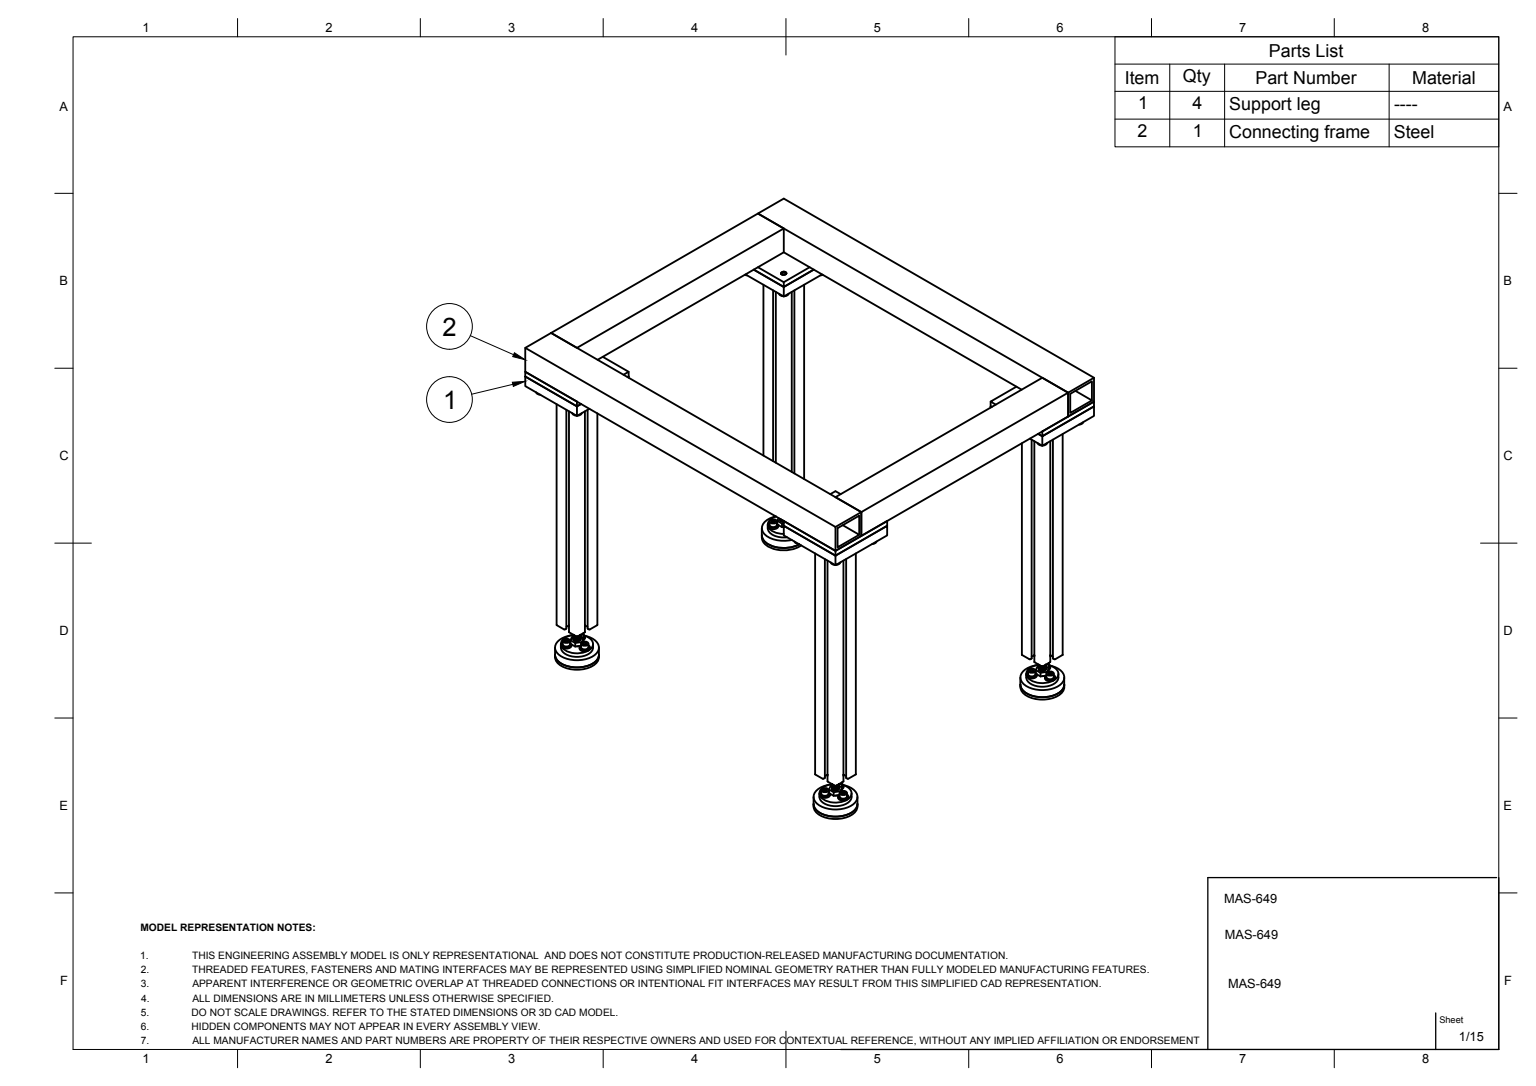
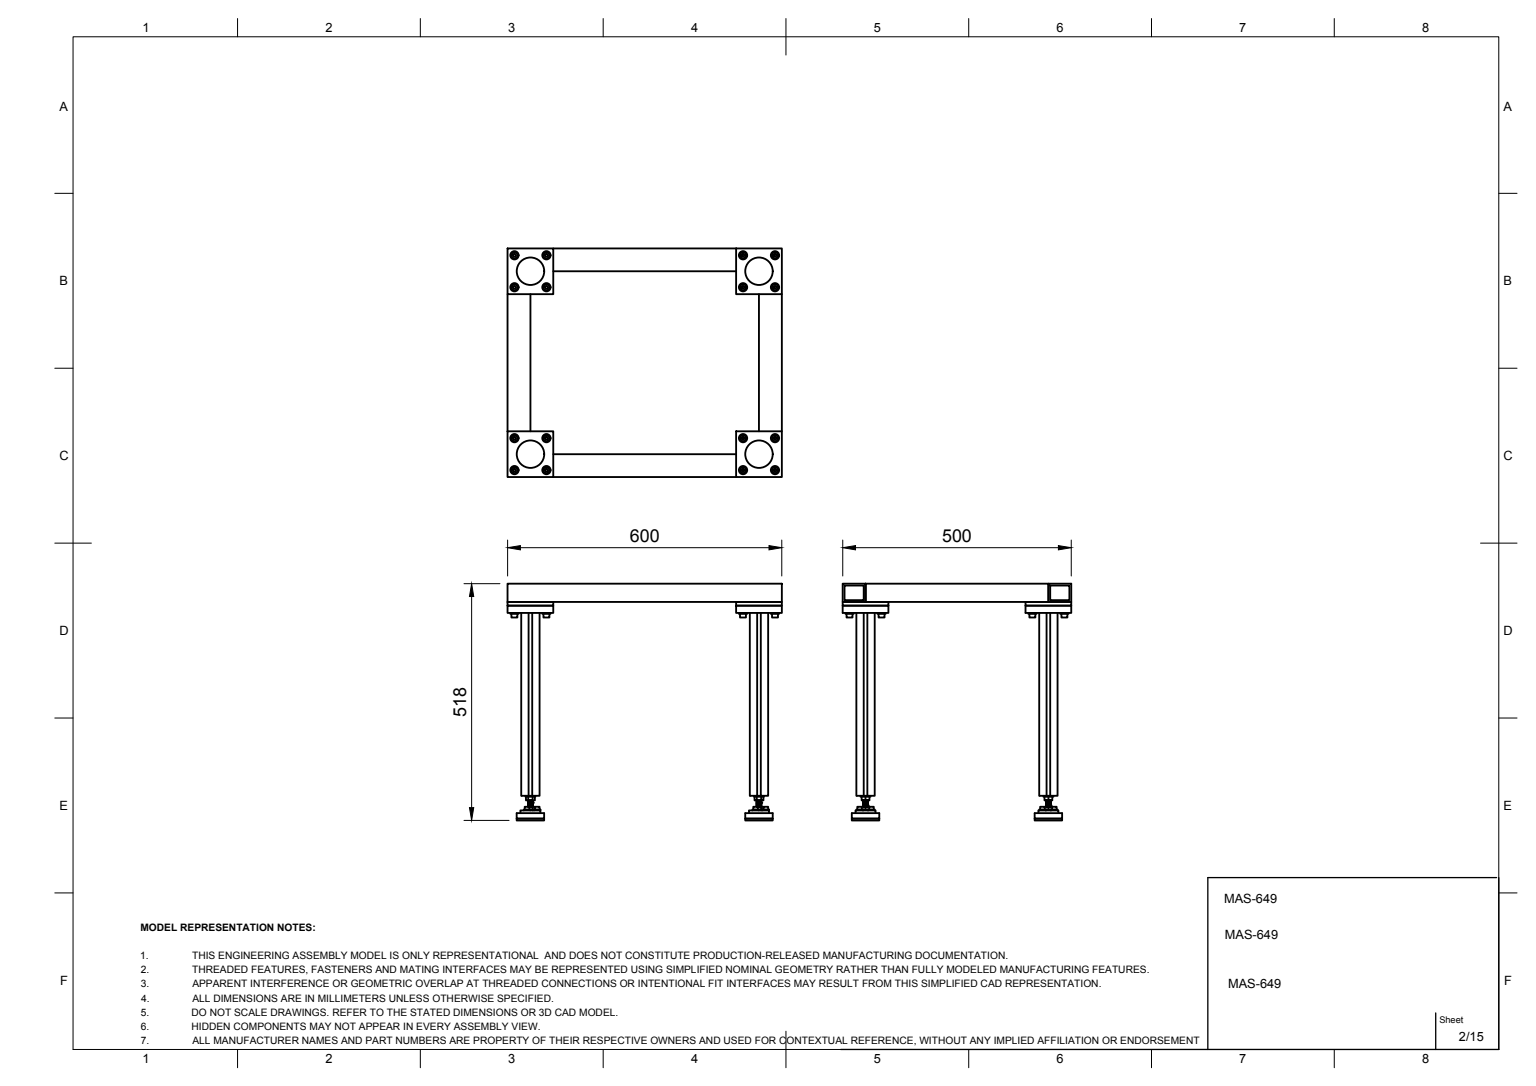
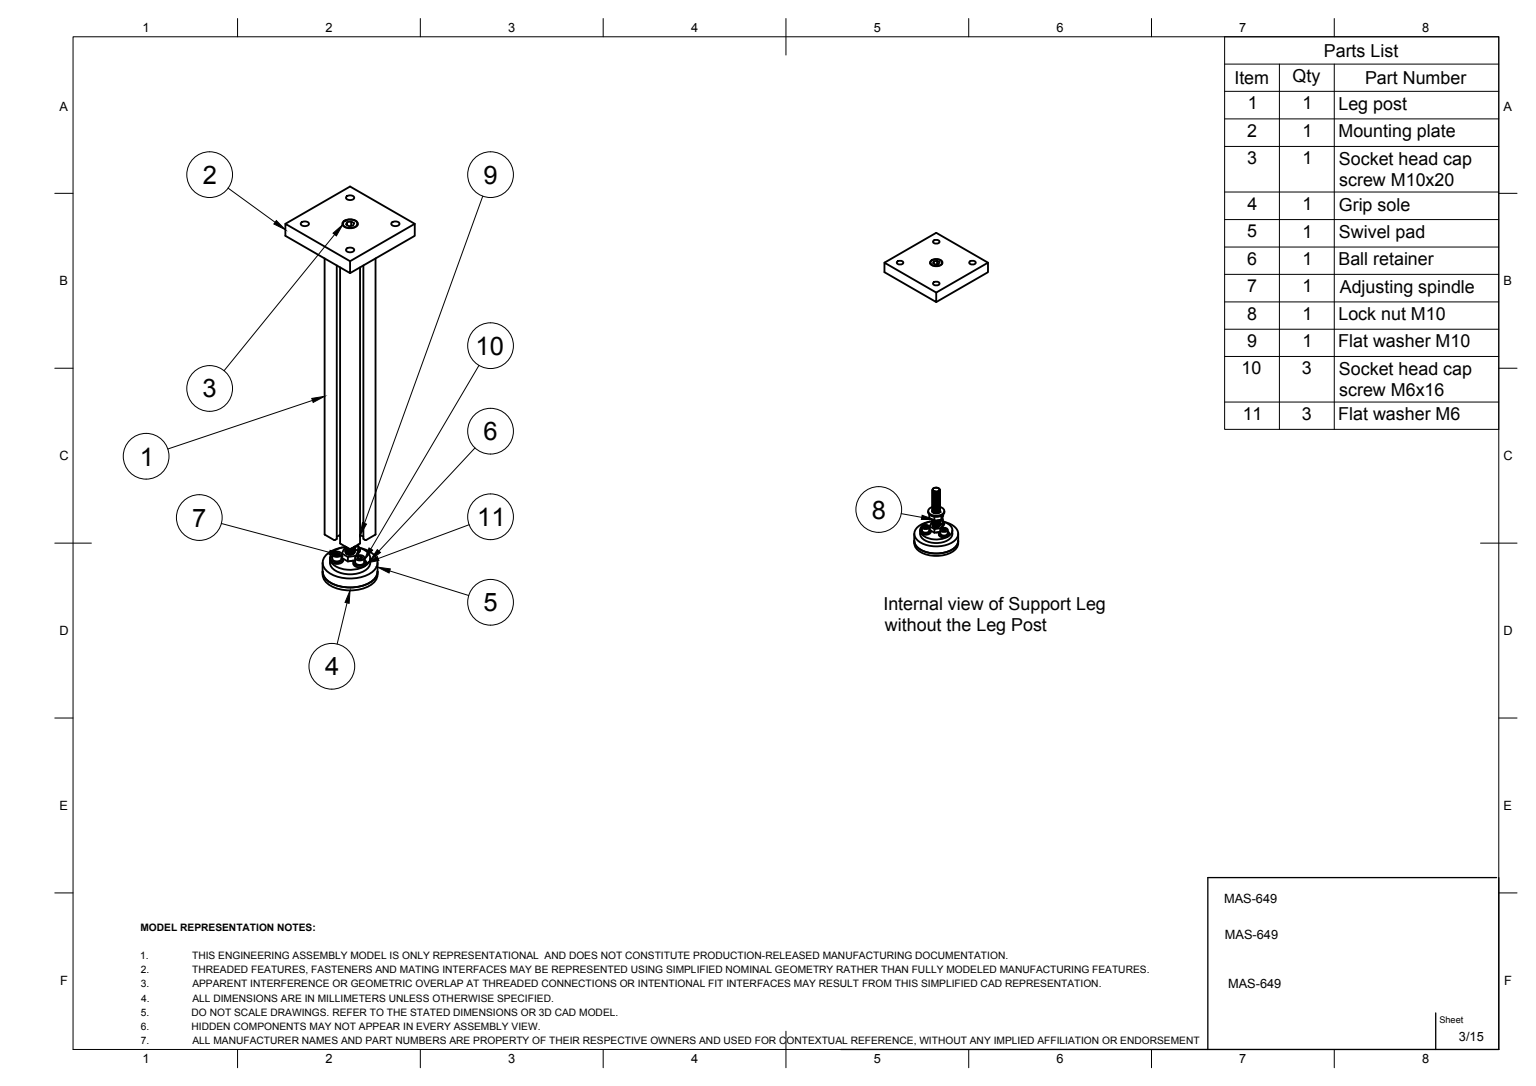
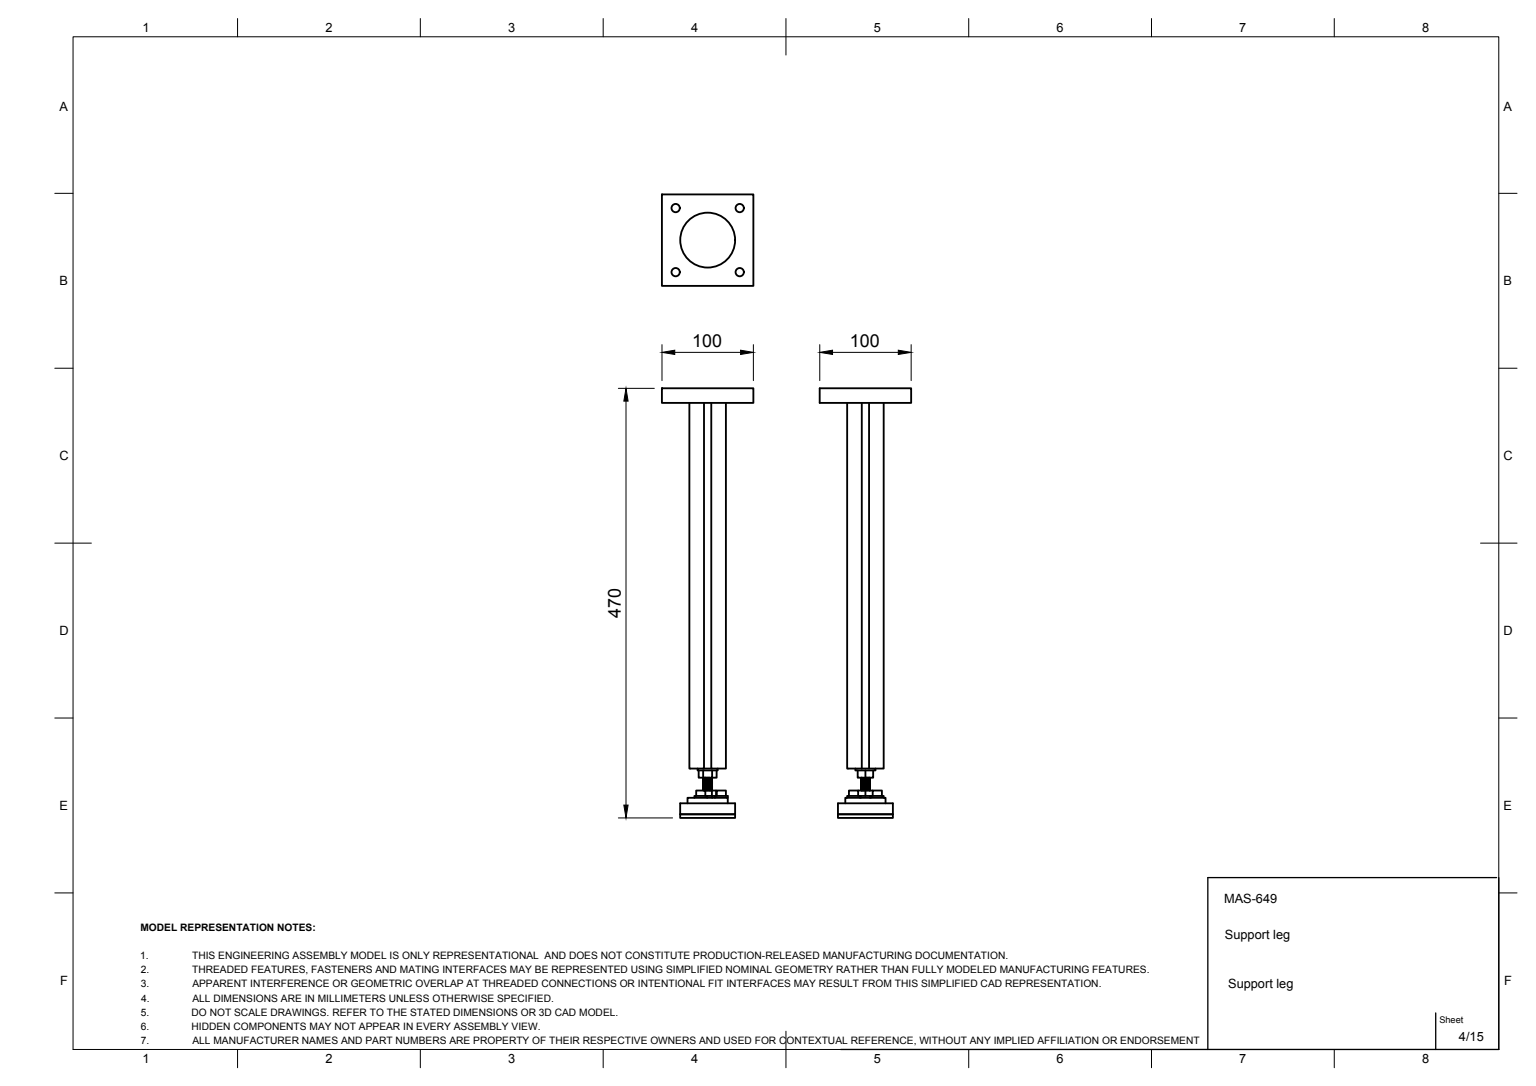
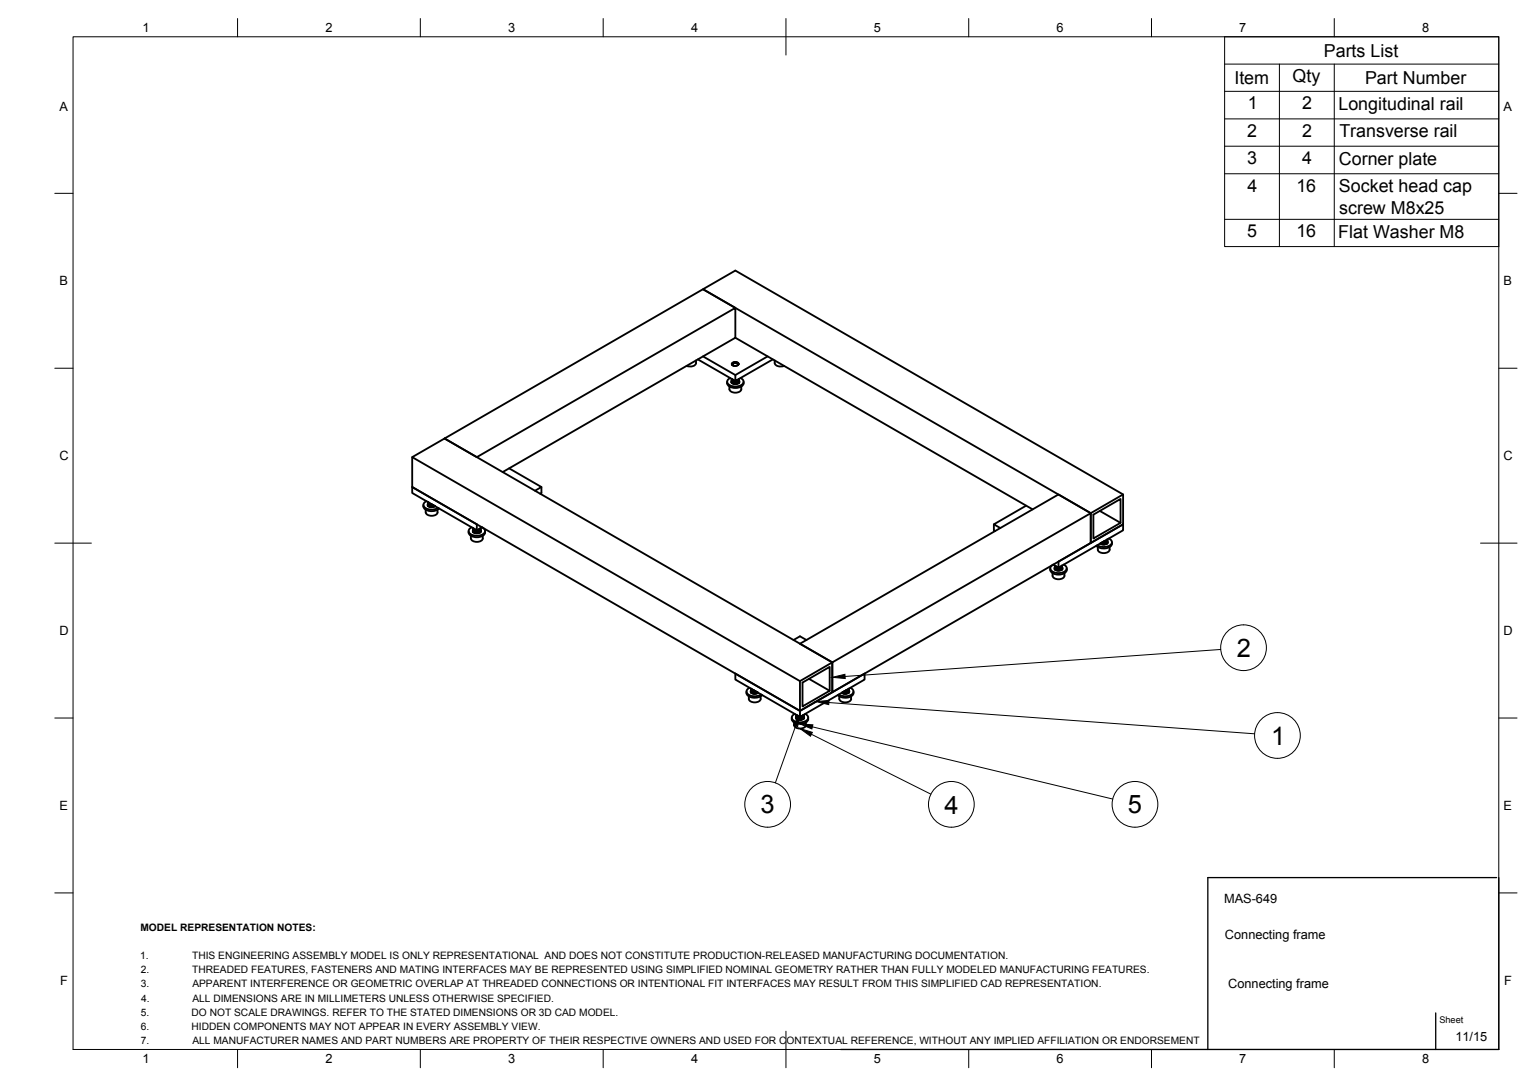
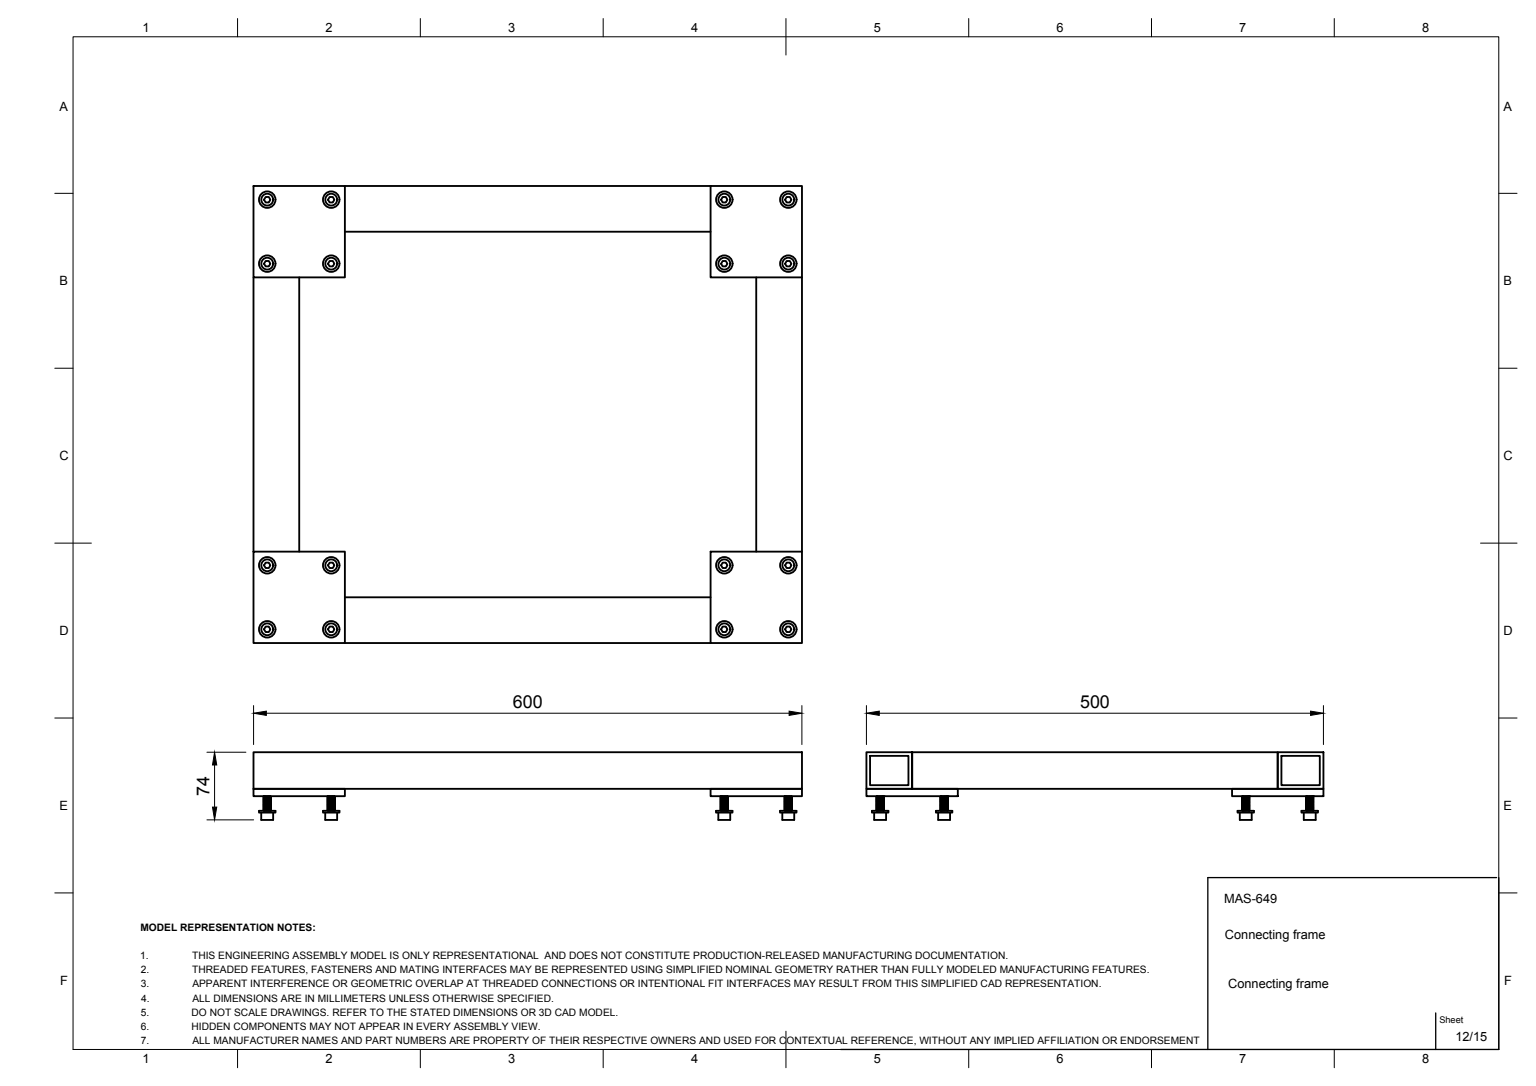
ISO-10303-21;
HEADER;
/* Generated by software containing ST-Developer
 * from STEP Tools, Inc. (www.steptools.com) 
 */

FILE_DESCRIPTION(
/* description */ ('Independent equipment support assembly with bolted 600 x 500 mm welde
d perimeter frame, four adjustable legs and swivel feet. Nominal overa
ll height 518 mm. No load rating assigned.'),
/* implementation_level */ '2;1');

FILE_NAME(
/* name */ 'MAS-649.step',
/* time_stamp */ '2026-11-07T17:30:39-08:00',
/* author */ (''),
/* organization */ (''),
/* preprocessor_version */ 'ST-DEVELOPER v20.2',
/* originating_system */ 'Autodesk Translation Framework v15.17.0.0',
/* authorisation */ '');

FILE_SCHEMA (('AUTOMOTIVE_DESIGN { 1 0 10303 214 3 1 1 }'));
ENDSEC;

DATA;
#10=MECHANICAL_DESIGN_GEOMETRIC_PRESENTATION_REPRESENTATION('',(#2208,#2209,
#2210,#2211,#2212,#2213,#2214,#2215,#2216,#2217,#2218,#2219,#2220,#2221,
#2222,#2223),#63755);
#11=SPHERICAL_SURFACE('',#15224,6.);
#12=SPHERICAL_SURFACE('',#15242,6.);
#13=SPHERICAL_SURFACE('',#15392,6.);
#14=ITEM_DEFINED_TRANSFORMATION($,$,#14504,#14700);
#15=ITEM_DEFINED_TRANSFORMATION($,$,#14515,#14701);
#16=ITEM_DEFINED_TRANSFORMATION($,$,#14526,#14702);
#17=ITEM_DEFINED_TRANSFORMATION($,$,#14621,#14703);
#18=ITEM_DEFINED_TRANSFORMATION($,$,#14691,#14704);
#19=ITEM_DEFINED_TRANSFORMATION($,$,#14504,#14705);
#20=ITEM_DEFINED_TRANSFORMATION($,$,#14515,#14706);
#21=ITEM_DEFINED_TRANSFORMATION($,$,#14526,#14707);
#22=ITEM_DEFINED_TRANSFORMATION($,$,#14526,#14708);
#23=ITEM_DEFINED_TRANSFORMATION($,$,#14526,#14709);
#24=ITEM_DEFINED_TRANSFORMATION($,$,#14621,#14710);
#25=ITEM_DEFINED_TRANSFORMATION($,$,#14691,#14711);
#26=ITEM_DEFINED_TRANSFORMATION($,$,#14621,#14712);
#27=ITEM_DEFINED_TRANSFORMATION($,$,#14691,#14713);
#28=ITEM_DEFINED_TRANSFORMATION($,$,#14621,#14714);
#29=ITEM_DEFINED_TRANSFORMATION($,$,#14691,#14715);
#30=ITEM_DEFINED_TRANSFORMATION($,$,#14621,#14716);
#31=ITEM_DEFINED_TRANSFORMATION($,$,#14691,#14717);
#32=ITEM_DEFINED_TRANSFORMATION($,$,#14621,#14718);
#33=ITEM_DEFINED_TRANSFORMATION($,$,#14691,#14719);
#34=ITEM_DEFINED_TRANSFORMATION($,$,#14621,#14720);
#35=ITEM_DEFINED_TRANSFORMATION($,$,#14691,#14721);
#36=ITEM_DEFINED_TRANSFORMATION($,$,#14621,#14722);
#37=ITEM_DEFINED_TRANSFORMATION($,$,#14691,#14723);
#38=ITEM_DEFINED_TRANSFORMATION($,$,#14621,#14724);
#39=ITEM_DEFINED_TRANSFORMATION($,$,#14691,#14725);
#40=ITEM_DEFINED_TRANSFORMATION($,$,#14621,#14726);
#41=ITEM_DEFINED_TRANSFORMATION($,$,#14691,#14727);
#42=ITEM_DEFINED_TRANSFORMATION($,$,#14621,#14728);
#43=ITEM_DEFINED_TRANSFORMATION($,$,#14691,#14729);
#44=ITEM_DEFINED_TRANSFORMATION($,$,#14621,#14730);
#45=ITEM_DEFINED_TRANSFORMATION($,$,#14691,#14731);
#46=ITEM_DEFINED_TRANSFORMATION($,$,#14621,#14732);
#47=ITEM_DEFINED_TRANSFORMATION($,$,#14691,#14733);
#48=ITEM_DEFINED_TRANSFORMATION($,$,#14621,#14734);
#49=ITEM_DEFINED_TRANSFORMATION($,$,#14691,#14735);
#50=ITEM_DEFINED_TRANSFORMATION($,$,#14621,#14736);
#51=ITEM_DEFINED_TRANSFORMATION($,$,#14691,#14737);
#52=ITEM_DEFINED_TRANSFORMATION($,$,#14621,#14738);
#53=ITEM_DEFINED_TRANSFORMATION($,$,#14691,#14739);
#54=ITEM_DEFINED_TRANSFORMATION($,$,#14741,#15495);
#55=ITEM_DEFINED_TRANSFORMATION($,$,#15053,#15496);
#56=ITEM_DEFINED_TRANSFORMATION($,$,#15079,#15497);
#57=ITEM_DEFINED_TRANSFORMATION($,$,#15139,#15498);
#58=ITEM_DEFINED_TRANSFORMATION($,$,#15145,#15499);
#59=ITEM_DEFINED_TRANSFORMATION($,$,#15232,#15500);
#60=ITEM_DEFINED_TRANSFORMATION($,$,#15253,#15501);
#61=ITEM_DEFINED_TRANSFORMATION($,$,#15394,#15502);
#62=ITEM_DEFINED_TRANSFORMATION($,$,#15425,#15503);
#63=ITEM_DEFINED_TRANSFORMATION($,$,#15434,#15504);
#64=ITEM_DEFINED_TRANSFORMATION($,$,#15486,#15505);
#65=ITEM_DEFINED_TRANSFORMATION($,$,#15434,#15506);
#66=ITEM_DEFINED_TRANSFORMATION($,$,#15486,#15507);
#67=ITEM_DEFINED_TRANSFORMATION($,$,#15434,#15508);
#68=ITEM_DEFINED_TRANSFORMATION($,$,#15486,#15509);
#69=ITEM_DEFINED_TRANSFORMATION($,$,#14740,#15510);
#70=ITEM_DEFINED_TRANSFORMATION($,$,#14503,#15511);
#71=ITEM_DEFINED_TRANSFORMATION($,$,#14740,#15512);
#72=ITEM_DEFINED_TRANSFORMATION($,$,#14740,#15513);
#73=ITEM_DEFINED_TRANSFORMATION($,$,#14740,#15514);
#74=(
REPRESENTATION_RELATIONSHIP($,$,#63860,#63859)
REPRESENTATION_RELATIONSHIP_WITH_TRANSFORMATION(#14)
SHAPE_REPRESENTATION_RELATIONSHIP()
);
#75=(
REPRESENTATION_RELATIONSHIP($,$,#63861,#63859)
REPRESENTATION_RELATIONSHIP_WITH_TRANSFORMATION(#15)
SHAPE_REPRESENTATION_RELATIONSHIP()
);
#76=(
REPRESENTATION_RELATIONSHIP($,$,#63862,#63859)
REPRESENTATION_RELATIONSHIP_WITH_TRANSFORMATION(#16)
SHAPE_REPRESENTATION_RELATIONSHIP()
);
#77=(
REPRESENTATION_RELATIONSHIP($,$,#63863,#63859)
REPRESENTATION_RELATIONSHIP_WITH_TRANSFORMATION(#17)
SHAPE_REPRESENTATION_RELATIONSHIP()
);
#78=(
REPRESENTATION_RELATIONSHIP($,$,#63864,#63859)
REPRESENTATION_RELATIONSHIP_WITH_TRANSFORMATION(#18)
SHAPE_REPRESENTATION_RELATIONSHIP()
);
#79=(
REPRESENTATION_RELATIONSHIP($,$,#63860,#63859)
REPRESENTATION_RELATIONSHIP_WITH_TRANSFORMATION(#19)
SHAPE_REPRESENTATION_RELATIONSHIP()
);
#80=(
REPRESENTATION_RELATIONSHIP($,$,#63861,#63859)
REPRESENTATION_RELATIONSHIP_WITH_TRANSFORMATION(#20)
SHAPE_REPRESENTATION_RELATIONSHIP()
);
#81=(
REPRESENTATION_RELATIONSHIP($,$,#63862,#63859)
REPRESENTATION_RELATIONSHIP_WITH_TRANSFORMATION(#21)
SHAPE_REPRESENTATION_RELATIONSHIP()
);
#82=(
REPRESENTATION_RELATIONSHIP($,$,#63862,#63859)
REPRESENTATION_RELATIONSHIP_WITH_TRANSFORMATION(#22)
SHAPE_REPRESENTATION_RELATIONSHIP()
);
#83=(
REPRESENTATION_RELATIONSHIP($,$,#63862,#63859)
REPRESENTATION_RELATIONSHIP_WITH_TRANSFORMATION(#23)
SHAPE_REPRESENTATION_RELATIONSHIP()
);
#84=(
REPRESENTATION_RELATIONSHIP($,$,#63863,#63859)
REPRESENTATION_RELATIONSHIP_WITH_TRANSFORMATION(#24)
SHAPE_REPRESENTATION_RELATIONSHIP()
);
#85=(
REPRESENTATION_RELATIONSHIP($,$,#63864,#63859)
REPRESENTATION_RELATIONSHIP_WITH_TRANSFORMATION(#25)
SHAPE_REPRESENTATION_RELATIONSHIP()
);
#86=(
REPRESENTATION_RELATIONSHIP($,$,#63863,#63859)
REPRESENTATION_RELATIONSHIP_WITH_TRANSFORMATION(#26)
SHAPE_REPRESENTATION_RELATIONSHIP()
);
#87=(
REPRESENTATION_RELATIONSHIP($,$,#63864,#63859)
REPRESENTATION_RELATIONSHIP_WITH_TRANSFORMATION(#27)
SHAPE_REPRESENTATION_RELATIONSHIP()
);
#88=(
REPRESENTATION_RELATIONSHIP($,$,#63863,#63859)
REPRESENTATION_RELATIONSHIP_WITH_TRANSFORMATION(#28)
SHAPE_REPRESENTATION_RELATIONSHIP()
);
#89=(
REPRESENTATION_RELATIONSHIP($,$,#63864,#63859)
REPRESENTATION_RELATIONSHIP_WITH_TRANSFORMATION(#29)
SHAPE_REPRESENTATION_RELATIONSHIP()
);
#90=(
REPRESENTATION_RELATIONSHIP($,$,#63863,#63859)
REPRESENTATION_RELATIONSHIP_WITH_TRANSFORMATION(#30)
SHAPE_REPRESENTATION_RELATIONSHIP()
);
#91=(
REPRESENTATION_RELATIONSHIP($,$,#63864,#63859)
REPRESENTATION_RELATIONSHIP_WITH_TRANSFORMATION(#31)
SHAPE_REPRESENTATION_RELATIONSHIP()
);
#92=(
REPRESENTATION_RELATIONSHIP($,$,#63863,#63859)
REPRESENTATION_RELATIONSHIP_WITH_TRANSFORMATION(#32)
SHAPE_REPRESENTATION_RELATIONSHIP()
);
#93=(
REPRESENTATION_RELATIONSHIP($,$,#63864,#63859)
REPRESENTATION_RELATIONSHIP_WITH_TRANSFORMATION(#33)
SHAPE_REPRESENTATION_RELATIONSHIP()
);
#94=(
REPRESENTATION_RELATIONSHIP($,$,#63863,#63859)
REPRESENTATION_RELATIONSHIP_WITH_TRANSFORMATION(#34)
SHAPE_REPRESENTATION_RELATIONSHIP()
);
#95=(
REPRESENTATION_RELATIONSHIP($,$,#63864,#63859)
REPRESENTATION_RELATIONSHIP_WITH_TRANSFORMATION(#35)
SHAPE_REPRESENTATION_RELATIONSHIP()
);
#96=(
REPRESENTATION_RELATIONSHIP($,$,#63863,#63859)
REPRESENTATION_RELATIONSHIP_WITH_TRANSFORMATION(#36)
SHAPE_REPRESENTATION_RELATIONSHIP()
);
#97=(
REPRESENTATION_RELATIONSHIP($,$,#63864,#63859)
REPRESENTATION_RELATIONSHIP_WITH_TRANSFORMATION(#37)
SHAPE_REPRESENTATION_RELATIONSHIP()
);
#98=(
REPRESENTATION_RELATIONSHIP($,$,#63863,#63859)
REPRESENTATION_RELATIONSHIP_WITH_TRANSFORMATION(#38)
SHAPE_REPRESENTATION_RELATIONSHIP()
);
#99=(
REPRESENTATION_RELATIONSHIP($,$,#63864,#63859)
REPRESENTATION_RELATIONSHIP_WITH_TRANSFORMATION(#39)
SHAPE_REPRESENTATION_RELATIONSHIP()
);
#100=(
REPRESENTATION_RELATIONSHIP($,$,#63863,#63859)
REPRESENTATION_RELATIONSHIP_WITH_TRANSFORMATION(#40)
SHAPE_REPRESENTATION_RELATIONSHIP()
);
#101=(
REPRESENTATION_RELATIONSHIP($,$,#63864,#63859)
REPRESENTATION_RELATIONSHIP_WITH_TRANSFORMATION(#41)
SHAPE_REPRESENTATION_RELATIONSHIP()
);
#102=(
REPRESENTATION_RELATIONSHIP($,$,#63863,#63859)
REPRESENTATION_RELATIONSHIP_WITH_TRANSFORMATION(#42)
SHAPE_REPRESENTATION_RELATIONSHIP()
);
#103=(
REPRESENTATION_RELATIONSHIP($,$,#63864,#63859)
REPRESENTATION_RELATIONSHIP_WITH_TRANSFORMATION(#43)
SHAPE_REPRESENTATION_RELATIONSHIP()
);
#104=(
REPRESENTATION_RELATIONSHIP($,$,#63863,#63859)
REPRESENTATION_RELATIONSHIP_WITH_TRANSFORMATION(#44)
SHAPE_REPRESENTATION_RELATIONSHIP()
);
#105=(
REPRESENTATION_RELATIONSHIP($,$,#63864,#63859)
REPRESENTATION_RELATIONSHIP_WITH_TRANSFORMATION(#45)
SHAPE_REPRESENTATION_RELATIONSHIP()
);
#106=(
REPRESENTATION_RELATIONSHIP($,$,#63863,#63859)
REPRESENTATION_RELATIONSHIP_WITH_TRANSFORMATION(#46)
SHAPE_REPRESENTATION_RELATIONSHIP()
);
#107=(
REPRESENTATION_RELATIONSHIP($,$,#63864,#63859)
REPRESENTATION_RELATIONSHIP_WITH_TRANSFORMATION(#47)
SHAPE_REPRESENTATION_RELATIONSHIP()
);
#108=(
REPRESENTATION_RELATIONSHIP($,$,#63863,#63859)
REPRESENTATION_RELATIONSHIP_WITH_TRANSFORMATION(#48)
SHAPE_REPRESENTATION_RELATIONSHIP()
);
#109=(
REPRESENTATION_RELATIONSHIP($,$,#63864,#63859)
REPRESENTATION_RELATIONSHIP_WITH_TRANSFORMATION(#49)
SHAPE_REPRESENTATION_RELATIONSHIP()
);
#110=(
REPRESENTATION_RELATIONSHIP($,$,#63863,#63859)
REPRESENTATION_RELATIONSHIP_WITH_TRANSFORMATION(#50)
SHAPE_REPRESENTATION_RELATIONSHIP()
);
#111=(
REPRESENTATION_RELATIONSHIP($,$,#63864,#63859)
REPRESENTATION_RELATIONSHIP_WITH_TRANSFORMATION(#51)
SHAPE_REPRESENTATION_RELATIONSHIP()
);
#112=(
REPRESENTATION_RELATIONSHIP($,$,#63863,#63859)
REPRESENTATION_RELATIONSHIP_WITH_TRANSFORMATION(#52)
SHAPE_REPRESENTATION_RELATIONSHIP()
);
#113=(
REPRESENTATION_RELATIONSHIP($,$,#63864,#63859)
REPRESENTATION_RELATIONSHIP_WITH_TRANSFORMATION(#53)
SHAPE_REPRESENTATION_RELATIONSHIP()
);
#114=(
REPRESENTATION_RELATIONSHIP($,$,#63866,#63865)
REPRESENTATION_RELATIONSHIP_WITH_TRANSFORMATION(#54)
SHAPE_REPRESENTATION_RELATIONSHIP()
);
#115=(
REPRESENTATION_RELATIONSHIP($,$,#63867,#63865)
REPRESENTATION_RELATIONSHIP_WITH_TRANSFORMATION(#55)
SHAPE_REPRESENTATION_RELATIONSHIP()
);
#116=(
REPRESENTATION_RELATIONSHIP($,$,#63868,#63865)
REPRESENTATION_RELATIONSHIP_WITH_TRANSFORMATION(#56)
SHAPE_REPRESENTATION_RELATIONSHIP()
);
#117=(
REPRESENTATION_RELATIONSHIP($,$,#63869,#63865)
REPRESENTATION_RELATIONSHIP_WITH_TRANSFORMATION(#57)
SHAPE_REPRESENTATION_RELATIONSHIP()
);
#118=(
REPRESENTATION_RELATIONSHIP($,$,#63870,#63865)
REPRESENTATION_RELATIONSHIP_WITH_TRANSFORMATION(#58)
SHAPE_REPRESENTATION_RELATIONSHIP()
);
#119=(
REPRESENTATION_RELATIONSHIP($,$,#63871,#63865)
REPRESENTATION_RELATIONSHIP_WITH_TRANSFORMATION(#59)
SHAPE_REPRESENTATION_RELATIONSHIP()
);
#120=(
REPRESENTATION_RELATIONSHIP($,$,#63872,#63865)
REPRESENTATION_RELATIONSHIP_WITH_TRANSFORMATION(#60)
SHAPE_REPRESENTATION_RELATIONSHIP()
);
#121=(
REPRESENTATION_RELATIONSHIP($,$,#63873,#63865)
REPRESENTATION_RELATIONSHIP_WITH_TRANSFORMATION(#61)
SHAPE_REPRESENTATION_RELATIONSHIP()
);
#122=(
REPRESENTATION_RELATIONSHIP($,$,#63874,#63865)
REPRESENTATION_RELATIONSHIP_WITH_TRANSFORMATION(#62)
SHAPE_REPRESENTATION_RELATIONSHIP()
);
#123=(
REPRESENTATION_RELATIONSHIP($,$,#63875,#63865)
REPRESENTATION_RELATIONSHIP_WITH_TRANSFORMATION(#63)
SHAPE_REPRESENTATION_RELATIONSHIP()
);
#124=(
REPRESENTATION_RELATIONSHIP($,$,#63876,#63865)
REPRESENTATION_RELATIONSHIP_WITH_TRANSFORMATION(#64)
SHAPE_REPRESENTATION_RELATIONSHIP()
);
#125=(
REPRESENTATION_RELATIONSHIP($,$,#63875,#63865)
REPRESENTATION_RELATIONSHIP_WITH_TRANSFORMATION(#65)
SHAPE_REPRESENTATION_RELATIONSHIP()
);
#126=(
REPRESENTATION_RELATIONSHIP($,$,#63876,#63865)
REPRESENTATION_RELATIONSHIP_WITH_TRANSFORMATION(#66)
SHAPE_REPRESENTATION_RELATIONSHIP()
);
#127=(
REPRESENTATION_RELATIONSHIP($,$,#63875,#63865)
REPRESENTATION_RELATIONSHIP_WITH_TRANSFORMATION(#67)
SHAPE_REPRESENTATION_RELATIONSHIP()
);
#128=(
REPRESENTATION_RELATIONSHIP($,$,#63876,#63865)
REPRESENTATION_RELATIONSHIP_WITH_TRANSFORMATION(#68)
SHAPE_REPRESENTATION_RELATIONSHIP()
);
#129=(
REPRESENTATION_RELATIONSHIP($,$,#63865,#63858)
REPRESENTATION_RELATIONSHIP_WITH_TRANSFORMATION(#69)
SHAPE_REPRESENTATION_RELATIONSHIP()
);
#130=(
REPRESENTATION_RELATIONSHIP($,$,#63859,#63858)
REPRESENTATION_RELATIONSHIP_WITH_TRANSFORMATION(#70)
SHAPE_REPRESENTATION_RELATIONSHIP()
);
#131=(
REPRESENTATION_RELATIONSHIP($,$,#63865,#63858)
REPRESENTATION_RELATIONSHIP_WITH_TRANSFORMATION(#71)
SHAPE_REPRESENTATION_RELATIONSHIP()
);
#132=(
REPRESENTATION_RELATIONSHIP($,$,#63865,#63858)
REPRESENTATION_RELATIONSHIP_WITH_TRANSFORMATION(#72)
SHAPE_REPRESENTATION_RELATIONSHIP()
);
#133=(
REPRESENTATION_RELATIONSHIP($,$,#63865,#63858)
REPRESENTATION_RELATIONSHIP_WITH_TRANSFORMATION(#73)
SHAPE_REPRESENTATION_RELATIONSHIP()
);
#134=CONTEXT_DEPENDENT_SHAPE_REPRESENTATION(#74,#63786);
#135=CONTEXT_DEPENDENT_SHAPE_REPRESENTATION(#75,#63787);
#136=CONTEXT_DEPENDENT_SHAPE_REPRESENTATION(#76,#63788);
#137=CONTEXT_DEPENDENT_SHAPE_REPRESENTATION(#77,#63789);
#138=CONTEXT_DEPENDENT_SHAPE_REPRESENTATION(#78,#63790);
#139=CONTEXT_DEPENDENT_SHAPE_REPRESENTATION(#79,#63791);
#140=CONTEXT_DEPENDENT_SHAPE_REPRESENTATION(#80,#63792);
#141=CONTEXT_DEPENDENT_SHAPE_REPRESENTATION(#81,#63793);
#142=CONTEXT_DEPENDENT_SHAPE_REPRESENTATION(#82,#63794);
#143=CONTEXT_DEPENDENT_SHAPE_REPRESENTATION(#83,#63795);
#144=CONTEXT_DEPENDENT_SHAPE_REPRESENTATION(#84,#63796);
#145=CONTEXT_DEPENDENT_SHAPE_REPRESENTATION(#85,#63797);
#146=CONTEXT_DEPENDENT_SHAPE_REPRESENTATION(#86,#63798);
#147=CONTEXT_DEPENDENT_SHAPE_REPRESENTATION(#87,#63799);
#148=CONTEXT_DEPENDENT_SHAPE_REPRESENTATION(#88,#63800);
#149=CONTEXT_DEPENDENT_SHAPE_REPRESENTATION(#89,#63801);
#150=CONTEXT_DEPENDENT_SHAPE_REPRESENTATION(#90,#63802);
#151=CONTEXT_DEPENDENT_SHAPE_REPRESENTATION(#91,#63803);
#152=CONTEXT_DEPENDENT_SHAPE_REPRESENTATION(#92,#63804);
#153=CONTEXT_DEPENDENT_SHAPE_REPRESENTATION(#93,#63805);
#154=CONTEXT_DEPENDENT_SHAPE_REPRESENTATION(#94,#63806);
#155=CONTEXT_DEPENDENT_SHAPE_REPRESENTATION(#95,#63807);
#156=CONTEXT_DEPENDENT_SHAPE_REPRESENTATION(#96,#63808);
#157=CONTEXT_DEPENDENT_SHAPE_REPRESENTATION(#97,#63809);
#158=CONTEXT_DEPENDENT_SHAPE_REPRESENTATION(#98,#63810);
#159=CONTEXT_DEPENDENT_SHAPE_REPRESENTATION(#99,#63811);
#160=CONTEXT_DEPENDENT_SHAPE_REPRESENTATION(#100,#63812);
#161=CONTEXT_DEPENDENT_SHAPE_REPRESENTATION(#101,#63813);
#162=CONTEXT_DEPENDENT_SHAPE_REPRESENTATION(#102,#63814);
#163=CONTEXT_DEPENDENT_SHAPE_REPRESENTATION(#103,#63815);
#164=CONTEXT_DEPENDENT_SHAPE_REPRESENTATION(#104,#63816);
#165=CONTEXT_DEPENDENT_SHAPE_REPRESENTATION(#105,#63817);
#166=CONTEXT_DEPENDENT_SHAPE_REPRESENTATION(#106,#63818);
#167=CONTEXT_DEPENDENT_SHAPE_REPRESENTATION(#107,#63819);
#168=CONTEXT_DEPENDENT_SHAPE_REPRESENTATION(#108,#63820);
#169=CONTEXT_DEPENDENT_SHAPE_REPRESENTATION(#109,#63821);
#170=CONTEXT_DEPENDENT_SHAPE_REPRESENTATION(#110,#63822);
#171=CONTEXT_DEPENDENT_SHAPE_REPRESENTATION(#111,#63823);
#172=CONTEXT_DEPENDENT_SHAPE_REPRESENTATION(#112,#63824);
#173=CONTEXT_DEPENDENT_SHAPE_REPRESENTATION(#113,#63825);
#174=CONTEXT_DEPENDENT_SHAPE_REPRESENTATION(#114,#63838);
#175=CONTEXT_DEPENDENT_SHAPE_REPRESENTATION(#115,#63839);
#176=CONTEXT_DEPENDENT_SHAPE_REPRESENTATION(#116,#63840);
#177=CONTEXT_DEPENDENT_SHAPE_REPRESENTATION(#117,#63841);
#178=CONTEXT_DEPENDENT_SHAPE_REPRESENTATION(#118,#63842);
#179=CONTEXT_DEPENDENT_SHAPE_REPRESENTATION(#119,#63843);
#180=CONTEXT_DEPENDENT_SHAPE_REPRESENTATION(#120,#63844);
#181=CONTEXT_DEPENDENT_SHAPE_REPRESENTATION(#121,#63845);
#182=CONTEXT_DEPENDENT_SHAPE_REPRESENTATION(#122,#63846);
#183=CONTEXT_DEPENDENT_SHAPE_REPRESENTATION(#123,#63847);
#184=CONTEXT_DEPENDENT_SHAPE_REPRESENTATION(#124,#63848);
#185=CONTEXT_DEPENDENT_SHAPE_REPRESENTATION(#125,#63849);
#186=CONTEXT_DEPENDENT_SHAPE_REPRESENTATION(#126,#63850);
#187=CONTEXT_DEPENDENT_SHAPE_REPRESENTATION(#127,#63851);
#188=CONTEXT_DEPENDENT_SHAPE_REPRESENTATION(#128,#63852);
#189=CONTEXT_DEPENDENT_SHAPE_REPRESENTATION(#129,#63853);
#190=CONTEXT_DEPENDENT_SHAPE_REPRESENTATION(#130,#63854);
#191=CONTEXT_DEPENDENT_SHAPE_REPRESENTATION(#131,#63855);
#192=CONTEXT_DEPENDENT_SHAPE_REPRESENTATION(#132,#63856);
#193=CONTEXT_DEPENDENT_SHAPE_REPRESENTATION(#133,#63857);
#194=NEXT_ASSEMBLY_USAGE_OCCURRENCE('Longitudinal rail:1',
'Longitudinal rail:1','Longitudinal rail:1',#63879,#63880,
'Longitudinal rail:1');
#195=NEXT_ASSEMBLY_USAGE_OCCURRENCE('Transverse rail:1',
'Transverse rail:1','Transverse rail:1',#63879,#63881,
'Transverse rail:1');
#196=NEXT_ASSEMBLY_USAGE_OCCURRENCE('Corner plate:1','Corner plate:1',
'Corner plate:1',#63879,#63882,'Corner plate:1');
#197=NEXT_ASSEMBLY_USAGE_OCCURRENCE('Socket head cap screw M8x25:1',
'Socket head cap screw M8x25:1','Socket head cap screw M8x25:1',#63879,
#63883,'Socket head cap screw M8x25:1');
#198=NEXT_ASSEMBLY_USAGE_OCCURRENCE('Flat washer M8:1',
'Flat washer M8:1','Flat washer M8:1',#63879,#63884,'Flat washer M8:1');
#199=NEXT_ASSEMBLY_USAGE_OCCURRENCE('Longitudinal rail:2',
'Longitudinal rail:2','Longitudinal rail:2',#63879,#63880,
'Longitudinal rail:2');
#200=NEXT_ASSEMBLY_USAGE_OCCURRENCE('Transverse rail:2',
'Transverse rail:2','Transverse rail:2',#63879,#63881,
'Transverse rail:2');
#201=NEXT_ASSEMBLY_USAGE_OCCURRENCE('Corner plate:2','Corner plate:2',
'Corner plate:2',#63879,#63882,'Corner plate:2');
#202=NEXT_ASSEMBLY_USAGE_OCCURRENCE('Corner plate:3','Corner plate:3',
'Corner plate:3',#63879,#63882,'Corner plate:3');
#203=NEXT_ASSEMBLY_USAGE_OCCURRENCE('Corner plate:4','Corner plate:4',
'Corner plate:4',#63879,#63882,'Corner plate:4');
#204=NEXT_ASSEMBLY_USAGE_OCCURRENCE('Socket head cap screw M8x25:2',
'Socket head cap screw M8x25:2','Socket head cap screw M8x25:2',#63879,
#63883,'Socket head cap screw M8x25:2');
#205=NEXT_ASSEMBLY_USAGE_OCCURRENCE('Flat washer M8:2',
'Flat washer M8:2','Flat washer M8:2',#63879,#63884,'Flat washer M8:2');
#206=NEXT_ASSEMBLY_USAGE_OCCURRENCE('Socket head cap screw M8x25:3',
'Socket head cap screw M8x25:3','Socket head cap screw M8x25:3',#63879,
#63883,'Socket head cap screw M8x25:3');
#207=NEXT_ASSEMBLY_USAGE_OCCURRENCE('Flat washer M8:3',
'Flat washer M8:3','Flat washer M8:3',#63879,#63884,'Flat washer M8:3');
#208=NEXT_ASSEMBLY_USAGE_OCCURRENCE('Socket head cap screw M8x25:4',
'Socket head cap screw M8x25:4','Socket head cap screw M8x25:4',#63879,
#63883,'Socket head cap screw M8x25:4');
#209=NEXT_ASSEMBLY_USAGE_OCCURRENCE('Flat washer M8:4',
'Flat washer M8:4','Flat washer M8:4',#63879,#63884,'Flat washer M8:4');
#210=NEXT_ASSEMBLY_USAGE_OCCURRENCE('Socket head cap screw M8x25:5',
'Socket head cap screw M8x25:5','Socket head cap screw M8x25:5',#63879,
#63883,'Socket head cap screw M8x25:5');
#211=NEXT_ASSEMBLY_USAGE_OCCURRENCE('Flat washer M8:5',
'Flat washer M8:5','Flat washer M8:5',#63879,#63884,'Flat washer M8:5');
#212=NEXT_ASSEMBLY_USAGE_OCCURRENCE('Socket head cap screw M8x25:6',
'Socket head cap screw M8x25:6','Socket head cap screw M8x25:6',#63879,
#63883,'Socket head cap screw M8x25:6');
#213=NEXT_ASSEMBLY_USAGE_OCCURRENCE('Flat washer M8:6',
'Flat washer M8:6','Flat washer M8:6',#63879,#63884,'Flat washer M8:6');
#214=NEXT_ASSEMBLY_USAGE_OCCURRENCE('Socket head cap screw M8x25:7',
'Socket head cap screw M8x25:7','Socket head cap screw M8x25:7',#63879,
#63883,'Socket head cap screw M8x25:7');
#215=NEXT_ASSEMBLY_USAGE_OCCURRENCE('Flat washer M8:7',
'Flat washer M8:7','Flat washer M8:7',#63879,#63884,'Flat washer M8:7');
#216=NEXT_ASSEMBLY_USAGE_OCCURRENCE('Socket head cap screw M8x25:8',
'Socket head cap screw M8x25:8','Socket head cap screw M8x25:8',#63879,
#63883,'Socket head cap screw M8x25:8');
#217=NEXT_ASSEMBLY_USAGE_OCCURRENCE('Flat washer M8:8',
'Flat washer M8:8','Flat washer M8:8',#63879,#63884,'Flat washer M8:8');
#218=NEXT_ASSEMBLY_USAGE_OCCURRENCE('Socket head cap screw M8x25:9',
'Socket head cap screw M8x25:9','Socket head cap screw M8x25:9',#63879,
#63883,'Socket head cap screw M8x25:9');
#219=NEXT_ASSEMBLY_USAGE_OCCURRENCE('Flat washer M8:9',
'Flat washer M8:9','Flat washer M8:9',#63879,#63884,'Flat washer M8:9');
#220=NEXT_ASSEMBLY_USAGE_OCCURRENCE('Socket head cap screw M8x25:10',
'Socket head cap screw M8x25:10','Socket head cap screw M8x25:10',#63879,
#63883,'Socket head cap screw M8x25:10');
#221=NEXT_ASSEMBLY_USAGE_OCCURRENCE('Flat washer M8:10',
'Flat washer M8:10','Flat washer M8:10',#63879,#63884,
'Flat washer M8:10');
#222=NEXT_ASSEMBLY_USAGE_OCCURRENCE('Socket head cap screw M8x25:11',
'Socket head cap screw M8x25:11','Socket head cap screw M8x25:11',#63879,
#63883,'Socket head cap screw M8x25:11');
#223=NEXT_ASSEMBLY_USAGE_OCCURRENCE('Flat washer M8:11',
'Flat washer M8:11','Flat washer M8:11',#63879,#63884,
'Flat washer M8:11');
#224=NEXT_ASSEMBLY_USAGE_OCCURRENCE('Socket head cap screw M8x25:12',
'Socket head cap screw M8x25:12','Socket head cap screw M8x25:12',#63879,
#63883,'Socket head cap screw M8x25:12');
#225=NEXT_ASSEMBLY_USAGE_OCCURRENCE('Flat washer M8:12',
'Flat washer M8:12','Flat washer M8:12',#63879,#63884,
'Flat washer M8:12');
#226=NEXT_ASSEMBLY_USAGE_OCCURRENCE('Socket head cap screw M8x25:13',
'Socket head cap screw M8x25:13','Socket head cap screw M8x25:13',#63879,
#63883,'Socket head cap screw M8x25:13');
#227=NEXT_ASSEMBLY_USAGE_OCCURRENCE('Flat washer M8:13',
'Flat washer M8:13','Flat washer M8:13',#63879,#63884,
'Flat washer M8:13');
#228=NEXT_ASSEMBLY_USAGE_OCCURRENCE('Socket head cap screw M8x25:14',
'Socket head cap screw M8x25:14','Socket head cap screw M8x25:14',#63879,
#63883,'Socket head cap screw M8x25:14');
#229=NEXT_ASSEMBLY_USAGE_OCCURRENCE('Flat washer M8:14',
'Flat washer M8:14','Flat washer M8:14',#63879,#63884,
'Flat washer M8:14');
#230=NEXT_ASSEMBLY_USAGE_OCCURRENCE('Socket head cap screw M8x25:15',
'Socket head cap screw M8x25:15','Socket head cap screw M8x25:15',#63879,
#63883,'Socket head cap screw M8x25:15');
#231=NEXT_ASSEMBLY_USAGE_OCCURRENCE('Flat washer M8:15',
'Flat washer M8:15','Flat washer M8:15',#63879,#63884,
'Flat washer M8:15');
#232=NEXT_ASSEMBLY_USAGE_OCCURRENCE('Socket head cap screw M8x25:16',
'Socket head cap screw M8x25:16','Socket head cap screw M8x25:16',#63879,
#63883,'Socket head cap screw M8x25:16');
#233=NEXT_ASSEMBLY_USAGE_OCCURRENCE('Flat washer M8:16',
'Flat washer M8:16','Flat washer M8:16',#63879,#63884,
'Flat washer M8:16');
#234=NEXT_ASSEMBLY_USAGE_OCCURRENCE('Leg post:1','Leg post:1',
'Leg post:1',#63885,#63886,'Leg post:1');
#235=NEXT_ASSEMBLY_USAGE_OCCURRENCE('Mounting plate:1',
'Mounting plate:1','Mounting plate:1',#63885,#63887,'Mounting plate:1');
#236=NEXT_ASSEMBLY_USAGE_OCCURRENCE('Socket head cap screw M10x20:1',
'Socket head cap screw M10x20:1','Socket head cap screw M10x20:1',#63885,
#63888,'Socket head cap screw M10x20:1');
#237=NEXT_ASSEMBLY_USAGE_OCCURRENCE('Grip sole:1','Grip sole:1',
'Grip sole:1',#63885,#63889,'Grip sole:1');
#238=NEXT_ASSEMBLY_USAGE_OCCURRENCE('Swivel pad:1','Swivel pad:1',
'Swivel pad:1',#63885,#63890,'Swivel pad:1');
#239=NEXT_ASSEMBLY_USAGE_OCCURRENCE('Ball retainer:1','Ball retainer:1',
'Ball retainer:1',#63885,#63891,'Ball retainer:1');
#240=NEXT_ASSEMBLY_USAGE_OCCURRENCE('Adjusting spindle:1',
'Adjusting spindle:1','Adjusting spindle:1',#63885,#63892,
'Adjusting spindle:1');
#241=NEXT_ASSEMBLY_USAGE_OCCURRENCE('Lock nut M10:1','Lock nut M10:1',
'Lock nut M10:1',#63885,#63893,'Lock nut M10:1');
#242=NEXT_ASSEMBLY_USAGE_OCCURRENCE('Flat washer M10:1',
'Flat washer M10:1','Flat washer M10:1',#63885,#63894,
'Flat washer M10:1');
#243=NEXT_ASSEMBLY_USAGE_OCCURRENCE('Socket head cap screw M6x16:1',
'Socket head cap screw M6x16:1','Socket head cap screw M6x16:1',#63885,
#63895,'Socket head cap screw M6x16:1');
#244=NEXT_ASSEMBLY_USAGE_OCCURRENCE('Flat washer M6:1',
'Flat washer M6:1','Flat washer M6:1',#63885,#63896,'Flat washer M6:1');
#245=NEXT_ASSEMBLY_USAGE_OCCURRENCE('Socket head cap screw M6x16:2',
'Socket head cap screw M6x16:2','Socket head cap screw M6x16:2',#63885,
#63895,'Socket head cap screw M6x16:2');
#246=NEXT_ASSEMBLY_USAGE_OCCURRENCE('Flat washer M6:2',
'Flat washer M6:2','Flat washer M6:2',#63885,#63896,'Flat washer M6:2');
#247=NEXT_ASSEMBLY_USAGE_OCCURRENCE('Socket head cap screw M6x16:3',
'Socket head cap screw M6x16:3','Socket head cap screw M6x16:3',#63885,
#63895,'Socket head cap screw M6x16:3');
#248=NEXT_ASSEMBLY_USAGE_OCCURRENCE('Flat washer M6:3',
'Flat washer M6:3','Flat washer M6:3',#63885,#63896,'Flat washer M6:3');
#249=NEXT_ASSEMBLY_USAGE_OCCURRENCE('Support leg:1','Support leg:1',
'Support leg:1',#63878,#63885,'Support leg:1');
#250=NEXT_ASSEMBLY_USAGE_OCCURRENCE('Connecting frame:1',
'Connecting frame:1','Connecting frame:1',#63878,#63879,
'Connecting frame:1');
#251=NEXT_ASSEMBLY_USAGE_OCCURRENCE('Support leg:2','Support leg:2',
'Support leg:2',#63878,#63885,'Support leg:2');
#252=NEXT_ASSEMBLY_USAGE_OCCURRENCE('Support leg:3','Support leg:3',
'Support leg:3',#63878,#63885,'Support leg:3');
#253=NEXT_ASSEMBLY_USAGE_OCCURRENCE('Support leg:4','Support leg:4',
'Support leg:4',#63878,#63885,'Support leg:4');
#254=CONICAL_SURFACE('',#14672,3.5,0.785398163397448);
#255=CONICAL_SURFACE('',#15120,4.5,0.785398163397448);
#256=CONICAL_SURFACE('',#15467,2.5,0.785398163397448);
#257=B_SPLINE_SURFACE_WITH_KNOTS('',3,3,((#20700,#20701,#20702,#20703,#20704,
#20705,#20706,#20707,#20708,#20709,#20710,#20711,#20712,#20713,#20714,#20715,
#20716,#20717,#20718,#20719,#20720,#20721,#20722,#20723,#20724,#20725,#20726,
#20727,#20728,#20729,#20730,#20731,#20732,#20733,#20734,#20735,#20736,#20737,
#20738,#20739,#20740,#20741,#20742,#20743,#20744,#20745,#20746,#20747,#20748,
#20749,#20750,#20751,#20752,#20753,#20754,#20755),(#20756,#20757,#20758,
#20759,#20760,#20761,#20762,#20763,#20764,#20765,#20766,#20767,#20768,#20769,
#20770,#20771,#20772,#20773,#20774,#20775,#20776,#20777,#20778,#20779,#20780,
#20781,#20782,#20783,#20784,#20785,#20786,#20787,#20788,#20789,#20790,#20791,
#20792,#20793,#20794,#20795,#20796,#20797,#20798,#20799,#20800,#20801,#20802,
#20803,#20804,#20805,#20806,#20807,#20808,#20809,#20810,#20811),(#20812,
#20813,#20814,#20815,#20816,#20817,#20818,#20819,#20820,#20821,#20822,#20823,
#20824,#20825,#20826,#20827,#20828,#20829,#20830,#20831,#20832,#20833,#20834,
#20835,#20836,#20837,#20838,#20839,#20840,#20841,#20842,#20843,#20844,#20845,
#20846,#20847,#20848,#20849,#20850,#20851,#20852,#20853,#20854,#20855,#20856,
#20857,#20858,#20859,#20860,#20861,#20862,#20863,#20864,#20865,#20866,#20867),
(#20868,#20869,#20870,#20871,#20872,#20873,#20874,#20875,#20876,#20877,
#20878,#20879,#20880,#20881,#20882,#20883,#20884,#20885,#20886,#20887,#20888,
#20889,#20890,#20891,#20892,#20893,#20894,#20895,#20896,#20897,#20898,#20899,
#20900,#20901,#20902,#20903,#20904,#20905,#20906,#20907,#20908,#20909,#20910,
#20911,#20912,#20913,#20914,#20915,#20916,#20917,#20918,#20919,#20920,#20921,
#20922,#20923)),.UNSPECIFIED.,.F.,.F.,.F.,(4,4),(4,1,1,1,1,1,1,1,1,1,1,
1,1,1,1,1,1,1,1,1,1,1,1,1,1,1,1,1,1,1,1,1,1,1,1,1,1,1,1,1,1,1,1,1,1,1,1,
1,1,1,1,1,1,4),(0.,0.0642013499338865),(11.8589888623078,12.8454497557128,
13.8319106491178,14.8183715425228,15.8048324359278,16.7912933293328,17.7777542227378,
18.7642151161428,19.7506760095478,20.7371369029528,21.7235977963578,22.7100586897628,
23.6965195831678,24.6829804765728,25.6694413699778,26.6559022633828,27.6423631567878,
28.6288240501928,29.6152849435978,30.6017458370028,31.5882067304078,32.5746676238129,
33.5611285172179,34.5475894106229,35.5340503040279,36.5205111974329,37.5069720908379,
38.4934329842429,39.4798938776479,40.4663547710529,41.4528156644579,42.4392765578629,
43.4257374512679,44.4121983446729,45.3986592380779,46.3851201314829,47.3715810248879,
48.3580419182929,49.3445028116979,50.3309637051029,51.3174245985079,52.3038854919129,
53.2903463853179,54.2768072787229,55.2632681721279,56.2497290655329,57.2361899589379,
58.2226508523429,59.2091117457479,60.1955726391529,61.1820335325579,62.1684944259629,
63.1549553193679,64.1414162127729),.UNSPECIFIED.);
#258=B_SPLINE_SURFACE_WITH_KNOTS('',3,3,((#21140,#21141,#21142,#21143,#21144,
#21145,#21146,#21147,#21148,#21149,#21150,#21151,#21152,#21153,#21154,#21155,
#21156,#21157,#21158,#21159,#21160,#21161,#21162,#21163,#21164,#21165,#21166,
#21167,#21168,#21169,#21170,#21171,#21172,#21173,#21174,#21175,#21176,#21177,
#21178,#21179,#21180,#21181,#21182,#21183,#21184,#21185,#21186,#21187,#21188,
#21189,#21190,#21191,#21192,#21193,#21194,#21195),(#21196,#21197,#21198,
#21199,#21200,#21201,#21202,#21203,#21204,#21205,#21206,#21207,#21208,#21209,
#21210,#21211,#21212,#21213,#21214,#21215,#21216,#21217,#21218,#21219,#21220,
#21221,#21222,#21223,#21224,#21225,#21226,#21227,#21228,#21229,#21230,#21231,
#21232,#21233,#21234,#21235,#21236,#21237,#21238,#21239,#21240,#21241,#21242,
#21243,#21244,#21245,#21246,#21247,#21248,#21249,#21250,#21251),(#21252,
#21253,#21254,#21255,#21256,#21257,#21258,#21259,#21260,#21261,#21262,#21263,
#21264,#21265,#21266,#21267,#21268,#21269,#21270,#21271,#21272,#21273,#21274,
#21275,#21276,#21277,#21278,#21279,#21280,#21281,#21282,#21283,#21284,#21285,
#21286,#21287,#21288,#21289,#21290,#21291,#21292,#21293,#21294,#21295,#21296,
#21297,#21298,#21299,#21300,#21301,#21302,#21303,#21304,#21305,#21306,#21307),
(#21308,#21309,#21310,#21311,#21312,#21313,#21314,#21315,#21316,#21317,
#21318,#21319,#21320,#21321,#21322,#21323,#21324,#21325,#21326,#21327,#21328,
#21329,#21330,#21331,#21332,#21333,#21334,#21335,#21336,#21337,#21338,#21339,
#21340,#21341,#21342,#21343,#21344,#21345,#21346,#21347,#21348,#21349,#21350,
#21351,#21352,#21353,#21354,#21355,#21356,#21357,#21358,#21359,#21360,#21361,
#21362,#21363)),.UNSPECIFIED.,.F.,.F.,.F.,(4,4),(4,1,1,1,1,1,1,1,1,1,1,
1,1,1,1,1,1,1,1,1,1,1,1,1,1,1,1,1,1,1,1,1,1,1,1,1,1,1,1,1,1,1,1,1,1,1,1,
1,1,1,1,1,1,4),(0.,0.0642013499338865),(14.3984001269718,15.3848610203768,
16.3713219137818,17.3577828071868,18.3442437005918,19.3307045939968,20.3171654874019,
21.3036263808069,22.2900872742119,23.2765481676169,24.2630090610219,25.2494699544269,
26.2359308478319,27.2223917412369,28.2088526346419,29.1953135280469,30.1817744214519,
31.1682353148569,32.1546962082619,33.1411571016669,34.1276179950719,35.1140788884769,
36.1005397818819,37.0870006752869,38.0734615686919,39.0599224620969,40.0463833555019,
41.0328442489069,42.0193051423119,43.0057660357169,43.9922269291219,44.9786878225269,
45.9651487159319,46.9516096093369,47.9380705027419,48.9245313961469,49.9109922895519,
50.8974531829569,51.8839140763619,52.8703749697669,53.856835863172,54.843296756577,
55.829757649982,56.816218543387,57.802679436792,58.789140330197,59.775601223602,
60.762062117007,61.748523010412,62.734983903817,63.721444797222,64.707905690627,
65.694366584032,66.680827477437),.UNSPECIFIED.);
#259=B_SPLINE_SURFACE_WITH_KNOTS('',3,3,((#22184,#22185,#22186,#22187,#22188,
#22189,#22190,#22191,#22192,#22193,#22194,#22195,#22196,#22197,#22198,#22199,
#22200,#22201,#22202,#22203,#22204,#22205,#22206,#22207,#22208,#22209,#22210,
#22211,#22212,#22213,#22214,#22215,#22216,#22217,#22218,#22219,#22220,#22221,
#22222,#22223,#22224,#22225,#22226,#22227,#22228,#22229,#22230,#22231,#22232,
#22233,#22234,#22235,#22236,#22237,#22238,#22239),(#22240,#22241,#22242,
#22243,#22244,#22245,#22246,#22247,#22248,#22249,#22250,#22251,#22252,#22253,
#22254,#22255,#22256,#22257,#22258,#22259,#22260,#22261,#22262,#22263,#22264,
#22265,#22266,#22267,#22268,#22269,#22270,#22271,#22272,#22273,#22274,#22275,
#22276,#22277,#22278,#22279,#22280,#22281,#22282,#22283,#22284,#22285,#22286,
#22287,#22288,#22289,#22290,#22291,#22292,#22293,#22294,#22295),(#22296,
#22297,#22298,#22299,#22300,#22301,#22302,#22303,#22304,#22305,#22306,#22307,
#22308,#22309,#22310,#22311,#22312,#22313,#22314,#22315,#22316,#22317,#22318,
#22319,#22320,#22321,#22322,#22323,#22324,#22325,#22326,#22327,#22328,#22329,
#22330,#22331,#22332,#22333,#22334,#22335,#22336,#22337,#22338,#22339,#22340,
#22341,#22342,#22343,#22344,#22345,#22346,#22347,#22348,#22349,#22350,#22351),
(#22352,#22353,#22354,#22355,#22356,#22357,#22358,#22359,#22360,#22361,
#22362,#22363,#22364,#22365,#22366,#22367,#22368,#22369,#22370,#22371,#22372,
#22373,#22374,#22375,#22376,#22377,#22378,#22379,#22380,#22381,#22382,#22383,
#22384,#22385,#22386,#22387,#22388,#22389,#22390,#22391,#22392,#22393,#22394,
#22395,#22396,#22397,#22398,#22399,#22400,#22401,#22402,#22403,#22404,#22405,
#22406,#22407)),.UNSPECIFIED.,.F.,.F.,.F.,(4,4),(4,1,1,1,1,1,1,1,1,1,1,
1,1,1,1,1,1,1,1,1,1,1,1,1,1,1,1,1,1,1,1,1,1,1,1,1,1,1,1,1,1,1,1,1,1,1,1,
1,1,1,1,1,1,4),(0.,0.0642013499338865),(11.8589888623078,12.8454497557128,
13.8319106491178,14.8183715425228,15.8048324359278,16.7912933293328,17.7777542227378,
18.7642151161428,19.7506760095478,20.7371369029528,21.7235977963578,22.7100586897628,
23.6965195831678,24.6829804765728,25.6694413699778,26.6559022633828,27.6423631567879,
28.6288240501929,29.6152849435979,30.6017458370029,31.5882067304079,32.5746676238129,
33.5611285172179,34.5475894106229,35.5340503040279,36.5205111974329,37.5069720908379,
38.4934329842429,39.4798938776479,40.4663547710529,41.4528156644579,42.4392765578629,
43.4257374512679,44.4121983446729,45.3986592380779,46.3851201314829,47.3715810248879,
48.3580419182929,49.3445028116979,50.3309637051029,51.3174245985079,52.3038854919129,
53.2903463853179,54.2768072787229,55.2632681721279,56.2497290655329,57.2361899589379,
58.2226508523429,59.2091117457479,60.1955726391529,61.1820335325579,62.1684944259629,
63.154955319368,64.141416212773),.UNSPECIFIED.);
#260=B_SPLINE_SURFACE_WITH_KNOTS('',3,3,((#22530,#22531,#22532,#22533,#22534,
#22535,#22536,#22537,#22538,#22539,#22540,#22541,#22542,#22543,#22544,#22545,
#22546,#22547,#22548,#22549,#22550,#22551,#22552,#22553,#22554,#22555,#22556,
#22557,#22558,#22559,#22560,#22561,#22562,#22563,#22564,#22565,#22566,#22567,
#22568,#22569,#22570,#22571,#22572,#22573,#22574,#22575,#22576,#22577,#22578,
#22579,#22580,#22581,#22582,#22583,#22584,#22585),(#22586,#22587,#22588,
#22589,#22590,#22591,#22592,#22593,#22594,#22595,#22596,#22597,#22598,#22599,
#22600,#22601,#22602,#22603,#22604,#22605,#22606,#22607,#22608,#22609,#22610,
#22611,#22612,#22613,#22614,#22615,#22616,#22617,#22618,#22619,#22620,#22621,
#22622,#22623,#22624,#22625,#22626,#22627,#22628,#22629,#22630,#22631,#22632,
#22633,#22634,#22635,#22636,#22637,#22638,#22639,#22640,#22641),(#22642,
#22643,#22644,#22645,#22646,#22647,#22648,#22649,#22650,#22651,#22652,#22653,
#22654,#22655,#22656,#22657,#22658,#22659,#22660,#22661,#22662,#22663,#22664,
#22665,#22666,#22667,#22668,#22669,#22670,#22671,#22672,#22673,#22674,#22675,
#22676,#22677,#22678,#22679,#22680,#22681,#22682,#22683,#22684,#22685,#22686,
#22687,#22688,#22689,#22690,#22691,#22692,#22693,#22694,#22695,#22696,#22697),
(#22698,#22699,#22700,#22701,#22702,#22703,#22704,#22705,#22706,#22707,
#22708,#22709,#22710,#22711,#22712,#22713,#22714,#22715,#22716,#22717,#22718,
#22719,#22720,#22721,#22722,#22723,#22724,#22725,#22726,#22727,#22728,#22729,
#22730,#22731,#22732,#22733,#22734,#22735,#22736,#22737,#22738,#22739,#22740,
#22741,#22742,#22743,#22744,#22745,#22746,#22747,#22748,#22749,#22750,#22751,
#22752,#22753)),.UNSPECIFIED.,.F.,.F.,.F.,(4,4),(4,1,1,1,1,1,1,1,1,1,1,
1,1,1,1,1,1,1,1,1,1,1,1,1,1,1,1,1,1,1,1,1,1,1,1,1,1,1,1,1,1,1,1,1,1,1,1,
1,1,1,1,1,1,4),(0.,0.0642013499338865),(14.3984001269718,15.3848610203768,
16.3713219137818,17.3577828071869,18.3442437005919,19.3307045939969,20.3171654874019,
21.3036263808069,22.2900872742119,23.2765481676169,24.2630090610219,25.2494699544269,
26.2359308478319,27.2223917412369,28.2088526346419,29.1953135280469,30.1817744214519,
31.1682353148569,32.1546962082619,33.1411571016669,34.1276179950719,35.1140788884769,
36.1005397818819,37.0870006752869,38.0734615686919,39.0599224620969,40.0463833555019,
41.0328442489069,42.0193051423119,43.0057660357169,43.9922269291219,44.9786878225269,
45.9651487159319,46.9516096093369,47.9380705027419,48.9245313961469,49.9109922895519,
50.8974531829569,51.8839140763619,52.8703749697669,53.856835863172,54.843296756577,
55.829757649982,56.816218543387,57.802679436792,58.789140330197,59.775601223602,
60.762062117007,61.748523010412,62.734983903817,63.721444797222,64.707905690627,
65.694366584032,66.680827477437),.UNSPECIFIED.);
#261=B_SPLINE_SURFACE_WITH_KNOTS('',3,3,((#22895,#22896,#22897,#22898,#22899,
#22900,#22901,#22902,#22903,#22904,#22905,#22906,#22907,#22908,#22909,#22910,
#22911,#22912,#22913,#22914,#22915,#22916,#22917,#22918,#22919,#22920,#22921,
#22922,#22923,#22924,#22925,#22926,#22927,#22928,#22929,#22930,#22931,#22932,
#22933,#22934,#22935,#22936,#22937,#22938,#22939,#22940,#22941,#22942,#22943,
#22944,#22945,#22946,#22947,#22948,#22949,#22950),(#22951,#22952,#22953,
#22954,#22955,#22956,#22957,#22958,#22959,#22960,#22961,#22962,#22963,#22964,
#22965,#22966,#22967,#22968,#22969,#22970,#22971,#22972,#22973,#22974,#22975,
#22976,#22977,#22978,#22979,#22980,#22981,#22982,#22983,#22984,#22985,#22986,
#22987,#22988,#22989,#22990,#22991,#22992,#22993,#22994,#22995,#22996,#22997,
#22998,#22999,#23000,#23001,#23002,#23003,#23004,#23005,#23006),(#23007,
#23008,#23009,#23010,#23011,#23012,#23013,#23014,#23015,#23016,#23017,#23018,
#23019,#23020,#23021,#23022,#23023,#23024,#23025,#23026,#23027,#23028,#23029,
#23030,#23031,#23032,#23033,#23034,#23035,#23036,#23037,#23038,#23039,#23040,
#23041,#23042,#23043,#23044,#23045,#23046,#23047,#23048,#23049,#23050,#23051,
#23052,#23053,#23054,#23055,#23056,#23057,#23058,#23059,#23060,#23061,#23062),
(#23063,#23064,#23065,#23066,#23067,#23068,#23069,#23070,#23071,#23072,
#23073,#23074,#23075,#23076,#23077,#23078,#23079,#23080,#23081,#23082,#23083,
#23084,#23085,#23086,#23087,#23088,#23089,#23090,#23091,#23092,#23093,#23094,
#23095,#23096,#23097,#23098,#23099,#23100,#23101,#23102,#23103,#23104,#23105,
#23106,#23107,#23108,#23109,#23110,#23111,#23112,#23113,#23114,#23115,#23116,
#23117,#23118)),.UNSPECIFIED.,.F.,.F.,.F.,(4,4),(4,1,1,1,1,1,1,1,1,1,1,
1,1,1,1,1,1,1,1,1,1,1,1,1,1,1,1,1,1,1,1,1,1,1,1,1,1,1,1,1,1,1,1,1,1,1,1,
1,1,1,1,1,1,4),(0.,0.0642013499338865),(11.8589888623078,12.8454497557128,
13.8319106491178,14.8183715425228,15.8048324359278,16.7912933293328,17.7777542227378,
18.7642151161428,19.7506760095478,20.7371369029528,21.7235977963578,22.7100586897628,
23.6965195831678,24.6829804765728,25.6694413699778,26.6559022633828,27.6423631567878,
28.6288240501928,29.6152849435978,30.6017458370028,31.5882067304078,32.5746676238129,
33.5611285172179,34.5475894106229,35.5340503040279,36.5205111974329,37.5069720908379,
38.4934329842429,39.4798938776479,40.4663547710529,41.4528156644579,42.4392765578629,
43.4257374512679,44.4121983446729,45.3986592380779,46.3851201314829,47.3715810248879,
48.3580419182929,49.3445028116979,50.3309637051029,51.3174245985079,52.3038854919129,
53.2903463853179,54.2768072787229,55.2632681721279,56.2497290655329,57.2361899589379,
58.2226508523429,59.2091117457479,60.1955726391529,61.1820335325579,62.1684944259629,
63.1549553193679,64.1414162127729),.UNSPECIFIED.);
#262=B_SPLINE_SURFACE_WITH_KNOTS('',3,3,((#23241,#23242,#23243,#23244,#23245,
#23246,#23247,#23248,#23249,#23250,#23251,#23252,#23253,#23254,#23255,#23256,
#23257,#23258,#23259,#23260,#23261,#23262,#23263,#23264,#23265,#23266,#23267,
#23268,#23269,#23270,#23271,#23272,#23273,#23274,#23275,#23276,#23277,#23278,
#23279,#23280,#23281,#23282,#23283,#23284,#23285,#23286,#23287,#23288,#23289,
#23290,#23291,#23292,#23293,#23294,#23295,#23296),(#23297,#23298,#23299,
#23300,#23301,#23302,#23303,#23304,#23305,#23306,#23307,#23308,#23309,#23310,
#23311,#23312,#23313,#23314,#23315,#23316,#23317,#23318,#23319,#23320,#23321,
#23322,#23323,#23324,#23325,#23326,#23327,#23328,#23329,#23330,#23331,#23332,
#23333,#23334,#23335,#23336,#23337,#23338,#23339,#23340,#23341,#23342,#23343,
#23344,#23345,#23346,#23347,#23348,#23349,#23350,#23351,#23352),(#23353,
#23354,#23355,#23356,#23357,#23358,#23359,#23360,#23361,#23362,#23363,#23364,
#23365,#23366,#23367,#23368,#23369,#23370,#23371,#23372,#23373,#23374,#23375,
#23376,#23377,#23378,#23379,#23380,#23381,#23382,#23383,#23384,#23385,#23386,
#23387,#23388,#23389,#23390,#23391,#23392,#23393,#23394,#23395,#23396,#23397,
#23398,#23399,#23400,#23401,#23402,#23403,#23404,#23405,#23406,#23407,#23408),
(#23409,#23410,#23411,#23412,#23413,#23414,#23415,#23416,#23417,#23418,
#23419,#23420,#23421,#23422,#23423,#23424,#23425,#23426,#23427,#23428,#23429,
#23430,#23431,#23432,#23433,#23434,#23435,#23436,#23437,#23438,#23439,#23440,
#23441,#23442,#23443,#23444,#23445,#23446,#23447,#23448,#23449,#23450,#23451,
#23452,#23453,#23454,#23455,#23456,#23457,#23458,#23459,#23460,#23461,#23462,
#23463,#23464)),.UNSPECIFIED.,.F.,.F.,.F.,(4,4),(4,1,1,1,1,1,1,1,1,1,1,
1,1,1,1,1,1,1,1,1,1,1,1,1,1,1,1,1,1,1,1,1,1,1,1,1,1,1,1,1,1,1,1,1,1,1,1,
1,1,1,1,1,1,4),(0.,0.0642013499338865),(14.3984001269718,15.3848610203768,
16.3713219137818,17.3577828071868,18.3442437005918,19.3307045939968,20.3171654874019,
21.3036263808069,22.2900872742119,23.2765481676169,24.2630090610219,25.2494699544269,
26.2359308478319,27.2223917412369,28.2088526346419,29.1953135280469,30.1817744214519,
31.1682353148569,32.1546962082619,33.1411571016669,34.1276179950719,35.1140788884769,
36.1005397818819,37.0870006752869,38.0734615686919,39.0599224620969,40.0463833555019,
41.0328442489069,42.0193051423119,43.0057660357169,43.9922269291219,44.9786878225269,
45.9651487159319,46.9516096093369,47.9380705027419,48.9245313961469,49.9109922895519,
50.8974531829569,51.8839140763619,52.8703749697669,53.856835863172,54.843296756577,
55.829757649982,56.816218543387,57.802679436792,58.789140330197,59.775601223602,
60.762062117007,61.748523010412,62.734983903817,63.721444797222,64.707905690627,
65.694366584032,66.680827477437),.UNSPECIFIED.);
#263=B_SPLINE_SURFACE_WITH_KNOTS('',3,3,((#23606,#23607,#23608,#23609,#23610,
#23611,#23612,#23613,#23614,#23615,#23616,#23617,#23618,#23619,#23620,#23621,
#23622,#23623,#23624,#23625,#23626,#23627,#23628,#23629,#23630,#23631,#23632,
#23633,#23634,#23635,#23636,#23637,#23638,#23639,#23640,#23641,#23642,#23643,
#23644,#23645,#23646,#23647,#23648,#23649,#23650,#23651,#23652,#23653,#23654,
#23655,#23656,#23657,#23658,#23659,#23660,#23661),(#23662,#23663,#23664,
#23665,#23666,#23667,#23668,#23669,#23670,#23671,#23672,#23673,#23674,#23675,
#23676,#23677,#23678,#23679,#23680,#23681,#23682,#23683,#23684,#23685,#23686,
#23687,#23688,#23689,#23690,#23691,#23692,#23693,#23694,#23695,#23696,#23697,
#23698,#23699,#23700,#23701,#23702,#23703,#23704,#23705,#23706,#23707,#23708,
#23709,#23710,#23711,#23712,#23713,#23714,#23715,#23716,#23717),(#23718,
#23719,#23720,#23721,#23722,#23723,#23724,#23725,#23726,#23727,#23728,#23729,
#23730,#23731,#23732,#23733,#23734,#23735,#23736,#23737,#23738,#23739,#23740,
#23741,#23742,#23743,#23744,#23745,#23746,#23747,#23748,#23749,#23750,#23751,
#23752,#23753,#23754,#23755,#23756,#23757,#23758,#23759,#23760,#23761,#23762,
#23763,#23764,#23765,#23766,#23767,#23768,#23769,#23770,#23771,#23772,#23773),
(#23774,#23775,#23776,#23777,#23778,#23779,#23780,#23781,#23782,#23783,
#23784,#23785,#23786,#23787,#23788,#23789,#23790,#23791,#23792,#23793,#23794,
#23795,#23796,#23797,#23798,#23799,#23800,#23801,#23802,#23803,#23804,#23805,
#23806,#23807,#23808,#23809,#23810,#23811,#23812,#23813,#23814,#23815,#23816,
#23817,#23818,#23819,#23820,#23821,#23822,#23823,#23824,#23825,#23826,#23827,
#23828,#23829)),.UNSPECIFIED.,.F.,.F.,.F.,(4,4),(4,1,1,1,1,1,1,1,1,1,1,
1,1,1,1,1,1,1,1,1,1,1,1,1,1,1,1,1,1,1,1,1,1,1,1,1,1,1,1,1,1,1,1,1,1,1,1,
1,1,1,1,1,1,4),(0.,0.0642013499338865),(11.8589888623078,12.8454497557128,
13.8319106491178,14.8183715425228,15.8048324359278,16.7912933293328,17.7777542227378,
18.7642151161428,19.7506760095478,20.7371369029528,21.7235977963578,22.7100586897628,
23.6965195831678,24.6829804765728,25.6694413699778,26.6559022633828,27.6423631567879,
28.6288240501929,29.6152849435979,30.6017458370029,31.5882067304079,32.5746676238129,
33.5611285172179,34.5475894106229,35.5340503040279,36.5205111974329,37.5069720908379,
38.4934329842429,39.4798938776479,40.4663547710529,41.4528156644579,42.4392765578629,
43.4257374512679,44.4121983446729,45.3986592380779,46.3851201314829,47.3715810248879,
48.3580419182929,49.3445028116979,50.3309637051029,51.3174245985079,52.3038854919129,
53.2903463853179,54.2768072787229,55.2632681721279,56.2497290655329,57.2361899589379,
58.2226508523429,59.2091117457479,60.1955726391529,61.1820335325579,62.1684944259629,
63.154955319368,64.141416212773),.UNSPECIFIED.);
#264=B_SPLINE_SURFACE_WITH_KNOTS('',3,3,((#23952,#23953,#23954,#23955,#23956,
#23957,#23958,#23959,#23960,#23961,#23962,#23963,#23964,#23965,#23966,#23967,
#23968,#23969,#23970,#23971,#23972,#23973,#23974,#23975,#23976,#23977,#23978,
#23979,#23980,#23981,#23982,#23983,#23984,#23985,#23986,#23987,#23988,#23989,
#23990,#23991,#23992,#23993,#23994,#23995,#23996,#23997,#23998,#23999,#24000,
#24001,#24002,#24003,#24004,#24005,#24006,#24007),(#24008,#24009,#24010,
#24011,#24012,#24013,#24014,#24015,#24016,#24017,#24018,#24019,#24020,#24021,
#24022,#24023,#24024,#24025,#24026,#24027,#24028,#24029,#24030,#24031,#24032,
#24033,#24034,#24035,#24036,#24037,#24038,#24039,#24040,#24041,#24042,#24043,
#24044,#24045,#24046,#24047,#24048,#24049,#24050,#24051,#24052,#24053,#24054,
#24055,#24056,#24057,#24058,#24059,#24060,#24061,#24062,#24063),(#24064,
#24065,#24066,#24067,#24068,#24069,#24070,#24071,#24072,#24073,#24074,#24075,
#24076,#24077,#24078,#24079,#24080,#24081,#24082,#24083,#24084,#24085,#24086,
#24087,#24088,#24089,#24090,#24091,#24092,#24093,#24094,#24095,#24096,#24097,
#24098,#24099,#24100,#24101,#24102,#24103,#24104,#24105,#24106,#24107,#24108,
#24109,#24110,#24111,#24112,#24113,#24114,#24115,#24116,#24117,#24118,#24119),
(#24120,#24121,#24122,#24123,#24124,#24125,#24126,#24127,#24128,#24129,
#24130,#24131,#24132,#24133,#24134,#24135,#24136,#24137,#24138,#24139,#24140,
#24141,#24142,#24143,#24144,#24145,#24146,#24147,#24148,#24149,#24150,#24151,
#24152,#24153,#24154,#24155,#24156,#24157,#24158,#24159,#24160,#24161,#24162,
#24163,#24164,#24165,#24166,#24167,#24168,#24169,#24170,#24171,#24172,#24173,
#24174,#24175)),.UNSPECIFIED.,.F.,.F.,.F.,(4,4),(4,1,1,1,1,1,1,1,1,1,1,
1,1,1,1,1,1,1,1,1,1,1,1,1,1,1,1,1,1,1,1,1,1,1,1,1,1,1,1,1,1,1,1,1,1,1,1,
1,1,1,1,1,1,4),(0.,0.0642013499338865),(14.3984001269718,15.3848610203768,
16.3713219137818,17.3577828071869,18.3442437005919,19.3307045939969,20.3171654874019,
21.3036263808069,22.2900872742119,23.2765481676169,24.2630090610219,25.2494699544269,
26.2359308478319,27.2223917412369,28.2088526346419,29.1953135280469,30.1817744214519,
31.1682353148569,32.1546962082619,33.1411571016669,34.1276179950719,35.1140788884769,
36.1005397818819,37.0870006752869,38.0734615686919,39.0599224620969,40.0463833555019,
41.0328442489069,42.0193051423119,43.0057660357169,43.9922269291219,44.9786878225269,
45.9651487159319,46.9516096093369,47.9380705027419,48.9245313961469,49.9109922895519,
50.8974531829569,51.8839140763619,52.8703749697669,53.856835863172,54.843296756577,
55.829757649982,56.816218543387,57.802679436792,58.789140330197,59.775601223602,
60.762062117007,61.748523010412,62.734983903817,63.721444797222,64.707905690627,
65.694366584032,66.680827477437),.UNSPECIFIED.);
#265=B_SPLINE_SURFACE_WITH_KNOTS('',3,3,((#26409,#26410,#26411,#26412,#26413,
#26414,#26415,#26416,#26417,#26418,#26419,#26420,#26421,#26422,#26423,#26424,
#26425,#26426,#26427,#26428,#26429,#26430,#26431,#26432,#26433,#26434,#26435,
#26436,#26437,#26438,#26439,#26440,#26441,#26442,#26443,#26444,#26445,#26446,
#26447,#26448,#26449,#26450,#26451,#26452,#26453,#26454,#26455,#26456,#26457,
#26458,#26459,#26460,#26461,#26462,#26463,#26464,#26465,#26466,#26467,#26468,
#26469,#26470,#26471,#26472,#26473,#26474,#26475,#26476,#26477,#26478,#26479,
#26480,#26481,#26482,#26483,#26484,#26485,#26486,#26487,#26488,#26489,#26490,
#26491,#26492,#26493,#26494,#26495,#26496,#26497,#26498,#26499,#26500,#26501,
#26502,#26503,#26504,#26505,#26506,#26507,#26508,#26509,#26510,#26511,#26512,
#26513,#26514,#26515,#26516,#26517,#26518,#26519,#26520,#26521,#26522,#26523,
#26524,#26525,#26526,#26527,#26528,#26529,#26530,#26531,#26532,#26533,#26534,
#26535,#26536,#26537,#26538,#26539,#26540,#26541,#26542,#26543,#26544,#26545,
#26546,#26547,#26548,#26549,#26550,#26551,#26552,#26553,#26554,#26555,#26556,
#26557,#26558,#26559,#26560,#26561,#26562,#26563,#26564,#26565,#26566),
(#26567,#26568,#26569,#26570,#26571,#26572,#26573,#26574,#26575,#26576,
#26577,#26578,#26579,#26580,#26581,#26582,#26583,#26584,#26585,#26586,#26587,
#26588,#26589,#26590,#26591,#26592,#26593,#26594,#26595,#26596,#26597,#26598,
#26599,#26600,#26601,#26602,#26603,#26604,#26605,#26606,#26607,#26608,#26609,
#26610,#26611,#26612,#26613,#26614,#26615,#26616,#26617,#26618,#26619,#26620,
#26621,#26622,#26623,#26624,#26625,#26626,#26627,#26628,#26629,#26630,#26631,
#26632,#26633,#26634,#26635,#26636,#26637,#26638,#26639,#26640,#26641,#26642,
#26643,#26644,#26645,#26646,#26647,#26648,#26649,#26650,#26651,#26652,#26653,
#26654,#26655,#26656,#26657,#26658,#26659,#26660,#26661,#26662,#26663,#26664,
#26665,#26666,#26667,#26668,#26669,#26670,#26671,#26672,#26673,#26674,#26675,
#26676,#26677,#26678,#26679,#26680,#26681,#26682,#26683,#26684,#26685,#26686,
#26687,#26688,#26689,#26690,#26691,#26692,#26693,#26694,#26695,#26696,#26697,
#26698,#26699,#26700,#26701,#26702,#26703,#26704,#26705,#26706,#26707,#26708,
#26709,#26710,#26711,#26712,#26713,#26714,#26715,#26716,#26717,#26718,#26719,
#26720,#26721,#26722,#26723,#26724),(#26725,#26726,#26727,#26728,#26729,
#26730,#26731,#26732,#26733,#26734,#26735,#26736,#26737,#26738,#26739,#26740,
#26741,#26742,#26743,#26744,#26745,#26746,#26747,#26748,#26749,#26750,#26751,
#26752,#26753,#26754,#26755,#26756,#26757,#26758,#26759,#26760,#26761,#26762,
#26763,#26764,#26765,#26766,#26767,#26768,#26769,#26770,#26771,#26772,#26773,
#26774,#26775,#26776,#26777,#26778,#26779,#26780,#26781,#26782,#26783,#26784,
#26785,#26786,#26787,#26788,#26789,#26790,#26791,#26792,#26793,#26794,#26795,
#26796,#26797,#26798,#26799,#26800,#26801,#26802,#26803,#26804,#26805,#26806,
#26807,#26808,#26809,#26810,#26811,#26812,#26813,#26814,#26815,#26816,#26817,
#26818,#26819,#26820,#26821,#26822,#26823,#26824,#26825,#26826,#26827,#26828,
#26829,#26830,#26831,#26832,#26833,#26834,#26835,#26836,#26837,#26838,#26839,
#26840,#26841,#26842,#26843,#26844,#26845,#26846,#26847,#26848,#26849,#26850,
#26851,#26852,#26853,#26854,#26855,#26856,#26857,#26858,#26859,#26860,#26861,
#26862,#26863,#26864,#26865,#26866,#26867,#26868,#26869,#26870,#26871,#26872,
#26873,#26874,#26875,#26876,#26877,#26878,#26879,#26880,#26881,#26882),
(#26883,#26884,#26885,#26886,#26887,#26888,#26889,#26890,#26891,#26892,
#26893,#26894,#26895,#26896,#26897,#26898,#26899,#26900,#26901,#26902,#26903,
#26904,#26905,#26906,#26907,#26908,#26909,#26910,#26911,#26912,#26913,#26914,
#26915,#26916,#26917,#26918,#26919,#26920,#26921,#26922,#26923,#26924,#26925,
#26926,#26927,#26928,#26929,#26930,#26931,#26932,#26933,#26934,#26935,#26936,
#26937,#26938,#26939,#26940,#26941,#26942,#26943,#26944,#26945,#26946,#26947,
#26948,#26949,#26950,#26951,#26952,#26953,#26954,#26955,#26956,#26957,#26958,
#26959,#26960,#26961,#26962,#26963,#26964,#26965,#26966,#26967,#26968,#26969,
#26970,#26971,#26972,#26973,#26974,#26975,#26976,#26977,#26978,#26979,#26980,
#26981,#26982,#26983,#26984,#26985,#26986,#26987,#26988,#26989,#26990,#26991,
#26992,#26993,#26994,#26995,#26996,#26997,#26998,#26999,#27000,#27001,#27002,
#27003,#27004,#27005,#27006,#27007,#27008,#27009,#27010,#27011,#27012,#27013,
#27014,#27015,#27016,#27017,#27018,#27019,#27020,#27021,#27022,#27023,#27024,
#27025,#27026,#27027,#27028,#27029,#27030,#27031,#27032,#27033,#27034,#27035,
#27036,#27037,#27038,#27039,#27040)),.UNSPECIFIED.,.F.,.F.,.F.,(4,4),(4,
1,1,1,1,1,1,1,1,1,1,1,1,1,1,1,1,1,1,1,1,1,1,1,1,1,1,1,1,1,1,1,1,1,1,1,1,
1,1,1,1,1,1,1,1,1,1,1,1,1,1,1,1,1,1,1,1,1,1,1,1,1,1,1,1,1,1,1,1,1,1,1,1,
1,1,1,1,1,1,1,1,1,1,1,1,1,1,1,1,1,1,1,1,1,1,1,1,1,1,1,1,1,1,1,1,1,1,1,1,
1,1,1,1,1,1,1,1,1,1,1,1,1,1,1,1,1,1,1,1,1,1,1,1,1,1,1,1,1,1,1,1,1,1,1,1,
1,1,1,1,1,1,1,1,1,1,4),(0.,0.0658467982010769),(11.6150328478184,12.61338032228,
13.6117277967416,14.6100752712031,15.6084227456647,16.6067702201263,17.6051176945879,
18.6034651690495,19.6018126435111,20.6001601179726,21.5985075924342,22.5968550668958,
23.5952025413574,24.593550015819,25.5918974902806,26.5902449647422,27.5885924392037,
28.5869399136653,29.5852873881269,30.5836348625885,31.5819823370501,32.5803298115117,
33.5786772859732,34.5770247604348,35.5753722348964,36.573719709358,37.5720671838196,
38.5704146582812,39.5687621327428,40.5671096072043,41.5654570816659,42.5638045561275,
43.5621520305891,44.5604995050507,45.5588469795123,46.5571944539738,47.5555419284354,
48.553889402897,49.5522368773586,50.5505843518202,51.5489318262818,52.5472793007434,
53.545626775205,54.5439742496665,55.5423217241281,56.5406691985897,57.5390166730513,
58.5373641475129,59.5357116219745,60.534059096436,61.5324065708976,62.5307540453592,
63.5291015198208,64.5274489942824,65.525796468744,66.5241439432056,67.5224914176671,
68.5208388921287,69.5191863665903,70.5175338410519,71.5158813155135,72.5142287899751,
73.5125762644366,74.5109237388982,75.5092712133598,76.5076186878214,77.505966162283,
78.5043136367446,79.5026611112062,80.5010085856677,81.4993560601293,82.4977035345909,
83.4960510090525,84.4943984835141,85.4927459579757,86.4910934324373,87.4894409068988,
88.4877883813604,89.486135855822,90.4844833302836,91.4828308047452,92.4811782792068,
93.4795257536684,94.4778732281299,95.4762207025915,96.4745681770531,97.4729156515147,
98.4712631259763,99.4696106004379,100.467958074899,101.466305549361,102.464653023823,
103.463000498284,104.461347972746,105.459695447207,106.458042921669,107.456390396131,
108.454737870592,109.453085345054,110.451432819515,111.449780293977,112.448127768438,
113.4464752429,114.444822717362,115.443170191823,116.441517666285,117.439865140746,
118.438212615208,119.43656008967,120.434907564131,121.433255038593,122.431602513054,
123.429949987516,124.428297461977,125.426644936439,126.424992410901,127.423339885362,
128.421687359824,129.420034834285,130.418382308747,131.416729783209,132.41507725767,
133.413424732132,134.411772206593,135.410119681055,136.408467155516,137.406814629978,
138.40516210444,139.403509578901,140.401857053363,141.400204527824,142.398552002286,
143.396899476748,144.395246951209,145.393594425671,146.391941900132,147.390289374594,
148.388636849056,149.386984323517,150.385331797979,151.38367927244,152.382026746902,
153.380374221363,154.378721695825,155.377069170287,156.375416644748,157.37376411921,
158.372111593671,159.370459068133,160.368806542595,161.367154017056,162.365501491518,
163.363848965979,164.362196440441,165.360543914902,166.358891389364),
 .UNSPECIFIED.);
#266=B_SPLINE_SURFACE_WITH_KNOTS('',3,3,((#27178,#27179,#27180,#27181,#27182,
#27183,#27184,#27185,#27186,#27187,#27188,#27189,#27190,#27191,#27192,#27193,
#27194,#27195,#27196,#27197,#27198,#27199,#27200,#27201,#27202,#27203,#27204,
#27205,#27206,#27207,#27208,#27209,#27210,#27211,#27212,#27213,#27214,#27215,
#27216,#27217,#27218,#27219,#27220,#27221,#27222,#27223,#27224,#27225,#27226,
#27227,#27228,#27229,#27230,#27231,#27232,#27233,#27234,#27235,#27236,#27237,
#27238,#27239,#27240,#27241,#27242,#27243,#27244,#27245,#27246,#27247,#27248,
#27249,#27250,#27251,#27252,#27253,#27254,#27255,#27256,#27257,#27258,#27259,
#27260,#27261,#27262,#27263,#27264,#27265,#27266,#27267,#27268,#27269,#27270,
#27271,#27272,#27273,#27274,#27275,#27276,#27277,#27278,#27279,#27280,#27281,
#27282,#27283,#27284,#27285,#27286,#27287,#27288,#27289,#27290,#27291,#27292,
#27293,#27294,#27295,#27296,#27297,#27298,#27299,#27300,#27301,#27302,#27303,
#27304,#27305,#27306,#27307,#27308,#27309,#27310,#27311,#27312,#27313,#27314,
#27315,#27316,#27317,#27318,#27319,#27320,#27321,#27322,#27323,#27324,#27325,
#27326,#27327,#27328,#27329,#27330,#27331,#27332,#27333,#27334,#27335,#27336,
#27337),(#27338,#27339,#27340,#27341,#27342,#27343,#27344,#27345,#27346,
#27347,#27348,#27349,#27350,#27351,#27352,#27353,#27354,#27355,#27356,#27357,
#27358,#27359,#27360,#27361,#27362,#27363,#27364,#27365,#27366,#27367,#27368,
#27369,#27370,#27371,#27372,#27373,#27374,#27375,#27376,#27377,#27378,#27379,
#27380,#27381,#27382,#27383,#27384,#27385,#27386,#27387,#27388,#27389,#27390,
#27391,#27392,#27393,#27394,#27395,#27396,#27397,#27398,#27399,#27400,#27401,
#27402,#27403,#27404,#27405,#27406,#27407,#27408,#27409,#27410,#27411,#27412,
#27413,#27414,#27415,#27416,#27417,#27418,#27419,#27420,#27421,#27422,#27423,
#27424,#27425,#27426,#27427,#27428,#27429,#27430,#27431,#27432,#27433,#27434,
#27435,#27436,#27437,#27438,#27439,#27440,#27441,#27442,#27443,#27444,#27445,
#27446,#27447,#27448,#27449,#27450,#27451,#27452,#27453,#27454,#27455,#27456,
#27457,#27458,#27459,#27460,#27461,#27462,#27463,#27464,#27465,#27466,#27467,
#27468,#27469,#27470,#27471,#27472,#27473,#27474,#27475,#27476,#27477,#27478,
#27479,#27480,#27481,#27482,#27483,#27484,#27485,#27486,#27487,#27488,#27489,
#27490,#27491,#27492,#27493,#27494,#27495,#27496,#27497),(#27498,#27499,
#27500,#27501,#27502,#27503,#27504,#27505,#27506,#27507,#27508,#27509,#27510,
#27511,#27512,#27513,#27514,#27515,#27516,#27517,#27518,#27519,#27520,#27521,
#27522,#27523,#27524,#27525,#27526,#27527,#27528,#27529,#27530,#27531,#27532,
#27533,#27534,#27535,#27536,#27537,#27538,#27539,#27540,#27541,#27542,#27543,
#27544,#27545,#27546,#27547,#27548,#27549,#27550,#27551,#27552,#27553,#27554,
#27555,#27556,#27557,#27558,#27559,#27560,#27561,#27562,#27563,#27564,#27565,
#27566,#27567,#27568,#27569,#27570,#27571,#27572,#27573,#27574,#27575,#27576,
#27577,#27578,#27579,#27580,#27581,#27582,#27583,#27584,#27585,#27586,#27587,
#27588,#27589,#27590,#27591,#27592,#27593,#27594,#27595,#27596,#27597,#27598,
#27599,#27600,#27601,#27602,#27603,#27604,#27605,#27606,#27607,#27608,#27609,
#27610,#27611,#27612,#27613,#27614,#27615,#27616,#27617,#27618,#27619,#27620,
#27621,#27622,#27623,#27624,#27625,#27626,#27627,#27628,#27629,#27630,#27631,
#27632,#27633,#27634,#27635,#27636,#27637,#27638,#27639,#27640,#27641,#27642,
#27643,#27644,#27645,#27646,#27647,#27648,#27649,#27650,#27651,#27652,#27653,
#27654,#27655,#27656,#27657),(#27658,#27659,#27660,#27661,#27662,#27663,
#27664,#27665,#27666,#27667,#27668,#27669,#27670,#27671,#27672,#27673,#27674,
#27675,#27676,#27677,#27678,#27679,#27680,#27681,#27682,#27683,#27684,#27685,
#27686,#27687,#27688,#27689,#27690,#27691,#27692,#27693,#27694,#27695,#27696,
#27697,#27698,#27699,#27700,#27701,#27702,#27703,#27704,#27705,#27706,#27707,
#27708,#27709,#27710,#27711,#27712,#27713,#27714,#27715,#27716,#27717,#27718,
#27719,#27720,#27721,#27722,#27723,#27724,#27725,#27726,#27727,#27728,#27729,
#27730,#27731,#27732,#27733,#27734,#27735,#27736,#27737,#27738,#27739,#27740,
#27741,#27742,#27743,#27744,#27745,#27746,#27747,#27748,#27749,#27750,#27751,
#27752,#27753,#27754,#27755,#27756,#27757,#27758,#27759,#27760,#27761,#27762,
#27763,#27764,#27765,#27766,#27767,#27768,#27769,#27770,#27771,#27772,#27773,
#27774,#27775,#27776,#27777,#27778,#27779,#27780,#27781,#27782,#27783,#27784,
#27785,#27786,#27787,#27788,#27789,#27790,#27791,#27792,#27793,#27794,#27795,
#27796,#27797,#27798,#27799,#27800,#27801,#27802,#27803,#27804,#27805,#27806,
#27807,#27808,#27809,#27810,#27811,#27812,#27813,#27814,#27815,#27816,#27817)),
 .UNSPECIFIED.,.F.,.F.,.F.,(4,4),(4,1,1,1,1,1,1,1,1,1,1,1,1,1,1,1,1,1,1,
1,1,1,1,1,1,1,1,1,1,1,1,1,1,1,1,1,1,1,1,1,1,1,1,1,1,1,1,1,1,1,1,1,1,1,1,
1,1,1,1,1,1,1,1,1,1,1,1,1,1,1,1,1,1,1,1,1,1,1,1,1,1,1,1,1,1,1,1,1,1,1,1,
1,1,1,1,1,1,1,1,1,1,1,1,1,1,1,1,1,1,1,1,1,1,1,1,1,1,1,1,1,1,1,1,1,1,1,1,
1,1,1,1,1,1,1,1,1,1,1,1,1,1,1,1,1,1,1,1,1,1,1,1,1,1,1,1,1,1,4),(0.,0.0658467982010769),
(8.30747755240114,9.30628326397092,10.3050889755407,11.3038946871105,12.3027003986802,
13.30150611025,14.3003118218198,15.2991175333896,16.2979232449593,17.2967289565291,
18.2955346680989,19.2943403796687,20.2931460912385,21.2919518028082,22.290757514378,
23.2895632259478,24.2883689375176,25.2871746490873,26.2859803606571,27.2847860722269,
28.2835917837967,29.2823974953664,30.2812032069362,31.280008918506,32.2788146300758,
33.2776203416455,34.2764260532153,35.2752317647851,36.2740374763549,37.2728431879246,
38.2716488994944,39.2704546110642,40.269260322634,41.2680660342037,42.2668717457735,
43.2656774573433,44.2644831689131,45.2632888804829,46.2620945920526,47.2609003036224,
48.2597060151922,49.258511726762,50.2573174383317,51.2561231499015,52.2549288614713,
53.2537345730411,54.2525402846108,55.2513459961806,56.2501517077504,57.2489574193202,
58.2477631308899,59.2465688424597,60.2453745540295,61.2441802655993,62.242985977169,
63.2417916887388,64.2405974003086,65.2394031118784,66.2382088234481,67.2370145350179,
68.2358202465877,69.2346259581575,70.2334316697272,71.232237381297,72.2310430928668,
73.2298488044366,74.2286545160063,75.2274602275761,76.2262659391459,77.2250716507157,
78.2238773622854,79.2226830738552,80.221488785425,81.2202944969948,82.2191002085646,
83.2179059201343,84.2167116317041,85.2155173432739,86.2143230548436,87.2131287664134,
88.2119344779832,89.210740189553,90.2095459011228,91.2083516126925,92.2071573242623,
93.2059630358321,94.2047687474019,95.2035744589716,96.2023801705414,97.2011858821112,
98.199991593681,99.1987973052507,100.197603016821,101.19640872839,102.19521443996,
103.19402015153,104.1928258631,105.191631574669,106.190437286239,107.189242997809,
108.188048709379,109.186854420948,110.185660132518,111.184465844088,112.183271555658,
113.182077267228,114.180882978797,115.179688690367,116.178494401937,117.177300113507,
118.176105825076,119.174911536646,120.173717248216,121.172522959786,122.171328671356,
123.170134382925,124.168940094495,125.167745806065,126.166551517635,127.165357229204,
128.164162940774,129.162968652344,130.161774363914,131.160580075484,132.159385787053,
133.158191498623,134.156997210193,135.155802921763,136.154608633332,137.153414344902,
138.152220056472,139.151025768042,140.149831479612,141.148637191181,142.147442902751,
143.146248614321,144.145054325891,145.14386003746,146.14266574903,147.1414714606,
148.14027717217,149.13908288374,150.137888595309,151.136694306879,152.135500018449,
153.134305730019,154.133111441588,155.131917153158,156.130722864728,157.129528576298,
158.128334287868,159.127139999437,160.125945711007,161.124751422577,162.123557134147,
163.122362845716,164.121168557286,165.119974268856),.UNSPECIFIED.);
#267=B_SPLINE_SURFACE_WITH_KNOTS('',3,3,((#36107,#36108,#36109,#36110,#36111,
#36112,#36113,#36114,#36115,#36116,#36117,#36118,#36119,#36120,#36121,#36122,
#36123,#36124,#36125,#36126,#36127,#36128,#36129,#36130,#36131,#36132,#36133,
#36134,#36135,#36136,#36137,#36138,#36139,#36140,#36141,#36142,#36143,#36144,
#36145,#36146,#36147,#36148,#36149,#36150,#36151,#36152,#36153,#36154,#36155,
#36156,#36157,#36158,#36159,#36160,#36161,#36162,#36163,#36164,#36165,#36166,
#36167,#36168,#36169,#36170,#36171,#36172,#36173,#36174,#36175,#36176,#36177,
#36178,#36179,#36180,#36181,#36182,#36183,#36184,#36185,#36186,#36187,#36188,
#36189,#36190,#36191,#36192,#36193,#36194,#36195,#36196,#36197,#36198,#36199,
#36200,#36201,#36202,#36203,#36204,#36205,#36206,#36207,#36208,#36209,#36210,
#36211,#36212,#36213,#36214,#36215,#36216,#36217,#36218,#36219,#36220,#36221,
#36222,#36223,#36224,#36225,#36226,#36227,#36228,#36229,#36230,#36231,#36232,
#36233,#36234,#36235,#36236,#36237,#36238,#36239,#36240,#36241,#36242,#36243,
#36244,#36245,#36246,#36247,#36248,#36249,#36250,#36251,#36252,#36253,#36254,
#36255,#36256,#36257,#36258,#36259,#36260,#36261,#36262,#36263,#36264,#36265,
#36266,#36267,#36268,#36269,#36270,#36271,#36272,#36273,#36274,#36275,#36276,
#36277,#36278,#36279,#36280,#36281,#36282,#36283,#36284,#36285,#36286,#36287,
#36288,#36289,#36290,#36291,#36292,#36293,#36294,#36295,#36296,#36297,#36298,
#36299,#36300,#36301,#36302,#36303,#36304,#36305,#36306,#36307,#36308,#36309,
#36310,#36311,#36312,#36313,#36314,#36315,#36316,#36317,#36318,#36319,#36320,
#36321,#36322,#36323,#36324,#36325,#36326,#36327,#36328,#36329,#36330,#36331,
#36332,#36333,#36334,#36335,#36336,#36337,#36338,#36339,#36340,#36341,#36342,
#36343,#36344,#36345,#36346,#36347,#36348,#36349,#36350,#36351,#36352,#36353,
#36354,#36355,#36356,#36357,#36358,#36359,#36360,#36361,#36362,#36363,#36364,
#36365,#36366,#36367,#36368,#36369,#36370,#36371,#36372,#36373,#36374,#36375,
#36376,#36377,#36378,#36379,#36380,#36381,#36382,#36383,#36384,#36385,#36386,
#36387,#36388,#36389,#36390,#36391,#36392,#36393,#36394,#36395,#36396,#36397,
#36398,#36399,#36400,#36401,#36402,#36403,#36404,#36405,#36406,#36407,#36408,
#36409,#36410,#36411,#36412,#36413,#36414,#36415,#36416,#36417,#36418,#36419,
#36420,#36421,#36422,#36423,#36424,#36425,#36426,#36427,#36428,#36429,#36430,
#36431,#36432,#36433,#36434,#36435,#36436,#36437,#36438,#36439,#36440,#36441,
#36442,#36443,#36444,#36445,#36446,#36447,#36448,#36449,#36450,#36451,#36452,
#36453,#36454,#36455,#36456,#36457,#36458,#36459,#36460,#36461,#36462,#36463,
#36464,#36465,#36466,#36467,#36468,#36469,#36470,#36471,#36472,#36473,#36474,
#36475,#36476,#36477,#36478,#36479,#36480,#36481,#36482,#36483,#36484,#36485,
#36486,#36487,#36488,#36489,#36490,#36491,#36492,#36493,#36494,#36495,#36496,
#36497,#36498,#36499,#36500,#36501,#36502,#36503,#36504,#36505,#36506,#36507,
#36508,#36509,#36510,#36511,#36512,#36513,#36514,#36515,#36516,#36517,#36518,
#36519,#36520,#36521,#36522,#36523,#36524,#36525,#36526,#36527,#36528,#36529,
#36530,#36531,#36532,#36533,#36534,#36535,#36536,#36537,#36538,#36539,#36540,
#36541,#36542,#36543,#36544,#36545,#36546,#36547,#36548,#36549,#36550,#36551,
#36552,#36553,#36554,#36555,#36556,#36557,#36558,#36559,#36560,#36561,#36562,
#36563,#36564,#36565,#36566,#36567,#36568,#36569,#36570,#36571,#36572,#36573,
#36574,#36575,#36576,#36577,#36578,#36579,#36580,#36581,#36582,#36583,#36584,
#36585,#36586,#36587,#36588,#36589,#36590,#36591,#36592,#36593,#36594,#36595,
#36596,#36597,#36598,#36599,#36600,#36601,#36602,#36603),(#36604,#36605,
#36606,#36607,#36608,#36609,#36610,#36611,#36612,#36613,#36614,#36615,#36616,
#36617,#36618,#36619,#36620,#36621,#36622,#36623,#36624,#36625,#36626,#36627,
#36628,#36629,#36630,#36631,#36632,#36633,#36634,#36635,#36636,#36637,#36638,
#36639,#36640,#36641,#36642,#36643,#36644,#36645,#36646,#36647,#36648,#36649,
#36650,#36651,#36652,#36653,#36654,#36655,#36656,#36657,#36658,#36659,#36660,
#36661,#36662,#36663,#36664,#36665,#36666,#36667,#36668,#36669,#36670,#36671,
#36672,#36673,#36674,#36675,#36676,#36677,#36678,#36679,#36680,#36681,#36682,
#36683,#36684,#36685,#36686,#36687,#36688,#36689,#36690,#36691,#36692,#36693,
#36694,#36695,#36696,#36697,#36698,#36699,#36700,#36701,#36702,#36703,#36704,
#36705,#36706,#36707,#36708,#36709,#36710,#36711,#36712,#36713,#36714,#36715,
#36716,#36717,#36718,#36719,#36720,#36721,#36722,#36723,#36724,#36725,#36726,
#36727,#36728,#36729,#36730,#36731,#36732,#36733,#36734,#36735,#36736,#36737,
#36738,#36739,#36740,#36741,#36742,#36743,#36744,#36745,#36746,#36747,#36748,
#36749,#36750,#36751,#36752,#36753,#36754,#36755,#36756,#36757,#36758,#36759,
#36760,#36761,#36762,#36763,#36764,#36765,#36766,#36767,#36768,#36769,#36770,
#36771,#36772,#36773,#36774,#36775,#36776,#36777,#36778,#36779,#36780,#36781,
#36782,#36783,#36784,#36785,#36786,#36787,#36788,#36789,#36790,#36791,#36792,
#36793,#36794,#36795,#36796,#36797,#36798,#36799,#36800,#36801,#36802,#36803,
#36804,#36805,#36806,#36807,#36808,#36809,#36810,#36811,#36812,#36813,#36814,
#36815,#36816,#36817,#36818,#36819,#36820,#36821,#36822,#36823,#36824,#36825,
#36826,#36827,#36828,#36829,#36830,#36831,#36832,#36833,#36834,#36835,#36836,
#36837,#36838,#36839,#36840,#36841,#36842,#36843,#36844,#36845,#36846,#36847,
#36848,#36849,#36850,#36851,#36852,#36853,#36854,#36855,#36856,#36857,#36858,
#36859,#36860,#36861,#36862,#36863,#36864,#36865,#36866,#36867,#36868,#36869,
#36870,#36871,#36872,#36873,#36874,#36875,#36876,#36877,#36878,#36879,#36880,
#36881,#36882,#36883,#36884,#36885,#36886,#36887,#36888,#36889,#36890,#36891,
#36892,#36893,#36894,#36895,#36896,#36897,#36898,#36899,#36900,#36901,#36902,
#36903,#36904,#36905,#36906,#36907,#36908,#36909,#36910,#36911,#36912,#36913,
#36914,#36915,#36916,#36917,#36918,#36919,#36920,#36921,#36922,#36923,#36924,
#36925,#36926,#36927,#36928,#36929,#36930,#36931,#36932,#36933,#36934,#36935,
#36936,#36937,#36938,#36939,#36940,#36941,#36942,#36943,#36944,#36945,#36946,
#36947,#36948,#36949,#36950,#36951,#36952,#36953,#36954,#36955,#36956,#36957,
#36958,#36959,#36960,#36961,#36962,#36963,#36964,#36965,#36966,#36967,#36968,
#36969,#36970,#36971,#36972,#36973,#36974,#36975,#36976,#36977,#36978,#36979,
#36980,#36981,#36982,#36983,#36984,#36985,#36986,#36987,#36988,#36989,#36990,
#36991,#36992,#36993,#36994,#36995,#36996,#36997,#36998,#36999,#37000,#37001,
#37002,#37003,#37004,#37005,#37006,#37007,#37008,#37009,#37010,#37011,#37012,
#37013,#37014,#37015,#37016,#37017,#37018,#37019,#37020,#37021,#37022,#37023,
#37024,#37025,#37026,#37027,#37028,#37029,#37030,#37031,#37032,#37033,#37034,
#37035,#37036,#37037,#37038,#37039,#37040,#37041,#37042,#37043,#37044,#37045,
#37046,#37047,#37048,#37049,#37050,#37051,#37052,#37053,#37054,#37055,#37056,
#37057,#37058,#37059,#37060,#37061,#37062,#37063,#37064,#37065,#37066,#37067,
#37068,#37069,#37070,#37071,#37072,#37073,#37074,#37075,#37076,#37077,#37078,
#37079,#37080,#37081,#37082,#37083,#37084,#37085,#37086,#37087,#37088,#37089,
#37090,#37091,#37092,#37093,#37094,#37095,#37096,#37097,#37098,#37099,#37100),
(#37101,#37102,#37103,#37104,#37105,#37106,#37107,#37108,#37109,#37110,
#37111,#37112,#37113,#37114,#37115,#37116,#37117,#37118,#37119,#37120,#37121,
#37122,#37123,#37124,#37125,#37126,#37127,#37128,#37129,#37130,#37131,#37132,
#37133,#37134,#37135,#37136,#37137,#37138,#37139,#37140,#37141,#37142,#37143,
#37144,#37145,#37146,#37147,#37148,#37149,#37150,#37151,#37152,#37153,#37154,
#37155,#37156,#37157,#37158,#37159,#37160,#37161,#37162,#37163,#37164,#37165,
#37166,#37167,#37168,#37169,#37170,#37171,#37172,#37173,#37174,#37175,#37176,
#37177,#37178,#37179,#37180,#37181,#37182,#37183,#37184,#37185,#37186,#37187,
#37188,#37189,#37190,#37191,#37192,#37193,#37194,#37195,#37196,#37197,#37198,
#37199,#37200,#37201,#37202,#37203,#37204,#37205,#37206,#37207,#37208,#37209,
#37210,#37211,#37212,#37213,#37214,#37215,#37216,#37217,#37218,#37219,#37220,
#37221,#37222,#37223,#37224,#37225,#37226,#37227,#37228,#37229,#37230,#37231,
#37232,#37233,#37234,#37235,#37236,#37237,#37238,#37239,#37240,#37241,#37242,
#37243,#37244,#37245,#37246,#37247,#37248,#37249,#37250,#37251,#37252,#37253,
#37254,#37255,#37256,#37257,#37258,#37259,#37260,#37261,#37262,#37263,#37264,
#37265,#37266,#37267,#37268,#37269,#37270,#37271,#37272,#37273,#37274,#37275,
#37276,#37277,#37278,#37279,#37280,#37281,#37282,#37283,#37284,#37285,#37286,
#37287,#37288,#37289,#37290,#37291,#37292,#37293,#37294,#37295,#37296,#37297,
#37298,#37299,#37300,#37301,#37302,#37303,#37304,#37305,#37306,#37307,#37308,
#37309,#37310,#37311,#37312,#37313,#37314,#37315,#37316,#37317,#37318,#37319,
#37320,#37321,#37322,#37323,#37324,#37325,#37326,#37327,#37328,#37329,#37330,
#37331,#37332,#37333,#37334,#37335,#37336,#37337,#37338,#37339,#37340,#37341,
#37342,#37343,#37344,#37345,#37346,#37347,#37348,#37349,#37350,#37351,#37352,
#37353,#37354,#37355,#37356,#37357,#37358,#37359,#37360,#37361,#37362,#37363,
#37364,#37365,#37366,#37367,#37368,#37369,#37370,#37371,#37372,#37373,#37374,
#37375,#37376,#37377,#37378,#37379,#37380,#37381,#37382,#37383,#37384,#37385,
#37386,#37387,#37388,#37389,#37390,#37391,#37392,#37393,#37394,#37395,#37396,
#37397,#37398,#37399,#37400,#37401,#37402,#37403,#37404,#37405,#37406,#37407,
#37408,#37409,#37410,#37411,#37412,#37413,#37414,#37415,#37416,#37417,#37418,
#37419,#37420,#37421,#37422,#37423,#37424,#37425,#37426,#37427,#37428,#37429,
#37430,#37431,#37432,#37433,#37434,#37435,#37436,#37437,#37438,#37439,#37440,
#37441,#37442,#37443,#37444,#37445,#37446,#37447,#37448,#37449,#37450,#37451,
#37452,#37453,#37454,#37455,#37456,#37457,#37458,#37459,#37460,#37461,#37462,
#37463,#37464,#37465,#37466,#37467,#37468,#37469,#37470,#37471,#37472,#37473,
#37474,#37475,#37476,#37477,#37478,#37479,#37480,#37481,#37482,#37483,#37484,
#37485,#37486,#37487,#37488,#37489,#37490,#37491,#37492,#37493,#37494,#37495,
#37496,#37497,#37498,#37499,#37500,#37501,#37502,#37503,#37504,#37505,#37506,
#37507,#37508,#37509,#37510,#37511,#37512,#37513,#37514,#37515,#37516,#37517,
#37518,#37519,#37520,#37521,#37522,#37523,#37524,#37525,#37526,#37527,#37528,
#37529,#37530,#37531,#37532,#37533,#37534,#37535,#37536,#37537,#37538,#37539,
#37540,#37541,#37542,#37543,#37544,#37545,#37546,#37547,#37548,#37549,#37550,
#37551,#37552,#37553,#37554,#37555,#37556,#37557,#37558,#37559,#37560,#37561,
#37562,#37563,#37564,#37565,#37566,#37567,#37568,#37569,#37570,#37571,#37572,
#37573,#37574,#37575,#37576,#37577,#37578,#37579,#37580,#37581,#37582,#37583,
#37584,#37585,#37586,#37587,#37588,#37589,#37590,#37591,#37592,#37593,#37594,
#37595,#37596,#37597),(#37598,#37599,#37600,#37601,#37602,#37603,#37604,
#37605,#37606,#37607,#37608,#37609,#37610,#37611,#37612,#37613,#37614,#37615,
#37616,#37617,#37618,#37619,#37620,#37621,#37622,#37623,#37624,#37625,#37626,
#37627,#37628,#37629,#37630,#37631,#37632,#37633,#37634,#37635,#37636,#37637,
#37638,#37639,#37640,#37641,#37642,#37643,#37644,#37645,#37646,#37647,#37648,
#37649,#37650,#37651,#37652,#37653,#37654,#37655,#37656,#37657,#37658,#37659,
#37660,#37661,#37662,#37663,#37664,#37665,#37666,#37667,#37668,#37669,#37670,
#37671,#37672,#37673,#37674,#37675,#37676,#37677,#37678,#37679,#37680,#37681,
#37682,#37683,#37684,#37685,#37686,#37687,#37688,#37689,#37690,#37691,#37692,
#37693,#37694,#37695,#37696,#37697,#37698,#37699,#37700,#37701,#37702,#37703,
#37704,#37705,#37706,#37707,#37708,#37709,#37710,#37711,#37712,#37713,#37714,
#37715,#37716,#37717,#37718,#37719,#37720,#37721,#37722,#37723,#37724,#37725,
#37726,#37727,#37728,#37729,#37730,#37731,#37732,#37733,#37734,#37735,#37736,
#37737,#37738,#37739,#37740,#37741,#37742,#37743,#37744,#37745,#37746,#37747,
#37748,#37749,#37750,#37751,#37752,#37753,#37754,#37755,#37756,#37757,#37758,
#37759,#37760,#37761,#37762,#37763,#37764,#37765,#37766,#37767,#37768,#37769,
#37770,#37771,#37772,#37773,#37774,#37775,#37776,#37777,#37778,#37779,#37780,
#37781,#37782,#37783,#37784,#37785,#37786,#37787,#37788,#37789,#37790,#37791,
#37792,#37793,#37794,#37795,#37796,#37797,#37798,#37799,#37800,#37801,#37802,
#37803,#37804,#37805,#37806,#37807,#37808,#37809,#37810,#37811,#37812,#37813,
#37814,#37815,#37816,#37817,#37818,#37819,#37820,#37821,#37822,#37823,#37824,
#37825,#37826,#37827,#37828,#37829,#37830,#37831,#37832,#37833,#37834,#37835,
#37836,#37837,#37838,#37839,#37840,#37841,#37842,#37843,#37844,#37845,#37846,
#37847,#37848,#37849,#37850,#37851,#37852,#37853,#37854,#37855,#37856,#37857,
#37858,#37859,#37860,#37861,#37862,#37863,#37864,#37865,#37866,#37867,#37868,
#37869,#37870,#37871,#37872,#37873,#37874,#37875,#37876,#37877,#37878,#37879,
#37880,#37881,#37882,#37883,#37884,#37885,#37886,#37887,#37888,#37889,#37890,
#37891,#37892,#37893,#37894,#37895,#37896,#37897,#37898,#37899,#37900,#37901,
#37902,#37903,#37904,#37905,#37906,#37907,#37908,#37909,#37910,#37911,#37912,
#37913,#37914,#37915,#37916,#37917,#37918,#37919,#37920,#37921,#37922,#37923,
#37924,#37925,#37926,#37927,#37928,#37929,#37930,#37931,#37932,#37933,#37934,
#37935,#37936,#37937,#37938,#37939,#37940,#37941,#37942,#37943,#37944,#37945,
#37946,#37947,#37948,#37949,#37950,#37951,#37952,#37953,#37954,#37955,#37956,
#37957,#37958,#37959,#37960,#37961,#37962,#37963,#37964,#37965,#37966,#37967,
#37968,#37969,#37970,#37971,#37972,#37973,#37974,#37975,#37976,#37977,#37978,
#37979,#37980,#37981,#37982,#37983,#37984,#37985,#37986,#37987,#37988,#37989,
#37990,#37991,#37992,#37993,#37994,#37995,#37996,#37997,#37998,#37999,#38000,
#38001,#38002,#38003,#38004,#38005,#38006,#38007,#38008,#38009,#38010,#38011,
#38012,#38013,#38014,#38015,#38016,#38017,#38018,#38019,#38020,#38021,#38022,
#38023,#38024,#38025,#38026,#38027,#38028,#38029,#38030,#38031,#38032,#38033,
#38034,#38035,#38036,#38037,#38038,#38039,#38040,#38041,#38042,#38043,#38044,
#38045,#38046,#38047,#38048,#38049,#38050,#38051,#38052,#38053,#38054,#38055,
#38056,#38057,#38058,#38059,#38060,#38061,#38062,#38063,#38064,#38065,#38066,
#38067,#38068,#38069,#38070,#38071,#38072,#38073,#38074,#38075,#38076,#38077,
#38078,#38079,#38080,#38081,#38082,#38083,#38084,#38085,#38086,#38087,#38088,
#38089,#38090,#38091,#38092,#38093,#38094)),.UNSPECIFIED.,.F.,.F.,.F.,(4,
4),(4,1,1,1,1,1,1,1,1,1,1,1,1,1,1,1,1,1,1,1,1,1,1,1,1,1,1,1,1,1,1,1,1,1,
1,1,1,1,1,1,1,1,1,1,1,1,1,1,1,1,1,1,1,1,1,1,1,1,1,1,1,1,1,1,1,1,1,1,1,1,
1,1,1,1,1,1,1,1,1,1,1,1,1,1,1,1,1,1,1,1,1,1,1,1,1,1,1,1,1,1,1,1,1,1,1,1,
1,1,1,1,1,1,1,1,1,1,1,1,1,1,1,1,1,1,1,1,1,1,1,1,1,1,1,1,1,1,1,1,1,1,1,1,
1,1,1,1,1,1,1,1,1,1,1,1,1,1,1,1,1,1,1,1,1,1,1,1,1,1,1,1,1,1,1,1,1,1,1,1,
1,1,1,1,1,1,1,1,1,1,1,1,1,1,1,1,1,1,1,1,1,1,1,1,1,1,1,1,1,1,1,1,1,1,1,1,
1,1,1,1,1,1,1,1,1,1,1,1,1,1,1,1,1,1,1,1,1,1,1,1,1,1,1,1,1,1,1,1,1,1,1,1,
1,1,1,1,1,1,1,1,1,1,1,1,1,1,1,1,1,1,1,1,1,1,1,1,1,1,1,1,1,1,1,1,1,1,1,1,
1,1,1,1,1,1,1,1,1,1,1,1,1,1,1,1,1,1,1,1,1,1,1,1,1,1,1,1,1,1,1,1,1,1,1,1,
1,1,1,1,1,1,1,1,1,1,1,1,1,1,1,1,1,1,1,1,1,1,1,1,1,1,1,1,1,1,1,1,1,1,1,1,
1,1,1,1,1,1,1,1,1,1,1,1,1,1,1,1,1,1,1,1,1,1,1,1,1,1,1,1,1,1,1,1,1,1,1,1,
1,1,1,1,1,1,1,1,1,1,1,1,1,1,1,1,1,1,1,1,1,1,1,1,1,1,1,1,1,1,1,1,1,1,1,1,
1,1,1,1,1,1,1,1,1,1,1,1,1,1,1,1,1,1,1,1,1,1,1,1,1,1,1,1,1,1,1,1,1,1,1,1,
1,1,1,1,1,1,1,1,1,1,1,1,1,1,1,1,1,1,1,1,1,1,1,1,1,1,1,1,4),(0.,0.0641840294258107),
(11.8589888623082,12.3576971556948,12.8564054490814,13.355113742468,13.8538220358547,
14.3525303292413,14.8512386226279,15.3499469160145,15.8486552094011,16.3473635027878,
16.8460717961744,17.344780089561,17.8434883829476,18.3421966763342,18.8409049697209,
19.3396132631075,19.8383215564941,20.3370298498807,20.8357381432673,21.334446436654,
21.8331547300406,22.3318630234272,22.8305713168138,23.3292796102004,23.8279879035871,
24.3266961969737,24.8254044903603,25.3241127837469,25.8228210771335,26.3215293705201,
26.8202376639068,27.3189459572934,27.81765425068,28.3163625440666,28.8150708374532,
29.3137791308399,29.8124874242265,30.3111957176131,30.8099040109997,31.3086123043863,
31.807320597773,32.3060288911596,32.8047371845462,33.3034454779328,33.8021537713194,
34.3008620647061,34.7995703580927,35.2982786514793,35.7969869448659,36.2956952382525,
36.7944035316392,37.2931118250258,37.7918201184124,38.290528411799,38.7892367051856,
39.2879449985723,39.7866532919589,40.2853615853455,40.7840698787321,41.2827781721187,
41.7814864655054,42.280194758892,42.7789030522786,43.2776113456652,43.7763196390518,
44.2750279324384,44.7737362258251,45.2724445192117,45.7711528125983,46.2698611059849,
46.7685693993716,47.2672776927582,47.7659859861448,48.2646942795314,48.763402572918,
49.2621108663046,49.7608191596913,50.2595274530779,50.7582357464645,51.2569440398511,
51.7556523332377,52.2543606266244,52.753068920011,53.2517772133976,53.7504855067842,
54.2491938001708,54.7479020935575,55.2466103869441,55.7453186803307,56.2440269737173,
56.7427352671039,57.2414435604906,57.7401518538772,58.2388601472638,58.7375684406504,
59.236276734037,59.7349850274237,60.2336933208103,60.7324016141969,61.2311099075835,
61.7298182009701,62.2285264943567,62.7272347877434,63.22594308113,63.7246513745166,
64.2233596679032,64.7220679612898,65.2207762546765,65.7194845480631,66.2181928414497,
66.7169011348363,67.2156094282229,67.7143177216096,68.2130260149962,68.7117343083828,
69.2104426017694,69.709150895156,70.2078591885427,70.7065674819293,71.2052757753159,
71.7039840687025,72.2026923620891,72.7014006554758,73.2001089488624,73.698817242249,
74.1975255356356,74.6962338290222,75.1949421224089,75.6936504157955,76.1923587091821,
76.6910670025687,77.1897752959553,77.6884835893419,78.1871918827286,78.6859001761152,
79.1846084695018,79.6833167628884,80.1820250562751,80.6807333496617,81.1794416430483,
81.6781499364349,82.1768582298215,82.6755665232081,83.1742748165948,83.6729831099814,
84.171691403368,84.6703996967546,85.1691079901412,85.6678162835279,86.1665245769145,
86.6652328703011,87.1639411636877,87.6626494570743,88.161357750461,88.6600660438476,
89.1587743372342,89.6574826306208,90.1561909240074,90.654899217394,91.1536075107807,
91.6523158041673,92.1510240975539,92.6497323909405,93.1484406843271,93.6471489777138,
94.1458572711004,94.644565564487,95.1432738578736,95.6419821512603,96.1406904446469,
96.6393987380335,97.1381070314201,97.6368153248067,98.1355236181933,98.63423191158,
99.1329402049666,99.6316484983532,100.13035679174,100.629065085126,101.127773378513,
101.6264816719,102.125189965286,102.623898258673,103.12260655206,103.621314845446,
104.120023138833,104.618731432219,105.117439725606,105.616148018993,106.114856312379,
106.613564605766,107.112272899152,107.610981192539,108.109689485926,108.608397779312,
109.107106072699,109.605814366086,110.104522659472,110.603230952859,111.101939246245,
111.600647539632,112.099355833019,112.598064126405,113.096772419792,113.595480713179,
114.094189006565,114.592897299952,115.091605593338,115.590313886725,116.089022180112,
116.587730473498,117.086438766885,117.585147060271,118.083855353658,118.582563647045,
119.081271940431,119.579980233818,120.078688527205,120.577396820591,121.076105113978,
121.574813407364,122.073521700751,122.572229994138,123.070938287524,123.569646580911,
124.068354874298,124.567063167684,125.065771461071,125.564479754457,126.063188047844,
126.561896341231,127.060604634617,127.559312928004,128.058021221391,128.556729514777,
129.055437808164,129.55414610155,130.052854394937,130.551562688324,131.05027098171,
131.548979275097,132.54639586187,133.543812448643,134.541229035417,135.53864562219,
136.536062208963,137.533478795736,138.53089538251,139.528311969283,140.525728556056,
141.523145142829,142.520561729602,143.517978316376,144.515394903149,145.512811489922,
146.011519783309,146.510228076695,147.008936370082,147.507644663469,148.006352956855,
148.505061250242,149.003769543629,149.502477837015,150.001186130402,150.499894423788,
150.998602717175,151.497311010562,151.996019303948,152.494727597335,152.993435890721,
153.492144184108,153.990852477495,154.489560770881,154.988269064268,155.486977357655,
155.985685651041,156.484393944428,156.983102237814,157.481810531201,157.980518824588,
158.479227117974,158.977935411361,159.476643704748,159.975351998134,160.474060291521,
160.972768584907,161.471476878294,161.970185171681,162.468893465067,162.967601758454,
163.466310051841,163.965018345227,164.463726638614,164.962434932,165.461143225387,
165.959851518774,166.45855981216,166.957268105547,167.455976398933,167.95468469232,
168.453392985707,168.952101279093,169.45080957248,169.949517865867,170.448226159253,
170.94693445264,171.445642746026,171.944351039413,172.4430593328,172.941767626186,
173.440475919573,173.93918421296,174.437892506346,174.936600799733,175.435309093119,
175.934017386506,176.432725679893,176.931433973279,177.430142266666,177.928850560052,
178.427558853439,178.926267146826,179.424975440212,179.923683733599,180.422392026986,
180.921100320372,181.419808613759,181.918516907145,182.417225200532,182.915933493919,
183.414641787305,183.913350080692,184.412058374079,184.910766667465,185.409474960852,
185.908183254238,186.406891547625,186.905599841012,187.404308134398,187.903016427785,
188.401724721171,188.900433014558,189.399141307945,189.897849601331,190.396557894718,
190.895266188105,191.393974481491,191.892682774878,192.391391068264,192.890099361651,
193.388807655038,193.887515948424,194.386224241811,194.884932535198,195.383640828584,
195.882349121971,196.381057415357,196.879765708744,197.378474002131,197.877182295517,
198.375890588904,198.87459888229,199.373307175677,199.872015469064,200.37072376245,
200.869432055837,201.368140349224,201.86684864261,202.365556935997,202.864265229383,
203.36297352277,203.861681816157,204.360390109543,204.85909840293,205.357806696317,
205.856514989703,206.35522328309,206.853931576476,207.352639869863,207.85134816325,
208.350056456636,208.848764750023,209.347473043409,209.846181336796,210.344889630183,
210.843597923569,211.342306216956,211.841014510343,212.339722803729,212.838431097116,
213.337139390502,213.835847683889,214.334555977276,214.833264270662,215.331972564049,
215.830680857436,216.329389150822,216.828097444209,217.326805737595,217.825514030982,
218.324222324369,218.822930617755,219.321638911142,219.820347204529,220.319055497915,
220.817763791302,221.316472084688,221.815180378075,222.313888671462,222.812596964848,
223.311305258235,223.810013551621,224.308721845008,224.807430138395,225.306138431781,
225.804846725168,226.303555018555,226.802263311941,227.300971605328,227.799679898714,
228.298388192101,228.797096485488,229.295804778874,229.794513072261,230.293221365647,
230.791929659034,231.290637952421,231.789346245807,232.288054539194,232.786762832581,
233.285471125967,233.784179419354,234.28288771274,234.781596006127,235.280304299514,
235.7790125929,236.277720886287,236.776429179674,237.27513747306,237.773845766447,
238.272554059833,238.77126235322,239.269970646607,239.768678939993,240.26738723338,
240.766095526767,241.264803820153,241.76351211354,242.262220406926,242.760928700313,
243.2596369937,243.758345287086,244.257053580473,244.755761873859,245.254470167246,
245.753178460633,246.251886754019,246.750595047406,247.249303340793,247.748011634179,
248.246719927566,248.745428220952,249.244136514339,249.742844807726,250.241553101112,
250.740261394499,251.238969687886,251.737677981272,252.236386274659,252.735094568045,
253.233802861432,253.732511154819,254.231219448205,254.729927741592,255.228636034978,
255.727344328365,256.226052621752,256.724760915138,257.223469208525,257.722177501912,
258.220885795298,258.719594088685,259.218302382071,259.717010675458,260.215718968845,
260.714427262231,261.213135555618,261.711843849004,262.210552142391,262.709260435778,
263.207968729164,263.706677022551,264.205385315938,264.704093609324,265.202801902711),
 .UNSPECIFIED.);
#268=B_SPLINE_SURFACE_WITH_KNOTS('',3,3,((#38244,#38245,#38246,#38247,#38248,
#38249,#38250,#38251,#38252,#38253,#38254,#38255,#38256,#38257,#38258,#38259,
#38260,#38261,#38262,#38263,#38264,#38265,#38266,#38267,#38268,#38269,#38270,
#38271,#38272,#38273,#38274,#38275,#38276,#38277,#38278,#38279,#38280,#38281,
#38282,#38283,#38284,#38285,#38286,#38287,#38288,#38289,#38290,#38291,#38292,
#38293,#38294,#38295,#38296,#38297,#38298,#38299,#38300,#38301,#38302,#38303,
#38304,#38305,#38306,#38307,#38308,#38309,#38310,#38311,#38312,#38313,#38314,
#38315,#38316,#38317,#38318,#38319,#38320,#38321,#38322,#38323,#38324,#38325,
#38326,#38327,#38328,#38329,#38330,#38331,#38332,#38333,#38334,#38335,#38336,
#38337,#38338,#38339,#38340,#38341,#38342,#38343,#38344,#38345,#38346,#38347,
#38348,#38349,#38350,#38351,#38352,#38353,#38354,#38355,#38356,#38357,#38358,
#38359,#38360,#38361,#38362,#38363,#38364,#38365,#38366,#38367,#38368,#38369,
#38370,#38371,#38372,#38373,#38374,#38375,#38376,#38377,#38378,#38379,#38380,
#38381,#38382,#38383,#38384,#38385,#38386,#38387,#38388,#38389,#38390,#38391,
#38392,#38393,#38394,#38395,#38396,#38397,#38398,#38399,#38400,#38401,#38402,
#38403,#38404,#38405,#38406,#38407,#38408,#38409,#38410,#38411,#38412,#38413,
#38414,#38415,#38416,#38417,#38418,#38419,#38420,#38421,#38422,#38423,#38424,
#38425,#38426,#38427,#38428,#38429,#38430,#38431,#38432,#38433,#38434,#38435,
#38436,#38437,#38438,#38439,#38440,#38441,#38442,#38443,#38444,#38445,#38446,
#38447,#38448,#38449,#38450,#38451,#38452,#38453,#38454,#38455,#38456,#38457,
#38458,#38459,#38460,#38461,#38462,#38463,#38464,#38465,#38466,#38467,#38468,
#38469,#38470,#38471,#38472,#38473,#38474,#38475,#38476,#38477,#38478,#38479,
#38480,#38481,#38482,#38483,#38484,#38485,#38486,#38487,#38488,#38489,#38490,
#38491,#38492,#38493,#38494,#38495,#38496,#38497,#38498,#38499,#38500,#38501,
#38502,#38503,#38504,#38505,#38506,#38507,#38508,#38509,#38510,#38511,#38512,
#38513,#38514,#38515,#38516,#38517,#38518,#38519,#38520,#38521,#38522,#38523,
#38524,#38525,#38526,#38527,#38528,#38529,#38530,#38531,#38532,#38533,#38534,
#38535,#38536,#38537,#38538,#38539,#38540,#38541,#38542,#38543,#38544,#38545,
#38546,#38547,#38548,#38549,#38550,#38551,#38552,#38553,#38554,#38555,#38556,
#38557,#38558,#38559,#38560,#38561,#38562,#38563,#38564,#38565,#38566,#38567,
#38568,#38569,#38570,#38571,#38572,#38573,#38574,#38575,#38576,#38577,#38578,
#38579,#38580,#38581,#38582,#38583,#38584,#38585,#38586,#38587,#38588,#38589,
#38590,#38591,#38592,#38593,#38594,#38595,#38596,#38597,#38598,#38599,#38600,
#38601,#38602,#38603,#38604,#38605,#38606,#38607,#38608,#38609,#38610,#38611,
#38612,#38613,#38614,#38615,#38616,#38617,#38618,#38619,#38620,#38621,#38622,
#38623,#38624,#38625,#38626,#38627,#38628,#38629,#38630,#38631,#38632,#38633,
#38634,#38635,#38636,#38637,#38638,#38639,#38640,#38641,#38642,#38643,#38644,
#38645,#38646,#38647,#38648,#38649,#38650,#38651,#38652,#38653,#38654,#38655,
#38656,#38657,#38658,#38659,#38660,#38661,#38662,#38663,#38664,#38665,#38666,
#38667,#38668,#38669,#38670,#38671,#38672,#38673,#38674,#38675,#38676,#38677,
#38678,#38679,#38680,#38681,#38682,#38683,#38684,#38685,#38686,#38687,#38688,
#38689,#38690,#38691,#38692,#38693,#38694,#38695,#38696,#38697,#38698,#38699,
#38700,#38701,#38702,#38703,#38704,#38705,#38706,#38707,#38708,#38709,#38710,
#38711,#38712,#38713,#38714,#38715,#38716,#38717,#38718,#38719,#38720,#38721,
#38722,#38723,#38724,#38725,#38726,#38727,#38728,#38729,#38730,#38731,#38732,
#38733,#38734,#38735,#38736,#38737,#38738,#38739,#38740),(#38741,#38742,
#38743,#38744,#38745,#38746,#38747,#38748,#38749,#38750,#38751,#38752,#38753,
#38754,#38755,#38756,#38757,#38758,#38759,#38760,#38761,#38762,#38763,#38764,
#38765,#38766,#38767,#38768,#38769,#38770,#38771,#38772,#38773,#38774,#38775,
#38776,#38777,#38778,#38779,#38780,#38781,#38782,#38783,#38784,#38785,#38786,
#38787,#38788,#38789,#38790,#38791,#38792,#38793,#38794,#38795,#38796,#38797,
#38798,#38799,#38800,#38801,#38802,#38803,#38804,#38805,#38806,#38807,#38808,
#38809,#38810,#38811,#38812,#38813,#38814,#38815,#38816,#38817,#38818,#38819,
#38820,#38821,#38822,#38823,#38824,#38825,#38826,#38827,#38828,#38829,#38830,
#38831,#38832,#38833,#38834,#38835,#38836,#38837,#38838,#38839,#38840,#38841,
#38842,#38843,#38844,#38845,#38846,#38847,#38848,#38849,#38850,#38851,#38852,
#38853,#38854,#38855,#38856,#38857,#38858,#38859,#38860,#38861,#38862,#38863,
#38864,#38865,#38866,#38867,#38868,#38869,#38870,#38871,#38872,#38873,#38874,
#38875,#38876,#38877,#38878,#38879,#38880,#38881,#38882,#38883,#38884,#38885,
#38886,#38887,#38888,#38889,#38890,#38891,#38892,#38893,#38894,#38895,#38896,
#38897,#38898,#38899,#38900,#38901,#38902,#38903,#38904,#38905,#38906,#38907,
#38908,#38909,#38910,#38911,#38912,#38913,#38914,#38915,#38916,#38917,#38918,
#38919,#38920,#38921,#38922,#38923,#38924,#38925,#38926,#38927,#38928,#38929,
#38930,#38931,#38932,#38933,#38934,#38935,#38936,#38937,#38938,#38939,#38940,
#38941,#38942,#38943,#38944,#38945,#38946,#38947,#38948,#38949,#38950,#38951,
#38952,#38953,#38954,#38955,#38956,#38957,#38958,#38959,#38960,#38961,#38962,
#38963,#38964,#38965,#38966,#38967,#38968,#38969,#38970,#38971,#38972,#38973,
#38974,#38975,#38976,#38977,#38978,#38979,#38980,#38981,#38982,#38983,#38984,
#38985,#38986,#38987,#38988,#38989,#38990,#38991,#38992,#38993,#38994,#38995,
#38996,#38997,#38998,#38999,#39000,#39001,#39002,#39003,#39004,#39005,#39006,
#39007,#39008,#39009,#39010,#39011,#39012,#39013,#39014,#39015,#39016,#39017,
#39018,#39019,#39020,#39021,#39022,#39023,#39024,#39025,#39026,#39027,#39028,
#39029,#39030,#39031,#39032,#39033,#39034,#39035,#39036,#39037,#39038,#39039,
#39040,#39041,#39042,#39043,#39044,#39045,#39046,#39047,#39048,#39049,#39050,
#39051,#39052,#39053,#39054,#39055,#39056,#39057,#39058,#39059,#39060,#39061,
#39062,#39063,#39064,#39065,#39066,#39067,#39068,#39069,#39070,#39071,#39072,
#39073,#39074,#39075,#39076,#39077,#39078,#39079,#39080,#39081,#39082,#39083,
#39084,#39085,#39086,#39087,#39088,#39089,#39090,#39091,#39092,#39093,#39094,
#39095,#39096,#39097,#39098,#39099,#39100,#39101,#39102,#39103,#39104,#39105,
#39106,#39107,#39108,#39109,#39110,#39111,#39112,#39113,#39114,#39115,#39116,
#39117,#39118,#39119,#39120,#39121,#39122,#39123,#39124,#39125,#39126,#39127,
#39128,#39129,#39130,#39131,#39132,#39133,#39134,#39135,#39136,#39137,#39138,
#39139,#39140,#39141,#39142,#39143,#39144,#39145,#39146,#39147,#39148,#39149,
#39150,#39151,#39152,#39153,#39154,#39155,#39156,#39157,#39158,#39159,#39160,
#39161,#39162,#39163,#39164,#39165,#39166,#39167,#39168,#39169,#39170,#39171,
#39172,#39173,#39174,#39175,#39176,#39177,#39178,#39179,#39180,#39181,#39182,
#39183,#39184,#39185,#39186,#39187,#39188,#39189,#39190,#39191,#39192,#39193,
#39194,#39195,#39196,#39197,#39198,#39199,#39200,#39201,#39202,#39203,#39204,
#39205,#39206,#39207,#39208,#39209,#39210,#39211,#39212,#39213,#39214,#39215,
#39216,#39217,#39218,#39219,#39220,#39221,#39222,#39223,#39224,#39225,#39226,
#39227,#39228,#39229,#39230,#39231,#39232,#39233,#39234,#39235,#39236,#39237),
(#39238,#39239,#39240,#39241,#39242,#39243,#39244,#39245,#39246,#39247,
#39248,#39249,#39250,#39251,#39252,#39253,#39254,#39255,#39256,#39257,#39258,
#39259,#39260,#39261,#39262,#39263,#39264,#39265,#39266,#39267,#39268,#39269,
#39270,#39271,#39272,#39273,#39274,#39275,#39276,#39277,#39278,#39279,#39280,
#39281,#39282,#39283,#39284,#39285,#39286,#39287,#39288,#39289,#39290,#39291,
#39292,#39293,#39294,#39295,#39296,#39297,#39298,#39299,#39300,#39301,#39302,
#39303,#39304,#39305,#39306,#39307,#39308,#39309,#39310,#39311,#39312,#39313,
#39314,#39315,#39316,#39317,#39318,#39319,#39320,#39321,#39322,#39323,#39324,
#39325,#39326,#39327,#39328,#39329,#39330,#39331,#39332,#39333,#39334,#39335,
#39336,#39337,#39338,#39339,#39340,#39341,#39342,#39343,#39344,#39345,#39346,
#39347,#39348,#39349,#39350,#39351,#39352,#39353,#39354,#39355,#39356,#39357,
#39358,#39359,#39360,#39361,#39362,#39363,#39364,#39365,#39366,#39367,#39368,
#39369,#39370,#39371,#39372,#39373,#39374,#39375,#39376,#39377,#39378,#39379,
#39380,#39381,#39382,#39383,#39384,#39385,#39386,#39387,#39388,#39389,#39390,
#39391,#39392,#39393,#39394,#39395,#39396,#39397,#39398,#39399,#39400,#39401,
#39402,#39403,#39404,#39405,#39406,#39407,#39408,#39409,#39410,#39411,#39412,
#39413,#39414,#39415,#39416,#39417,#39418,#39419,#39420,#39421,#39422,#39423,
#39424,#39425,#39426,#39427,#39428,#39429,#39430,#39431,#39432,#39433,#39434,
#39435,#39436,#39437,#39438,#39439,#39440,#39441,#39442,#39443,#39444,#39445,
#39446,#39447,#39448,#39449,#39450,#39451,#39452,#39453,#39454,#39455,#39456,
#39457,#39458,#39459,#39460,#39461,#39462,#39463,#39464,#39465,#39466,#39467,
#39468,#39469,#39470,#39471,#39472,#39473,#39474,#39475,#39476,#39477,#39478,
#39479,#39480,#39481,#39482,#39483,#39484,#39485,#39486,#39487,#39488,#39489,
#39490,#39491,#39492,#39493,#39494,#39495,#39496,#39497,#39498,#39499,#39500,
#39501,#39502,#39503,#39504,#39505,#39506,#39507,#39508,#39509,#39510,#39511,
#39512,#39513,#39514,#39515,#39516,#39517,#39518,#39519,#39520,#39521,#39522,
#39523,#39524,#39525,#39526,#39527,#39528,#39529,#39530,#39531,#39532,#39533,
#39534,#39535,#39536,#39537,#39538,#39539,#39540,#39541,#39542,#39543,#39544,
#39545,#39546,#39547,#39548,#39549,#39550,#39551,#39552,#39553,#39554,#39555,
#39556,#39557,#39558,#39559,#39560,#39561,#39562,#39563,#39564,#39565,#39566,
#39567,#39568,#39569,#39570,#39571,#39572,#39573,#39574,#39575,#39576,#39577,
#39578,#39579,#39580,#39581,#39582,#39583,#39584,#39585,#39586,#39587,#39588,
#39589,#39590,#39591,#39592,#39593,#39594,#39595,#39596,#39597,#39598,#39599,
#39600,#39601,#39602,#39603,#39604,#39605,#39606,#39607,#39608,#39609,#39610,
#39611,#39612,#39613,#39614,#39615,#39616,#39617,#39618,#39619,#39620,#39621,
#39622,#39623,#39624,#39625,#39626,#39627,#39628,#39629,#39630,#39631,#39632,
#39633,#39634,#39635,#39636,#39637,#39638,#39639,#39640,#39641,#39642,#39643,
#39644,#39645,#39646,#39647,#39648,#39649,#39650,#39651,#39652,#39653,#39654,
#39655,#39656,#39657,#39658,#39659,#39660,#39661,#39662,#39663,#39664,#39665,
#39666,#39667,#39668,#39669,#39670,#39671,#39672,#39673,#39674,#39675,#39676,
#39677,#39678,#39679,#39680,#39681,#39682,#39683,#39684,#39685,#39686,#39687,
#39688,#39689,#39690,#39691,#39692,#39693,#39694,#39695,#39696,#39697,#39698,
#39699,#39700,#39701,#39702,#39703,#39704,#39705,#39706,#39707,#39708,#39709,
#39710,#39711,#39712,#39713,#39714,#39715,#39716,#39717,#39718,#39719,#39720,
#39721,#39722,#39723,#39724,#39725,#39726,#39727,#39728,#39729,#39730,#39731,
#39732,#39733,#39734),(#39735,#39736,#39737,#39738,#39739,#39740,#39741,
#39742,#39743,#39744,#39745,#39746,#39747,#39748,#39749,#39750,#39751,#39752,
#39753,#39754,#39755,#39756,#39757,#39758,#39759,#39760,#39761,#39762,#39763,
#39764,#39765,#39766,#39767,#39768,#39769,#39770,#39771,#39772,#39773,#39774,
#39775,#39776,#39777,#39778,#39779,#39780,#39781,#39782,#39783,#39784,#39785,
#39786,#39787,#39788,#39789,#39790,#39791,#39792,#39793,#39794,#39795,#39796,
#39797,#39798,#39799,#39800,#39801,#39802,#39803,#39804,#39805,#39806,#39807,
#39808,#39809,#39810,#39811,#39812,#39813,#39814,#39815,#39816,#39817,#39818,
#39819,#39820,#39821,#39822,#39823,#39824,#39825,#39826,#39827,#39828,#39829,
#39830,#39831,#39832,#39833,#39834,#39835,#39836,#39837,#39838,#39839,#39840,
#39841,#39842,#39843,#39844,#39845,#39846,#39847,#39848,#39849,#39850,#39851,
#39852,#39853,#39854,#39855,#39856,#39857,#39858,#39859,#39860,#39861,#39862,
#39863,#39864,#39865,#39866,#39867,#39868,#39869,#39870,#39871,#39872,#39873,
#39874,#39875,#39876,#39877,#39878,#39879,#39880,#39881,#39882,#39883,#39884,
#39885,#39886,#39887,#39888,#39889,#39890,#39891,#39892,#39893,#39894,#39895,
#39896,#39897,#39898,#39899,#39900,#39901,#39902,#39903,#39904,#39905,#39906,
#39907,#39908,#39909,#39910,#39911,#39912,#39913,#39914,#39915,#39916,#39917,
#39918,#39919,#39920,#39921,#39922,#39923,#39924,#39925,#39926,#39927,#39928,
#39929,#39930,#39931,#39932,#39933,#39934,#39935,#39936,#39937,#39938,#39939,
#39940,#39941,#39942,#39943,#39944,#39945,#39946,#39947,#39948,#39949,#39950,
#39951,#39952,#39953,#39954,#39955,#39956,#39957,#39958,#39959,#39960,#39961,
#39962,#39963,#39964,#39965,#39966,#39967,#39968,#39969,#39970,#39971,#39972,
#39973,#39974,#39975,#39976,#39977,#39978,#39979,#39980,#39981,#39982,#39983,
#39984,#39985,#39986,#39987,#39988,#39989,#39990,#39991,#39992,#39993,#39994,
#39995,#39996,#39997,#39998,#39999,#40000,#40001,#40002,#40003,#40004,#40005,
#40006,#40007,#40008,#40009,#40010,#40011,#40012,#40013,#40014,#40015,#40016,
#40017,#40018,#40019,#40020,#40021,#40022,#40023,#40024,#40025,#40026,#40027,
#40028,#40029,#40030,#40031,#40032,#40033,#40034,#40035,#40036,#40037,#40038,
#40039,#40040,#40041,#40042,#40043,#40044,#40045,#40046,#40047,#40048,#40049,
#40050,#40051,#40052,#40053,#40054,#40055,#40056,#40057,#40058,#40059,#40060,
#40061,#40062,#40063,#40064,#40065,#40066,#40067,#40068,#40069,#40070,#40071,
#40072,#40073,#40074,#40075,#40076,#40077,#40078,#40079,#40080,#40081,#40082,
#40083,#40084,#40085,#40086,#40087,#40088,#40089,#40090,#40091,#40092,#40093,
#40094,#40095,#40096,#40097,#40098,#40099,#40100,#40101,#40102,#40103,#40104,
#40105,#40106,#40107,#40108,#40109,#40110,#40111,#40112,#40113,#40114,#40115,
#40116,#40117,#40118,#40119,#40120,#40121,#40122,#40123,#40124,#40125,#40126,
#40127,#40128,#40129,#40130,#40131,#40132,#40133,#40134,#40135,#40136,#40137,
#40138,#40139,#40140,#40141,#40142,#40143,#40144,#40145,#40146,#40147,#40148,
#40149,#40150,#40151,#40152,#40153,#40154,#40155,#40156,#40157,#40158,#40159,
#40160,#40161,#40162,#40163,#40164,#40165,#40166,#40167,#40168,#40169,#40170,
#40171,#40172,#40173,#40174,#40175,#40176,#40177,#40178,#40179,#40180,#40181,
#40182,#40183,#40184,#40185,#40186,#40187,#40188,#40189,#40190,#40191,#40192,
#40193,#40194,#40195,#40196,#40197,#40198,#40199,#40200,#40201,#40202,#40203,
#40204,#40205,#40206,#40207,#40208,#40209,#40210,#40211,#40212,#40213,#40214,
#40215,#40216,#40217,#40218,#40219,#40220,#40221,#40222,#40223,#40224,#40225,
#40226,#40227,#40228,#40229,#40230,#40231)),.UNSPECIFIED.,.F.,.F.,.F.,(4,
4),(4,1,1,1,1,1,1,1,1,1,1,1,1,1,1,1,1,1,1,1,1,1,1,1,1,1,1,1,1,1,1,1,1,1,
1,1,1,1,1,1,1,1,1,1,1,1,1,1,1,1,1,1,1,1,1,1,1,1,1,1,1,1,1,1,1,1,1,1,1,1,
1,1,1,1,1,1,1,1,1,1,1,1,1,1,1,1,1,1,1,1,1,1,1,1,1,1,1,1,1,1,1,1,1,1,1,1,
1,1,1,1,1,1,1,1,1,1,1,1,1,1,1,1,1,1,1,1,1,1,1,1,1,1,1,1,1,1,1,1,1,1,1,1,
1,1,1,1,1,1,1,1,1,1,1,1,1,1,1,1,1,1,1,1,1,1,1,1,1,1,1,1,1,1,1,1,1,1,1,1,
1,1,1,1,1,1,1,1,1,1,1,1,1,1,1,1,1,1,1,1,1,1,1,1,1,1,1,1,1,1,1,1,1,1,1,1,
1,1,1,1,1,1,1,1,1,1,1,1,1,1,1,1,1,1,1,1,1,1,1,1,1,1,1,1,1,1,1,1,1,1,1,1,
1,1,1,1,1,1,1,1,1,1,1,1,1,1,1,1,1,1,1,1,1,1,1,1,1,1,1,1,1,1,1,1,1,1,1,1,
1,1,1,1,1,1,1,1,1,1,1,1,1,1,1,1,1,1,1,1,1,1,1,1,1,1,1,1,1,1,1,1,1,1,1,1,
1,1,1,1,1,1,1,1,1,1,1,1,1,1,1,1,1,1,1,1,1,1,1,1,1,1,1,1,1,1,1,1,1,1,1,1,
1,1,1,1,1,1,1,1,1,1,1,1,1,1,1,1,1,1,1,1,1,1,1,1,1,1,1,1,1,1,1,1,1,1,1,1,
1,1,1,1,1,1,1,1,1,1,1,1,1,1,1,1,1,1,1,1,1,1,1,1,1,1,1,1,1,1,1,1,1,1,1,1,
1,1,1,1,1,1,1,1,1,1,1,1,1,1,1,1,1,1,1,1,1,1,1,1,1,1,1,1,1,1,1,1,1,1,1,1,
1,1,1,1,1,1,1,1,1,1,1,1,1,1,1,1,1,1,1,1,1,1,1,1,1,1,1,1,4),(0.,0.0641840294258107),
(14.3989442667815,14.8976525601681,15.3963608535547,15.8950691469414,16.393777440328,
16.8924857337146,17.3911940271012,17.8899023204878,18.3886106138744,18.8873189072611,
19.3860272006477,19.8847354940343,20.3834437874209,20.8821520808075,21.3808603741942,
21.8795686675808,22.3782769609674,22.876985254354,23.3756935477406,23.8744018411273,
24.3731101345139,24.8718184279005,25.3705267212871,25.8692350146737,26.3679433080604,
26.866651601447,27.3653598948336,27.8640681882202,28.3627764816068,28.8614847749935,
29.3601930683801,29.8589013617667,30.3576096551533,30.8563179485399,31.3550262419266,
31.8537345353132,32.3524428286998,32.8511511220864,33.349859415473,33.8485677088597,
34.3472760022463,34.8459842956329,35.3446925890195,35.8434008824061,36.3421091757927,
36.8408174691794,37.339525762566,37.8382340559526,38.3369423493392,38.8356506427259,
39.3343589361125,39.8330672294991,40.3317755228857,40.8304838162723,41.3291921096589,
41.8279004030456,42.3266086964322,42.8253169898188,43.3240252832054,43.822733576592,
44.3214418699787,44.8201501633653,45.3188584567519,45.8175667501385,46.3162750435251,
46.8149833369118,47.3136916302984,47.812399923685,48.3111082170716,48.8098165104582,
49.3085248038449,49.8072330972315,50.3059413906181,50.8046496840047,51.3033579773913,
51.802066270778,52.3007745641646,52.7994828575512,53.2981911509378,53.7968994443244,
54.2956077377111,54.7943160310977,55.2930243244843,55.7917326178709,56.2904409112575,
56.7891492046442,57.2878574980308,57.7865657914174,58.285274084804,58.7839823781906,
59.2826906715772,59.7813989649639,60.2801072583505,60.7788155517371,61.2775238451237,
61.7762321385104,62.274940431897,62.7736487252836,63.2723570186702,63.7710653120568,
64.2697736054434,64.7684818988301,65.2671901922167,65.7658984856033,66.2646067789899,
66.7633150723765,67.2620233657632,67.7607316591498,68.2594399525364,68.758148245923,
69.2568565393096,69.7555648326963,70.2542731260829,70.7529814194695,71.2516897128561,
71.7503980062427,72.2491062996294,72.747814593016,73.2465228864026,73.7452311797892,
74.2439394731758,74.7426477665625,75.2413560599491,75.7400643533357,76.2387726467223,
76.7374809401089,77.2361892334956,77.7348975268822,78.2336058202688,78.7323141136554,
79.231022407042,79.7297307004287,80.2284389938153,80.7271472872019,81.2258555805885,
81.7245638739751,82.2232721673618,82.7219804607484,83.220688754135,83.7193970475216,
84.2181053409082,84.7168136342949,85.2155219276815,85.7142302210681,86.2129385144547,
86.7116468078413,87.2103551012279,87.7090633946146,88.2077716880012,88.7064799813878,
89.2051882747744,89.703896568161,90.2026048615477,90.7013131549343,91.2000214483209,
91.6987297417075,92.1974380350942,92.6961463284808,93.1948546218674,93.693562915254,
94.1922712086406,94.6909795020272,95.1896877954139,95.6883960888005,96.1871043821871,
96.6858126755737,97.1845209689603,97.683229262347,98.1819375557336,98.6806458491202,
99.1793541425068,99.6780624358935,100.17677072928,100.675479022667,101.174187316053,
101.67289560944,102.171603902827,102.670312196213,103.1690204896,103.667728782986,
104.166437076373,104.66514536976,105.163853663146,105.662561956533,106.161270249919,
106.659978543306,107.158686836693,107.657395130079,108.156103423466,108.654811716853,
109.153520010239,109.652228303626,110.150936597012,110.649644890399,111.148353183786,
111.647061477172,112.145769770559,112.644478063946,113.143186357332,113.641894650719,
114.140602944105,114.639311237492,115.138019530879,115.636727824265,116.135436117652,
116.634144411039,117.132852704425,117.631560997812,118.130269291198,118.628977584585,
119.127685877972,119.626394171358,120.125102464745,120.623810758131,121.122519051518,
121.621227344905,122.119935638291,122.618643931678,123.117352225065,123.616060518451,
124.114768811838,124.613477105224,125.112185398611,125.610893691998,126.109601985384,
126.608310278771,127.107018572158,127.605726865544,128.104435158931,128.603143452317,
129.101851745704,129.600560039091,130.099268332477,130.597976625864,131.09668491925,
131.595393212637,132.094101506024,132.59280979941,133.091518092797,133.590226386184,
134.08893467957,135.086351266343,136.083767853117,137.08118443989,138.078601026663,
139.076017613436,140.07343420021,141.070850786983,142.068267373756,143.065683960529,
144.063100547303,145.060517134076,146.057933720849,147.055350307622,148.052766894396,
148.551475187782,149.050183481169,149.548891774555,150.047600067942,150.546308361329,
151.045016654715,151.543724948102,152.042433241488,152.541141534875,153.039849828262,
153.538558121648,154.037266415035,154.535974708422,155.034683001808,155.533391295195,
156.032099588581,156.530807881968,157.029516175355,157.528224468741,158.026932762128,
158.525641055515,159.024349348901,159.523057642288,160.021765935674,160.520474229061,
161.019182522448,161.517890815834,162.016599109221,162.515307402608,163.014015695994,
163.512723989381,164.011432282767,164.510140576154,165.008848869541,165.507557162927,
166.006265456314,166.5049737497,167.003682043087,167.502390336474,168.00109862986,
168.499806923247,168.998515216634,169.49722351002,169.995931803407,170.494640096793,
170.99334839018,171.492056683567,171.990764976953,172.48947327034,172.988181563726,
173.486889857113,173.9855981505,174.484306443886,174.983014737273,175.48172303066,
175.980431324046,176.479139617433,176.977847910819,177.476556204206,177.975264497593,
178.473972790979,178.972681084366,179.471389377753,179.970097671139,180.468805964526,
180.967514257912,181.466222551299,181.964930844686,182.463639138072,182.962347431459,
183.461055724845,183.959764018232,184.458472311619,184.957180605005,185.455888898392,
185.954597191779,186.453305485165,186.952013778552,187.450722071938,187.949430365325,
188.448138658712,188.946846952098,189.445555245485,189.944263538872,190.442971832258,
190.941680125645,191.440388419031,191.939096712418,192.437805005805,192.936513299191,
193.435221592578,193.933929885965,194.432638179351,194.931346472738,195.430054766124,
195.928763059511,196.427471352898,196.926179646284,197.424887939671,197.923596233057,
198.422304526444,198.921012819831,199.419721113217,199.918429406604,200.417137699991,
200.915845993377,201.414554286764,201.91326258015,202.411970873537,202.910679166924,
203.40938746031,203.908095753697,204.406804047084,204.90551234047,205.404220633857,
205.902928927243,206.40163722063,206.900345514017,207.399053807403,207.89776210079,
208.396470394177,208.895178687563,209.39388698095,209.892595274336,210.391303567723,
210.89001186111,211.388720154496,211.887428447883,212.386136741269,212.884845034656,
213.383553328043,213.882261621429,214.380969914816,214.879678208203,215.378386501589,
215.877094794976,216.375803088362,216.874511381749,217.373219675136,217.871927968522,
218.370636261909,218.869344555295,219.368052848682,219.866761142069,220.365469435455,
220.864177728842,221.362886022229,221.861594315615,222.360302609002,222.859010902388,
223.357719195775,223.856427489162,224.355135782548,224.853844075935,225.352552369322,
225.851260662708,226.349968956095,226.848677249481,227.347385542868,227.846093836255,
228.344802129641,228.843510423028,229.342218716414,229.840927009801,230.339635303188,
230.838343596574,231.337051889961,231.835760183348,232.334468476734,232.833176770121,
233.331885063507,233.830593356894,234.329301650281,234.828009943667,235.326718237054,
235.825426530441,236.324134823827,236.822843117214,237.3215514106,237.820259703987,
238.318967997374,238.81767629076,239.316384584147,239.815092877534,240.31380117092,
240.812509464307,241.311217757693,241.80992605108,242.308634344467,242.807342637853,
243.30605093124,243.804759224626,244.303467518013,244.8021758114,245.300884104786,
245.799592398173,246.29830069156,246.797008984946,247.295717278333,247.794425571719,
248.293133865106,248.791842158493,249.290550451879,249.789258745266,250.287967038653,
250.786675332039,251.285383625426,251.784091918812,252.282800212199,252.781508505586,
253.280216798972,253.778925092359,254.277633385745,254.776341679132,255.275049972519,
255.773758265905,256.272466559292,256.771174852679,257.269883146065,257.768591439452,
258.267299732838,258.766008026225,259.264716319612,259.763424612998,260.262132906385,
260.760841199772,261.259549493158,261.758257786545,262.256966079931,262.755674373318,
263.254382666705,263.753090960091,264.251799253478,264.750507546865,265.249215840251,
265.747924133638,266.246632427024,266.745340720411,267.244049013798,267.742757307184),
 .UNSPECIFIED.);
#269=B_SPLINE_SURFACE_WITH_KNOTS('',3,3,((#40624,#40625,#40626,#40627,#40628,
#40629,#40630,#40631,#40632,#40633,#40634,#40635,#40636,#40637,#40638,#40639,
#40640,#40641,#40642,#40643,#40644,#40645,#40646,#40647,#40648,#40649,#40650,
#40651,#40652,#40653,#40654,#40655,#40656,#40657,#40658,#40659,#40660,#40661,
#40662,#40663,#40664,#40665,#40666,#40667,#40668,#40669,#40670,#40671,#40672,
#40673,#40674,#40675,#40676,#40677,#40678,#40679,#40680,#40681,#40682,#40683,
#40684,#40685,#40686,#40687,#40688,#40689,#40690,#40691,#40692,#40693,#40694,
#40695,#40696,#40697,#40698,#40699,#40700,#40701,#40702,#40703,#40704,#40705,
#40706,#40707,#40708,#40709,#40710,#40711,#40712,#40713,#40714,#40715,#40716,
#40717,#40718,#40719,#40720,#40721,#40722,#40723,#40724,#40725,#40726,#40727,
#40728,#40729,#40730,#40731,#40732,#40733,#40734,#40735,#40736,#40737,#40738,
#40739,#40740,#40741,#40742,#40743,#40744,#40745,#40746,#40747,#40748,#40749,
#40750,#40751,#40752,#40753,#40754,#40755,#40756,#40757,#40758,#40759,#40760,
#40761,#40762,#40763,#40764,#40765,#40766,#40767,#40768,#40769,#40770,#40771,
#40772,#40773,#40774,#40775,#40776,#40777,#40778,#40779,#40780,#40781,#40782,
#40783,#40784,#40785,#40786,#40787,#40788,#40789,#40790,#40791,#40792,#40793,
#40794,#40795,#40796,#40797,#40798,#40799,#40800,#40801,#40802,#40803,#40804,
#40805,#40806,#40807,#40808,#40809,#40810,#40811,#40812,#40813,#40814,#40815,
#40816,#40817,#40818,#40819,#40820,#40821,#40822,#40823,#40824,#40825,#40826,
#40827,#40828,#40829,#40830,#40831,#40832,#40833,#40834,#40835,#40836,#40837,
#40838,#40839,#40840,#40841,#40842,#40843,#40844,#40845,#40846,#40847,#40848,
#40849,#40850,#40851,#40852,#40853,#40854,#40855,#40856,#40857,#40858,#40859,
#40860,#40861,#40862,#40863,#40864,#40865,#40866,#40867,#40868,#40869,#40870,
#40871,#40872,#40873,#40874,#40875,#40876,#40877,#40878,#40879,#40880,#40881,
#40882,#40883,#40884,#40885,#40886,#40887,#40888,#40889,#40890,#40891,#40892,
#40893,#40894,#40895,#40896,#40897,#40898,#40899,#40900,#40901,#40902,#40903,
#40904,#40905,#40906,#40907,#40908,#40909,#40910,#40911,#40912,#40913,#40914,
#40915,#40916,#40917,#40918,#40919,#40920,#40921,#40922,#40923,#40924,#40925,
#40926,#40927,#40928,#40929,#40930,#40931,#40932,#40933,#40934,#40935,#40936,
#40937,#40938,#40939,#40940,#40941,#40942,#40943,#40944,#40945,#40946),
(#40947,#40948,#40949,#40950,#40951,#40952,#40953,#40954,#40955,#40956,
#40957,#40958,#40959,#40960,#40961,#40962,#40963,#40964,#40965,#40966,#40967,
#40968,#40969,#40970,#40971,#40972,#40973,#40974,#40975,#40976,#40977,#40978,
#40979,#40980,#40981,#40982,#40983,#40984,#40985,#40986,#40987,#40988,#40989,
#40990,#40991,#40992,#40993,#40994,#40995,#40996,#40997,#40998,#40999,#41000,
#41001,#41002,#41003,#41004,#41005,#41006,#41007,#41008,#41009,#41010,#41011,
#41012,#41013,#41014,#41015,#41016,#41017,#41018,#41019,#41020,#41021,#41022,
#41023,#41024,#41025,#41026,#41027,#41028,#41029,#41030,#41031,#41032,#41033,
#41034,#41035,#41036,#41037,#41038,#41039,#41040,#41041,#41042,#41043,#41044,
#41045,#41046,#41047,#41048,#41049,#41050,#41051,#41052,#41053,#41054,#41055,
#41056,#41057,#41058,#41059,#41060,#41061,#41062,#41063,#41064,#41065,#41066,
#41067,#41068,#41069,#41070,#41071,#41072,#41073,#41074,#41075,#41076,#41077,
#41078,#41079,#41080,#41081,#41082,#41083,#41084,#41085,#41086,#41087,#41088,
#41089,#41090,#41091,#41092,#41093,#41094,#41095,#41096,#41097,#41098,#41099,
#41100,#41101,#41102,#41103,#41104,#41105,#41106,#41107,#41108,#41109,#41110,
#41111,#41112,#41113,#41114,#41115,#41116,#41117,#41118,#41119,#41120,#41121,
#41122,#41123,#41124,#41125,#41126,#41127,#41128,#41129,#41130,#41131,#41132,
#41133,#41134,#41135,#41136,#41137,#41138,#41139,#41140,#41141,#41142,#41143,
#41144,#41145,#41146,#41147,#41148,#41149,#41150,#41151,#41152,#41153,#41154,
#41155,#41156,#41157,#41158,#41159,#41160,#41161,#41162,#41163,#41164,#41165,
#41166,#41167,#41168,#41169,#41170,#41171,#41172,#41173,#41174,#41175,#41176,
#41177,#41178,#41179,#41180,#41181,#41182,#41183,#41184,#41185,#41186,#41187,
#41188,#41189,#41190,#41191,#41192,#41193,#41194,#41195,#41196,#41197,#41198,
#41199,#41200,#41201,#41202,#41203,#41204,#41205,#41206,#41207,#41208,#41209,
#41210,#41211,#41212,#41213,#41214,#41215,#41216,#41217,#41218,#41219,#41220,
#41221,#41222,#41223,#41224,#41225,#41226,#41227,#41228,#41229,#41230,#41231,
#41232,#41233,#41234,#41235,#41236,#41237,#41238,#41239,#41240,#41241,#41242,
#41243,#41244,#41245,#41246,#41247,#41248,#41249,#41250,#41251,#41252,#41253,
#41254,#41255,#41256,#41257,#41258,#41259,#41260,#41261,#41262,#41263,#41264,
#41265,#41266,#41267,#41268,#41269),(#41270,#41271,#41272,#41273,#41274,
#41275,#41276,#41277,#41278,#41279,#41280,#41281,#41282,#41283,#41284,#41285,
#41286,#41287,#41288,#41289,#41290,#41291,#41292,#41293,#41294,#41295,#41296,
#41297,#41298,#41299,#41300,#41301,#41302,#41303,#41304,#41305,#41306,#41307,
#41308,#41309,#41310,#41311,#41312,#41313,#41314,#41315,#41316,#41317,#41318,
#41319,#41320,#41321,#41322,#41323,#41324,#41325,#41326,#41327,#41328,#41329,
#41330,#41331,#41332,#41333,#41334,#41335,#41336,#41337,#41338,#41339,#41340,
#41341,#41342,#41343,#41344,#41345,#41346,#41347,#41348,#41349,#41350,#41351,
#41352,#41353,#41354,#41355,#41356,#41357,#41358,#41359,#41360,#41361,#41362,
#41363,#41364,#41365,#41366,#41367,#41368,#41369,#41370,#41371,#41372,#41373,
#41374,#41375,#41376,#41377,#41378,#41379,#41380,#41381,#41382,#41383,#41384,
#41385,#41386,#41387,#41388,#41389,#41390,#41391,#41392,#41393,#41394,#41395,
#41396,#41397,#41398,#41399,#41400,#41401,#41402,#41403,#41404,#41405,#41406,
#41407,#41408,#41409,#41410,#41411,#41412,#41413,#41414,#41415,#41416,#41417,
#41418,#41419,#41420,#41421,#41422,#41423,#41424,#41425,#41426,#41427,#41428,
#41429,#41430,#41431,#41432,#41433,#41434,#41435,#41436,#41437,#41438,#41439,
#41440,#41441,#41442,#41443,#41444,#41445,#41446,#41447,#41448,#41449,#41450,
#41451,#41452,#41453,#41454,#41455,#41456,#41457,#41458,#41459,#41460,#41461,
#41462,#41463,#41464,#41465,#41466,#41467,#41468,#41469,#41470,#41471,#41472,
#41473,#41474,#41475,#41476,#41477,#41478,#41479,#41480,#41481,#41482,#41483,
#41484,#41485,#41486,#41487,#41488,#41489,#41490,#41491,#41492,#41493,#41494,
#41495,#41496,#41497,#41498,#41499,#41500,#41501,#41502,#41503,#41504,#41505,
#41506,#41507,#41508,#41509,#41510,#41511,#41512,#41513,#41514,#41515,#41516,
#41517,#41518,#41519,#41520,#41521,#41522,#41523,#41524,#41525,#41526,#41527,
#41528,#41529,#41530,#41531,#41532,#41533,#41534,#41535,#41536,#41537,#41538,
#41539,#41540,#41541,#41542,#41543,#41544,#41545,#41546,#41547,#41548,#41549,
#41550,#41551,#41552,#41553,#41554,#41555,#41556,#41557,#41558,#41559,#41560,
#41561,#41562,#41563,#41564,#41565,#41566,#41567,#41568,#41569,#41570,#41571,
#41572,#41573,#41574,#41575,#41576,#41577,#41578,#41579,#41580,#41581,#41582,
#41583,#41584,#41585,#41586,#41587,#41588,#41589,#41590,#41591,#41592),
(#41593,#41594,#41595,#41596,#41597,#41598,#41599,#41600,#41601,#41602,
#41603,#41604,#41605,#41606,#41607,#41608,#41609,#41610,#41611,#41612,#41613,
#41614,#41615,#41616,#41617,#41618,#41619,#41620,#41621,#41622,#41623,#41624,
#41625,#41626,#41627,#41628,#41629,#41630,#41631,#41632,#41633,#41634,#41635,
#41636,#41637,#41638,#41639,#41640,#41641,#41642,#41643,#41644,#41645,#41646,
#41647,#41648,#41649,#41650,#41651,#41652,#41653,#41654,#41655,#41656,#41657,
#41658,#41659,#41660,#41661,#41662,#41663,#41664,#41665,#41666,#41667,#41668,
#41669,#41670,#41671,#41672,#41673,#41674,#41675,#41676,#41677,#41678,#41679,
#41680,#41681,#41682,#41683,#41684,#41685,#41686,#41687,#41688,#41689,#41690,
#41691,#41692,#41693,#41694,#41695,#41696,#41697,#41698,#41699,#41700,#41701,
#41702,#41703,#41704,#41705,#41706,#41707,#41708,#41709,#41710,#41711,#41712,
#41713,#41714,#41715,#41716,#41717,#41718,#41719,#41720,#41721,#41722,#41723,
#41724,#41725,#41726,#41727,#41728,#41729,#41730,#41731,#41732,#41733,#41734,
#41735,#41736,#41737,#41738,#41739,#41740,#41741,#41742,#41743,#41744,#41745,
#41746,#41747,#41748,#41749,#41750,#41751,#41752,#41753,#41754,#41755,#41756,
#41757,#41758,#41759,#41760,#41761,#41762,#41763,#41764,#41765,#41766,#41767,
#41768,#41769,#41770,#41771,#41772,#41773,#41774,#41775,#41776,#41777,#41778,
#41779,#41780,#41781,#41782,#41783,#41784,#41785,#41786,#41787,#41788,#41789,
#41790,#41791,#41792,#41793,#41794,#41795,#41796,#41797,#41798,#41799,#41800,
#41801,#41802,#41803,#41804,#41805,#41806,#41807,#41808,#41809,#41810,#41811,
#41812,#41813,#41814,#41815,#41816,#41817,#41818,#41819,#41820,#41821,#41822,
#41823,#41824,#41825,#41826,#41827,#41828,#41829,#41830,#41831,#41832,#41833,
#41834,#41835,#41836,#41837,#41838,#41839,#41840,#41841,#41842,#41843,#41844,
#41845,#41846,#41847,#41848,#41849,#41850,#41851,#41852,#41853,#41854,#41855,
#41856,#41857,#41858,#41859,#41860,#41861,#41862,#41863,#41864,#41865,#41866,
#41867,#41868,#41869,#41870,#41871,#41872,#41873,#41874,#41875,#41876,#41877,
#41878,#41879,#41880,#41881,#41882,#41883,#41884,#41885,#41886,#41887,#41888,
#41889,#41890,#41891,#41892,#41893,#41894,#41895,#41896,#41897,#41898,#41899,
#41900,#41901,#41902,#41903,#41904,#41905,#41906,#41907,#41908,#41909,#41910,
#41911,#41912,#41913,#41914,#41915)),.UNSPECIFIED.,.F.,.F.,.F.,(4,4),(4,
1,1,1,1,1,1,1,1,1,1,1,1,1,1,1,1,1,1,1,1,1,1,1,1,1,1,1,1,1,1,1,1,1,1,1,1,
1,1,1,1,1,1,1,1,1,1,1,1,1,1,1,1,1,1,1,1,1,1,1,1,1,1,1,1,1,1,1,1,1,1,1,1,
1,1,1,1,1,1,1,1,1,1,1,1,1,1,1,1,1,1,1,1,1,1,1,1,1,1,1,1,1,1,1,1,1,1,1,1,
1,1,1,1,1,1,1,1,1,1,1,1,1,1,1,1,1,1,1,1,1,1,1,1,1,1,1,1,1,1,1,1,1,1,1,1,
1,1,1,1,1,1,1,1,1,1,1,1,1,1,1,1,1,1,1,1,1,1,1,1,1,1,1,1,1,1,1,1,1,1,1,1,
1,1,1,1,1,1,1,1,1,1,1,1,1,1,1,1,1,1,1,1,1,1,1,1,1,1,1,1,1,1,1,1,1,1,1,1,
1,1,1,1,1,1,1,1,1,1,1,1,1,1,1,1,1,1,1,1,1,1,1,1,1,1,1,1,1,1,1,1,1,1,1,1,
1,1,1,1,1,1,1,1,1,1,1,1,1,1,1,1,1,1,1,1,1,1,1,1,1,1,1,1,1,1,1,1,1,1,1,1,
1,1,1,1,1,1,1,1,1,1,1,1,1,1,1,1,1,1,1,1,1,1,1,1,1,1,1,1,1,1,1,4),(0.,0.0641840294258124),
(11.8589888623079,12.3561639667852,12.8533390712624,13.3505141757396,13.8476892802168,
14.344864384694,14.8420394891712,15.3392145936484,15.8363896981257,16.3335648026029,
16.8307399070801,17.3279150115573,17.8250901160345,18.3222652205117,18.8194403249889,
19.3166154294662,19.8137905339434,20.3109656384206,20.8081407428978,21.305315847375,
21.8024909518522,22.2996660563294,22.7968411608067,23.2940162652839,23.7911913697611,
24.2883664742383,24.7855415787155,25.2827166831927,25.7798917876699,26.2770668921472,
26.7742419966244,27.2714171011016,27.7685922055788,28.265767310056,28.7629424145332,
29.2601175190104,29.7572926234877,30.2544677279649,30.7516428324421,31.2488179369193,
31.7459930413965,32.2431681458737,32.7403432503509,33.2375183548282,33.7346934593054,
34.2318685637826,34.7290436682598,35.226218772737,35.7233938772142,36.2205689816915,
36.7177440861687,37.2149191906459,37.7120942951231,38.2092693996003,38.7064445040775,
39.2036196085547,39.700794713032,40.1979698175092,40.6951449219864,41.1923200264636,
41.6894951309408,42.186670235418,42.6838453398952,43.1810204443725,43.6781955488497,
44.1753706533269,44.6725457578041,45.1697208622813,45.6668959667585,46.1640710712357,
46.661246175713,47.1584212801902,47.6555963846674,48.1527714891446,48.6499465936218,
49.147121698099,49.6442968025762,50.1414719070535,50.6386470115307,51.1358221160079,
51.6329972204851,52.1301723249623,52.6273474294395,53.1245225339167,53.621697638394,
54.1188727428712,54.6160478473484,55.1132229518256,55.6103980563028,56.10757316078,
56.6047482652572,57.1019233697345,57.5990984742117,58.0962735786889,58.5934486831661,
59.0906237876433,59.5877988921205,60.0849739965977,60.582149101075,61.0793242055522,
61.5764993100294,62.0736744145066,62.5708495189838,63.068024623461,63.5651997279382,
64.0623748324155,64.5595499368927,65.0567250413699,65.5539001458471,66.0510752503243,
66.5482503548015,67.0454254592788,67.542600563756,68.0397756682332,68.5369507727104,
69.0341258771876,69.5313009816648,70.028476086142,70.5256511906192,71.0228262950965,
71.5200013995737,72.0171765040509,72.5143516085281,73.0115267130053,73.5087018174825,
74.0058769219598,74.503052026437,75.0002271309142,75.4974022353914,75.9945773398686,
76.4917524443458,76.988927548823,77.4861026533003,77.9832777577775,78.4804528622547,
78.9776279667319,79.4748030712091,79.9719781756863,80.4691532801635,80.9663283846407,
81.463503489118,81.9606785935952,82.4578536980724,82.9550288025496,83.4522039070268,
83.949379011504,84.4465541159813,84.9437292204585,85.4409043249357,85.9380794294129,
86.4352545338901,86.9324296383673,87.4296047428445,87.9267798473217,88.423954951799,
88.9211300562762,89.4183051607534,89.9154802652306,90.4126553697078,90.909830474185,
91.4070055786623,91.9041806831395,92.4013557876167,92.8985308920939,93.3957059965711,
93.8928811010483,94.3900562055255,94.8872313100028,95.38440641448,95.8815815189572,
96.3787566234344,96.8759317279116,97.3731068323888,97.870281936866,98.3674570413433,
98.8646321458205,99.3618072502977,99.8589823547749,100.356157459252,100.853332563729,
101.350507668207,101.847682772684,102.344857877161,102.842032981638,103.339208086115,
103.836383190593,104.33355829507,104.830733399547,105.327908504024,105.825083608501,
106.322258712979,106.819433817456,107.316608921933,107.81378402641,108.310959130888,
108.808134235365,109.305309339842,109.802484444319,110.299659548796,110.796834653274,
111.294009757751,111.791184862228,112.288359966705,112.785535071182,113.28271017566,
113.779885280137,114.277060384614,114.774235489091,115.271410593569,115.768585698046,
116.265760802523,116.762935907,117.260111011477,117.757286115955,118.254461220432,
118.751636324909,119.248811429386,119.745986533863,120.243161638341,120.740336742818,
121.237511847295,121.734686951772,122.23186205625,122.729037160727,123.226212265204,
123.723387369681,124.220562474158,124.717737578636,125.214912683113,125.71208778759,
126.209262892067,126.706437996544,127.203613101022,127.700788205499,128.197963309976,
128.695138414453,129.192313518931,129.689488623408,130.186663727885,130.683838832362,
131.181013936839,131.678189041317,132.175364145794,132.672539250271,133.169714354748,
133.666889459226,134.164064563703,134.66123966818,135.158414772657,135.655589877134,
136.152764981612,136.649940086089,137.147115190566,137.644290295043,138.14146539952,
138.638640503998,139.135815608475,139.632990712952,140.130165817429,140.627340921906,
141.124516026384,141.621691130861,142.118866235338,142.616041339815,143.113216444293,
143.61039154877,144.107566653247,144.604741757724,145.101916862201,145.599091966679,
146.096267071156,146.593442175633,147.09061728011,147.587792384587,148.084967489065,
148.582142593542,149.079317698019,149.576492802496,150.073667906974,150.570843011451,
151.068018115928,151.565193220405,152.062368324882,152.55954342936,153.056718533837,
153.553893638314,154.051068742791,154.548243847269,155.045418951746,155.542594056223,
156.0397691607,156.536944265177,157.034119369655,157.531294474132,158.028469578609,
158.525644683086,159.022819787563,159.519994892041,160.017169996518,160.514345100995,
161.011520205472,161.508695309949,162.005870414427,162.503045518904,163.000220623381,
163.497395727858,163.994570832336,164.491745936813,164.98892104129,165.486096145767,
165.983271250244,166.480446354722,166.977621459199,167.474796563676,167.971971668153,
168.46914677263,168.966321877108,169.463496981585,169.960672086062,170.457847190539,
170.955022295017),.UNSPECIFIED.);
#270=B_SPLINE_SURFACE_WITH_KNOTS('',3,3,((#42065,#42066,#42067,#42068,#42069,
#42070,#42071,#42072,#42073,#42074,#42075,#42076,#42077,#42078,#42079,#42080,
#42081,#42082,#42083,#42084,#42085,#42086,#42087,#42088,#42089,#42090,#42091,
#42092,#42093,#42094,#42095,#42096,#42097,#42098,#42099,#42100,#42101,#42102,
#42103,#42104,#42105,#42106,#42107,#42108,#42109,#42110,#42111,#42112,#42113,
#42114,#42115,#42116,#42117,#42118,#42119,#42120,#42121,#42122,#42123,#42124,
#42125,#42126,#42127,#42128,#42129,#42130,#42131,#42132,#42133,#42134,#42135,
#42136,#42137,#42138,#42139,#42140,#42141,#42142,#42143,#42144,#42145,#42146,
#42147,#42148,#42149,#42150,#42151,#42152,#42153,#42154,#42155,#42156,#42157,
#42158,#42159,#42160,#42161,#42162,#42163,#42164,#42165,#42166,#42167,#42168,
#42169,#42170,#42171,#42172,#42173,#42174,#42175,#42176,#42177,#42178,#42179,
#42180,#42181,#42182,#42183,#42184,#42185,#42186,#42187,#42188,#42189,#42190,
#42191,#42192,#42193,#42194,#42195,#42196,#42197,#42198,#42199,#42200,#42201,
#42202,#42203,#42204,#42205,#42206,#42207,#42208,#42209,#42210,#42211,#42212,
#42213,#42214,#42215,#42216,#42217,#42218,#42219,#42220,#42221,#42222,#42223,
#42224,#42225,#42226,#42227,#42228,#42229,#42230,#42231,#42232,#42233,#42234,
#42235,#42236,#42237,#42238,#42239,#42240,#42241,#42242,#42243,#42244,#42245,
#42246,#42247,#42248,#42249,#42250,#42251,#42252,#42253,#42254,#42255,#42256,
#42257,#42258,#42259,#42260,#42261,#42262,#42263,#42264,#42265,#42266,#42267,
#42268,#42269,#42270,#42271,#42272,#42273,#42274,#42275,#42276,#42277,#42278,
#42279,#42280,#42281,#42282,#42283,#42284,#42285,#42286,#42287,#42288,#42289,
#42290,#42291,#42292,#42293,#42294,#42295,#42296,#42297,#42298,#42299,#42300,
#42301,#42302,#42303,#42304,#42305,#42306,#42307,#42308,#42309,#42310,#42311,
#42312,#42313,#42314,#42315,#42316,#42317,#42318,#42319,#42320,#42321,#42322,
#42323,#42324,#42325,#42326,#42327,#42328,#42329,#42330,#42331,#42332,#42333,
#42334,#42335,#42336,#42337,#42338,#42339,#42340,#42341,#42342,#42343,#42344,
#42345,#42346,#42347,#42348,#42349,#42350,#42351,#42352,#42353,#42354,#42355,
#42356,#42357,#42358,#42359,#42360,#42361,#42362,#42363,#42364,#42365,#42366,
#42367,#42368,#42369,#42370,#42371,#42372,#42373,#42374,#42375,#42376,#42377,
#42378,#42379,#42380,#42381,#42382,#42383,#42384,#42385,#42386,#42387),
(#42388,#42389,#42390,#42391,#42392,#42393,#42394,#42395,#42396,#42397,
#42398,#42399,#42400,#42401,#42402,#42403,#42404,#42405,#42406,#42407,#42408,
#42409,#42410,#42411,#42412,#42413,#42414,#42415,#42416,#42417,#42418,#42419,
#42420,#42421,#42422,#42423,#42424,#42425,#42426,#42427,#42428,#42429,#42430,
#42431,#42432,#42433,#42434,#42435,#42436,#42437,#42438,#42439,#42440,#42441,
#42442,#42443,#42444,#42445,#42446,#42447,#42448,#42449,#42450,#42451,#42452,
#42453,#42454,#42455,#42456,#42457,#42458,#42459,#42460,#42461,#42462,#42463,
#42464,#42465,#42466,#42467,#42468,#42469,#42470,#42471,#42472,#42473,#42474,
#42475,#42476,#42477,#42478,#42479,#42480,#42481,#42482,#42483,#42484,#42485,
#42486,#42487,#42488,#42489,#42490,#42491,#42492,#42493,#42494,#42495,#42496,
#42497,#42498,#42499,#42500,#42501,#42502,#42503,#42504,#42505,#42506,#42507,
#42508,#42509,#42510,#42511,#42512,#42513,#42514,#42515,#42516,#42517,#42518,
#42519,#42520,#42521,#42522,#42523,#42524,#42525,#42526,#42527,#42528,#42529,
#42530,#42531,#42532,#42533,#42534,#42535,#42536,#42537,#42538,#42539,#42540,
#42541,#42542,#42543,#42544,#42545,#42546,#42547,#42548,#42549,#42550,#42551,
#42552,#42553,#42554,#42555,#42556,#42557,#42558,#42559,#42560,#42561,#42562,
#42563,#42564,#42565,#42566,#42567,#42568,#42569,#42570,#42571,#42572,#42573,
#42574,#42575,#42576,#42577,#42578,#42579,#42580,#42581,#42582,#42583,#42584,
#42585,#42586,#42587,#42588,#42589,#42590,#42591,#42592,#42593,#42594,#42595,
#42596,#42597,#42598,#42599,#42600,#42601,#42602,#42603,#42604,#42605,#42606,
#42607,#42608,#42609,#42610,#42611,#42612,#42613,#42614,#42615,#42616,#42617,
#42618,#42619,#42620,#42621,#42622,#42623,#42624,#42625,#42626,#42627,#42628,
#42629,#42630,#42631,#42632,#42633,#42634,#42635,#42636,#42637,#42638,#42639,
#42640,#42641,#42642,#42643,#42644,#42645,#42646,#42647,#42648,#42649,#42650,
#42651,#42652,#42653,#42654,#42655,#42656,#42657,#42658,#42659,#42660,#42661,
#42662,#42663,#42664,#42665,#42666,#42667,#42668,#42669,#42670,#42671,#42672,
#42673,#42674,#42675,#42676,#42677,#42678,#42679,#42680,#42681,#42682,#42683,
#42684,#42685,#42686,#42687,#42688,#42689,#42690,#42691,#42692,#42693,#42694,
#42695,#42696,#42697,#42698,#42699,#42700,#42701,#42702,#42703,#42704,#42705,
#42706,#42707,#42708,#42709,#42710),(#42711,#42712,#42713,#42714,#42715,
#42716,#42717,#42718,#42719,#42720,#42721,#42722,#42723,#42724,#42725,#42726,
#42727,#42728,#42729,#42730,#42731,#42732,#42733,#42734,#42735,#42736,#42737,
#42738,#42739,#42740,#42741,#42742,#42743,#42744,#42745,#42746,#42747,#42748,
#42749,#42750,#42751,#42752,#42753,#42754,#42755,#42756,#42757,#42758,#42759,
#42760,#42761,#42762,#42763,#42764,#42765,#42766,#42767,#42768,#42769,#42770,
#42771,#42772,#42773,#42774,#42775,#42776,#42777,#42778,#42779,#42780,#42781,
#42782,#42783,#42784,#42785,#42786,#42787,#42788,#42789,#42790,#42791,#42792,
#42793,#42794,#42795,#42796,#42797,#42798,#42799,#42800,#42801,#42802,#42803,
#42804,#42805,#42806,#42807,#42808,#42809,#42810,#42811,#42812,#42813,#42814,
#42815,#42816,#42817,#42818,#42819,#42820,#42821,#42822,#42823,#42824,#42825,
#42826,#42827,#42828,#42829,#42830,#42831,#42832,#42833,#42834,#42835,#42836,
#42837,#42838,#42839,#42840,#42841,#42842,#42843,#42844,#42845,#42846,#42847,
#42848,#42849,#42850,#42851,#42852,#42853,#42854,#42855,#42856,#42857,#42858,
#42859,#42860,#42861,#42862,#42863,#42864,#42865,#42866,#42867,#42868,#42869,
#42870,#42871,#42872,#42873,#42874,#42875,#42876,#42877,#42878,#42879,#42880,
#42881,#42882,#42883,#42884,#42885,#42886,#42887,#42888,#42889,#42890,#42891,
#42892,#42893,#42894,#42895,#42896,#42897,#42898,#42899,#42900,#42901,#42902,
#42903,#42904,#42905,#42906,#42907,#42908,#42909,#42910,#42911,#42912,#42913,
#42914,#42915,#42916,#42917,#42918,#42919,#42920,#42921,#42922,#42923,#42924,
#42925,#42926,#42927,#42928,#42929,#42930,#42931,#42932,#42933,#42934,#42935,
#42936,#42937,#42938,#42939,#42940,#42941,#42942,#42943,#42944,#42945,#42946,
#42947,#42948,#42949,#42950,#42951,#42952,#42953,#42954,#42955,#42956,#42957,
#42958,#42959,#42960,#42961,#42962,#42963,#42964,#42965,#42966,#42967,#42968,
#42969,#42970,#42971,#42972,#42973,#42974,#42975,#42976,#42977,#42978,#42979,
#42980,#42981,#42982,#42983,#42984,#42985,#42986,#42987,#42988,#42989,#42990,
#42991,#42992,#42993,#42994,#42995,#42996,#42997,#42998,#42999,#43000,#43001,
#43002,#43003,#43004,#43005,#43006,#43007,#43008,#43009,#43010,#43011,#43012,
#43013,#43014,#43015,#43016,#43017,#43018,#43019,#43020,#43021,#43022,#43023,
#43024,#43025,#43026,#43027,#43028,#43029,#43030,#43031,#43032,#43033),
(#43034,#43035,#43036,#43037,#43038,#43039,#43040,#43041,#43042,#43043,
#43044,#43045,#43046,#43047,#43048,#43049,#43050,#43051,#43052,#43053,#43054,
#43055,#43056,#43057,#43058,#43059,#43060,#43061,#43062,#43063,#43064,#43065,
#43066,#43067,#43068,#43069,#43070,#43071,#43072,#43073,#43074,#43075,#43076,
#43077,#43078,#43079,#43080,#43081,#43082,#43083,#43084,#43085,#43086,#43087,
#43088,#43089,#43090,#43091,#43092,#43093,#43094,#43095,#43096,#43097,#43098,
#43099,#43100,#43101,#43102,#43103,#43104,#43105,#43106,#43107,#43108,#43109,
#43110,#43111,#43112,#43113,#43114,#43115,#43116,#43117,#43118,#43119,#43120,
#43121,#43122,#43123,#43124,#43125,#43126,#43127,#43128,#43129,#43130,#43131,
#43132,#43133,#43134,#43135,#43136,#43137,#43138,#43139,#43140,#43141,#43142,
#43143,#43144,#43145,#43146,#43147,#43148,#43149,#43150,#43151,#43152,#43153,
#43154,#43155,#43156,#43157,#43158,#43159,#43160,#43161,#43162,#43163,#43164,
#43165,#43166,#43167,#43168,#43169,#43170,#43171,#43172,#43173,#43174,#43175,
#43176,#43177,#43178,#43179,#43180,#43181,#43182,#43183,#43184,#43185,#43186,
#43187,#43188,#43189,#43190,#43191,#43192,#43193,#43194,#43195,#43196,#43197,
#43198,#43199,#43200,#43201,#43202,#43203,#43204,#43205,#43206,#43207,#43208,
#43209,#43210,#43211,#43212,#43213,#43214,#43215,#43216,#43217,#43218,#43219,
#43220,#43221,#43222,#43223,#43224,#43225,#43226,#43227,#43228,#43229,#43230,
#43231,#43232,#43233,#43234,#43235,#43236,#43237,#43238,#43239,#43240,#43241,
#43242,#43243,#43244,#43245,#43246,#43247,#43248,#43249,#43250,#43251,#43252,
#43253,#43254,#43255,#43256,#43257,#43258,#43259,#43260,#43261,#43262,#43263,
#43264,#43265,#43266,#43267,#43268,#43269,#43270,#43271,#43272,#43273,#43274,
#43275,#43276,#43277,#43278,#43279,#43280,#43281,#43282,#43283,#43284,#43285,
#43286,#43287,#43288,#43289,#43290,#43291,#43292,#43293,#43294,#43295,#43296,
#43297,#43298,#43299,#43300,#43301,#43302,#43303,#43304,#43305,#43306,#43307,
#43308,#43309,#43310,#43311,#43312,#43313,#43314,#43315,#43316,#43317,#43318,
#43319,#43320,#43321,#43322,#43323,#43324,#43325,#43326,#43327,#43328,#43329,
#43330,#43331,#43332,#43333,#43334,#43335,#43336,#43337,#43338,#43339,#43340,
#43341,#43342,#43343,#43344,#43345,#43346,#43347,#43348,#43349,#43350,#43351,
#43352,#43353,#43354,#43355,#43356)),.UNSPECIFIED.,.F.,.F.,.F.,(4,4),(4,
1,1,1,1,1,1,1,1,1,1,1,1,1,1,1,1,1,1,1,1,1,1,1,1,1,1,1,1,1,1,1,1,1,1,1,1,
1,1,1,1,1,1,1,1,1,1,1,1,1,1,1,1,1,1,1,1,1,1,1,1,1,1,1,1,1,1,1,1,1,1,1,1,
1,1,1,1,1,1,1,1,1,1,1,1,1,1,1,1,1,1,1,1,1,1,1,1,1,1,1,1,1,1,1,1,1,1,1,1,
1,1,1,1,1,1,1,1,1,1,1,1,1,1,1,1,1,1,1,1,1,1,1,1,1,1,1,1,1,1,1,1,1,1,1,1,
1,1,1,1,1,1,1,1,1,1,1,1,1,1,1,1,1,1,1,1,1,1,1,1,1,1,1,1,1,1,1,1,1,1,1,1,
1,1,1,1,1,1,1,1,1,1,1,1,1,1,1,1,1,1,1,1,1,1,1,1,1,1,1,1,1,1,1,1,1,1,1,1,
1,1,1,1,1,1,1,1,1,1,1,1,1,1,1,1,1,1,1,1,1,1,1,1,1,1,1,1,1,1,1,1,1,1,1,1,
1,1,1,1,1,1,1,1,1,1,1,1,1,1,1,1,1,1,1,1,1,1,1,1,1,1,1,1,1,1,1,1,1,1,1,1,
1,1,1,1,1,1,1,1,1,1,1,1,1,1,1,1,1,1,1,1,1,1,1,1,1,1,1,1,1,1,1,4),(0.,0.0641840294258124),
(14.398944266781,14.8961193712582,15.3932944757354,15.8904695802126,16.3876446846898,
16.884819789167,17.3819948936443,17.8791699981215,18.3763451025987,18.8735202070759,
19.3706953115531,19.8678704160303,20.3650455205075,20.8622206249848,21.359395729462,
21.8565708339392,22.3537459384164,22.8509210428936,23.3480961473708,23.845271251848,
24.3424463563253,24.8396214608025,25.3367965652797,25.8339716697569,26.3311467742341,
26.8283218787113,27.3254969831885,27.8226720876658,28.319847192143,28.8170222966202,
29.3141974010974,29.8113725055746,30.3085476100518,30.805722714529,31.3028978190063,
31.8000729234835,32.2972480279607,32.7944231324379,33.2915982369151,33.7887733413923,
34.2859484458695,34.7831235503468,35.280298654824,35.7774737593012,36.2746488637784,
36.7718239682556,37.2689990727328,37.76617417721,38.2633492816873,38.7605243861645,
39.2576994906417,39.7548745951189,40.2520496995961,40.7492248040733,41.2463999085505,
41.7435750130278,42.240750117505,42.7379252219822,43.2351003264594,43.7322754309366,
44.2294505354138,44.726625639891,45.2238007443683,45.7209758488455,46.2181509533227,
46.7153260577999,47.2125011622771,47.7096762667543,48.2068513712315,48.7040264757088,
49.201201580186,49.6983766846632,50.1955517891404,50.6927268936176,51.1899019980948,
51.687077102572,52.1842522070493,52.6814273115265,53.1786024160037,53.6757775204809,
54.1729526249581,54.6701277294353,55.1673028339125,55.6644779383898,56.161653042867,
56.6588281473442,57.1560032518214,57.6531783562986,58.1503534607758,58.647528565253,
59.1447036697303,59.6418787742075,60.1390538786847,60.6362289831619,61.1334040876391,
61.6305791921163,62.1277542965935,62.6249294010708,63.122104505548,63.6192796100252,
64.1164547145024,64.6136298189796,65.1108049234568,65.607980027934,66.1051551324113,
66.6023302368885,67.0995053413657,67.5966804458429,68.0938555503201,68.5910306547973,
69.0882057592745,69.5853808637518,70.082555968229,70.5797310727062,71.0769061771834,
71.5740812816606,72.0712563861378,72.568431490615,73.0656065950923,73.5627816995695,
74.0599568040467,74.5571319085239,75.0543070130011,75.5514821174783,76.0486572219556,
76.5458323264328,77.04300743091,77.5401825353872,78.0373576398644,78.5345327443416,
79.0317078488188,79.528882953296,80.0260580577733,80.5232331622505,81.0204082667277,
81.5175833712049,82.0147584756821,82.5119335801593,83.0091086846365,83.5062837891138,
84.003458893591,84.5006339980682,84.9978091025454,85.4949842070226,85.9921593114998,
86.4893344159771,86.9865095204543,87.4836846249315,87.9808597294087,88.4780348338859,
88.9752099383631,89.4723850428403,89.9695601473175,90.4667352517948,90.963910356272,
91.4610854607492,91.9582605652264,92.4554356697036,92.9526107741808,93.449785878658,
93.9469609831353,94.4441360876125,94.9413111920897,95.4384862965669,95.9356614010441,
96.4328365055213,96.9300116099986,97.4271867144758,97.924361818953,98.4215369234302,
98.9187120279074,99.4158871323846,99.9130622368618,100.410237341339,100.907412445816,
101.404587550293,101.901762654771,102.398937759248,102.896112863725,103.393287968202,
103.89046307268,104.387638177157,104.884813281634,105.381988386111,105.879163490588,
106.376338595066,106.873513699543,107.37068880402,107.867863908497,108.365039012974,
108.862214117452,109.359389221929,109.856564326406,110.353739430883,110.850914535361,
111.348089639838,111.845264744315,112.342439848792,112.839614953269,113.336790057747,
113.833965162224,114.331140266701,114.828315371178,115.325490475655,115.822665580133,
116.31984068461,116.817015789087,117.314190893564,117.811365998042,118.308541102519,
118.805716206996,119.302891311473,119.80006641595,120.297241520428,120.794416624905,
121.291591729382,121.788766833859,122.285941938336,122.783117042814,123.280292147291,
123.777467251768,124.274642356245,124.771817460723,125.2689925652,125.766167669677,
126.263342774154,126.760517878631,127.257692983109,127.754868087586,128.252043192063,
128.74921829654,129.246393401017,129.743568505495,130.240743609972,130.737918714449,
131.235093818926,131.732268923404,132.229444027881,132.726619132358,133.223794236835,
133.720969341312,134.21814444579,134.715319550267,135.212494654744,135.709669759221,
136.206844863698,136.704019968176,137.201195072653,137.69837017713,138.195545281607,
138.692720386085,139.189895490562,139.687070595039,140.184245699516,140.681420803993,
141.178595908471,141.675771012948,142.172946117425,142.670121221902,143.167296326379,
143.664471430857,144.161646535334,144.658821639811,145.155996744288,145.653171848766,
146.150346953243,146.64752205772,147.144697162197,147.641872266674,148.139047371152,
148.636222475629,149.133397580106,149.630572684583,150.12774778906,150.624922893538,
151.122097998015,151.619273102492,152.116448206969,152.613623311447,153.110798415924,
153.607973520401,154.105148624878,154.602323729355,155.099498833833,155.59667393831,
156.093849042787,156.591024147264,157.088199251742,157.585374356219,158.082549460696,
158.579724565173,159.07689966965,159.574074774128,160.071249878605,160.568424983082,
161.065600087559,161.562775192036,162.059950296514,162.557125400991,163.054300505468,
163.551475609945,164.048650714422,164.5458258189,165.043000923377,165.540176027854,
166.037351132331,166.534526236809,167.031701341286,167.528876445763,168.02605155024,
168.523226654717,169.020401759195,169.517576863672,170.014751968149,170.511927072626,
171.009102177104,171.506277281581,172.003452386058,172.500627490535,172.997802595012,
173.49497769949),.UNSPECIFIED.);
#271=B_SPLINE_SURFACE_WITH_KNOTS('',3,3,((#45785,#45786,#45787,#45788,#45789,
#45790,#45791,#45792,#45793,#45794,#45795,#45796,#45797,#45798,#45799,#45800,
#45801,#45802,#45803,#45804,#45805,#45806,#45807,#45808,#45809,#45810,#45811,
#45812,#45813,#45814,#45815,#45816,#45817,#45818,#45819,#45820,#45821,#45822,
#45823,#45824,#45825,#45826,#45827,#45828,#45829,#45830,#45831,#45832,#45833,
#45834,#45835,#45836,#45837,#45838,#45839,#45840,#45841,#45842,#45843,#45844,
#45845,#45846,#45847,#45848,#45849,#45850,#45851,#45852,#45853,#45854,#45855,
#45856,#45857,#45858,#45859,#45860,#45861,#45862,#45863,#45864,#45865,#45866,
#45867,#45868,#45869,#45870,#45871,#45872,#45873,#45874,#45875,#45876,#45877,
#45878,#45879,#45880,#45881,#45882,#45883,#45884,#45885,#45886,#45887,#45888,
#45889,#45890,#45891,#45892,#45893,#45894,#45895,#45896,#45897,#45898,#45899,
#45900,#45901,#45902,#45903,#45904,#45905,#45906,#45907,#45908,#45909,#45910,
#45911,#45912,#45913),(#45914,#45915,#45916,#45917,#45918,#45919,#45920,
#45921,#45922,#45923,#45924,#45925,#45926,#45927,#45928,#45929,#45930,#45931,
#45932,#45933,#45934,#45935,#45936,#45937,#45938,#45939,#45940,#45941,#45942,
#45943,#45944,#45945,#45946,#45947,#45948,#45949,#45950,#45951,#45952,#45953,
#45954,#45955,#45956,#45957,#45958,#45959,#45960,#45961,#45962,#45963,#45964,
#45965,#45966,#45967,#45968,#45969,#45970,#45971,#45972,#45973,#45974,#45975,
#45976,#45977,#45978,#45979,#45980,#45981,#45982,#45983,#45984,#45985,#45986,
#45987,#45988,#45989,#45990,#45991,#45992,#45993,#45994,#45995,#45996,#45997,
#45998,#45999,#46000,#46001,#46002,#46003,#46004,#46005,#46006,#46007,#46008,
#46009,#46010,#46011,#46012,#46013,#46014,#46015,#46016,#46017,#46018,#46019,
#46020,#46021,#46022,#46023,#46024,#46025,#46026,#46027,#46028,#46029,#46030,
#46031,#46032,#46033,#46034,#46035,#46036,#46037,#46038,#46039,#46040,#46041,
#46042),(#46043,#46044,#46045,#46046,#46047,#46048,#46049,#46050,#46051,
#46052,#46053,#46054,#46055,#46056,#46057,#46058,#46059,#46060,#46061,#46062,
#46063,#46064,#46065,#46066,#46067,#46068,#46069,#46070,#46071,#46072,#46073,
#46074,#46075,#46076,#46077,#46078,#46079,#46080,#46081,#46082,#46083,#46084,
#46085,#46086,#46087,#46088,#46089,#46090,#46091,#46092,#46093,#46094,#46095,
#46096,#46097,#46098,#46099,#46100,#46101,#46102,#46103,#46104,#46105,#46106,
#46107,#46108,#46109,#46110,#46111,#46112,#46113,#46114,#46115,#46116,#46117,
#46118,#46119,#46120,#46121,#46122,#46123,#46124,#46125,#46126,#46127,#46128,
#46129,#46130,#46131,#46132,#46133,#46134,#46135,#46136,#46137,#46138,#46139,
#46140,#46141,#46142,#46143,#46144,#46145,#46146,#46147,#46148,#46149,#46150,
#46151,#46152,#46153,#46154,#46155,#46156,#46157,#46158,#46159,#46160,#46161,
#46162,#46163,#46164,#46165,#46166,#46167,#46168,#46169,#46170,#46171),
(#46172,#46173,#46174,#46175,#46176,#46177,#46178,#46179,#46180,#46181,
#46182,#46183,#46184,#46185,#46186,#46187,#46188,#46189,#46190,#46191,#46192,
#46193,#46194,#46195,#46196,#46197,#46198,#46199,#46200,#46201,#46202,#46203,
#46204,#46205,#46206,#46207,#46208,#46209,#46210,#46211,#46212,#46213,#46214,
#46215,#46216,#46217,#46218,#46219,#46220,#46221,#46222,#46223,#46224,#46225,
#46226,#46227,#46228,#46229,#46230,#46231,#46232,#46233,#46234,#46235,#46236,
#46237,#46238,#46239,#46240,#46241,#46242,#46243,#46244,#46245,#46246,#46247,
#46248,#46249,#46250,#46251,#46252,#46253,#46254,#46255,#46256,#46257,#46258,
#46259,#46260,#46261,#46262,#46263,#46264,#46265,#46266,#46267,#46268,#46269,
#46270,#46271,#46272,#46273,#46274,#46275,#46276,#46277,#46278,#46279,#46280,
#46281,#46282,#46283,#46284,#46285,#46286,#46287,#46288,#46289,#46290,#46291,
#46292,#46293,#46294,#46295,#46296,#46297,#46298,#46299,#46300)),
 .UNSPECIFIED.,.F.,.F.,.F.,(4,4),(4,1,1,1,1,1,1,1,1,1,1,1,1,1,1,1,1,1,1,
1,1,1,1,1,1,1,1,1,1,1,1,1,1,1,1,1,1,1,1,1,1,1,1,1,1,1,1,1,1,1,1,1,1,1,1,
1,1,1,1,1,1,1,1,1,1,1,1,1,1,1,1,1,1,1,1,1,1,1,1,1,1,1,1,1,1,1,1,1,1,1,1,
1,1,1,1,1,1,1,1,1,1,1,1,1,1,1,1,1,1,1,1,1,1,1,1,1,1,1,1,1,1,1,1,1,1,1,4),
(0.,0.0658179306876173),(11.6150328478182,12.1123165623719,12.6096002769257,
13.6041677060331,14.5987351351405,15.5933025642479,16.5878699933554,17.5824374224628,
18.5770048515702,19.5715722806776,20.5661397097851,21.5607071388925,22.5552745679999,
23.5498419971074,24.5444094262148,25.5389768553222,26.5335442844296,27.5281117135371,
28.5226791426445,29.5172465717519,30.5118140008593,31.5063814299668,32.5009488590742,
33.4955162881816,34.490083717289,35.4846511463965,36.4792185755039,37.4737860046113,
38.4683534337187,39.4629208628262,40.4574882919336,41.452055721041,42.4466231501485,
43.4411905792559,44.4357580083633,45.4303254374707,46.4248928665782,47.4194602956856,
48.414027724793,49.4085951539004,50.4031625830079,51.3977300121153,52.3922974412227,
53.3868648703302,54.3814322994376,55.375999728545,56.3705671576524,57.3651345867599,
58.3597020158673,59.3542694449747,60.3488368740821,61.3434043031896,62.337971732297,
63.3325391614044,64.3271065905118,65.3216740196193,66.3162414487267,67.3108088778341,
68.3053763069416,69.299943736049,70.2945111651564,71.2890785942638,72.2836460233713,
73.2782134524787,74.2727808815861,75.2673483106935,76.261915739801,77.2564831689084,
78.2510505980158,79.2456180271232,80.2401854562307,81.2347528853381,82.2293203144455,
83.223887743553,84.2184551726604,85.2130226017678,86.2075900308752,87.2021574599827,
88.1967248890901,89.1912923181975,90.1858597473049,91.1804271764124,92.1749946055198,
93.1695620346272,94.1641294637347,95.1586968928421,96.1532643219495,97.1478317510569,
98.1423991801644,99.1369666092718,100.131534038379,101.126101467487,102.120668896594,
103.115236325701,104.109803754809,105.104371183916,106.098938613024,107.093506042131,
108.088073471239,109.082640900346,110.077208329453,111.071775758561,112.066343187668,
113.060910616776,114.055478045883,115.050045474991,116.044612904098,117.039180333205,
118.033747762313,119.02831519142,120.022882620528,121.017450049635,122.012017478743,
123.00658490785,124.001152336957,124.995719766065,125.990287195172,126.98485462428,
127.979422053387,128.973989482495,129.968556911602,130.963124340709,131.957691769817,
132.952259198924,133.946826628032,134.444110342585,134.941394057139),
 .UNSPECIFIED.);
#272=B_SPLINE_SURFACE_WITH_KNOTS('',3,3,((#46445,#46446,#46447,#46448,#46449,
#46450,#46451,#46452,#46453,#46454,#46455,#46456,#46457,#46458,#46459,#46460,
#46461,#46462,#46463,#46464,#46465,#46466,#46467,#46468,#46469,#46470,#46471,
#46472,#46473,#46474,#46475,#46476,#46477,#46478,#46479,#46480,#46481,#46482,
#46483,#46484,#46485,#46486,#46487,#46488,#46489,#46490,#46491,#46492,#46493,
#46494,#46495,#46496,#46497,#46498,#46499,#46500,#46501,#46502,#46503,#46504,
#46505,#46506,#46507,#46508,#46509,#46510,#46511,#46512,#46513,#46514,#46515,
#46516,#46517,#46518,#46519,#46520,#46521,#46522,#46523,#46524,#46525,#46526,
#46527,#46528,#46529,#46530,#46531,#46532,#46533,#46534,#46535,#46536,#46537,
#46538,#46539,#46540,#46541,#46542,#46543,#46544,#46545,#46546,#46547,#46548,
#46549,#46550,#46551,#46552,#46553,#46554,#46555,#46556,#46557,#46558,#46559,
#46560,#46561,#46562,#46563,#46564,#46565,#46566,#46567,#46568,#46569,#46570,
#46571,#46572,#46573,#46574,#46575),(#46576,#46577,#46578,#46579,#46580,
#46581,#46582,#46583,#46584,#46585,#46586,#46587,#46588,#46589,#46590,#46591,
#46592,#46593,#46594,#46595,#46596,#46597,#46598,#46599,#46600,#46601,#46602,
#46603,#46604,#46605,#46606,#46607,#46608,#46609,#46610,#46611,#46612,#46613,
#46614,#46615,#46616,#46617,#46618,#46619,#46620,#46621,#46622,#46623,#46624,
#46625,#46626,#46627,#46628,#46629,#46630,#46631,#46632,#46633,#46634,#46635,
#46636,#46637,#46638,#46639,#46640,#46641,#46642,#46643,#46644,#46645,#46646,
#46647,#46648,#46649,#46650,#46651,#46652,#46653,#46654,#46655,#46656,#46657,
#46658,#46659,#46660,#46661,#46662,#46663,#46664,#46665,#46666,#46667,#46668,
#46669,#46670,#46671,#46672,#46673,#46674,#46675,#46676,#46677,#46678,#46679,
#46680,#46681,#46682,#46683,#46684,#46685,#46686,#46687,#46688,#46689,#46690,
#46691,#46692,#46693,#46694,#46695,#46696,#46697,#46698,#46699,#46700,#46701,
#46702,#46703,#46704,#46705,#46706),(#46707,#46708,#46709,#46710,#46711,
#46712,#46713,#46714,#46715,#46716,#46717,#46718,#46719,#46720,#46721,#46722,
#46723,#46724,#46725,#46726,#46727,#46728,#46729,#46730,#46731,#46732,#46733,
#46734,#46735,#46736,#46737,#46738,#46739,#46740,#46741,#46742,#46743,#46744,
#46745,#46746,#46747,#46748,#46749,#46750,#46751,#46752,#46753,#46754,#46755,
#46756,#46757,#46758,#46759,#46760,#46761,#46762,#46763,#46764,#46765,#46766,
#46767,#46768,#46769,#46770,#46771,#46772,#46773,#46774,#46775,#46776,#46777,
#46778,#46779,#46780,#46781,#46782,#46783,#46784,#46785,#46786,#46787,#46788,
#46789,#46790,#46791,#46792,#46793,#46794,#46795,#46796,#46797,#46798,#46799,
#46800,#46801,#46802,#46803,#46804,#46805,#46806,#46807,#46808,#46809,#46810,
#46811,#46812,#46813,#46814,#46815,#46816,#46817,#46818,#46819,#46820,#46821,
#46822,#46823,#46824,#46825,#46826,#46827,#46828,#46829,#46830,#46831,#46832,
#46833,#46834,#46835,#46836,#46837),(#46838,#46839,#46840,#46841,#46842,
#46843,#46844,#46845,#46846,#46847,#46848,#46849,#46850,#46851,#46852,#46853,
#46854,#46855,#46856,#46857,#46858,#46859,#46860,#46861,#46862,#46863,#46864,
#46865,#46866,#46867,#46868,#46869,#46870,#46871,#46872,#46873,#46874,#46875,
#46876,#46877,#46878,#46879,#46880,#46881,#46882,#46883,#46884,#46885,#46886,
#46887,#46888,#46889,#46890,#46891,#46892,#46893,#46894,#46895,#46896,#46897,
#46898,#46899,#46900,#46901,#46902,#46903,#46904,#46905,#46906,#46907,#46908,
#46909,#46910,#46911,#46912,#46913,#46914,#46915,#46916,#46917,#46918,#46919,
#46920,#46921,#46922,#46923,#46924,#46925,#46926,#46927,#46928,#46929,#46930,
#46931,#46932,#46933,#46934,#46935,#46936,#46937,#46938,#46939,#46940,#46941,
#46942,#46943,#46944,#46945,#46946,#46947,#46948,#46949,#46950,#46951,#46952,
#46953,#46954,#46955,#46956,#46957,#46958,#46959,#46960,#46961,#46962,#46963,
#46964,#46965,#46966,#46967,#46968)),.UNSPECIFIED.,.F.,.F.,.F.,(4,4),(4,
1,1,1,1,1,1,1,1,1,1,1,1,1,1,1,1,1,1,1,1,1,1,1,1,1,1,1,1,1,1,1,1,1,1,1,1,
1,1,1,1,1,1,1,1,1,1,1,1,1,1,1,1,1,1,1,1,1,1,1,1,1,1,1,1,1,1,1,1,1,1,1,1,
1,1,1,1,1,1,1,1,1,1,1,1,1,1,1,1,1,1,1,1,1,1,1,1,1,1,1,1,1,1,1,1,1,1,1,1,
1,1,1,1,1,1,1,1,1,1,1,1,1,1,1,1,1,1,1,4),(0.,0.0658179306876173),(8.30838445208313,
8.80598005718054,9.30357566227795,10.2987668724728,11.2939580826676,12.2891492928624,
13.2843405030573,14.2795317132521,15.2747229234469,16.2699141336417,17.2651053438366,
18.2602965540314,19.2554877642262,20.250678974421,21.2458701846159,22.2410613948107,
23.2362526050055,24.2314438152003,25.2266350253952,26.22182623559,27.2170174457848,
28.2122086559796,29.2073998661744,30.2025910763693,31.1977822865641,32.1929734967589,
33.1881647069537,34.1833559171486,35.1785471273434,36.1737383375382,37.168929547733,
38.1641207579279,39.1593119681227,40.1545031783175,41.1496943885123,42.1448855987072,
43.140076808902,44.1352680190968,45.1304592292916,46.1256504394865,47.1208416496813,
48.1160328598761,49.1112240700709,50.1064152802658,51.1016064904606,52.0967977006554,
53.0919889108502,54.0871801210451,55.0823713312399,56.0775625414347,57.0727537516295,
58.0679449618244,59.0631361720192,60.058327382214,61.0535185924088,62.0487098026037,
63.0439010127985,64.0390922229933,65.0342834331881,66.029474643383,67.0246658535778,
68.0198570637726,69.0150482739674,70.0102394841623,71.0054306943571,72.0006219045519,
72.9958131147467,73.9910043249416,74.9861955351364,75.9813867453312,76.976577955526,
77.9717691657209,78.9669603759157,79.9621515861105,80.9573427963053,81.9525340065002,
82.947725216695,83.9429164268898,84.9381076370846,85.9332988472795,86.9284900574743,
87.9236812676691,88.9188724778639,89.9140636880588,90.9092548982536,91.9044461084484,
92.8996373186432,93.8948285288381,94.8900197390329,95.8852109492277,96.8804021594225,
97.8755933696174,98.8707845798122,99.865975790007,100.861167000202,101.856358210397,
102.851549420591,103.846740630786,104.841931840981,105.837123051176,106.832314261371,
107.827505471566,108.82269668176,109.817887891955,110.81307910215,111.808270312345,
112.80346152254,113.798652732735,114.793843942929,115.789035153124,116.784226363319,
117.779417573514,118.774608783709,119.769799993904,120.764991204098,121.760182414293,
122.755373624488,123.750564834683,124.745756044878,125.740947255072,126.736138465267,
127.731329675462,128.726520885657,129.721712095852,130.716903306047,131.712094516241,
132.707285726436,133.204881331534,133.702476936631),.UNSPECIFIED.);
#273=B_SPLINE_SURFACE_WITH_KNOTS('',3,3,((#49030,#49031,#49032,#49033,#49034,
#49035,#49036,#49037,#49038,#49039,#49040,#49041,#49042,#49043,#49044,#49045,
#49046,#49047,#49048,#49049,#49050,#49051,#49052,#49053,#49054,#49055,#49056,
#49057,#49058,#49059,#49060,#49061,#49062,#49063,#49064,#49065,#49066,#49067,
#49068,#49069,#49070,#49071,#49072,#49073,#49074,#49075,#49076,#49077,#49078,
#49079,#49080,#49081,#49082,#49083,#49084,#49085),(#49086,#49087,#49088,
#49089,#49090,#49091,#49092,#49093,#49094,#49095,#49096,#49097,#49098,#49099,
#49100,#49101,#49102,#49103,#49104,#49105,#49106,#49107,#49108,#49109,#49110,
#49111,#49112,#49113,#49114,#49115,#49116,#49117,#49118,#49119,#49120,#49121,
#49122,#49123,#49124,#49125,#49126,#49127,#49128,#49129,#49130,#49131,#49132,
#49133,#49134,#49135,#49136,#49137,#49138,#49139,#49140,#49141),(#49142,
#49143,#49144,#49145,#49146,#49147,#49148,#49149,#49150,#49151,#49152,#49153,
#49154,#49155,#49156,#49157,#49158,#49159,#49160,#49161,#49162,#49163,#49164,
#49165,#49166,#49167,#49168,#49169,#49170,#49171,#49172,#49173,#49174,#49175,
#49176,#49177,#49178,#49179,#49180,#49181,#49182,#49183,#49184,#49185,#49186,
#49187,#49188,#49189,#49190,#49191,#49192,#49193,#49194,#49195,#49196,#49197),
(#49198,#49199,#49200,#49201,#49202,#49203,#49204,#49205,#49206,#49207,
#49208,#49209,#49210,#49211,#49212,#49213,#49214,#49215,#49216,#49217,#49218,
#49219,#49220,#49221,#49222,#49223,#49224,#49225,#49226,#49227,#49228,#49229,
#49230,#49231,#49232,#49233,#49234,#49235,#49236,#49237,#49238,#49239,#49240,
#49241,#49242,#49243,#49244,#49245,#49246,#49247,#49248,#49249,#49250,#49251,
#49252,#49253)),.UNSPECIFIED.,.F.,.F.,.F.,(4,4),(4,1,1,1,1,1,1,1,1,1,1,
1,1,1,1,1,1,1,1,1,1,1,1,1,1,1,1,1,1,1,1,1,1,1,1,1,1,1,1,1,1,1,1,1,1,1,1,
1,1,1,1,1,1,4),(0.,0.0642013499338865),(11.8589888623078,12.8454497557128,
13.8319106491178,14.8183715425228,15.8048324359278,16.7912933293328,17.7777542227378,
18.7642151161428,19.7506760095478,20.7371369029528,21.7235977963578,22.7100586897628,
23.6965195831678,24.6829804765729,25.6694413699779,26.6559022633829,27.6423631567879,
28.6288240501929,29.6152849435979,30.6017458370029,31.5882067304079,32.5746676238129,
33.5611285172179,34.5475894106229,35.5340503040279,36.5205111974329,37.5069720908379,
38.4934329842429,39.4798938776479,40.4663547710529,41.4528156644579,42.4392765578629,
43.4257374512679,44.4121983446729,45.3986592380779,46.3851201314829,47.3715810248879,
48.3580419182929,49.3445028116979,50.3309637051029,51.3174245985079,52.3038854919129,
53.2903463853179,54.2768072787229,55.2632681721279,56.2497290655329,57.2361899589379,
58.2226508523429,59.2091117457479,60.1955726391529,61.1820335325579,62.1684944259629,
63.154955319368,64.141416212773),.UNSPECIFIED.);
#274=B_SPLINE_SURFACE_WITH_KNOTS('',3,3,((#49370,#49371,#49372,#49373,#49374,
#49375,#49376,#49377,#49378,#49379,#49380,#49381,#49382,#49383,#49384,#49385,
#49386,#49387,#49388,#49389,#49390,#49391,#49392,#49393,#49394,#49395,#49396,
#49397,#49398,#49399,#49400,#49401,#49402,#49403,#49404,#49405,#49406,#49407,
#49408,#49409,#49410,#49411,#49412,#49413,#49414,#49415,#49416,#49417,#49418,
#49419,#49420,#49421,#49422,#49423,#49424,#49425),(#49426,#49427,#49428,
#49429,#49430,#49431,#49432,#49433,#49434,#49435,#49436,#49437,#49438,#49439,
#49440,#49441,#49442,#49443,#49444,#49445,#49446,#49447,#49448,#49449,#49450,
#49451,#49452,#49453,#49454,#49455,#49456,#49457,#49458,#49459,#49460,#49461,
#49462,#49463,#49464,#49465,#49466,#49467,#49468,#49469,#49470,#49471,#49472,
#49473,#49474,#49475,#49476,#49477,#49478,#49479,#49480,#49481),(#49482,
#49483,#49484,#49485,#49486,#49487,#49488,#49489,#49490,#49491,#49492,#49493,
#49494,#49495,#49496,#49497,#49498,#49499,#49500,#49501,#49502,#49503,#49504,
#49505,#49506,#49507,#49508,#49509,#49510,#49511,#49512,#49513,#49514,#49515,
#49516,#49517,#49518,#49519,#49520,#49521,#49522,#49523,#49524,#49525,#49526,
#49527,#49528,#49529,#49530,#49531,#49532,#49533,#49534,#49535,#49536,#49537),
(#49538,#49539,#49540,#49541,#49542,#49543,#49544,#49545,#49546,#49547,
#49548,#49549,#49550,#49551,#49552,#49553,#49554,#49555,#49556,#49557,#49558,
#49559,#49560,#49561,#49562,#49563,#49564,#49565,#49566,#49567,#49568,#49569,
#49570,#49571,#49572,#49573,#49574,#49575,#49576,#49577,#49578,#49579,#49580,
#49581,#49582,#49583,#49584,#49585,#49586,#49587,#49588,#49589,#49590,#49591,
#49592,#49593)),.UNSPECIFIED.,.F.,.F.,.F.,(4,4),(4,1,1,1,1,1,1,1,1,1,1,
1,1,1,1,1,1,1,1,1,1,1,1,1,1,1,1,1,1,1,1,1,1,1,1,1,1,1,1,1,1,1,1,1,1,1,1,
1,1,1,1,1,1,4),(0.,0.0642013499338865),(14.3984001269719,15.3848610203769,
16.3713219137819,17.3577828071869,18.3442437005919,19.3307045939969,20.3171654874019,
21.3036263808069,22.2900872742119,23.2765481676169,24.2630090610219,25.2494699544269,
26.2359308478319,27.2223917412369,28.2088526346419,29.1953135280469,30.1817744214519,
31.1682353148569,32.1546962082619,33.1411571016669,34.1276179950719,35.1140788884769,
36.1005397818819,37.0870006752869,38.0734615686919,39.0599224620969,40.0463833555019,
41.0328442489069,42.0193051423119,43.0057660357169,43.9922269291219,44.9786878225269,
45.9651487159319,46.9516096093369,47.9380705027419,48.9245313961469,49.9109922895519,
50.897453182957,51.883914076362,52.870374969767,53.856835863172,54.843296756577,
55.829757649982,56.816218543387,57.802679436792,58.789140330197,59.775601223602,
60.762062117007,61.748523010412,62.734983903817,63.721444797222,64.707905690627,
65.694366584032,66.680827477437),.UNSPECIFIED.);
#275=B_SPLINE_SURFACE_WITH_KNOTS('',3,3,((#49922,#49923,#49924,#49925,#49926,
#49927,#49928,#49929,#49930,#49931,#49932,#49933,#49934,#49935,#49936,#49937,
#49938,#49939,#49940,#49941,#49942,#49943,#49944,#49945,#49946,#49947,#49948,
#49949,#49950,#49951,#49952,#49953,#49954,#49955,#49956,#49957,#49958,#49959,
#49960,#49961,#49962,#49963,#49964,#49965,#49966,#49967,#49968,#49969,#49970,
#49971,#49972,#49973,#49974,#49975,#49976,#49977),(#49978,#49979,#49980,
#49981,#49982,#49983,#49984,#49985,#49986,#49987,#49988,#49989,#49990,#49991,
#49992,#49993,#49994,#49995,#49996,#49997,#49998,#49999,#50000,#50001,#50002,
#50003,#50004,#50005,#50006,#50007,#50008,#50009,#50010,#50011,#50012,#50013,
#50014,#50015,#50016,#50017,#50018,#50019,#50020,#50021,#50022,#50023,#50024,
#50025,#50026,#50027,#50028,#50029,#50030,#50031,#50032,#50033),(#50034,
#50035,#50036,#50037,#50038,#50039,#50040,#50041,#50042,#50043,#50044,#50045,
#50046,#50047,#50048,#50049,#50050,#50051,#50052,#50053,#50054,#50055,#50056,
#50057,#50058,#50059,#50060,#50061,#50062,#50063,#50064,#50065,#50066,#50067,
#50068,#50069,#50070,#50071,#50072,#50073,#50074,#50075,#50076,#50077,#50078,
#50079,#50080,#50081,#50082,#50083,#50084,#50085,#50086,#50087,#50088,#50089),
(#50090,#50091,#50092,#50093,#50094,#50095,#50096,#50097,#50098,#50099,
#50100,#50101,#50102,#50103,#50104,#50105,#50106,#50107,#50108,#50109,#50110,
#50111,#50112,#50113,#50114,#50115,#50116,#50117,#50118,#50119,#50120,#50121,
#50122,#50123,#50124,#50125,#50126,#50127,#50128,#50129,#50130,#50131,#50132,
#50133,#50134,#50135,#50136,#50137,#50138,#50139,#50140,#50141,#50142,#50143,
#50144,#50145)),.UNSPECIFIED.,.F.,.F.,.F.,(4,4),(4,1,1,1,1,1,1,1,1,1,1,
1,1,1,1,1,1,1,1,1,1,1,1,1,1,1,1,1,1,1,1,1,1,1,1,1,1,1,1,1,1,1,1,1,1,1,1,
1,1,1,1,1,1,4),(0.,0.0642013499338863),(11.8589888623078,12.8454497557128,
13.8319106491178,14.8183715425228,15.8048324359278,16.7912933293328,17.7777542227378,
18.7642151161428,19.7506760095478,20.7371369029528,21.7235977963578,22.7100586897628,
23.6965195831678,24.6829804765729,25.6694413699779,26.6559022633829,27.6423631567879,
28.6288240501929,29.6152849435979,30.6017458370029,31.5882067304079,32.5746676238129,
33.5611285172179,34.5475894106229,35.5340503040279,36.5205111974329,37.5069720908379,
38.4934329842429,39.4798938776479,40.4663547710529,41.4528156644579,42.4392765578629,
43.4257374512679,44.4121983446729,45.3986592380779,46.3851201314829,47.3715810248879,
48.3580419182929,49.3445028116979,50.3309637051029,51.3174245985079,52.3038854919129,
53.2903463853179,54.2768072787229,55.2632681721279,56.2497290655329,57.2361899589379,
58.2226508523429,59.2091117457479,60.1955726391529,61.1820335325579,62.1684944259629,
63.154955319368,64.141416212773),.UNSPECIFIED.);
#276=B_SPLINE_SURFACE_WITH_KNOTS('',3,3,((#50262,#50263,#50264,#50265,#50266,
#50267,#50268,#50269,#50270,#50271,#50272,#50273,#50274,#50275,#50276,#50277,
#50278,#50279,#50280,#50281,#50282,#50283,#50284,#50285,#50286,#50287,#50288,
#50289,#50290,#50291,#50292,#50293,#50294,#50295,#50296,#50297,#50298,#50299,
#50300,#50301,#50302,#50303,#50304,#50305,#50306,#50307,#50308,#50309,#50310,
#50311,#50312,#50313,#50314,#50315,#50316,#50317),(#50318,#50319,#50320,
#50321,#50322,#50323,#50324,#50325,#50326,#50327,#50328,#50329,#50330,#50331,
#50332,#50333,#50334,#50335,#50336,#50337,#50338,#50339,#50340,#50341,#50342,
#50343,#50344,#50345,#50346,#50347,#50348,#50349,#50350,#50351,#50352,#50353,
#50354,#50355,#50356,#50357,#50358,#50359,#50360,#50361,#50362,#50363,#50364,
#50365,#50366,#50367,#50368,#50369,#50370,#50371,#50372,#50373),(#50374,
#50375,#50376,#50377,#50378,#50379,#50380,#50381,#50382,#50383,#50384,#50385,
#50386,#50387,#50388,#50389,#50390,#50391,#50392,#50393,#50394,#50395,#50396,
#50397,#50398,#50399,#50400,#50401,#50402,#50403,#50404,#50405,#50406,#50407,
#50408,#50409,#50410,#50411,#50412,#50413,#50414,#50415,#50416,#50417,#50418,
#50419,#50420,#50421,#50422,#50423,#50424,#50425,#50426,#50427,#50428,#50429),
(#50430,#50431,#50432,#50433,#50434,#50435,#50436,#50437,#50438,#50439,
#50440,#50441,#50442,#50443,#50444,#50445,#50446,#50447,#50448,#50449,#50450,
#50451,#50452,#50453,#50454,#50455,#50456,#50457,#50458,#50459,#50460,#50461,
#50462,#50463,#50464,#50465,#50466,#50467,#50468,#50469,#50470,#50471,#50472,
#50473,#50474,#50475,#50476,#50477,#50478,#50479,#50480,#50481,#50482,#50483,
#50484,#50485)),.UNSPECIFIED.,.F.,.F.,.F.,(4,4),(4,1,1,1,1,1,1,1,1,1,1,
1,1,1,1,1,1,1,1,1,1,1,1,1,1,1,1,1,1,1,1,1,1,1,1,1,1,1,1,1,1,1,1,1,1,1,1,
1,1,1,1,1,1,4),(0.,0.0642013499338863),(14.3984001269719,15.3848610203769,
16.3713219137819,17.3577828071869,18.3442437005919,19.3307045939969,20.3171654874019,
21.3036263808069,22.2900872742119,23.2765481676169,24.2630090610219,25.2494699544269,
26.2359308478319,27.2223917412369,28.2088526346419,29.1953135280469,30.1817744214519,
31.1682353148569,32.1546962082619,33.1411571016669,34.1276179950719,35.1140788884769,
36.1005397818819,37.0870006752869,38.0734615686919,39.0599224620969,40.0463833555019,
41.0328442489069,42.0193051423119,43.0057660357169,43.9922269291219,44.9786878225269,
45.9651487159319,46.9516096093369,47.9380705027419,48.9245313961469,49.9109922895519,
50.897453182957,51.883914076362,52.870374969767,53.856835863172,54.843296756577,
55.829757649982,56.816218543387,57.802679436792,58.789140330197,59.775601223602,
60.762062117007,61.748523010412,62.734983903817,63.721444797222,64.707905690627,
65.694366584032,66.680827477437),.UNSPECIFIED.);
#277=B_SPLINE_SURFACE_WITH_KNOTS('',3,3,((#50814,#50815,#50816,#50817,#50818,
#50819,#50820,#50821,#50822,#50823,#50824,#50825,#50826,#50827,#50828,#50829,
#50830,#50831,#50832,#50833,#50834,#50835,#50836,#50837,#50838,#50839,#50840,
#50841,#50842,#50843,#50844,#50845,#50846,#50847,#50848,#50849,#50850,#50851,
#50852,#50853,#50854,#50855,#50856,#50857,#50858,#50859,#50860,#50861,#50862,
#50863,#50864,#50865,#50866,#50867,#50868,#50869),(#50870,#50871,#50872,
#50873,#50874,#50875,#50876,#50877,#50878,#50879,#50880,#50881,#50882,#50883,
#50884,#50885,#50886,#50887,#50888,#50889,#50890,#50891,#50892,#50893,#50894,
#50895,#50896,#50897,#50898,#50899,#50900,#50901,#50902,#50903,#50904,#50905,
#50906,#50907,#50908,#50909,#50910,#50911,#50912,#50913,#50914,#50915,#50916,
#50917,#50918,#50919,#50920,#50921,#50922,#50923,#50924,#50925),(#50926,
#50927,#50928,#50929,#50930,#50931,#50932,#50933,#50934,#50935,#50936,#50937,
#50938,#50939,#50940,#50941,#50942,#50943,#50944,#50945,#50946,#50947,#50948,
#50949,#50950,#50951,#50952,#50953,#50954,#50955,#50956,#50957,#50958,#50959,
#50960,#50961,#50962,#50963,#50964,#50965,#50966,#50967,#50968,#50969,#50970,
#50971,#50972,#50973,#50974,#50975,#50976,#50977,#50978,#50979,#50980,#50981),
(#50982,#50983,#50984,#50985,#50986,#50987,#50988,#50989,#50990,#50991,
#50992,#50993,#50994,#50995,#50996,#50997,#50998,#50999,#51000,#51001,#51002,
#51003,#51004,#51005,#51006,#51007,#51008,#51009,#51010,#51011,#51012,#51013,
#51014,#51015,#51016,#51017,#51018,#51019,#51020,#51021,#51022,#51023,#51024,
#51025,#51026,#51027,#51028,#51029,#51030,#51031,#51032,#51033,#51034,#51035,
#51036,#51037)),.UNSPECIFIED.,.F.,.F.,.F.,(4,4),(4,1,1,1,1,1,1,1,1,1,1,
1,1,1,1,1,1,1,1,1,1,1,1,1,1,1,1,1,1,1,1,1,1,1,1,1,1,1,1,1,1,1,1,1,1,1,1,
1,1,1,1,1,1,4),(0.,0.0642013499338863),(11.8589888623078,12.8454497557128,
13.8319106491178,14.8183715425228,15.8048324359278,16.7912933293328,17.7777542227378,
18.7642151161429,19.7506760095479,20.7371369029529,21.7235977963579,22.7100586897629,
23.6965195831679,24.6829804765729,25.6694413699779,26.6559022633829,27.6423631567879,
28.6288240501929,29.6152849435979,30.6017458370029,31.5882067304079,32.5746676238129,
33.5611285172179,34.5475894106229,35.5340503040279,36.5205111974329,37.5069720908379,
38.4934329842429,39.4798938776479,40.4663547710529,41.4528156644579,42.4392765578629,
43.4257374512679,44.4121983446729,45.3986592380779,46.3851201314829,47.3715810248879,
48.3580419182929,49.3445028116979,50.3309637051029,51.3174245985079,52.3038854919129,
53.2903463853179,54.2768072787229,55.2632681721279,56.2497290655329,57.2361899589379,
58.222650852343,59.209111745748,60.195572639153,61.182033532558,62.168494425963,
63.154955319368,64.141416212773),.UNSPECIFIED.);
#278=B_SPLINE_SURFACE_WITH_KNOTS('',3,3,((#51154,#51155,#51156,#51157,#51158,
#51159,#51160,#51161,#51162,#51163,#51164,#51165,#51166,#51167,#51168,#51169,
#51170,#51171,#51172,#51173,#51174,#51175,#51176,#51177,#51178,#51179,#51180,
#51181,#51182,#51183,#51184,#51185,#51186,#51187,#51188,#51189,#51190,#51191,
#51192,#51193,#51194,#51195,#51196,#51197,#51198,#51199,#51200,#51201,#51202,
#51203,#51204,#51205,#51206,#51207,#51208,#51209),(#51210,#51211,#51212,
#51213,#51214,#51215,#51216,#51217,#51218,#51219,#51220,#51221,#51222,#51223,
#51224,#51225,#51226,#51227,#51228,#51229,#51230,#51231,#51232,#51233,#51234,
#51235,#51236,#51237,#51238,#51239,#51240,#51241,#51242,#51243,#51244,#51245,
#51246,#51247,#51248,#51249,#51250,#51251,#51252,#51253,#51254,#51255,#51256,
#51257,#51258,#51259,#51260,#51261,#51262,#51263,#51264,#51265),(#51266,
#51267,#51268,#51269,#51270,#51271,#51272,#51273,#51274,#51275,#51276,#51277,
#51278,#51279,#51280,#51281,#51282,#51283,#51284,#51285,#51286,#51287,#51288,
#51289,#51290,#51291,#51292,#51293,#51294,#51295,#51296,#51297,#51298,#51299,
#51300,#51301,#51302,#51303,#51304,#51305,#51306,#51307,#51308,#51309,#51310,
#51311,#51312,#51313,#51314,#51315,#51316,#51317,#51318,#51319,#51320,#51321),
(#51322,#51323,#51324,#51325,#51326,#51327,#51328,#51329,#51330,#51331,
#51332,#51333,#51334,#51335,#51336,#51337,#51338,#51339,#51340,#51341,#51342,
#51343,#51344,#51345,#51346,#51347,#51348,#51349,#51350,#51351,#51352,#51353,
#51354,#51355,#51356,#51357,#51358,#51359,#51360,#51361,#51362,#51363,#51364,
#51365,#51366,#51367,#51368,#51369,#51370,#51371,#51372,#51373,#51374,#51375,
#51376,#51377)),.UNSPECIFIED.,.F.,.F.,.F.,(4,4),(4,1,1,1,1,1,1,1,1,1,1,
1,1,1,1,1,1,1,1,1,1,1,1,1,1,1,1,1,1,1,1,1,1,1,1,1,1,1,1,1,1,1,1,1,1,1,1,
1,1,1,1,1,1,4),(0.,0.0642013499338863),(14.3984001269719,15.3848610203769,
16.3713219137819,17.3577828071869,18.3442437005919,19.3307045939969,20.3171654874019,
21.3036263808069,22.2900872742119,23.2765481676169,24.2630090610219,25.2494699544269,
26.2359308478319,27.2223917412369,28.2088526346419,29.1953135280469,30.1817744214519,
31.1682353148569,32.1546962082619,33.1411571016669,34.1276179950719,35.1140788884769,
36.1005397818819,37.0870006752869,38.0734615686919,39.0599224620969,40.0463833555019,
41.0328442489069,42.0193051423119,43.0057660357169,43.9922269291219,44.978687822527,
45.965148715932,46.951609609337,47.938070502742,48.924531396147,49.910992289552,
50.897453182957,51.883914076362,52.870374969767,53.856835863172,54.843296756577,
55.829757649982,56.816218543387,57.802679436792,58.789140330197,59.775601223602,
60.762062117007,61.748523010412,62.734983903817,63.721444797222,64.707905690627,
65.694366584032,66.680827477437),.UNSPECIFIED.);
#279=B_SPLINE_SURFACE_WITH_KNOTS('',3,3,((#55973,#55974,#55975,#55976,#55977,
#55978,#55979,#55980,#55981,#55982,#55983,#55984,#55985,#55986,#55987,#55988,
#55989,#55990,#55991,#55992,#55993,#55994,#55995,#55996,#55997,#55998,#55999,
#56000,#56001,#56002,#56003,#56004,#56005,#56006,#56007,#56008,#56009,#56010,
#56011,#56012,#56013,#56014,#56015,#56016,#56017,#56018,#56019,#56020,#56021,
#56022,#56023,#56024,#56025,#56026,#56027,#56028,#56029,#56030,#56031,#56032,
#56033,#56034,#56035,#56036,#56037,#56038,#56039,#56040,#56041,#56042,#56043,
#56044,#56045,#56046,#56047,#56048,#56049,#56050,#56051,#56052,#56053,#56054,
#56055,#56056,#56057,#56058,#56059,#56060,#56061,#56062,#56063,#56064,#56065,
#56066,#56067,#56068,#56069,#56070,#56071,#56072,#56073,#56074,#56075,#56076,
#56077,#56078,#56079,#56080,#56081,#56082,#56083,#56084,#56085,#56086,#56087,
#56088,#56089,#56090,#56091,#56092,#56093,#56094,#56095,#56096,#56097,#56098,
#56099,#56100,#56101,#56102,#56103,#56104,#56105,#56106,#56107,#56108,#56109,
#56110,#56111,#56112,#56113,#56114,#56115,#56116,#56117,#56118,#56119,#56120,
#56121,#56122,#56123,#56124,#56125,#56126,#56127,#56128,#56129,#56130,#56131,
#56132,#56133,#56134,#56135,#56136,#56137,#56138,#56139,#56140,#56141,#56142,
#56143,#56144,#56145,#56146,#56147,#56148,#56149,#56150,#56151,#56152,#56153,
#56154,#56155,#56156,#56157,#56158,#56159,#56160,#56161,#56162,#56163,#56164,
#56165,#56166,#56167,#56168,#56169,#56170,#56171,#56172,#56173,#56174,#56175,
#56176,#56177,#56178,#56179,#56180,#56181,#56182,#56183,#56184,#56185,#56186,
#56187,#56188,#56189,#56190,#56191,#56192,#56193,#56194,#56195,#56196,#56197,
#56198,#56199,#56200,#56201,#56202,#56203,#56204,#56205,#56206,#56207,#56208,
#56209,#56210,#56211,#56212,#56213,#56214,#56215,#56216,#56217,#56218,#56219,
#56220,#56221,#56222,#56223,#56224,#56225,#56226,#56227,#56228,#56229,#56230,
#56231,#56232,#56233,#56234,#56235,#56236,#56237,#56238,#56239,#56240,#56241,
#56242,#56243,#56244,#56245,#56246,#56247,#56248,#56249,#56250,#56251,#56252,
#56253,#56254,#56255,#56256,#56257,#56258,#56259,#56260,#56261,#56262,#56263,
#56264,#56265,#56266,#56267,#56268,#56269,#56270,#56271,#56272,#56273,#56274,
#56275,#56276,#56277,#56278,#56279,#56280,#56281,#56282,#56283,#56284,#56285,
#56286,#56287,#56288,#56289,#56290,#56291,#56292,#56293,#56294,#56295,#56296,
#56297,#56298,#56299,#56300,#56301,#56302,#56303,#56304,#56305,#56306,#56307,
#56308,#56309,#56310,#56311,#56312,#56313,#56314,#56315,#56316,#56317,#56318,
#56319,#56320,#56321,#56322,#56323,#56324,#56325,#56326,#56327,#56328,#56329,
#56330,#56331,#56332,#56333,#56334,#56335,#56336,#56337,#56338,#56339,#56340,
#56341,#56342,#56343,#56344,#56345,#56346,#56347,#56348,#56349,#56350,#56351,
#56352,#56353,#56354,#56355,#56356,#56357),(#56358,#56359,#56360,#56361,
#56362,#56363,#56364,#56365,#56366,#56367,#56368,#56369,#56370,#56371,#56372,
#56373,#56374,#56375,#56376,#56377,#56378,#56379,#56380,#56381,#56382,#56383,
#56384,#56385,#56386,#56387,#56388,#56389,#56390,#56391,#56392,#56393,#56394,
#56395,#56396,#56397,#56398,#56399,#56400,#56401,#56402,#56403,#56404,#56405,
#56406,#56407,#56408,#56409,#56410,#56411,#56412,#56413,#56414,#56415,#56416,
#56417,#56418,#56419,#56420,#56421,#56422,#56423,#56424,#56425,#56426,#56427,
#56428,#56429,#56430,#56431,#56432,#56433,#56434,#56435,#56436,#56437,#56438,
#56439,#56440,#56441,#56442,#56443,#56444,#56445,#56446,#56447,#56448,#56449,
#56450,#56451,#56452,#56453,#56454,#56455,#56456,#56457,#56458,#56459,#56460,
#56461,#56462,#56463,#56464,#56465,#56466,#56467,#56468,#56469,#56470,#56471,
#56472,#56473,#56474,#56475,#56476,#56477,#56478,#56479,#56480,#56481,#56482,
#56483,#56484,#56485,#56486,#56487,#56488,#56489,#56490,#56491,#56492,#56493,
#56494,#56495,#56496,#56497,#56498,#56499,#56500,#56501,#56502,#56503,#56504,
#56505,#56506,#56507,#56508,#56509,#56510,#56511,#56512,#56513,#56514,#56515,
#56516,#56517,#56518,#56519,#56520,#56521,#56522,#56523,#56524,#56525,#56526,
#56527,#56528,#56529,#56530,#56531,#56532,#56533,#56534,#56535,#56536,#56537,
#56538,#56539,#56540,#56541,#56542,#56543,#56544,#56545,#56546,#56547,#56548,
#56549,#56550,#56551,#56552,#56553,#56554,#56555,#56556,#56557,#56558,#56559,
#56560,#56561,#56562,#56563,#56564,#56565,#56566,#56567,#56568,#56569,#56570,
#56571,#56572,#56573,#56574,#56575,#56576,#56577,#56578,#56579,#56580,#56581,
#56582,#56583,#56584,#56585,#56586,#56587,#56588,#56589,#56590,#56591,#56592,
#56593,#56594,#56595,#56596,#56597,#56598,#56599,#56600,#56601,#56602,#56603,
#56604,#56605,#56606,#56607,#56608,#56609,#56610,#56611,#56612,#56613,#56614,
#56615,#56616,#56617,#56618,#56619,#56620,#56621,#56622,#56623,#56624,#56625,
#56626,#56627,#56628,#56629,#56630,#56631,#56632,#56633,#56634,#56635,#56636,
#56637,#56638,#56639,#56640,#56641,#56642,#56643,#56644,#56645,#56646,#56647,
#56648,#56649,#56650,#56651,#56652,#56653,#56654,#56655,#56656,#56657,#56658,
#56659,#56660,#56661,#56662,#56663,#56664,#56665,#56666,#56667,#56668,#56669,
#56670,#56671,#56672,#56673,#56674,#56675,#56676,#56677,#56678,#56679,#56680,
#56681,#56682,#56683,#56684,#56685,#56686,#56687,#56688,#56689,#56690,#56691,
#56692,#56693,#56694,#56695,#56696,#56697,#56698,#56699,#56700,#56701,#56702,
#56703,#56704,#56705,#56706,#56707,#56708,#56709,#56710,#56711,#56712,#56713,
#56714,#56715,#56716,#56717,#56718,#56719,#56720,#56721,#56722,#56723,#56724,
#56725,#56726,#56727,#56728,#56729,#56730,#56731,#56732,#56733,#56734,#56735,
#56736,#56737,#56738,#56739,#56740,#56741,#56742),(#56743,#56744,#56745,
#56746,#56747,#56748,#56749,#56750,#56751,#56752,#56753,#56754,#56755,#56756,
#56757,#56758,#56759,#56760,#56761,#56762,#56763,#56764,#56765,#56766,#56767,
#56768,#56769,#56770,#56771,#56772,#56773,#56774,#56775,#56776,#56777,#56778,
#56779,#56780,#56781,#56782,#56783,#56784,#56785,#56786,#56787,#56788,#56789,
#56790,#56791,#56792,#56793,#56794,#56795,#56796,#56797,#56798,#56799,#56800,
#56801,#56802,#56803,#56804,#56805,#56806,#56807,#56808,#56809,#56810,#56811,
#56812,#56813,#56814,#56815,#56816,#56817,#56818,#56819,#56820,#56821,#56822,
#56823,#56824,#56825,#56826,#56827,#56828,#56829,#56830,#56831,#56832,#56833,
#56834,#56835,#56836,#56837,#56838,#56839,#56840,#56841,#56842,#56843,#56844,
#56845,#56846,#56847,#56848,#56849,#56850,#56851,#56852,#56853,#56854,#56855,
#56856,#56857,#56858,#56859,#56860,#56861,#56862,#56863,#56864,#56865,#56866,
#56867,#56868,#56869,#56870,#56871,#56872,#56873,#56874,#56875,#56876,#56877,
#56878,#56879,#56880,#56881,#56882,#56883,#56884,#56885,#56886,#56887,#56888,
#56889,#56890,#56891,#56892,#56893,#56894,#56895,#56896,#56897,#56898,#56899,
#56900,#56901,#56902,#56903,#56904,#56905,#56906,#56907,#56908,#56909,#56910,
#56911,#56912,#56913,#56914,#56915,#56916,#56917,#56918,#56919,#56920,#56921,
#56922,#56923,#56924,#56925,#56926,#56927,#56928,#56929,#56930,#56931,#56932,
#56933,#56934,#56935,#56936,#56937,#56938,#56939,#56940,#56941,#56942,#56943,
#56944,#56945,#56946,#56947,#56948,#56949,#56950,#56951,#56952,#56953,#56954,
#56955,#56956,#56957,#56958,#56959,#56960,#56961,#56962,#56963,#56964,#56965,
#56966,#56967,#56968,#56969,#56970,#56971,#56972,#56973,#56974,#56975,#56976,
#56977,#56978,#56979,#56980,#56981,#56982,#56983,#56984,#56985,#56986,#56987,
#56988,#56989,#56990,#56991,#56992,#56993,#56994,#56995,#56996,#56997,#56998,
#56999,#57000,#57001,#57002,#57003,#57004,#57005,#57006,#57007,#57008,#57009,
#57010,#57011,#57012,#57013,#57014,#57015,#57016,#57017,#57018,#57019,#57020,
#57021,#57022,#57023,#57024,#57025,#57026,#57027,#57028,#57029,#57030,#57031,
#57032,#57033,#57034,#57035,#57036,#57037,#57038,#57039,#57040,#57041,#57042,
#57043,#57044,#57045,#57046,#57047,#57048,#57049,#57050,#57051,#57052,#57053,
#57054,#57055,#57056,#57057,#57058,#57059,#57060,#57061,#57062,#57063,#57064,
#57065,#57066,#57067,#57068,#57069,#57070,#57071,#57072,#57073,#57074,#57075,
#57076,#57077,#57078,#57079,#57080,#57081,#57082,#57083,#57084,#57085,#57086,
#57087,#57088,#57089,#57090,#57091,#57092,#57093,#57094,#57095,#57096,#57097,
#57098,#57099,#57100,#57101,#57102,#57103,#57104,#57105,#57106,#57107,#57108,
#57109,#57110,#57111,#57112,#57113,#57114,#57115,#57116,#57117,#57118,#57119,
#57120,#57121,#57122,#57123,#57124,#57125,#57126,#57127),(#57128,#57129,
#57130,#57131,#57132,#57133,#57134,#57135,#57136,#57137,#57138,#57139,#57140,
#57141,#57142,#57143,#57144,#57145,#57146,#57147,#57148,#57149,#57150,#57151,
#57152,#57153,#57154,#57155,#57156,#57157,#57158,#57159,#57160,#57161,#57162,
#57163,#57164,#57165,#57166,#57167,#57168,#57169,#57170,#57171,#57172,#57173,
#57174,#57175,#57176,#57177,#57178,#57179,#57180,#57181,#57182,#57183,#57184,
#57185,#57186,#57187,#57188,#57189,#57190,#57191,#57192,#57193,#57194,#57195,
#57196,#57197,#57198,#57199,#57200,#57201,#57202,#57203,#57204,#57205,#57206,
#57207,#57208,#57209,#57210,#57211,#57212,#57213,#57214,#57215,#57216,#57217,
#57218,#57219,#57220,#57221,#57222,#57223,#57224,#57225,#57226,#57227,#57228,
#57229,#57230,#57231,#57232,#57233,#57234,#57235,#57236,#57237,#57238,#57239,
#57240,#57241,#57242,#57243,#57244,#57245,#57246,#57247,#57248,#57249,#57250,
#57251,#57252,#57253,#57254,#57255,#57256,#57257,#57258,#57259,#57260,#57261,
#57262,#57263,#57264,#57265,#57266,#57267,#57268,#57269,#57270,#57271,#57272,
#57273,#57274,#57275,#57276,#57277,#57278,#57279,#57280,#57281,#57282,#57283,
#57284,#57285,#57286,#57287,#57288,#57289,#57290,#57291,#57292,#57293,#57294,
#57295,#57296,#57297,#57298,#57299,#57300,#57301,#57302,#57303,#57304,#57305,
#57306,#57307,#57308,#57309,#57310,#57311,#57312,#57313,#57314,#57315,#57316,
#57317,#57318,#57319,#57320,#57321,#57322,#57323,#57324,#57325,#57326,#57327,
#57328,#57329,#57330,#57331,#57332,#57333,#57334,#57335,#57336,#57337,#57338,
#57339,#57340,#57341,#57342,#57343,#57344,#57345,#57346,#57347,#57348,#57349,
#57350,#57351,#57352,#57353,#57354,#57355,#57356,#57357,#57358,#57359,#57360,
#57361,#57362,#57363,#57364,#57365,#57366,#57367,#57368,#57369,#57370,#57371,
#57372,#57373,#57374,#57375,#57376,#57377,#57378,#57379,#57380,#57381,#57382,
#57383,#57384,#57385,#57386,#57387,#57388,#57389,#57390,#57391,#57392,#57393,
#57394,#57395,#57396,#57397,#57398,#57399,#57400,#57401,#57402,#57403,#57404,
#57405,#57406,#57407,#57408,#57409,#57410,#57411,#57412,#57413,#57414,#57415,
#57416,#57417,#57418,#57419,#57420,#57421,#57422,#57423,#57424,#57425,#57426,
#57427,#57428,#57429,#57430,#57431,#57432,#57433,#57434,#57435,#57436,#57437,
#57438,#57439,#57440,#57441,#57442,#57443,#57444,#57445,#57446,#57447,#57448,
#57449,#57450,#57451,#57452,#57453,#57454,#57455,#57456,#57457,#57458,#57459,
#57460,#57461,#57462,#57463,#57464,#57465,#57466,#57467,#57468,#57469,#57470,
#57471,#57472,#57473,#57474,#57475,#57476,#57477,#57478,#57479,#57480,#57481,
#57482,#57483,#57484,#57485,#57486,#57487,#57488,#57489,#57490,#57491,#57492,
#57493,#57494,#57495,#57496,#57497,#57498,#57499,#57500,#57501,#57502,#57503,
#57504,#57505,#57506,#57507,#57508,#57509,#57510,#57511,#57512)),
 .UNSPECIFIED.,.F.,.F.,.F.,(4,4),(4,1,1,1,1,1,1,1,1,1,1,1,1,1,1,1,1,1,1,
1,1,1,1,1,1,1,1,1,1,1,1,1,1,1,1,1,1,1,1,1,1,1,1,1,1,1,1,1,1,1,1,1,1,1,1,
1,1,1,1,1,1,1,1,1,1,1,1,1,1,1,1,1,1,1,1,1,1,1,1,1,1,1,1,1,1,1,1,1,1,1,1,
1,1,1,1,1,1,1,1,1,1,1,1,1,1,1,1,1,1,1,1,1,1,1,1,1,1,1,1,1,1,1,1,1,1,1,1,
1,1,1,1,1,1,1,1,1,1,1,1,1,1,1,1,1,1,1,1,1,1,1,1,1,1,1,1,1,1,1,1,1,1,1,1,
1,1,1,1,1,1,1,1,1,1,1,1,1,1,1,1,1,1,1,1,1,1,1,1,1,1,1,1,1,1,1,1,1,1,1,1,
1,1,1,1,1,1,1,1,1,1,1,1,1,1,1,1,1,1,1,1,1,1,1,1,1,1,1,1,1,1,1,1,1,1,1,1,
1,1,1,1,1,1,1,1,1,1,1,1,1,1,1,1,1,1,1,1,1,1,1,1,1,1,1,1,1,1,1,1,1,1,1,1,
1,1,1,1,1,1,1,1,1,1,1,1,1,1,1,1,1,1,1,1,1,1,1,1,1,1,1,1,1,1,1,1,1,1,1,1,
1,1,1,1,1,1,1,1,1,1,1,1,1,1,1,1,1,1,1,1,1,1,1,1,1,1,1,1,1,1,1,1,1,1,1,1,
1,1,1,1,1,1,1,1,1,1,1,1,1,1,1,1,1,1,1,1,1,1,1,1,1,1,1,1,1,1,1,1,1,1,1,1,
1,1,1,4),(0.,0.0658179306876174),(8.30838445208392,8.80714609643392,9.30590774078392,
10.3034310294839,11.3009543181839,12.2984776068839,13.2960008955839,14.2935241842839,
15.291047472984,16.288570761684,17.286094050384,18.283617339084,19.281140627784,
20.278663916484,21.276187205184,22.273710493884,23.271233782584,24.268757071284,
25.266280359984,26.263803648684,27.261326937384,28.258850226084,29.256373514784,
30.253896803484,31.251420092184,32.2489433808841,33.2464666695841,34.2439899582841,
35.2415132469841,36.2390365356841,37.2365598243841,38.2340831130841,39.2316064017841,
40.2291296904841,41.2266529791841,42.2241762678841,43.2216995565841,44.2192228452841,
45.2167461339841,46.2142694226841,47.2117927113841,48.2093160000841,49.2068392887841,
50.2043625774841,51.2018858661842,52.1994091548842,53.1969324435842,54.1944557322842,
55.1919790209842,56.1895023096842,57.1870255983842,58.1845488870842,59.1820721757842,
60.1795954644842,61.1771187531842,62.1746420418842,63.1721653305842,64.1696886192842,
65.1672119079842,66.1647351966842,67.1622584853842,68.1597817740843,69.1573050627842,
70.1548283514843,71.1523516401843,72.1498749288843,73.1473982175843,74.1449215062843,
75.1424447949843,76.1399680836843,77.1374913723843,78.1350146610843,79.1325379497843,
80.1300612384843,81.1275845271843,82.1251078158843,83.1226311045843,84.1201543932843,
85.1176776819843,86.1152009706843,87.1127242593844,88.1102475480844,89.1077708367844,
90.1052941254844,91.1028174141844,92.1003407028844,93.0978639915844,94.0953872802844,
95.0929105689844,96.0904338576844,97.0879571463844,98.0854804350844,99.0830037237844,
100.080527012484,101.078050301184,102.075573589884,103.073096878584,104.070620167284,
105.068143455984,106.065666744684,107.063190033384,108.060713322084,109.058236610784,
110.055759899484,111.053283188184,112.050806476884,113.048329765584,114.045853054284,
115.043376342985,116.040899631685,117.038422920385,118.035946209085,119.033469497785,
120.030992786485,121.028516075185,122.026039363885,123.023562652585,124.021085941285,
125.018609229985,126.016132518685,127.013655807385,128.011179096085,129.008702384785,
130.006225673485,131.003748962185,132.001272250885,132.998795539585,133.996318828285,
134.993842116985,135.991365405685,136.988888694385,137.986411983085,138.983935271785,
139.981458560485,140.978981849185,141.976505137885,142.974028426585,143.971551715285,
144.969075003985,145.966598292685,146.964121581385,147.961644870085,148.959168158785,
149.956691447485,150.954214736185,151.951738024885,152.949261313585,153.946784602285,
154.944307890985,155.941831179685,156.939354468385,157.936877757085,158.934401045785,
159.931924334485,160.929447623185,161.926970911885,162.924494200585,163.922017489285,
164.919540777985,165.917064066685,166.914587355385,167.912110644085,168.909633932785,
169.907157221485,170.904680510185,171.902203798885,172.899727087585,173.897250376285,
174.894773664985,175.892296953685,176.889820242385,177.887343531085,178.884866819785,
179.882390108485,180.879913397185,181.877436685885,182.874959974585,183.872483263285,
184.870006551985,185.867529840685,186.865053129385,187.862576418085,188.860099706785,
189.857622995485,190.855146284185,191.852669572885,192.850192861585,193.847716150285,
194.845239438985,195.842762727685,196.840286016385,197.837809305085,198.835332593785,
199.832855882485,200.830379171185,201.827902459885,202.825425748585,203.822949037285,
204.820472325985,205.817995614685,206.815518903385,207.813042192085,208.810565480785,
209.808088769485,210.805612058185,211.803135346885,212.800658635585,213.798181924285,
214.795705212985,215.793228501685,216.790751790385,217.788275079085,218.785798367785,
219.783321656485,220.780844945185,221.778368233885,222.775891522585,223.773414811285,
224.770938099985,225.768461388685,226.765984677385,227.763507966085,228.761031254785,
229.758554543485,230.756077832185,231.753601120885,232.751124409585,233.748647698285,
234.746170986985,235.743694275685,236.741217564385,237.738740853085,238.736264141785,
239.733787430485,240.731310719185,241.728834007885,242.726357296585,243.723880585285,
244.721403873985,245.718927162685,246.716450451385,247.713973740085,248.711497028785,
249.709020317485,250.706543606185,251.704066894885,252.701590183585,253.699113472285,
254.696636760985,255.694160049685,256.691683338385,257.689206627085,258.686729915785,
259.684253204485,260.681776493185,261.679299781885,262.676823070585,263.674346359285,
264.671869647985,265.669392936685,266.666916225385,267.664439514085,268.661962802785,
269.659486091485,270.657009380185,271.654532668885,272.652055957585,273.649579246285,
274.647102534985,275.644625823685,276.642149112385,277.639672401085,278.637195689785,
279.634718978485,280.632242267185,281.629765555885,282.627288844585,283.624812133285,
284.622335421985,285.619858710685,286.617381999385,287.614905288085,288.612428576785,
289.609951865485,290.607475154186,291.604998442886,292.602521731586,293.600045020286,
294.597568308986,295.595091597686,296.592614886386,297.590138175086,298.587661463786,
299.585184752486,300.582708041186,301.580231329886,302.577754618586,303.575277907286,
304.572801195986,305.570324484686,306.567847773386,307.565371062086,308.562894350786,
309.560417639486,310.557940928186,311.555464216886,312.552987505586,313.550510794286,
314.548034082986,315.545557371686,316.543080660386,317.540603949086,318.538127237786,
319.535650526486,320.533173815186,321.530697103886,322.528220392586,323.525743681286,
324.523266969986,325.520790258686,326.518313547386,327.515836836086,328.513360124786,
329.510883413486,330.508406702186,331.505929990886,332.503453279586,333.500976568286,
334.498499856986,335.496023145686,336.493546434386,337.491069723086,338.488593011786,
339.486116300486,340.483639589186,341.481162877886,342.478686166586,343.476209455286,
344.473732743986,345.471256032686,346.468779321386,347.466302610086,348.463825898786,
349.461349187486,350.458872476186,351.456395764886,352.453919053586,353.451442342286,
354.448965630986,355.446488919686,356.444012208386,357.441535497086,358.439058785786,
359.436582074486,360.434105363186,361.431628651886,362.429151940586,363.426675229286,
364.424198517986,365.421721806686,366.419245095386,367.416768384086,368.414291672786,
369.411814961486,370.409338250186,371.406861538886,372.404384827586,373.401908116286,
374.399431404986,375.396954693686,376.394477982386,377.392001271086,378.389524559786,
379.387047848486,380.384571137186,381.382094425886,382.379617714586,383.377141003286,
384.374664291986,385.372187580686,386.369710869386,386.868472513736,387.367234158086),
 .UNSPECIFIED.);
#280=B_SPLINE_SURFACE_WITH_KNOTS('',3,3,((#57770,#57771,#57772,#57773,#57774,
#57775,#57776,#57777,#57778,#57779,#57780,#57781,#57782,#57783,#57784,#57785,
#57786,#57787,#57788,#57789,#57790,#57791,#57792,#57793,#57794,#57795,#57796,
#57797,#57798,#57799,#57800,#57801,#57802,#57803,#57804,#57805,#57806,#57807,
#57808,#57809,#57810,#57811,#57812,#57813,#57814,#57815,#57816,#57817,#57818,
#57819,#57820,#57821,#57822,#57823,#57824,#57825,#57826,#57827,#57828,#57829,
#57830,#57831,#57832,#57833,#57834,#57835,#57836,#57837,#57838,#57839,#57840,
#57841,#57842,#57843,#57844,#57845,#57846,#57847,#57848,#57849,#57850,#57851,
#57852,#57853,#57854,#57855,#57856,#57857,#57858,#57859,#57860,#57861,#57862,
#57863,#57864,#57865,#57866,#57867,#57868,#57869,#57870,#57871,#57872,#57873,
#57874,#57875,#57876,#57877,#57878,#57879,#57880,#57881,#57882,#57883,#57884,
#57885,#57886,#57887,#57888,#57889,#57890,#57891,#57892,#57893,#57894,#57895,
#57896,#57897,#57898,#57899,#57900,#57901,#57902,#57903,#57904,#57905,#57906,
#57907,#57908,#57909,#57910,#57911,#57912,#57913,#57914,#57915,#57916,#57917,
#57918,#57919,#57920,#57921,#57922,#57923,#57924,#57925,#57926,#57927,#57928,
#57929,#57930,#57931,#57932,#57933,#57934,#57935,#57936,#57937,#57938,#57939,
#57940,#57941,#57942,#57943,#57944,#57945,#57946,#57947,#57948,#57949,#57950,
#57951,#57952,#57953,#57954,#57955,#57956,#57957,#57958,#57959,#57960,#57961,
#57962,#57963,#57964,#57965,#57966,#57967,#57968,#57969,#57970,#57971,#57972,
#57973,#57974,#57975,#57976,#57977,#57978,#57979,#57980,#57981,#57982,#57983,
#57984,#57985,#57986,#57987,#57988,#57989,#57990,#57991,#57992,#57993,#57994,
#57995,#57996,#57997,#57998,#57999,#58000,#58001,#58002,#58003,#58004,#58005,
#58006,#58007,#58008,#58009,#58010,#58011,#58012,#58013,#58014,#58015,#58016,
#58017,#58018,#58019,#58020,#58021,#58022,#58023,#58024,#58025,#58026,#58027,
#58028,#58029,#58030,#58031,#58032,#58033,#58034,#58035,#58036,#58037,#58038,
#58039,#58040,#58041,#58042,#58043,#58044,#58045,#58046,#58047,#58048,#58049,
#58050,#58051,#58052,#58053,#58054,#58055,#58056,#58057,#58058,#58059,#58060,
#58061,#58062,#58063,#58064,#58065,#58066,#58067,#58068,#58069,#58070,#58071,
#58072,#58073,#58074,#58075,#58076,#58077,#58078,#58079,#58080,#58081,#58082,
#58083,#58084,#58085,#58086,#58087,#58088,#58089,#58090,#58091,#58092,#58093,
#58094,#58095,#58096,#58097,#58098,#58099,#58100,#58101,#58102,#58103,#58104,
#58105,#58106,#58107,#58108,#58109,#58110,#58111,#58112,#58113,#58114,#58115,
#58116,#58117,#58118,#58119,#58120,#58121,#58122,#58123,#58124,#58125,#58126,
#58127,#58128,#58129,#58130,#58131,#58132,#58133,#58134,#58135,#58136,#58137,
#58138,#58139,#58140,#58141,#58142,#58143,#58144,#58145,#58146,#58147,#58148,
#58149,#58150,#58151,#58152,#58153,#58154),(#58155,#58156,#58157,#58158,
#58159,#58160,#58161,#58162,#58163,#58164,#58165,#58166,#58167,#58168,#58169,
#58170,#58171,#58172,#58173,#58174,#58175,#58176,#58177,#58178,#58179,#58180,
#58181,#58182,#58183,#58184,#58185,#58186,#58187,#58188,#58189,#58190,#58191,
#58192,#58193,#58194,#58195,#58196,#58197,#58198,#58199,#58200,#58201,#58202,
#58203,#58204,#58205,#58206,#58207,#58208,#58209,#58210,#58211,#58212,#58213,
#58214,#58215,#58216,#58217,#58218,#58219,#58220,#58221,#58222,#58223,#58224,
#58225,#58226,#58227,#58228,#58229,#58230,#58231,#58232,#58233,#58234,#58235,
#58236,#58237,#58238,#58239,#58240,#58241,#58242,#58243,#58244,#58245,#58246,
#58247,#58248,#58249,#58250,#58251,#58252,#58253,#58254,#58255,#58256,#58257,
#58258,#58259,#58260,#58261,#58262,#58263,#58264,#58265,#58266,#58267,#58268,
#58269,#58270,#58271,#58272,#58273,#58274,#58275,#58276,#58277,#58278,#58279,
#58280,#58281,#58282,#58283,#58284,#58285,#58286,#58287,#58288,#58289,#58290,
#58291,#58292,#58293,#58294,#58295,#58296,#58297,#58298,#58299,#58300,#58301,
#58302,#58303,#58304,#58305,#58306,#58307,#58308,#58309,#58310,#58311,#58312,
#58313,#58314,#58315,#58316,#58317,#58318,#58319,#58320,#58321,#58322,#58323,
#58324,#58325,#58326,#58327,#58328,#58329,#58330,#58331,#58332,#58333,#58334,
#58335,#58336,#58337,#58338,#58339,#58340,#58341,#58342,#58343,#58344,#58345,
#58346,#58347,#58348,#58349,#58350,#58351,#58352,#58353,#58354,#58355,#58356,
#58357,#58358,#58359,#58360,#58361,#58362,#58363,#58364,#58365,#58366,#58367,
#58368,#58369,#58370,#58371,#58372,#58373,#58374,#58375,#58376,#58377,#58378,
#58379,#58380,#58381,#58382,#58383,#58384,#58385,#58386,#58387,#58388,#58389,
#58390,#58391,#58392,#58393,#58394,#58395,#58396,#58397,#58398,#58399,#58400,
#58401,#58402,#58403,#58404,#58405,#58406,#58407,#58408,#58409,#58410,#58411,
#58412,#58413,#58414,#58415,#58416,#58417,#58418,#58419,#58420,#58421,#58422,
#58423,#58424,#58425,#58426,#58427,#58428,#58429,#58430,#58431,#58432,#58433,
#58434,#58435,#58436,#58437,#58438,#58439,#58440,#58441,#58442,#58443,#58444,
#58445,#58446,#58447,#58448,#58449,#58450,#58451,#58452,#58453,#58454,#58455,
#58456,#58457,#58458,#58459,#58460,#58461,#58462,#58463,#58464,#58465,#58466,
#58467,#58468,#58469,#58470,#58471,#58472,#58473,#58474,#58475,#58476,#58477,
#58478,#58479,#58480,#58481,#58482,#58483,#58484,#58485,#58486,#58487,#58488,
#58489,#58490,#58491,#58492,#58493,#58494,#58495,#58496,#58497,#58498,#58499,
#58500,#58501,#58502,#58503,#58504,#58505,#58506,#58507,#58508,#58509,#58510,
#58511,#58512,#58513,#58514,#58515,#58516,#58517,#58518,#58519,#58520,#58521,
#58522,#58523,#58524,#58525,#58526,#58527,#58528,#58529,#58530,#58531,#58532,
#58533,#58534,#58535,#58536,#58537,#58538,#58539),(#58540,#58541,#58542,
#58543,#58544,#58545,#58546,#58547,#58548,#58549,#58550,#58551,#58552,#58553,
#58554,#58555,#58556,#58557,#58558,#58559,#58560,#58561,#58562,#58563,#58564,
#58565,#58566,#58567,#58568,#58569,#58570,#58571,#58572,#58573,#58574,#58575,
#58576,#58577,#58578,#58579,#58580,#58581,#58582,#58583,#58584,#58585,#58586,
#58587,#58588,#58589,#58590,#58591,#58592,#58593,#58594,#58595,#58596,#58597,
#58598,#58599,#58600,#58601,#58602,#58603,#58604,#58605,#58606,#58607,#58608,
#58609,#58610,#58611,#58612,#58613,#58614,#58615,#58616,#58617,#58618,#58619,
#58620,#58621,#58622,#58623,#58624,#58625,#58626,#58627,#58628,#58629,#58630,
#58631,#58632,#58633,#58634,#58635,#58636,#58637,#58638,#58639,#58640,#58641,
#58642,#58643,#58644,#58645,#58646,#58647,#58648,#58649,#58650,#58651,#58652,
#58653,#58654,#58655,#58656,#58657,#58658,#58659,#58660,#58661,#58662,#58663,
#58664,#58665,#58666,#58667,#58668,#58669,#58670,#58671,#58672,#58673,#58674,
#58675,#58676,#58677,#58678,#58679,#58680,#58681,#58682,#58683,#58684,#58685,
#58686,#58687,#58688,#58689,#58690,#58691,#58692,#58693,#58694,#58695,#58696,
#58697,#58698,#58699,#58700,#58701,#58702,#58703,#58704,#58705,#58706,#58707,
#58708,#58709,#58710,#58711,#58712,#58713,#58714,#58715,#58716,#58717,#58718,
#58719,#58720,#58721,#58722,#58723,#58724,#58725,#58726,#58727,#58728,#58729,
#58730,#58731,#58732,#58733,#58734,#58735,#58736,#58737,#58738,#58739,#58740,
#58741,#58742,#58743,#58744,#58745,#58746,#58747,#58748,#58749,#58750,#58751,
#58752,#58753,#58754,#58755,#58756,#58757,#58758,#58759,#58760,#58761,#58762,
#58763,#58764,#58765,#58766,#58767,#58768,#58769,#58770,#58771,#58772,#58773,
#58774,#58775,#58776,#58777,#58778,#58779,#58780,#58781,#58782,#58783,#58784,
#58785,#58786,#58787,#58788,#58789,#58790,#58791,#58792,#58793,#58794,#58795,
#58796,#58797,#58798,#58799,#58800,#58801,#58802,#58803,#58804,#58805,#58806,
#58807,#58808,#58809,#58810,#58811,#58812,#58813,#58814,#58815,#58816,#58817,
#58818,#58819,#58820,#58821,#58822,#58823,#58824,#58825,#58826,#58827,#58828,
#58829,#58830,#58831,#58832,#58833,#58834,#58835,#58836,#58837,#58838,#58839,
#58840,#58841,#58842,#58843,#58844,#58845,#58846,#58847,#58848,#58849,#58850,
#58851,#58852,#58853,#58854,#58855,#58856,#58857,#58858,#58859,#58860,#58861,
#58862,#58863,#58864,#58865,#58866,#58867,#58868,#58869,#58870,#58871,#58872,
#58873,#58874,#58875,#58876,#58877,#58878,#58879,#58880,#58881,#58882,#58883,
#58884,#58885,#58886,#58887,#58888,#58889,#58890,#58891,#58892,#58893,#58894,
#58895,#58896,#58897,#58898,#58899,#58900,#58901,#58902,#58903,#58904,#58905,
#58906,#58907,#58908,#58909,#58910,#58911,#58912,#58913,#58914,#58915,#58916,
#58917,#58918,#58919,#58920,#58921,#58922,#58923,#58924),(#58925,#58926,
#58927,#58928,#58929,#58930,#58931,#58932,#58933,#58934,#58935,#58936,#58937,
#58938,#58939,#58940,#58941,#58942,#58943,#58944,#58945,#58946,#58947,#58948,
#58949,#58950,#58951,#58952,#58953,#58954,#58955,#58956,#58957,#58958,#58959,
#58960,#58961,#58962,#58963,#58964,#58965,#58966,#58967,#58968,#58969,#58970,
#58971,#58972,#58973,#58974,#58975,#58976,#58977,#58978,#58979,#58980,#58981,
#58982,#58983,#58984,#58985,#58986,#58987,#58988,#58989,#58990,#58991,#58992,
#58993,#58994,#58995,#58996,#58997,#58998,#58999,#59000,#59001,#59002,#59003,
#59004,#59005,#59006,#59007,#59008,#59009,#59010,#59011,#59012,#59013,#59014,
#59015,#59016,#59017,#59018,#59019,#59020,#59021,#59022,#59023,#59024,#59025,
#59026,#59027,#59028,#59029,#59030,#59031,#59032,#59033,#59034,#59035,#59036,
#59037,#59038,#59039,#59040,#59041,#59042,#59043,#59044,#59045,#59046,#59047,
#59048,#59049,#59050,#59051,#59052,#59053,#59054,#59055,#59056,#59057,#59058,
#59059,#59060,#59061,#59062,#59063,#59064,#59065,#59066,#59067,#59068,#59069,
#59070,#59071,#59072,#59073,#59074,#59075,#59076,#59077,#59078,#59079,#59080,
#59081,#59082,#59083,#59084,#59085,#59086,#59087,#59088,#59089,#59090,#59091,
#59092,#59093,#59094,#59095,#59096,#59097,#59098,#59099,#59100,#59101,#59102,
#59103,#59104,#59105,#59106,#59107,#59108,#59109,#59110,#59111,#59112,#59113,
#59114,#59115,#59116,#59117,#59118,#59119,#59120,#59121,#59122,#59123,#59124,
#59125,#59126,#59127,#59128,#59129,#59130,#59131,#59132,#59133,#59134,#59135,
#59136,#59137,#59138,#59139,#59140,#59141,#59142,#59143,#59144,#59145,#59146,
#59147,#59148,#59149,#59150,#59151,#59152,#59153,#59154,#59155,#59156,#59157,
#59158,#59159,#59160,#59161,#59162,#59163,#59164,#59165,#59166,#59167,#59168,
#59169,#59170,#59171,#59172,#59173,#59174,#59175,#59176,#59177,#59178,#59179,
#59180,#59181,#59182,#59183,#59184,#59185,#59186,#59187,#59188,#59189,#59190,
#59191,#59192,#59193,#59194,#59195,#59196,#59197,#59198,#59199,#59200,#59201,
#59202,#59203,#59204,#59205,#59206,#59207,#59208,#59209,#59210,#59211,#59212,
#59213,#59214,#59215,#59216,#59217,#59218,#59219,#59220,#59221,#59222,#59223,
#59224,#59225,#59226,#59227,#59228,#59229,#59230,#59231,#59232,#59233,#59234,
#59235,#59236,#59237,#59238,#59239,#59240,#59241,#59242,#59243,#59244,#59245,
#59246,#59247,#59248,#59249,#59250,#59251,#59252,#59253,#59254,#59255,#59256,
#59257,#59258,#59259,#59260,#59261,#59262,#59263,#59264,#59265,#59266,#59267,
#59268,#59269,#59270,#59271,#59272,#59273,#59274,#59275,#59276,#59277,#59278,
#59279,#59280,#59281,#59282,#59283,#59284,#59285,#59286,#59287,#59288,#59289,
#59290,#59291,#59292,#59293,#59294,#59295,#59296,#59297,#59298,#59299,#59300,
#59301,#59302,#59303,#59304,#59305,#59306,#59307,#59308,#59309)),
 .UNSPECIFIED.,.F.,.F.,.F.,(4,4),(4,1,1,1,1,1,1,1,1,1,1,1,1,1,1,1,1,1,1,
1,1,1,1,1,1,1,1,1,1,1,1,1,1,1,1,1,1,1,1,1,1,1,1,1,1,1,1,1,1,1,1,1,1,1,1,
1,1,1,1,1,1,1,1,1,1,1,1,1,1,1,1,1,1,1,1,1,1,1,1,1,1,1,1,1,1,1,1,1,1,1,1,
1,1,1,1,1,1,1,1,1,1,1,1,1,1,1,1,1,1,1,1,1,1,1,1,1,1,1,1,1,1,1,1,1,1,1,1,
1,1,1,1,1,1,1,1,1,1,1,1,1,1,1,1,1,1,1,1,1,1,1,1,1,1,1,1,1,1,1,1,1,1,1,1,
1,1,1,1,1,1,1,1,1,1,1,1,1,1,1,1,1,1,1,1,1,1,1,1,1,1,1,1,1,1,1,1,1,1,1,1,
1,1,1,1,1,1,1,1,1,1,1,1,1,1,1,1,1,1,1,1,1,1,1,1,1,1,1,1,1,1,1,1,1,1,1,1,
1,1,1,1,1,1,1,1,1,1,1,1,1,1,1,1,1,1,1,1,1,1,1,1,1,1,1,1,1,1,1,1,1,1,1,1,
1,1,1,1,1,1,1,1,1,1,1,1,1,1,1,1,1,1,1,1,1,1,1,1,1,1,1,1,1,1,1,1,1,1,1,1,
1,1,1,1,1,1,1,1,1,1,1,1,1,1,1,1,1,1,1,1,1,1,1,1,1,1,1,1,1,1,1,1,1,1,1,1,
1,1,1,1,1,1,1,1,1,1,1,1,1,1,1,1,1,1,1,1,1,1,1,1,1,1,1,1,1,1,1,1,1,1,1,1,
1,1,1,4),(0.,0.0658179306876174),(11.6150328478191,12.1137944921691,12.6125561365191,
13.6100794252191,14.6076027139191,15.6051260026191,16.6026492913191,17.6001725800191,
18.5976958687191,19.5952191574192,20.5927424461192,21.5902657348192,22.5877890235192,
23.5853123122192,24.5828356009192,25.5803588896192,26.5778821783192,27.5754054670192,
28.5729287557192,29.5704520444192,30.5679753331192,31.5654986218192,32.5630219105192,
33.5605451992192,34.5580684879192,35.5555917766192,36.5531150653192,37.5506383540192,
38.5481616427193,39.5456849314193,40.5432082201193,41.5407315088193,42.5382547975193,
43.5357780862193,44.5333013749193,45.5308246636193,46.5283479523193,47.5258712410193,
48.5233945297193,49.5209178184193,50.5184411071193,51.5159643958193,52.5134876845193,
53.5110109732193,54.5085342619193,55.5060575506193,56.5035808393194,57.5011041280194,
58.4986274167194,59.4961507054194,60.4936739941194,61.4911972828194,62.4887205715194,
63.4862438602194,64.4837671489194,65.4812904376194,66.4788137263194,67.4763370150194,
68.4738603037194,69.4713835924194,70.4689068811194,71.4664301698194,72.4639534585194,
73.4614767472195,74.4590000359194,75.4565233246195,76.4540466133195,77.4515699020195,
78.4490931907195,79.4466164794195,80.4441397681195,81.4416630568195,82.4391863455195,
83.4367096342195,84.4342329229195,85.4317562116195,86.4292795003195,87.4268027890195,
88.4243260777195,89.4218493664195,90.4193726551195,91.4168959438195,92.4144192325195,
93.4119425212196,94.4094658099196,95.4069890986196,96.4045123873196,97.4020356760196,
98.3995589647196,99.3970822534196,100.39460554212,101.39212883082,102.38965211952,
103.38717540822,104.38469869692,105.38222198562,106.37974527432,107.37726856302,
108.37479185172,109.37231514042,110.36983842912,111.36736171782,112.36488500652,
113.36240829522,114.35993158392,115.35745487262,116.35497816132,117.35250145002,
118.35002473872,119.34754802742,120.34507131612,121.34259460482,122.34011789352,
123.33764118222,124.33516447092,125.33268775962,126.33021104832,127.32773433702,
128.32525762572,129.32278091442,130.32030420312,131.31782749182,132.31535078052,
133.31287406922,134.31039735792,135.30792064662,136.30544393532,137.30296722402,
138.30049051272,139.29801380142,140.29553709012,141.29306037882,142.29058366752,
143.28810695622,144.28563024492,145.28315353362,146.28067682232,147.27820011102,
148.27572339972,149.27324668842,150.27076997712,151.26829326582,152.26581655452,
153.26333984322,154.26086313192,155.25838642062,156.25590970932,157.25343299802,
158.25095628672,159.24847957542,160.24600286412,161.24352615282,162.24104944152,
163.23857273022,164.23609601892,165.23361930762,166.23114259632,167.22866588502,
168.22618917372,169.22371246242,170.22123575112,171.21875903982,172.21628232852,
173.21380561722,174.21132890592,175.20885219462,176.20637548332,177.20389877202,
178.20142206072,179.19894534942,180.19646863812,181.19399192682,182.19151521552,
183.18903850422,184.18656179292,185.18408508162,186.18160837032,187.17913165902,
188.17665494772,189.17417823642,190.17170152512,191.16922481382,192.16674810252,
193.16427139122,194.16179467992,195.15931796862,196.15684125732,197.15436454602,
198.15188783472,199.14941112342,200.14693441212,201.14445770082,202.14198098952,
203.13950427822,204.13702756692,205.13455085562,206.13207414432,207.12959743302,
208.12712072172,209.12464401042,210.12216729912,211.11969058782,212.11721387652,
213.11473716522,214.11226045392,215.10978374262,216.10730703132,217.10483032002,
218.10235360872,219.09987689742,220.09740018612,221.09492347482,222.09244676352,
223.08997005222,224.08749334092,225.08501662962,226.08253991832,227.08006320702,
228.07758649572,229.07510978442,230.07263307312,231.07015636182,232.06767965052,
233.06520293922,234.06272622792,235.06024951662,236.05777280532,237.05529609402,
238.05281938272,239.05034267142,240.04786596012,241.04538924882,242.04291253752,
243.04043582622,244.03795911492,245.03548240362,246.03300569232,247.03052898102,
248.02805226972,249.02557555842,250.02309884712,251.02062213582,252.01814542452,
253.01566871322,254.01319200192,255.01071529062,256.00823857932,257.00576186802,
258.00328515672,259.00080844542,259.99833173412,260.99585502282,261.99337831152,
262.99090160022,263.98842488892,264.98594817762,265.983471466321,266.980994755021,
267.97851804372,268.97604133242,269.973564621121,270.971087909821,271.968611198521,
272.966134487221,273.963657775921,274.961181064621,275.958704353321,276.956227642021,
277.953750930721,278.951274219421,279.948797508121,280.946320796821,281.943844085521,
282.941367374221,283.938890662921,284.936413951621,285.933937240321,286.931460529021,
287.928983817721,288.926507106421,289.924030395121,290.921553683821,291.919076972521,
292.916600261221,293.914123549921,294.911646838621,295.909170127321,296.906693416021,
297.904216704721,298.901739993421,299.899263282121,300.896786570821,301.894309859521,
302.891833148221,303.889356436921,304.886879725621,305.884403014321,306.881926303021,
307.879449591721,308.876972880421,309.874496169121,310.872019457821,311.869542746521,
312.867066035221,313.864589323921,314.862112612621,315.859635901321,316.857159190021,
317.854682478721,318.852205767421,319.849729056121,320.847252344821,321.844775633521,
322.842298922221,323.839822210921,324.837345499621,325.834868788321,326.832392077021,
327.829915365721,328.827438654421,329.824961943121,330.822485231821,331.820008520521,
332.817531809221,333.815055097921,334.812578386621,335.810101675321,336.807624964021,
337.805148252721,338.802671541421,339.800194830121,340.797718118821,341.795241407521,
342.792764696221,343.790287984921,344.787811273621,345.785334562321,346.782857851021,
347.780381139721,348.777904428421,349.775427717121,350.772951005821,351.770474294521,
352.767997583221,353.765520871921,354.763044160621,355.760567449321,356.758090738021,
357.755614026721,358.753137315421,359.750660604121,360.748183892821,361.745707181521,
362.743230470221,363.740753758921,364.738277047621,365.735800336321,366.733323625021,
367.730846913721,368.728370202421,369.725893491121,370.723416779821,371.720940068521,
372.718463357221,373.715986645921,374.713509934621,375.711033223321,376.708556512021,
377.706079800721,378.703603089421,379.701126378121,380.698649666821,381.696172955521,
382.693696244221,383.691219532921,384.688742821621,385.686266110321,386.683789399021,
387.681312687721,388.678835976421,389.676359265121,390.175120909471,390.673882553821),
 .UNSPECIFIED.);
#281=B_SPLINE_SURFACE_WITH_KNOTS('',3,3,((#60172,#60173,#60174,#60175,#60176,
#60177,#60178,#60179,#60180,#60181,#60182,#60183,#60184,#60185,#60186,#60187,
#60188,#60189,#60190,#60191,#60192,#60193,#60194,#60195,#60196,#60197,#60198,
#60199,#60200,#60201,#60202,#60203,#60204,#60205,#60206,#60207,#60208,#60209,
#60210,#60211,#60212,#60213,#60214,#60215,#60216,#60217,#60218,#60219,#60220,
#60221,#60222,#60223,#60224,#60225,#60226,#60227,#60228,#60229),(#60230,
#60231,#60232,#60233,#60234,#60235,#60236,#60237,#60238,#60239,#60240,#60241,
#60242,#60243,#60244,#60245,#60246,#60247,#60248,#60249,#60250,#60251,#60252,
#60253,#60254,#60255,#60256,#60257,#60258,#60259,#60260,#60261,#60262,#60263,
#60264,#60265,#60266,#60267,#60268,#60269,#60270,#60271,#60272,#60273,#60274,
#60275,#60276,#60277,#60278,#60279,#60280,#60281,#60282,#60283,#60284,#60285,
#60286,#60287),(#60288,#60289,#60290,#60291,#60292,#60293,#60294,#60295,
#60296,#60297,#60298,#60299,#60300,#60301,#60302,#60303,#60304,#60305,#60306,
#60307,#60308,#60309,#60310,#60311,#60312,#60313,#60314,#60315,#60316,#60317,
#60318,#60319,#60320,#60321,#60322,#60323,#60324,#60325,#60326,#60327,#60328,
#60329,#60330,#60331,#60332,#60333,#60334,#60335,#60336,#60337,#60338,#60339,
#60340,#60341,#60342,#60343,#60344,#60345),(#60346,#60347,#60348,#60349,
#60350,#60351,#60352,#60353,#60354,#60355,#60356,#60357,#60358,#60359,#60360,
#60361,#60362,#60363,#60364,#60365,#60366,#60367,#60368,#60369,#60370,#60371,
#60372,#60373,#60374,#60375,#60376,#60377,#60378,#60379,#60380,#60381,#60382,
#60383,#60384,#60385,#60386,#60387,#60388,#60389,#60390,#60391,#60392,#60393,
#60394,#60395,#60396,#60397,#60398,#60399,#60400,#60401,#60402,#60403)),
 .UNSPECIFIED.,.F.,.F.,.F.,(4,4),(4,1,1,1,1,1,1,1,1,1,1,1,1,1,1,1,1,1,1,
1,1,1,1,1,1,1,1,1,1,1,1,1,1,1,1,1,1,1,1,1,1,1,1,1,1,1,1,1,1,1,1,1,1,1,1,
4),(0.,0.0641840294258107),(11.8589888623078,12.3522141756159,12.8454394889239,
13.8318901155401,14.8183407421562,15.8047913687724,16.7912419953885,17.7776926220047,
18.7641432486208,19.750593875237,20.7370445018531,21.7234951284693,22.7099457550854,
23.6963963817016,24.6828470083177,25.6692976349339,26.65574826155,27.6421988881662,
28.6286495147823,29.6151001413985,30.6015507680146,31.5880013946308,32.5744520212469,
33.5609026478631,34.5473532744792,35.5338039010954,36.5202545277115,37.5067051543277,
38.4931557809438,39.47960640756,40.4660570341761,41.4525076607923,42.4389582874084,
43.4254089140245,44.4118595406407,45.3983101672568,46.384760793873,47.3712114204891,
48.3576620471053,49.3441126737214,50.3305633003376,51.3170139269537,52.3034645535699,
53.289915180186,54.2763658068022,55.2628164334183,56.2492670600345,57.2357176866506,
58.2221683132668,59.2086189398829,60.1950695664991,61.1815201931152,62.1679708197314,
63.1544214463475,63.6476467596556,64.1408720729637),.UNSPECIFIED.);
#282=B_SPLINE_SURFACE_WITH_KNOTS('',3,3,((#60638,#60639,#60640,#60641,#60642,
#60643,#60644,#60645,#60646,#60647,#60648,#60649,#60650,#60651,#60652,#60653,
#60654,#60655,#60656,#60657,#60658,#60659,#60660,#60661,#60662,#60663,#60664,
#60665,#60666,#60667,#60668,#60669,#60670,#60671,#60672,#60673,#60674,#60675,
#60676,#60677,#60678,#60679,#60680,#60681,#60682,#60683,#60684,#60685,#60686,
#60687,#60688,#60689,#60690,#60691,#60692,#60693,#60694,#60695),(#60696,
#60697,#60698,#60699,#60700,#60701,#60702,#60703,#60704,#60705,#60706,#60707,
#60708,#60709,#60710,#60711,#60712,#60713,#60714,#60715,#60716,#60717,#60718,
#60719,#60720,#60721,#60722,#60723,#60724,#60725,#60726,#60727,#60728,#60729,
#60730,#60731,#60732,#60733,#60734,#60735,#60736,#60737,#60738,#60739,#60740,
#60741,#60742,#60743,#60744,#60745,#60746,#60747,#60748,#60749,#60750,#60751,
#60752,#60753),(#60754,#60755,#60756,#60757,#60758,#60759,#60760,#60761,
#60762,#60763,#60764,#60765,#60766,#60767,#60768,#60769,#60770,#60771,#60772,
#60773,#60774,#60775,#60776,#60777,#60778,#60779,#60780,#60781,#60782,#60783,
#60784,#60785,#60786,#60787,#60788,#60789,#60790,#60791,#60792,#60793,#60794,
#60795,#60796,#60797,#60798,#60799,#60800,#60801,#60802,#60803,#60804,#60805,
#60806,#60807,#60808,#60809,#60810,#60811),(#60812,#60813,#60814,#60815,
#60816,#60817,#60818,#60819,#60820,#60821,#60822,#60823,#60824,#60825,#60826,
#60827,#60828,#60829,#60830,#60831,#60832,#60833,#60834,#60835,#60836,#60837,
#60838,#60839,#60840,#60841,#60842,#60843,#60844,#60845,#60846,#60847,#60848,
#60849,#60850,#60851,#60852,#60853,#60854,#60855,#60856,#60857,#60858,#60859,
#60860,#60861,#60862,#60863,#60864,#60865,#60866,#60867,#60868,#60869)),
 .UNSPECIFIED.,.F.,.F.,.F.,(4,4),(4,1,1,1,1,1,1,1,1,1,1,1,1,1,1,1,1,1,1,
1,1,1,1,1,1,1,1,1,1,1,1,1,1,1,1,1,1,1,1,1,1,1,1,1,1,1,1,1,1,1,1,1,1,1,1,
4),(0.,0.0641840294258107),(14.3989442667811,14.8921695800892,15.3853948933972,
16.3718455200134,17.3582961466295,18.3447467732457,19.3311973998618,20.317648026478,
21.3040986530941,22.2905492797103,23.2769999063264,24.2634505329426,25.2499011595587,
26.2363517861749,27.222802412791,28.2092530394072,29.1957036660233,30.1821542926395,
31.1686049192556,32.1550555458718,33.1415061724879,34.1279567991041,35.1144074257202,
36.1008580523364,37.0873086789525,38.0737593055687,39.0602099321848,40.046660558801,
41.0331111854171,42.0195618120333,43.0060124386494,43.9924630652656,44.9789136918817,
45.9653643184979,46.951814945114,47.9382655717301,48.9247161983463,49.9111668249625,
50.8976174515786,51.8840680781948,52.8705187048109,53.856969331427,54.8434199580432,
55.8298705846593,56.8163212112755,57.8027718378916,58.7892224645078,59.7756730911239,
60.7621237177401,61.7485743443562,62.7350249709724,63.7214755975885,64.7079262242047,
65.6943768508208,66.1876021641289,66.680827477437),.UNSPECIFIED.);
#283=B_SPLINE_SURFACE_WITH_KNOTS('',3,3,((#62572,#62573,#62574,#62575,#62576,
#62577,#62578,#62579,#62580,#62581,#62582,#62583,#62584,#62585,#62586,#62587,
#62588,#62589,#62590,#62591,#62592,#62593,#62594,#62595,#62596,#62597,#62598,
#62599,#62600,#62601,#62602,#62603,#62604,#62605,#62606,#62607,#62608,#62609,
#62610,#62611,#62612,#62613,#62614,#62615,#62616,#62617,#62618,#62619,#62620,
#62621,#62622,#62623,#62624,#62625,#62626,#62627,#62628,#62629,#62630,#62631,
#62632,#62633,#62634,#62635,#62636,#62637,#62638,#62639,#62640,#62641,#62642,
#62643,#62644,#62645,#62646,#62647,#62648,#62649,#62650,#62651,#62652,#62653,
#62654,#62655,#62656,#62657,#62658,#62659,#62660,#62661,#62662,#62663,#62664,
#62665,#62666,#62667,#62668,#62669,#62670,#62671,#62672,#62673),(#62674,
#62675,#62676,#62677,#62678,#62679,#62680,#62681,#62682,#62683,#62684,#62685,
#62686,#62687,#62688,#62689,#62690,#62691,#62692,#62693,#62694,#62695,#62696,
#62697,#62698,#62699,#62700,#62701,#62702,#62703,#62704,#62705,#62706,#62707,
#62708,#62709,#62710,#62711,#62712,#62713,#62714,#62715,#62716,#62717,#62718,
#62719,#62720,#62721,#62722,#62723,#62724,#62725,#62726,#62727,#62728,#62729,
#62730,#62731,#62732,#62733,#62734,#62735,#62736,#62737,#62738,#62739,#62740,
#62741,#62742,#62743,#62744,#62745,#62746,#62747,#62748,#62749,#62750,#62751,
#62752,#62753,#62754,#62755,#62756,#62757,#62758,#62759,#62760,#62761,#62762,
#62763,#62764,#62765,#62766,#62767,#62768,#62769,#62770,#62771,#62772,#62773,
#62774,#62775),(#62776,#62777,#62778,#62779,#62780,#62781,#62782,#62783,
#62784,#62785,#62786,#62787,#62788,#62789,#62790,#62791,#62792,#62793,#62794,
#62795,#62796,#62797,#62798,#62799,#62800,#62801,#62802,#62803,#62804,#62805,
#62806,#62807,#62808,#62809,#62810,#62811,#62812,#62813,#62814,#62815,#62816,
#62817,#62818,#62819,#62820,#62821,#62822,#62823,#62824,#62825,#62826,#62827,
#62828,#62829,#62830,#62831,#62832,#62833,#62834,#62835,#62836,#62837,#62838,
#62839,#62840,#62841,#62842,#62843,#62844,#62845,#62846,#62847,#62848,#62849,
#62850,#62851,#62852,#62853,#62854,#62855,#62856,#62857,#62858,#62859,#62860,
#62861,#62862,#62863,#62864,#62865,#62866,#62867,#62868,#62869,#62870,#62871,
#62872,#62873,#62874,#62875,#62876,#62877),(#62878,#62879,#62880,#62881,
#62882,#62883,#62884,#62885,#62886,#62887,#62888,#62889,#62890,#62891,#62892,
#62893,#62894,#62895,#62896,#62897,#62898,#62899,#62900,#62901,#62902,#62903,
#62904,#62905,#62906,#62907,#62908,#62909,#62910,#62911,#62912,#62913,#62914,
#62915,#62916,#62917,#62918,#62919,#62920,#62921,#62922,#62923,#62924,#62925,
#62926,#62927,#62928,#62929,#62930,#62931,#62932,#62933,#62934,#62935,#62936,
#62937,#62938,#62939,#62940,#62941,#62942,#62943,#62944,#62945,#62946,#62947,
#62948,#62949,#62950,#62951,#62952,#62953,#62954,#62955,#62956,#62957,#62958,
#62959,#62960,#62961,#62962,#62963,#62964,#62965,#62966,#62967,#62968,#62969,
#62970,#62971,#62972,#62973,#62974,#62975,#62976,#62977,#62978,#62979)),
 .UNSPECIFIED.,.F.,.F.,.F.,(4,4),(4,1,1,1,1,1,1,1,1,1,1,1,1,1,1,1,1,1,1,
1,1,1,1,1,1,1,1,1,1,1,1,1,1,1,1,1,1,1,1,1,1,1,1,1,1,1,1,1,1,1,1,1,1,1,1,
1,1,1,1,1,1,1,1,1,1,1,1,1,1,1,1,1,1,1,1,1,1,1,1,1,1,1,1,1,1,1,1,1,1,1,1,
1,1,1,1,1,1,1,1,4),(0.,0.0658467982010768),(11.6150328478182,12.6069034617266,
13.598774075635,14.5906446895433,15.5825153034517,16.5743859173601,17.5662565312685,
18.5581271451769,19.5499977590852,20.5418683729936,21.533738986902,22.5256096008104,
23.5174802147187,24.5093508286271,25.5012214425355,26.4930920564439,27.4849626703523,
28.4768332842606,29.468703898169,30.4605745120774,31.4524451259858,32.4443157398941,
33.4361863538025,34.4280569677109,35.4199275816193,36.4117981955277,37.403668809436,
38.3955394233444,39.3874100372528,40.3792806511612,41.3711512650695,42.3630218789779,
43.3548924928863,44.3467631067947,45.3386337207031,46.3305043346114,47.3223749485198,
48.3142455624282,49.3061161763366,50.2979867902449,51.2898574041533,52.2817280180617,
53.2735986319701,54.2654692458785,55.2573398597868,56.2492104736952,57.2410810876036,
58.232951701512,59.2248223154203,60.2166929293287,61.2085635432371,62.2004341571455,
63.1923047710539,64.1841753849622,65.1760459988706,66.167916612779,67.1597872266874,
68.1516578405957,69.1435284545041,70.1353990684125,71.1272696823209,72.1191402962293,
73.1110109101376,74.102881524046,75.0947521379544,76.0866227518628,77.0784933657711,
78.0703639796795,79.0622345935879,80.0541052074963,81.0459758214047,82.037846435313,
83.0297170492214,84.0215876631298,85.0134582770382,86.0053288909465,86.9971995048549,
87.9890701187633,88.9809407326717,89.9728113465801,90.9646819604884,91.9565525743968,
92.9484231883052,93.9402938022136,94.9321644161219,95.9240350300303,96.9159056439387,
97.9077762578471,98.8996468717555,99.8915174856638,100.883388099572,101.875258713481,
102.867129327389,103.858999941297,104.850870555206,105.842741169114,106.834611783022,
107.826482396931,108.818353010839,109.810223624748),.UNSPECIFIED.);
#284=B_SPLINE_SURFACE_WITH_KNOTS('',3,3,((#63108,#63109,#63110,#63111,#63112,
#63113,#63114,#63115,#63116,#63117,#63118,#63119,#63120,#63121,#63122,#63123,
#63124,#63125,#63126,#63127,#63128,#63129,#63130,#63131,#63132,#63133,#63134,
#63135,#63136,#63137,#63138,#63139,#63140,#63141,#63142,#63143,#63144,#63145,
#63146,#63147,#63148,#63149,#63150,#63151,#63152,#63153,#63154,#63155,#63156,
#63157,#63158,#63159,#63160,#63161,#63162,#63163,#63164,#63165,#63166,#63167,
#63168,#63169,#63170,#63171,#63172,#63173,#63174,#63175,#63176,#63177,#63178,
#63179,#63180,#63181,#63182,#63183,#63184,#63185,#63186,#63187,#63188,#63189,
#63190,#63191,#63192,#63193,#63194,#63195,#63196,#63197,#63198,#63199,#63200,
#63201,#63202,#63203,#63204,#63205,#63206,#63207,#63208,#63209,#63210,#63211),
(#63212,#63213,#63214,#63215,#63216,#63217,#63218,#63219,#63220,#63221,
#63222,#63223,#63224,#63225,#63226,#63227,#63228,#63229,#63230,#63231,#63232,
#63233,#63234,#63235,#63236,#63237,#63238,#63239,#63240,#63241,#63242,#63243,
#63244,#63245,#63246,#63247,#63248,#63249,#63250,#63251,#63252,#63253,#63254,
#63255,#63256,#63257,#63258,#63259,#63260,#63261,#63262,#63263,#63264,#63265,
#63266,#63267,#63268,#63269,#63270,#63271,#63272,#63273,#63274,#63275,#63276,
#63277,#63278,#63279,#63280,#63281,#63282,#63283,#63284,#63285,#63286,#63287,
#63288,#63289,#63290,#63291,#63292,#63293,#63294,#63295,#63296,#63297,#63298,
#63299,#63300,#63301,#63302,#63303,#63304,#63305,#63306,#63307,#63308,#63309,
#63310,#63311,#63312,#63313,#63314,#63315),(#63316,#63317,#63318,#63319,
#63320,#63321,#63322,#63323,#63324,#63325,#63326,#63327,#63328,#63329,#63330,
#63331,#63332,#63333,#63334,#63335,#63336,#63337,#63338,#63339,#63340,#63341,
#63342,#63343,#63344,#63345,#63346,#63347,#63348,#63349,#63350,#63351,#63352,
#63353,#63354,#63355,#63356,#63357,#63358,#63359,#63360,#63361,#63362,#63363,
#63364,#63365,#63366,#63367,#63368,#63369,#63370,#63371,#63372,#63373,#63374,
#63375,#63376,#63377,#63378,#63379,#63380,#63381,#63382,#63383,#63384,#63385,
#63386,#63387,#63388,#63389,#63390,#63391,#63392,#63393,#63394,#63395,#63396,
#63397,#63398,#63399,#63400,#63401,#63402,#63403,#63404,#63405,#63406,#63407,
#63408,#63409,#63410,#63411,#63412,#63413,#63414,#63415,#63416,#63417,#63418,
#63419),(#63420,#63421,#63422,#63423,#63424,#63425,#63426,#63427,#63428,
#63429,#63430,#63431,#63432,#63433,#63434,#63435,#63436,#63437,#63438,#63439,
#63440,#63441,#63442,#63443,#63444,#63445,#63446,#63447,#63448,#63449,#63450,
#63451,#63452,#63453,#63454,#63455,#63456,#63457,#63458,#63459,#63460,#63461,
#63462,#63463,#63464,#63465,#63466,#63467,#63468,#63469,#63470,#63471,#63472,
#63473,#63474,#63475,#63476,#63477,#63478,#63479,#63480,#63481,#63482,#63483,
#63484,#63485,#63486,#63487,#63488,#63489,#63490,#63491,#63492,#63493,#63494,
#63495,#63496,#63497,#63498,#63499,#63500,#63501,#63502,#63503,#63504,#63505,
#63506,#63507,#63508,#63509,#63510,#63511,#63512,#63513,#63514,#63515,#63516,
#63517,#63518,#63519,#63520,#63521,#63522,#63523)),.UNSPECIFIED.,.F.,.F.,
 .F.,(4,4),(4,1,1,1,1,1,1,1,1,1,1,1,1,1,1,1,1,1,1,1,1,1,1,1,1,1,1,1,1,1,
1,1,1,1,1,1,1,1,1,1,1,1,1,1,1,1,1,1,1,1,1,1,1,1,1,1,1,1,1,1,1,1,1,1,1,1,
1,1,1,1,1,1,1,1,1,1,1,1,1,1,1,1,1,1,1,1,1,1,1,1,1,1,1,1,1,1,1,1,1,1,1,4),
(0.,0.0658467982010768),(8.30747755240101,9.30018873014199,10.292899907883,
11.2856110856239,12.2783222633649,13.2710334411059,14.2637446188469,15.2564557965878,
16.2491669743288,17.2418781520698,18.2345893298108,19.2273005075518,20.2200116852927,
21.2127228630337,22.2054340407747,23.1981452185157,24.1908563962566,25.1835675739976,
26.1762787517386,27.1689899294796,28.1617011072206,29.1544122849615,30.1471234627025,
31.1398346404435,32.1325458181845,33.1252569959254,34.1179681736664,35.1106793514074,
36.1033905291484,37.0961017068893,38.0888128846303,39.0815240623713,40.0742352401123,
41.0669464178533,42.0596575955942,43.0523687733352,44.0450799510762,45.0377911288172,
46.0305023065581,47.0232134842991,48.0159246620401,49.0086358397811,50.001347017522,
50.994058195263,51.986769373004,52.979480550745,53.972191728486,54.9649029062269,
55.9576140839679,56.9503252617089,57.9430364394499,58.9357476171908,59.9284587949318,
60.9211699726728,61.9138811504138,62.9065923281547,63.8993035058957,64.8920146836367,
65.8847258613777,66.8774370391187,67.8701482168596,68.8628593946006,69.8555705723416,
70.8482817500825,71.8409929278235,72.8337041055645,73.8264152833055,74.8191264610465,
75.8118376387874,76.8045488165284,77.7972599942694,78.7899711720104,79.7826823497514,
80.7753935274923,81.7681047052333,82.7608158829743,83.7535270607153,84.7462382384562,
85.7389494161972,86.7316605939382,87.7243717716792,88.7170829494201,89.7097941271611,
90.7025053049021,91.6952164826431,92.687927660384,93.680638838125,94.673350015866,
95.666061193607,96.658772371348,97.6514835490889,98.6441947268299,99.6369059045709,
100.629617082312,101.622328260053,102.615039437794,103.607750615535,104.600461793276,
105.593172971017,106.585884148758,107.578595326499,108.57130650424),
 .UNSPECIFIED.);
#285=CIRCLE('',#14528,3.5175);
#286=CIRCLE('',#14536,3.5175);
#287=CIRCLE('',#14538,3.5175);
#288=CIRCLE('',#14546,3.5175);
#289=CIRCLE('',#14548,3.5175);
#290=CIRCLE('',#14556,3.5175);
#291=CIRCLE('',#14558,3.5175);
#292=CIRCLE('',#14566,3.5175);
#293=CIRCLE('',#14568,4.0735);
#294=CIRCLE('',#14576,4.07350000000001);
#295=CIRCLE('',#14578,4.0735);
#296=CIRCLE('',#14586,4.07350000000001);
#297=CIRCLE('',#14588,4.0735);
#298=CIRCLE('',#14596,4.0735);
#299=CIRCLE('',#14598,4.0735);
#300=CIRCLE('',#14606,4.0735);
#301=CIRCLE('',#14623,3.942);
#302=CIRCLE('',#14648,3.37175);
#303=CIRCLE('',#14673,3.942);
#304=CIRCLE('',#14674,3.);
#305=CIRCLE('',#14676,3.37175);
#306=CIRCLE('',#14686,6.5);
#307=CIRCLE('',#14688,6.5);
#308=CIRCLE('',#14693,4.5);
#309=CIRCLE('',#14694,4.5);
#310=CIRCLE('',#14696,9.);
#311=CIRCLE('',#14697,9.);
#312=CIRCLE('',#14743,4.51775);
#313=CIRCLE('',#14744,4.51775);
#314=CIRCLE('',#14745,4.51775);
#315=CIRCLE('',#14770,4.51775);
#316=CIRCLE('',#14772,5.0736);
#317=CIRCLE('',#14797,5.0736);
#318=CIRCLE('',#14799,4.51775);
#319=CIRCLE('',#14800,4.51775);
#320=CIRCLE('',#14801,4.51775);
#321=CIRCLE('',#14841,4.51775);
#322=CIRCLE('',#14843,5.07359999999999);
#323=CIRCLE('',#14883,5.0736);
#324=CIRCLE('',#14888,4.);
#325=CIRCLE('',#14893,4.);
#326=CIRCLE('',#14895,1.);
#327=CIRCLE('',#14896,1.);
#328=CIRCLE('',#14899,1.);
#329=CIRCLE('',#14900,1.);
#330=CIRCLE('',#14901,1.);
#331=CIRCLE('',#14902,1.);
#332=CIRCLE('',#14903,1.);
#333=CIRCLE('',#14904,1.);
#334=CIRCLE('',#14905,1.);
#335=CIRCLE('',#14906,1.);
#336=CIRCLE('',#14907,1.);
#337=CIRCLE('',#14908,1.);
#338=CIRCLE('',#14909,1.);
#339=CIRCLE('',#14910,1.);
#340=CIRCLE('',#14911,1.);
#341=CIRCLE('',#14912,1.);
#342=CIRCLE('',#14913,1.);
#343=CIRCLE('',#14914,1.);
#344=CIRCLE('',#14915,1.);
#345=CIRCLE('',#14916,1.);
#346=CIRCLE('',#14917,1.);
#347=CIRCLE('',#14918,1.);
#348=CIRCLE('',#14919,1.);
#349=CIRCLE('',#14920,1.);
#350=CIRCLE('',#14921,1.);
#351=CIRCLE('',#14922,1.);
#352=CIRCLE('',#14923,1.);
#353=CIRCLE('',#14924,1.);
#354=CIRCLE('',#14925,1.);
#355=CIRCLE('',#14926,1.);
#356=CIRCLE('',#14927,1.);
#357=CIRCLE('',#14928,1.);
#358=CIRCLE('',#14929,1.);
#359=CIRCLE('',#14930,1.);
#360=CIRCLE('',#14931,1.);
#361=CIRCLE('',#14932,1.);
#362=CIRCLE('',#14933,1.);
#363=CIRCLE('',#14934,3.);
#364=CIRCLE('',#14935,3.);
#365=CIRCLE('',#14936,3.);
#366=CIRCLE('',#14937,3.);
#367=CIRCLE('',#14939,1.);
#368=CIRCLE('',#14942,1.);
#369=CIRCLE('',#14945,1.);
#370=CIRCLE('',#14948,1.);
#371=CIRCLE('',#14951,1.);
#372=CIRCLE('',#14953,1.);
#373=CIRCLE('',#14956,1.);
#374=CIRCLE('',#14958,1.);
#375=CIRCLE('',#14961,1.);
#376=CIRCLE('',#14963,1.);
#377=CIRCLE('',#14966,1.);
#378=CIRCLE('',#14969,1.);
#379=CIRCLE('',#14972,1.);
#380=CIRCLE('',#14975,1.);
#381=CIRCLE('',#14977,1.);
#382=CIRCLE('',#14980,1.);
#383=CIRCLE('',#14982,1.);
#384=CIRCLE('',#14985,1.);
#385=CIRCLE('',#14987,1.);
#386=CIRCLE('',#14990,1.);
#387=CIRCLE('',#14993,1.);
#388=CIRCLE('',#14996,1.);
#389=CIRCLE('',#14999,1.);
#390=CIRCLE('',#15001,1.);
#391=CIRCLE('',#15004,1.);
#392=CIRCLE('',#15006,1.);
#393=CIRCLE('',#15009,1.);
#394=CIRCLE('',#15011,1.);
#395=CIRCLE('',#15014,1.);
#396=CIRCLE('',#15017,1.);
#397=CIRCLE('',#15020,1.);
#398=CIRCLE('',#15023,1.);
#399=CIRCLE('',#15025,1.);
#400=CIRCLE('',#15028,1.);
#401=CIRCLE('',#15030,1.);
#402=CIRCLE('',#15032,3.);
#403=CIRCLE('',#15034,3.);
#404=CIRCLE('',#15037,3.);
#405=CIRCLE('',#15039,3.);
#406=CIRCLE('',#15055,8.5);
#407=CIRCLE('',#15056,5.5);
#408=CIRCLE('',#15058,8.5);
#409=CIRCLE('',#15060,5.5);
#410=CIRCLE('',#15062,4.5);
#411=CIRCLE('',#15063,4.5);
#412=CIRCLE('',#15065,4.5);
#413=CIRCLE('',#15066,4.5);
#414=CIRCLE('',#15068,4.5);
#415=CIRCLE('',#15069,4.5);
#416=CIRCLE('',#15071,4.5);
#417=CIRCLE('',#15072,4.5);
#418=CIRCLE('',#15081,4.942);
#419=CIRCLE('',#15101,4.372);
#420=CIRCLE('',#15121,4.942);
#421=CIRCLE('',#15122,4.);
#422=CIRCLE('',#15124,4.372);
#423=CIRCLE('',#15134,8.);
#424=CIRCLE('',#15136,8.);
#425=CIRCLE('',#15141,30.);
#426=CIRCLE('',#15142,30.);
#427=CIRCLE('',#15147,2.5175);
#428=CIRCLE('',#15148,2.5175);
#429=CIRCLE('',#15149,2.5175);
#430=CIRCLE('',#15157,2.5175);
#431=CIRCLE('',#15159,3.0735);
#432=CIRCLE('',#15167,3.0735);
#433=CIRCLE('',#15169,2.5175);
#434=CIRCLE('',#15170,2.5175);
#435=CIRCLE('',#15171,2.5175);
#436=CIRCLE('',#15179,2.5175);
#437=CIRCLE('',#15181,3.0735);
#438=CIRCLE('',#15189,3.0735);
#439=CIRCLE('',#15191,2.5175);
#440=CIRCLE('',#15192,2.5175);
#441=CIRCLE('',#15193,2.5175);
#442=CIRCLE('',#15201,2.5175);
#443=CIRCLE('',#15203,3.0735);
#444=CIRCLE('',#15211,3.0735);
#445=CIRCLE('',#15225,5.65685424949238);
#446=CIRCLE('',#15226,6.);
#447=CIRCLE('',#15228,30.);
#448=CIRCLE('',#15229,30.);
#449=CIRCLE('',#15234,3.5);
#450=CIRCLE('',#15235,3.5);
#451=CIRCLE('',#15237,3.5);
#452=CIRCLE('',#15238,3.5);
#453=CIRCLE('',#15240,3.5);
#454=CIRCLE('',#15241,3.5);
#455=CIRCLE('',#15243,5.65685424949238);
#456=CIRCLE('',#15244,6.);
#457=CIRCLE('',#15245,5.5);
#458=CIRCLE('',#15247,5.5);
#459=CIRCLE('',#15249,22.);
#460=CIRCLE('',#15250,22.);
#461=CIRCLE('',#15255,4.942);
#462=CIRCLE('',#15316,4.372);
#463=CIRCLE('',#15377,4.372);
#464=CIRCLE('',#15379,4.942);
#465=CIRCLE('',#15382,5.);
#466=CIRCLE('',#15390,5.);
#467=CIRCLE('',#15393,6.);
#468=CIRCLE('',#15396,4.51775);
#469=CIRCLE('',#15404,4.51775);
#470=CIRCLE('',#15406,5.0736);
#471=CIRCLE('',#15414,5.0736);
#472=CIRCLE('',#15427,5.5);
#473=CIRCLE('',#15428,5.5);
#474=CIRCLE('',#15430,11.);
#475=CIRCLE('',#15431,11.);
#476=CIRCLE('',#15436,2.942);
#477=CIRCLE('',#15452,2.37175);
#478=CIRCLE('',#15468,2.942);
#479=CIRCLE('',#15469,2.);
#480=CIRCLE('',#15471,2.37175);
#481=CIRCLE('',#15481,5.);
#482=CIRCLE('',#15483,5.);
#483=CIRCLE('',#15488,3.5);
#484=CIRCLE('',#15489,3.5);
#485=CIRCLE('',#15491,7.);
#486=CIRCLE('',#15492,7.);
#487=B_SPLINE_CURVE_WITH_KNOTS('',3,(#18487,#18488,#18489,#18490),
 .UNSPECIFIED.,.F.,.F.,(4,4),(51.5750455984138,52.2824273504652),
 .UNSPECIFIED.);
#488=B_SPLINE_CURVE_WITH_KNOTS('',3,(#18493,#18494,#18495,#18496,#18497,
#18498,#18499,#18500,#18501,#18502),.UNSPECIFIED.,.F.,.F.,(4,3,3,4),(-50.2654824574367,
-49.3230446702501,-48.3365837768451,-47.8312715558983),.UNSPECIFIED.);
#489=B_SPLINE_CURVE_WITH_KNOTS('',3,(#18507,#18508,#18509,#18510,#18511,
#18512,#18513,#18514,#18515,#18516,#18517,#18518,#18519,#18520,#18521,#18522,
#18523,#18524,#18525,#18526,#18527,#18528,#18529,#18530,#18531),
 .UNSPECIFIED.,.F.,.F.,(4,3,3,3,3,3,3,3,4),(45.2918602912342,45.3772010966301,
46.3636619900351,47.3501228834401,48.3365837768452,49.3230446702501,50.3095055636552,
51.2959664570602,51.5750455984138),.UNSPECIFIED.);
#490=B_SPLINE_CURVE_WITH_KNOTS('',3,(#18532,#18533,#18534,#18535,#18536,
#18537,#18538,#18539,#18540,#18541,#18542,#18543,#18544,#18545,#18546,#18547,
#18548,#18549,#18550,#18551,#18552,#18553),.UNSPECIFIED.,.F.,.F.,(4,3,3,
3,3,3,3,4),(-47.8312715558983,-47.3501228834401,-46.3636619900351,-45.3772010966301,
-44.3907402032251,-43.4042793098201,-42.4178184164151,-41.5480862487187),
 .UNSPECIFIED.);
#491=B_SPLINE_CURVE_WITH_KNOTS('',3,(#18558,#18559,#18560,#18561,#18562,
#18563,#18564,#18565,#18566,#18567,#18568,#18569,#18570,#18571,#18572,#18573,
#18574,#18575,#18576,#18577,#18578,#18579),.UNSPECIFIED.,.F.,.F.,(4,3,3,
3,3,3,3,4),(39.0086749840546,39.4584357362001,40.4448966296051,41.4313575230101,
42.4178184164151,43.4042793098201,44.3907402032251,45.2918602912342),
 .UNSPECIFIED.);
#492=B_SPLINE_CURVE_WITH_KNOTS('',3,(#18580,#18581,#18582,#18583,#18584,
#18585,#18586,#18587,#18588,#18589,#18590,#18591,#18592,#18593,#18594,#18595,
#18596,#18597,#18598,#18599,#18600,#18601,#18602,#18603,#18604),
 .UNSPECIFIED.,.F.,.F.,(4,3,3,3,3,3,3,3,4),(-41.5480862487187,-41.4313575230101,
-40.4448966296051,-39.4584357362001,-38.4719748427951,-37.4855139493901,
-36.4990530559851,-35.5125921625801,-35.2649009415391),.UNSPECIFIED.);
#493=B_SPLINE_CURVE_WITH_KNOTS('',3,(#18609,#18610,#18611,#18612,#18613,
#18614,#18615,#18616,#18617,#18618,#18619,#18620,#18621,#18622,#18623,#18624,
#18625,#18626,#18627,#18628,#18629,#18630),.UNSPECIFIED.,.F.,.F.,(4,3,3,
3,3,3,3,4),(32.725489676875,33.5396703757701,34.5261312691751,35.5125921625801,
36.4990530559851,37.4855139493901,38.4719748427951,39.0086749840546),
 .UNSPECIFIED.);
#494=B_SPLINE_CURVE_WITH_KNOTS('',3,(#18631,#18632,#18633,#18634,#18635,
#18636,#18637,#18638,#18639,#18640,#18641,#18642,#18643,#18644,#18645,#18646,
#18647,#18648,#18649,#18650,#18651,#18652),.UNSPECIFIED.,.F.,.F.,(4,3,3,
3,3,3,3,4),(-35.2649009415391,-34.5261312691751,-33.5396703757701,-32.5532094823651,
-31.5667485889601,-30.5802876955551,-29.5938268021501,-28.9817156343595),
 .UNSPECIFIED.);
#495=B_SPLINE_CURVE_WITH_KNOTS('',3,(#18657,#18658,#18659,#18660,#18661,
#18662,#18663,#18664,#18665,#18666,#18667,#18668,#18669,#18670,#18671,#18672,
#18673,#18674,#18675,#18676,#18677,#18678,#18679,#18680,#18681),
 .UNSPECIFIED.,.F.,.F.,(4,3,3,3,3,3,3,3,4),(26.4423043696954,26.6344441219351,
27.6209050153401,28.6073659087451,29.5938268021501,30.5802876955551,31.5667485889601,
32.5532094823651,32.725489676875),.UNSPECIFIED.);
#496=B_SPLINE_CURVE_WITH_KNOTS('',3,(#18682,#18683,#18684,#18685,#18686,
#18687,#18688,#18689,#18690,#18691,#18692,#18693,#18694,#18695,#18696,#18697,
#18698,#18699,#18700,#18701,#18702,#18703),.UNSPECIFIED.,.F.,.F.,(4,3,3,
3,3,3,3,4),(-28.9817156343595,-28.6073659087451,-27.6209050153401,-26.6344441219351,
-25.6479832285301,-24.6615223351251,-23.6750614417201,-22.6985303271799),
 .UNSPECIFIED.);
#497=B_SPLINE_CURVE_WITH_KNOTS('',3,(#18708,#18709,#18710,#18711,#18712,
#18713,#18714,#18715,#18716,#18717,#18718,#18719,#18720,#18721,#18722,#18723,
#18724,#18725,#18726,#18727,#18728,#18729),.UNSPECIFIED.,.F.,.F.,(4,3,3,
3,3,3,3,4),(20.1591190625159,20.7156787615051,21.7021396549101,22.6886005483151,
23.6750614417201,24.6615223351251,25.6479832285301,26.4423043696954),
 .UNSPECIFIED.);
#498=B_SPLINE_CURVE_WITH_KNOTS('',3,(#18730,#18731,#18732,#18733,#18734,
#18735,#18736,#18737,#18738,#18739,#18740,#18741,#18742,#18743,#18744,#18745,
#18746,#18747,#18748,#18749,#18750,#18751,#18752,#18753,#18754),
 .UNSPECIFIED.,.F.,.F.,(4,3,3,3,3,3,3,3,4),(-22.6985303271799,-22.6886005483151,
-21.7021396549101,-20.7156787615051,-19.7292178681001,-18.7427569746951,
-17.7562960812901,-16.7698351878851,-16.4153450200003),.UNSPECIFIED.);
#499=B_SPLINE_CURVE_WITH_KNOTS('',3,(#18759,#18760,#18761,#18762,#18763,
#18764,#18765,#18766,#18767,#18768,#18769,#18770,#18771,#18772,#18773,#18774,
#18775,#18776,#18777,#18778,#18779,#18780),.UNSPECIFIED.,.F.,.F.,(4,3,3,
3,3,3,3,4),(13.8759337553363,14.7969134010751,15.78337429448,16.7698351878851,
17.75629608129,18.7427569746951,19.7292178681001,20.1591190625159),
 .UNSPECIFIED.);
#500=B_SPLINE_CURVE_WITH_KNOTS('',3,(#18781,#18782,#18783,#18784,#18785,
#18786,#18787,#18788,#18789,#18790,#18791,#18792,#18793,#18794,#18795,#18796,
#18797,#18798,#18799,#18800,#18801,#18802),.UNSPECIFIED.,.F.,.F.,(4,3,3,
3,3,3,3,4),(-16.4153450200003,-15.78337429448,-14.796913401075,-13.81045250767,
-12.823991614265,-11.83753072086,-10.851069827455,-10.1321597128207),
 .UNSPECIFIED.);
#501=B_SPLINE_CURVE_WITH_KNOTS('',3,(#18808,#18809,#18810,#18811,#18812,
#18813,#18814,#18815,#18816,#18817,#18818,#18819,#18820),.UNSPECIFIED.,
 .F.,.F.,(4,3,3,3,4),(-3.84897440564115,-2.95938268021501,-1.97292178681001,
-0.986460893405001,0.),.UNSPECIFIED.);
#502=B_SPLINE_CURVE_WITH_KNOTS('',3,(#18823,#18824,#18825,#18826,#18827,
#18828,#18829,#18830,#18831,#18832,#18833,#18834,#18835,#18836,#18837,#18838,
#18839,#18840,#18841),.UNSPECIFIED.,.F.,.F.,(4,3,3,3,3,3,4),(2.01694489302848,
2.95938268021501,3.94584357362001,4.93230446702502,5.91876536043002,6.90522625383502,
7.59274844815668),.UNSPECIFIED.);
#503=B_SPLINE_CURVE_WITH_KNOTS('',3,(#18847,#18848,#18849,#18850),
 .UNSPECIFIED.,.F.,.F.,(4,4),(51.5750455984138,52.2824273504652),
 .UNSPECIFIED.);
#504=B_SPLINE_CURVE_WITH_KNOTS('',3,(#18853,#18854,#18855,#18856,#18857,
#18858,#18859,#18860,#18861,#18862),.UNSPECIFIED.,.F.,.F.,(4,3,3,4),(-50.2654824574367,
-49.3230446702501,-48.3365837768451,-47.8312715558982),.UNSPECIFIED.);
#505=B_SPLINE_CURVE_WITH_KNOTS('',3,(#18867,#18868,#18869,#18870,#18871,
#18872,#18873,#18874,#18875,#18876,#18877,#18878,#18879,#18880,#18881,#18882,
#18883,#18884,#18885,#18886,#18887,#18888,#18889,#18890,#18891),
 .UNSPECIFIED.,.F.,.F.,(4,3,3,3,3,3,3,3,4),(45.2918602912342,45.3772010966301,
46.3636619900351,47.3501228834401,48.3365837768451,49.3230446702501,50.3095055636551,
51.2959664570602,51.5750455984138),.UNSPECIFIED.);
#506=B_SPLINE_CURVE_WITH_KNOTS('',3,(#18892,#18893,#18894,#18895,#18896,
#18897,#18898,#18899,#18900,#18901,#18902,#18903,#18904,#18905,#18906,#18907,
#18908,#18909,#18910,#18911,#18912,#18913),.UNSPECIFIED.,.F.,.F.,(4,3,3,
3,3,3,3,4),(-47.8312715558982,-47.3501228834401,-46.3636619900351,-45.3772010966301,
-44.3907402032251,-43.4042793098201,-42.4178184164151,-41.5480862487187),
 .UNSPECIFIED.);
#507=B_SPLINE_CURVE_WITH_KNOTS('',3,(#18918,#18919,#18920,#18921,#18922,
#18923,#18924,#18925,#18926,#18927,#18928,#18929,#18930,#18931,#18932,#18933,
#18934,#18935,#18936,#18937,#18938,#18939),.UNSPECIFIED.,.F.,.F.,(4,3,3,
3,3,3,3,4),(39.0086749840546,39.4584357362001,40.4448966296051,41.4313575230101,
42.4178184164151,43.4042793098201,44.3907402032251,45.2918602912342),
 .UNSPECIFIED.);
#508=B_SPLINE_CURVE_WITH_KNOTS('',3,(#18940,#18941,#18942,#18943,#18944,
#18945,#18946,#18947,#18948,#18949,#18950,#18951,#18952,#18953,#18954,#18955,
#18956,#18957,#18958,#18959,#18960,#18961,#18962,#18963,#18964),
 .UNSPECIFIED.,.F.,.F.,(4,3,3,3,3,3,3,3,4),(-41.5480862487187,-41.4313575230101,
-40.4448966296051,-39.4584357362001,-38.4719748427951,-37.4855139493901,
-36.4990530559851,-35.5125921625801,-35.2649009415391),.UNSPECIFIED.);
#509=B_SPLINE_CURVE_WITH_KNOTS('',3,(#18969,#18970,#18971,#18972,#18973,
#18974,#18975,#18976,#18977,#18978,#18979,#18980,#18981,#18982,#18983,#18984,
#18985,#18986,#18987,#18988,#18989,#18990),.UNSPECIFIED.,.F.,.F.,(4,3,3,
3,3,3,3,4),(32.725489676875,33.5396703757701,34.5261312691751,35.5125921625801,
36.4990530559851,37.4855139493901,38.4719748427951,39.0086749840546),
 .UNSPECIFIED.);
#510=B_SPLINE_CURVE_WITH_KNOTS('',3,(#18991,#18992,#18993,#18994,#18995,
#18996,#18997,#18998,#18999,#19000,#19001,#19002,#19003,#19004,#19005,#19006,
#19007,#19008,#19009,#19010,#19011,#19012),.UNSPECIFIED.,.F.,.F.,(4,3,3,
3,3,3,3,4),(-35.2649009415391,-34.5261312691751,-33.5396703757701,-32.5532094823651,
-31.5667485889601,-30.5802876955551,-29.5938268021501,-28.9817156343595),
 .UNSPECIFIED.);
#511=B_SPLINE_CURVE_WITH_KNOTS('',3,(#19017,#19018,#19019,#19020,#19021,
#19022,#19023,#19024,#19025,#19026,#19027,#19028,#19029,#19030,#19031,#19032,
#19033,#19034,#19035,#19036,#19037,#19038,#19039,#19040,#19041),
 .UNSPECIFIED.,.F.,.F.,(4,3,3,3,3,3,3,3,4),(26.4423043696954,26.6344441219351,
27.6209050153401,28.6073659087451,29.5938268021501,30.5802876955551,31.5667485889601,
32.5532094823651,32.725489676875),.UNSPECIFIED.);
#512=B_SPLINE_CURVE_WITH_KNOTS('',3,(#19042,#19043,#19044,#19045,#19046,
#19047,#19048,#19049,#19050,#19051,#19052,#19053,#19054,#19055,#19056,#19057,
#19058,#19059,#19060,#19061,#19062,#19063),.UNSPECIFIED.,.F.,.F.,(4,3,3,
3,3,3,3,4),(-28.9817156343595,-28.6073659087451,-27.6209050153401,-26.6344441219351,
-25.6479832285301,-24.6615223351251,-23.6750614417201,-22.6985303271799),
 .UNSPECIFIED.);
#513=B_SPLINE_CURVE_WITH_KNOTS('',3,(#19068,#19069,#19070,#19071,#19072,
#19073,#19074,#19075,#19076,#19077,#19078,#19079,#19080,#19081,#19082,#19083,
#19084,#19085,#19086,#19087,#19088,#19089),.UNSPECIFIED.,.F.,.F.,(4,3,3,
3,3,3,3,4),(20.1591190625158,20.7156787615051,21.7021396549101,22.6886005483151,
23.6750614417201,24.6615223351251,25.6479832285301,26.4423043696954),
 .UNSPECIFIED.);
#514=B_SPLINE_CURVE_WITH_KNOTS('',3,(#19090,#19091,#19092,#19093,#19094,
#19095,#19096,#19097,#19098,#19099,#19100,#19101,#19102,#19103,#19104,#19105,
#19106,#19107,#19108,#19109,#19110,#19111,#19112,#19113,#19114),
 .UNSPECIFIED.,.F.,.F.,(4,3,3,3,3,3,3,3,4),(-22.6985303271799,-22.6886005483151,
-21.7021396549101,-20.7156787615051,-19.7292178681001,-18.7427569746951,
-17.7562960812901,-16.7698351878851,-16.4153450200003),.UNSPECIFIED.);
#515=B_SPLINE_CURVE_WITH_KNOTS('',3,(#19119,#19120,#19121,#19122,#19123,
#19124,#19125,#19126,#19127,#19128,#19129,#19130,#19131,#19132,#19133,#19134,
#19135,#19136,#19137,#19138,#19139,#19140),.UNSPECIFIED.,.F.,.F.,(4,3,3,
3,3,3,3,4),(13.8759337553363,14.796913401075,15.78337429448,16.7698351878851,
17.7562960812901,18.7427569746951,19.7292178681001,20.1591190625158),
 .UNSPECIFIED.);
#516=B_SPLINE_CURVE_WITH_KNOTS('',3,(#19141,#19142,#19143,#19144,#19145,
#19146,#19147,#19148,#19149,#19150,#19151,#19152,#19153,#19154,#19155,#19156,
#19157,#19158,#19159,#19160,#19161,#19162),.UNSPECIFIED.,.F.,.F.,(4,3,3,
3,3,3,3,4),(-16.4153450200003,-15.7833742944801,-14.796913401075,-13.81045250767,
-12.823991614265,-11.83753072086,-10.851069827455,-10.1321597128207),
 .UNSPECIFIED.);
#517=B_SPLINE_CURVE_WITH_KNOTS('',3,(#19168,#19169,#19170,#19171,#19172,
#19173,#19174,#19175,#19176,#19177,#19178,#19179,#19180),.UNSPECIFIED.,
 .F.,.F.,(4,3,3,3,4),(-3.84897440564114,-2.95938268021501,-1.97292178681001,
-0.986460893405001,0.),.UNSPECIFIED.);
#518=B_SPLINE_CURVE_WITH_KNOTS('',3,(#19183,#19184,#19185,#19186,#19187,
#19188,#19189,#19190,#19191,#19192,#19193,#19194,#19195,#19196,#19197,#19198,
#19199,#19200,#19201),.UNSPECIFIED.,.F.,.F.,(4,3,3,3,3,3,4),(2.01694489302845,
2.95938268021501,3.94584357362001,4.93230446702501,5.91876536043001,6.90522625383501,
7.59274844815667),.UNSPECIFIED.);
#519=B_SPLINE_CURVE_WITH_KNOTS('',3,(#19207,#19208,#19209,#19210),
 .UNSPECIFIED.,.F.,.F.,(4,4),(51.5750455984138,52.2824273504652),
 .UNSPECIFIED.);
#520=B_SPLINE_CURVE_WITH_KNOTS('',3,(#19213,#19214,#19215,#19216,#19217,
#19218,#19219,#19220,#19221,#19222),.UNSPECIFIED.,.F.,.F.,(4,3,3,4),(-50.2654824574367,
-49.3230446702501,-48.3365837768451,-47.8312715558982),.UNSPECIFIED.);
#521=B_SPLINE_CURVE_WITH_KNOTS('',3,(#19227,#19228,#19229,#19230,#19231,
#19232,#19233,#19234,#19235,#19236,#19237,#19238,#19239,#19240,#19241,#19242,
#19243,#19244,#19245,#19246,#19247,#19248,#19249,#19250,#19251),
 .UNSPECIFIED.,.F.,.F.,(4,3,3,3,3,3,3,3,4),(45.2918602912342,45.3772010966301,
46.3636619900351,47.3501228834401,48.3365837768451,49.3230446702501,50.3095055636552,
51.2959664570602,51.5750455984138),.UNSPECIFIED.);
#522=B_SPLINE_CURVE_WITH_KNOTS('',3,(#19252,#19253,#19254,#19255,#19256,
#19257,#19258,#19259,#19260,#19261,#19262,#19263,#19264,#19265,#19266,#19267,
#19268,#19269,#19270,#19271,#19272,#19273),.UNSPECIFIED.,.F.,.F.,(4,3,3,
3,3,3,3,4),(-47.8312715558982,-47.3501228834401,-46.3636619900351,-45.3772010966301,
-44.3907402032251,-43.4042793098201,-42.4178184164151,-41.5480862487187),
 .UNSPECIFIED.);
#523=B_SPLINE_CURVE_WITH_KNOTS('',3,(#19278,#19279,#19280,#19281,#19282,
#19283,#19284,#19285,#19286,#19287,#19288,#19289,#19290,#19291,#19292,#19293,
#19294,#19295,#19296,#19297,#19298,#19299),.UNSPECIFIED.,.F.,.F.,(4,3,3,
3,3,3,3,4),(39.0086749840546,39.4584357362001,40.4448966296051,41.4313575230101,
42.4178184164151,43.4042793098201,44.3907402032251,45.2918602912342),
 .UNSPECIFIED.);
#524=B_SPLINE_CURVE_WITH_KNOTS('',3,(#19300,#19301,#19302,#19303,#19304,
#19305,#19306,#19307,#19308,#19309,#19310,#19311,#19312,#19313,#19314,#19315,
#19316,#19317,#19318,#19319,#19320,#19321,#19322,#19323,#19324),
 .UNSPECIFIED.,.F.,.F.,(4,3,3,3,3,3,3,3,4),(-41.5480862487187,-41.4313575230101,
-40.4448966296051,-39.4584357362001,-38.4719748427951,-37.4855139493901,
-36.4990530559851,-35.5125921625801,-35.2649009415391),.UNSPECIFIED.);
#525=B_SPLINE_CURVE_WITH_KNOTS('',3,(#19329,#19330,#19331,#19332,#19333,
#19334,#19335,#19336,#19337,#19338,#19339,#19340,#19341,#19342,#19343,#19344,
#19345,#19346,#19347,#19348,#19349,#19350),.UNSPECIFIED.,.F.,.F.,(4,3,3,
3,3,3,3,4),(32.725489676875,33.5396703757701,34.5261312691751,35.5125921625801,
36.4990530559851,37.4855139493901,38.4719748427951,39.0086749840546),
 .UNSPECIFIED.);
#526=B_SPLINE_CURVE_WITH_KNOTS('',3,(#19351,#19352,#19353,#19354,#19355,
#19356,#19357,#19358,#19359,#19360,#19361,#19362,#19363,#19364,#19365,#19366,
#19367,#19368,#19369,#19370,#19371,#19372),.UNSPECIFIED.,.F.,.F.,(4,3,3,
3,3,3,3,4),(-35.2649009415391,-34.5261312691751,-33.5396703757701,-32.5532094823651,
-31.5667485889601,-30.5802876955551,-29.5938268021501,-28.9817156343595),
 .UNSPECIFIED.);
#527=B_SPLINE_CURVE_WITH_KNOTS('',3,(#19377,#19378,#19379,#19380,#19381,
#19382,#19383,#19384,#19385,#19386,#19387,#19388,#19389,#19390,#19391,#19392,
#19393,#19394,#19395,#19396,#19397,#19398,#19399,#19400,#19401),
 .UNSPECIFIED.,.F.,.F.,(4,3,3,3,3,3,3,3,4),(26.4423043696954,26.6344441219351,
27.6209050153401,28.6073659087451,29.5938268021501,30.5802876955551,31.5667485889601,
32.5532094823651,32.725489676875),.UNSPECIFIED.);
#528=B_SPLINE_CURVE_WITH_KNOTS('',3,(#19402,#19403,#19404,#19405,#19406,
#19407,#19408,#19409,#19410,#19411,#19412,#19413,#19414,#19415,#19416,#19417,
#19418,#19419,#19420,#19421,#19422,#19423),.UNSPECIFIED.,.F.,.F.,(4,3,3,
3,3,3,3,4),(-28.9817156343595,-28.6073659087451,-27.6209050153401,-26.6344441219351,
-25.6479832285301,-24.6615223351251,-23.6750614417201,-22.6985303271799),
 .UNSPECIFIED.);
#529=B_SPLINE_CURVE_WITH_KNOTS('',3,(#19428,#19429,#19430,#19431,#19432,
#19433,#19434,#19435,#19436,#19437,#19438,#19439,#19440,#19441,#19442,#19443,
#19444,#19445,#19446,#19447,#19448,#19449),.UNSPECIFIED.,.F.,.F.,(4,3,3,
3,3,3,3,4),(20.1591190625158,20.7156787615051,21.7021396549101,22.6886005483151,
23.6750614417201,24.6615223351251,25.6479832285301,26.4423043696954),
 .UNSPECIFIED.);
#530=B_SPLINE_CURVE_WITH_KNOTS('',3,(#19450,#19451,#19452,#19453,#19454,
#19455,#19456,#19457,#19458,#19459,#19460,#19461,#19462,#19463,#19464,#19465,
#19466,#19467,#19468,#19469,#19470,#19471,#19472,#19473,#19474),
 .UNSPECIFIED.,.F.,.F.,(4,3,3,3,3,3,3,3,4),(-22.6985303271799,-22.6886005483151,
-21.7021396549101,-20.715678761505,-19.7292178681001,-18.742756974695,-17.75629608129,
-16.769835187885,-16.4153450200003),.UNSPECIFIED.);
#531=B_SPLINE_CURVE_WITH_KNOTS('',3,(#19479,#19480,#19481,#19482,#19483,
#19484,#19485,#19486,#19487,#19488,#19489,#19490,#19491,#19492,#19493,#19494,
#19495,#19496,#19497,#19498,#19499,#19500),.UNSPECIFIED.,.F.,.F.,(4,3,3,
3,3,3,3,4),(13.8759337553363,14.796913401075,15.78337429448,16.7698351878851,
17.7562960812901,18.7427569746951,19.7292178681001,20.1591190625158),
 .UNSPECIFIED.);
#532=B_SPLINE_CURVE_WITH_KNOTS('',3,(#19501,#19502,#19503,#19504,#19505,
#19506,#19507,#19508,#19509,#19510,#19511,#19512,#19513,#19514,#19515,#19516,
#19517,#19518,#19519,#19520,#19521,#19522),.UNSPECIFIED.,.F.,.F.,(4,3,3,
3,3,3,3,4),(-16.4153450200003,-15.78337429448,-14.796913401075,-13.81045250767,
-12.823991614265,-11.83753072086,-10.851069827455,-10.1321597128207),
 .UNSPECIFIED.);
#533=B_SPLINE_CURVE_WITH_KNOTS('',3,(#19528,#19529,#19530,#19531,#19532,
#19533,#19534,#19535,#19536,#19537,#19538,#19539,#19540),.UNSPECIFIED.,
 .F.,.F.,(4,3,3,3,4),(-3.84897440564114,-2.95938268021501,-1.97292178681001,
-0.986460893405004,0.),.UNSPECIFIED.);
#534=B_SPLINE_CURVE_WITH_KNOTS('',3,(#19543,#19544,#19545,#19546,#19547,
#19548,#19549,#19550,#19551,#19552,#19553,#19554,#19555,#19556,#19557,#19558,
#19559,#19560,#19561),.UNSPECIFIED.,.F.,.F.,(4,3,3,3,3,3,4),(2.01694489302844,
2.95938268021501,3.94584357362001,4.93230446702501,5.91876536043001,6.90522625383502,
7.59274844815667),.UNSPECIFIED.);
#535=B_SPLINE_CURVE_WITH_KNOTS('',3,(#19567,#19568,#19569,#19570),
 .UNSPECIFIED.,.F.,.F.,(4,4),(51.5750455984138,52.2824273504652),
 .UNSPECIFIED.);
#536=B_SPLINE_CURVE_WITH_KNOTS('',3,(#19573,#19574,#19575,#19576,#19577,
#19578,#19579,#19580,#19581,#19582),.UNSPECIFIED.,.F.,.F.,(4,3,3,4),(-50.2654824574367,
-49.3230446702501,-48.3365837768451,-47.8312715558983),.UNSPECIFIED.);
#537=B_SPLINE_CURVE_WITH_KNOTS('',3,(#19587,#19588,#19589,#19590,#19591,
#19592,#19593,#19594,#19595,#19596,#19597,#19598,#19599,#19600,#19601,#19602,
#19603,#19604,#19605,#19606,#19607,#19608,#19609,#19610,#19611),
 .UNSPECIFIED.,.F.,.F.,(4,3,3,3,3,3,3,3,4),(45.2918602912342,45.3772010966301,
46.3636619900351,47.3501228834401,48.3365837768452,49.3230446702501,50.3095055636552,
51.2959664570602,51.5750455984138),.UNSPECIFIED.);
#538=B_SPLINE_CURVE_WITH_KNOTS('',3,(#19612,#19613,#19614,#19615,#19616,
#19617,#19618,#19619,#19620,#19621,#19622,#19623,#19624,#19625,#19626,#19627,
#19628,#19629,#19630,#19631,#19632,#19633),.UNSPECIFIED.,.F.,.F.,(4,3,3,
3,3,3,3,4),(-47.8312715558983,-47.3501228834401,-46.3636619900351,-45.3772010966301,
-44.3907402032251,-43.4042793098201,-42.4178184164151,-41.5480862487187),
 .UNSPECIFIED.);
#539=B_SPLINE_CURVE_WITH_KNOTS('',3,(#19638,#19639,#19640,#19641,#19642,
#19643,#19644,#19645,#19646,#19647,#19648,#19649,#19650,#19651,#19652,#19653,
#19654,#19655,#19656,#19657,#19658,#19659),.UNSPECIFIED.,.F.,.F.,(4,3,3,
3,3,3,3,4),(39.0086749840546,39.4584357362001,40.4448966296051,41.4313575230101,
42.4178184164151,43.4042793098201,44.3907402032251,45.2918602912342),
 .UNSPECIFIED.);
#540=B_SPLINE_CURVE_WITH_KNOTS('',3,(#19660,#19661,#19662,#19663,#19664,
#19665,#19666,#19667,#19668,#19669,#19670,#19671,#19672,#19673,#19674,#19675,
#19676,#19677,#19678,#19679,#19680,#19681,#19682,#19683,#19684),
 .UNSPECIFIED.,.F.,.F.,(4,3,3,3,3,3,3,3,4),(-41.5480862487187,-41.4313575230101,
-40.4448966296051,-39.4584357362001,-38.4719748427951,-37.4855139493901,
-36.4990530559851,-35.5125921625801,-35.2649009415391),.UNSPECIFIED.);
#541=B_SPLINE_CURVE_WITH_KNOTS('',3,(#19689,#19690,#19691,#19692,#19693,
#19694,#19695,#19696,#19697,#19698,#19699,#19700,#19701,#19702,#19703,#19704,
#19705,#19706,#19707,#19708,#19709,#19710),.UNSPECIFIED.,.F.,.F.,(4,3,3,
3,3,3,3,4),(32.725489676875,33.5396703757701,34.5261312691751,35.5125921625801,
36.4990530559851,37.4855139493901,38.4719748427951,39.0086749840546),
 .UNSPECIFIED.);
#542=B_SPLINE_CURVE_WITH_KNOTS('',3,(#19711,#19712,#19713,#19714,#19715,
#19716,#19717,#19718,#19719,#19720,#19721,#19722,#19723,#19724,#19725,#19726,
#19727,#19728,#19729,#19730,#19731,#19732),.UNSPECIFIED.,.F.,.F.,(4,3,3,
3,3,3,3,4),(-35.2649009415391,-34.5261312691751,-33.5396703757701,-32.5532094823651,
-31.5667485889601,-30.5802876955551,-29.5938268021501,-28.9817156343595),
 .UNSPECIFIED.);
#543=B_SPLINE_CURVE_WITH_KNOTS('',3,(#19737,#19738,#19739,#19740,#19741,
#19742,#19743,#19744,#19745,#19746,#19747,#19748,#19749,#19750,#19751,#19752,
#19753,#19754,#19755,#19756,#19757,#19758,#19759,#19760,#19761),
 .UNSPECIFIED.,.F.,.F.,(4,3,3,3,3,3,3,3,4),(26.4423043696954,26.6344441219351,
27.6209050153401,28.6073659087451,29.5938268021501,30.5802876955551,31.5667485889601,
32.5532094823651,32.725489676875),.UNSPECIFIED.);
#544=B_SPLINE_CURVE_WITH_KNOTS('',3,(#19762,#19763,#19764,#19765,#19766,
#19767,#19768,#19769,#19770,#19771,#19772,#19773,#19774,#19775,#19776,#19777,
#19778,#19779,#19780,#19781,#19782,#19783),.UNSPECIFIED.,.F.,.F.,(4,3,3,
3,3,3,3,4),(-28.9817156343595,-28.6073659087451,-27.6209050153401,-26.6344441219351,
-25.6479832285301,-24.6615223351251,-23.6750614417201,-22.6985303271799),
 .UNSPECIFIED.);
#545=B_SPLINE_CURVE_WITH_KNOTS('',3,(#19788,#19789,#19790,#19791,#19792,
#19793,#19794,#19795,#19796,#19797,#19798,#19799,#19800,#19801,#19802,#19803,
#19804,#19805,#19806,#19807,#19808,#19809),.UNSPECIFIED.,.F.,.F.,(4,3,3,
3,3,3,3,4),(20.1591190625159,20.7156787615051,21.7021396549101,22.6886005483151,
23.6750614417201,24.6615223351251,25.6479832285301,26.4423043696954),
 .UNSPECIFIED.);
#546=B_SPLINE_CURVE_WITH_KNOTS('',3,(#19810,#19811,#19812,#19813,#19814,
#19815,#19816,#19817,#19818,#19819,#19820,#19821,#19822,#19823,#19824,#19825,
#19826,#19827,#19828,#19829,#19830,#19831,#19832,#19833,#19834),
 .UNSPECIFIED.,.F.,.F.,(4,3,3,3,3,3,3,3,4),(-22.6985303271799,-22.6886005483151,
-21.7021396549101,-20.7156787615051,-19.7292178681001,-18.7427569746951,
-17.7562960812901,-16.7698351878851,-16.4153450200003),.UNSPECIFIED.);
#547=B_SPLINE_CURVE_WITH_KNOTS('',3,(#19839,#19840,#19841,#19842,#19843,
#19844,#19845,#19846,#19847,#19848,#19849,#19850,#19851,#19852,#19853,#19854,
#19855,#19856,#19857,#19858,#19859,#19860),.UNSPECIFIED.,.F.,.F.,(4,3,3,
3,3,3,3,4),(13.8759337553363,14.7969134010751,15.78337429448,16.7698351878851,
17.75629608129,18.7427569746951,19.7292178681001,20.1591190625159),
 .UNSPECIFIED.);
#548=B_SPLINE_CURVE_WITH_KNOTS('',3,(#19861,#19862,#19863,#19864,#19865,
#19866,#19867,#19868,#19869,#19870,#19871,#19872,#19873,#19874,#19875,#19876,
#19877,#19878,#19879,#19880,#19881,#19882),.UNSPECIFIED.,.F.,.F.,(4,3,3,
3,3,3,3,4),(-16.4153450200003,-15.78337429448,-14.796913401075,-13.81045250767,
-12.823991614265,-11.83753072086,-10.851069827455,-10.1321597128207),
 .UNSPECIFIED.);
#549=B_SPLINE_CURVE_WITH_KNOTS('',3,(#19888,#19889,#19890,#19891,#19892,
#19893,#19894,#19895,#19896,#19897,#19898,#19899,#19900),.UNSPECIFIED.,
 .F.,.F.,(4,3,3,3,4),(-3.84897440564115,-2.95938268021501,-1.97292178681001,
-0.986460893405001,0.),.UNSPECIFIED.);
#550=B_SPLINE_CURVE_WITH_KNOTS('',3,(#19903,#19904,#19905,#19906,#19907,
#19908,#19909,#19910,#19911,#19912,#19913,#19914,#19915,#19916,#19917,#19918,
#19919,#19920,#19921),.UNSPECIFIED.,.F.,.F.,(4,3,3,3,3,3,4),(2.01694489302845,
2.95938268021501,3.94584357362001,4.93230446702501,5.91876536043001,6.90522625383502,
7.59274844815668),.UNSPECIFIED.);
#551=B_SPLINE_CURVE_WITH_KNOTS('',3,(#19927,#19928,#19929,#19930,#19931,
#19932,#19933,#19934),.UNSPECIFIED.,.F.,.F.,(4,1,1,1,1,4),(59.6902604182061,
60.1955726391529,61.1820335325579,62.1684944259629,63.154955319368,64.141416212773),
 .UNSPECIFIED.);
#552=B_SPLINE_CURVE_WITH_KNOTS('',3,(#19937,#19938,#19939,#19940,#19941,
#19942,#19943,#19944,#19945),.UNSPECIFIED.,.F.,.F.,(4,1,1,1,1,1,4),(59.6902604182061,
59.775601223602,60.762062117007,61.748523010412,62.734983903817,63.721444797222,
64.6638825844085),.UNSPECIFIED.);
#553=B_SPLINE_CURVE_WITH_KNOTS('',3,(#19950,#19951,#19952,#19953,#19954,
#19955,#19956,#19957,#19958,#19959),.UNSPECIFIED.,.F.,.F.,(4,1,1,1,1,1,
1,4),(53.4070751110265,54.2768072787229,55.2632681721279,56.2497290655329,
57.2361899589379,58.2226508523429,59.2091117457479,59.6902604182061),
 .UNSPECIFIED.);
#554=B_SPLINE_CURVE_WITH_KNOTS('',3,(#19960,#19961,#19962,#19963,#19964,
#19965,#19966,#19967,#19968,#19969),.UNSPECIFIED.,.F.,.F.,(4,1,1,1,1,1,
1,4),(53.4070751110265,53.856835863172,54.843296756577,55.829757649982,
56.816218543387,57.802679436792,58.789140330197,59.6902604182061),
 .UNSPECIFIED.);
#555=B_SPLINE_CURVE_WITH_KNOTS('',3,(#19974,#19975,#19976,#19977,#19978,
#19979,#19980,#19981,#19982,#19983,#19984),.UNSPECIFIED.,.F.,.F.,(4,1,1,
1,1,1,1,1,4),(47.1238898038469,47.3715810248879,48.3580419182929,49.3445028116979,
50.3309637051029,51.3174245985079,52.3038854919129,53.2903463853179,53.4070751110265),
 .UNSPECIFIED.);
#556=B_SPLINE_CURVE_WITH_KNOTS('',3,(#19985,#19986,#19987,#19988,#19989,
#19990,#19991,#19992,#19993,#19994),.UNSPECIFIED.,.F.,.F.,(4,1,1,1,1,1,
1,4),(47.1238898038469,47.9380705027419,48.9245313961469,49.9109922895519,
50.8974531829569,51.8839140763619,52.8703749697669,53.4070751110265),
 .UNSPECIFIED.);
#557=B_SPLINE_CURVE_WITH_KNOTS('',3,(#19999,#20000,#20001,#20002,#20003,
#20004,#20005,#20006,#20007,#20008),.UNSPECIFIED.,.F.,.F.,(4,1,1,1,1,1,
1,4),(40.8407044966673,41.4528156644579,42.4392765578629,43.4257374512679,
44.4121983446729,45.3986592380779,46.3851201314829,47.1238898038469),
 .UNSPECIFIED.);
#558=B_SPLINE_CURVE_WITH_KNOTS('',3,(#20009,#20010,#20011,#20012,#20013,
#20014,#20015,#20016,#20017,#20018,#20019),.UNSPECIFIED.,.F.,.F.,(4,1,1,
1,1,1,1,1,4),(40.8407044966673,41.0328442489069,42.0193051423119,43.0057660357169,
43.9922269291219,44.9786878225269,45.9651487159319,46.9516096093369,47.1238898038469),
 .UNSPECIFIED.);
#559=B_SPLINE_CURVE_WITH_KNOTS('',3,(#20024,#20025,#20026,#20027,#20028,
#20029,#20030,#20031,#20032,#20033),.UNSPECIFIED.,.F.,.F.,(4,1,1,1,1,1,
1,4),(34.5575191894877,35.5340503040279,36.5205111974329,37.5069720908379,
38.4934329842429,39.4798938776479,40.4663547710529,40.8407044966673),
 .UNSPECIFIED.);
#560=B_SPLINE_CURVE_WITH_KNOTS('',3,(#20034,#20035,#20036,#20037,#20038,
#20039,#20040,#20041,#20042,#20043),.UNSPECIFIED.,.F.,.F.,(4,1,1,1,1,1,
1,4),(34.5575191894877,35.1140788884769,36.1005397818819,37.0870006752869,
38.0734615686919,39.0599224620969,40.0463833555019,40.8407044966673),
 .UNSPECIFIED.);
#561=B_SPLINE_CURVE_WITH_KNOTS('',3,(#20048,#20049,#20050,#20051,#20052,
#20053,#20054,#20055,#20056,#20057,#20058),.UNSPECIFIED.,.F.,.F.,(4,1,1,
1,1,1,1,1,4),(28.2743338823081,28.6288240501929,29.6152849435979,30.6017458370029,
31.5882067304079,32.5746676238129,33.5611285172179,34.5475894106229,34.5575191894877),
 .UNSPECIFIED.);
#562=B_SPLINE_CURVE_WITH_KNOTS('',3,(#20059,#20060,#20061,#20062,#20063,
#20064,#20065,#20066,#20067,#20068),.UNSPECIFIED.,.F.,.F.,(4,1,1,1,1,1,
1,4),(28.2743338823081,29.1953135280469,30.1817744214519,31.1682353148569,
32.1546962082619,33.1411571016669,34.1276179950719,34.5575191894877),
 .UNSPECIFIED.);
#563=B_SPLINE_CURVE_WITH_KNOTS('',3,(#20073,#20074,#20075,#20076,#20077,
#20078,#20079,#20080,#20081,#20082),.UNSPECIFIED.,.F.,.F.,(4,1,1,1,1,1,
1,4),(21.9911485751285,22.7100586897628,23.6965195831678,24.6829804765728,
25.6694413699778,26.6559022633828,27.6423631567879,28.2743338823081),
 .UNSPECIFIED.);
#564=B_SPLINE_CURVE_WITH_KNOTS('',3,(#20083,#20084,#20085,#20086,#20087,
#20088,#20089,#20090,#20091,#20092,#20093),.UNSPECIFIED.,.F.,.F.,(4,1,1,
1,1,1,1,1,4),(21.9911485751285,22.2900872742119,23.2765481676169,24.2630090610219,
25.2494699544269,26.2359308478319,27.2223917412369,28.2088526346419,28.2743338823081),
 .UNSPECIFIED.);
#565=B_SPLINE_CURVE_WITH_KNOTS('',3,(#20099,#20100,#20101,#20102,#20103),
 .UNSPECIFIED.,.F.,.F.,(4,1,4),(14.3984001269718,15.3848610203768,15.7079632679489),
 .UNSPECIFIED.);
#566=B_SPLINE_CURVE_WITH_KNOTS('',3,(#20106,#20107,#20108,#20109,#20110),
 .UNSPECIFIED.,.F.,.F.,(4,1,4),(13.8759337553363,14.8183715425228,15.7079632679489),
 .UNSPECIFIED.);
#567=B_SPLINE_CURVE_WITH_KNOTS('',3,(#20116,#20117,#20118,#20119,#20120,
#20121,#20122,#20123),.UNSPECIFIED.,.F.,.F.,(4,1,1,1,1,4),(59.6902604182061,
60.1955726391529,61.1820335325579,62.1684944259629,63.1549553193679,64.1414162127729),
 .UNSPECIFIED.);
#568=B_SPLINE_CURVE_WITH_KNOTS('',3,(#20126,#20127,#20128,#20129,#20130,
#20131,#20132,#20133,#20134),.UNSPECIFIED.,.F.,.F.,(4,1,1,1,1,1,4),(59.6902604182061,
59.775601223602,60.762062117007,61.748523010412,62.734983903817,63.721444797222,
64.6638825844085),.UNSPECIFIED.);
#569=B_SPLINE_CURVE_WITH_KNOTS('',3,(#20139,#20140,#20141,#20142,#20143,
#20144,#20145,#20146,#20147,#20148),.UNSPECIFIED.,.F.,.F.,(4,1,1,1,1,1,
1,4),(53.4070751110265,54.2768072787229,55.2632681721279,56.2497290655329,
57.2361899589379,58.2226508523429,59.2091117457479,59.6902604182061),
 .UNSPECIFIED.);
#570=B_SPLINE_CURVE_WITH_KNOTS('',3,(#20149,#20150,#20151,#20152,#20153,
#20154,#20155,#20156,#20157,#20158),.UNSPECIFIED.,.F.,.F.,(4,1,1,1,1,1,
1,4),(53.4070751110265,53.856835863172,54.843296756577,55.829757649982,
56.816218543387,57.802679436792,58.789140330197,59.6902604182061),
 .UNSPECIFIED.);
#571=B_SPLINE_CURVE_WITH_KNOTS('',3,(#20163,#20164,#20165,#20166,#20167,
#20168,#20169,#20170,#20171,#20172,#20173),.UNSPECIFIED.,.F.,.F.,(4,1,1,
1,1,1,1,1,4),(47.1238898038469,47.3715810248879,48.3580419182929,49.3445028116979,
50.3309637051029,51.3174245985079,52.3038854919129,53.2903463853179,53.4070751110265),
 .UNSPECIFIED.);
#572=B_SPLINE_CURVE_WITH_KNOTS('',3,(#20174,#20175,#20176,#20177,#20178,
#20179,#20180,#20181,#20182,#20183),.UNSPECIFIED.,.F.,.F.,(4,1,1,1,1,1,
1,4),(47.1238898038469,47.9380705027419,48.9245313961469,49.9109922895519,
50.8974531829569,51.8839140763619,52.8703749697669,53.4070751110265),
 .UNSPECIFIED.);
#573=B_SPLINE_CURVE_WITH_KNOTS('',3,(#20188,#20189,#20190,#20191,#20192,
#20193,#20194,#20195,#20196,#20197),.UNSPECIFIED.,.F.,.F.,(4,1,1,1,1,1,
1,4),(40.8407044966673,41.4528156644579,42.4392765578629,43.4257374512679,
44.4121983446729,45.3986592380779,46.3851201314829,47.1238898038469),
 .UNSPECIFIED.);
#574=B_SPLINE_CURVE_WITH_KNOTS('',3,(#20198,#20199,#20200,#20201,#20202,
#20203,#20204,#20205,#20206,#20207,#20208),.UNSPECIFIED.,.F.,.F.,(4,1,1,
1,1,1,1,1,4),(40.8407044966673,41.0328442489069,42.0193051423119,43.0057660357169,
43.9922269291219,44.9786878225269,45.9651487159319,46.9516096093369,47.1238898038469),
 .UNSPECIFIED.);
#575=B_SPLINE_CURVE_WITH_KNOTS('',3,(#20213,#20214,#20215,#20216,#20217,
#20218,#20219,#20220,#20221,#20222),.UNSPECIFIED.,.F.,.F.,(4,1,1,1,1,1,
1,4),(34.5575191894877,35.5340503040279,36.5205111974329,37.5069720908379,
38.4934329842429,39.4798938776479,40.4663547710529,40.8407044966673),
 .UNSPECIFIED.);
#576=B_SPLINE_CURVE_WITH_KNOTS('',3,(#20223,#20224,#20225,#20226,#20227,
#20228,#20229,#20230,#20231,#20232),.UNSPECIFIED.,.F.,.F.,(4,1,1,1,1,1,
1,4),(34.5575191894877,35.1140788884769,36.1005397818819,37.0870006752869,
38.0734615686919,39.0599224620969,40.0463833555019,40.8407044966673),
 .UNSPECIFIED.);
#577=B_SPLINE_CURVE_WITH_KNOTS('',3,(#20237,#20238,#20239,#20240,#20241,
#20242,#20243,#20244,#20245,#20246,#20247),.UNSPECIFIED.,.F.,.F.,(4,1,1,
1,1,1,1,1,4),(28.2743338823081,28.6288240501928,29.6152849435978,30.6017458370028,
31.5882067304078,32.5746676238129,33.5611285172179,34.5475894106229,34.5575191894877),
 .UNSPECIFIED.);
#578=B_SPLINE_CURVE_WITH_KNOTS('',3,(#20248,#20249,#20250,#20251,#20252,
#20253,#20254,#20255,#20256,#20257),.UNSPECIFIED.,.F.,.F.,(4,1,1,1,1,1,
1,4),(28.2743338823081,29.1953135280469,30.1817744214519,31.1682353148569,
32.1546962082619,33.1411571016669,34.1276179950719,34.5575191894877),
 .UNSPECIFIED.);
#579=B_SPLINE_CURVE_WITH_KNOTS('',3,(#20262,#20263,#20264,#20265,#20266,
#20267,#20268,#20269,#20270,#20271),.UNSPECIFIED.,.F.,.F.,(4,1,1,1,1,1,
1,4),(21.9911485751285,22.7100586897628,23.6965195831678,24.6829804765728,
25.6694413699778,26.6559022633828,27.6423631567878,28.2743338823081),
 .UNSPECIFIED.);
#580=B_SPLINE_CURVE_WITH_KNOTS('',3,(#20272,#20273,#20274,#20275,#20276,
#20277,#20278,#20279,#20280,#20281,#20282),.UNSPECIFIED.,.F.,.F.,(4,1,1,
1,1,1,1,1,4),(21.9911485751285,22.2900872742119,23.2765481676169,24.2630090610219,
25.2494699544269,26.2359308478319,27.2223917412369,28.2088526346419,28.2743338823081),
 .UNSPECIFIED.);
#581=B_SPLINE_CURVE_WITH_KNOTS('',3,(#20288,#20289,#20290,#20291,#20292),
 .UNSPECIFIED.,.F.,.F.,(4,1,4),(14.3984001269718,15.3848610203768,15.7079632679489),
 .UNSPECIFIED.);
#582=B_SPLINE_CURVE_WITH_KNOTS('',3,(#20295,#20296,#20297,#20298,#20299),
 .UNSPECIFIED.,.F.,.F.,(4,1,4),(13.8759337553362,14.8183715425228,15.707963267949),
 .UNSPECIFIED.);
#583=B_SPLINE_CURVE_WITH_KNOTS('',3,(#20305,#20306,#20307,#20308,#20309,
#20310,#20311,#20312),.UNSPECIFIED.,.F.,.F.,(4,1,1,1,1,4),(59.6902604182061,
60.1955726391529,61.1820335325579,62.1684944259629,63.154955319368,64.141416212773),
 .UNSPECIFIED.);
#584=B_SPLINE_CURVE_WITH_KNOTS('',3,(#20315,#20316,#20317,#20318,#20319,
#20320,#20321,#20322,#20323),.UNSPECIFIED.,.F.,.F.,(4,1,1,1,1,1,4),(59.6902604182061,
59.775601223602,60.762062117007,61.748523010412,62.734983903817,63.721444797222,
64.6638825844085),.UNSPECIFIED.);
#585=B_SPLINE_CURVE_WITH_KNOTS('',3,(#20328,#20329,#20330,#20331,#20332,
#20333,#20334,#20335,#20336,#20337),.UNSPECIFIED.,.F.,.F.,(4,1,1,1,1,1,
1,4),(53.4070751110265,54.2768072787229,55.2632681721279,56.2497290655329,
57.2361899589379,58.2226508523429,59.2091117457479,59.6902604182061),
 .UNSPECIFIED.);
#586=B_SPLINE_CURVE_WITH_KNOTS('',3,(#20338,#20339,#20340,#20341,#20342,
#20343,#20344,#20345,#20346,#20347),.UNSPECIFIED.,.F.,.F.,(4,1,1,1,1,1,
1,4),(53.4070751110265,53.856835863172,54.843296756577,55.829757649982,
56.816218543387,57.802679436792,58.789140330197,59.6902604182061),
 .UNSPECIFIED.);
#587=B_SPLINE_CURVE_WITH_KNOTS('',3,(#20352,#20353,#20354,#20355,#20356,
#20357,#20358,#20359,#20360,#20361,#20362),.UNSPECIFIED.,.F.,.F.,(4,1,1,
1,1,1,1,1,4),(47.1238898038469,47.3715810248879,48.3580419182929,49.3445028116979,
50.3309637051029,51.3174245985079,52.3038854919129,53.2903463853179,53.4070751110265),
 .UNSPECIFIED.);
#588=B_SPLINE_CURVE_WITH_KNOTS('',3,(#20363,#20364,#20365,#20366,#20367,
#20368,#20369,#20370,#20371,#20372),.UNSPECIFIED.,.F.,.F.,(4,1,1,1,1,1,
1,4),(47.1238898038469,47.9380705027419,48.9245313961469,49.9109922895519,
50.8974531829569,51.8839140763619,52.8703749697669,53.4070751110265),
 .UNSPECIFIED.);
#589=B_SPLINE_CURVE_WITH_KNOTS('',3,(#20377,#20378,#20379,#20380,#20381,
#20382,#20383,#20384,#20385,#20386),.UNSPECIFIED.,.F.,.F.,(4,1,1,1,1,1,
1,4),(40.8407044966673,41.4528156644579,42.4392765578629,43.4257374512679,
44.4121983446729,45.3986592380779,46.3851201314829,47.1238898038469),
 .UNSPECIFIED.);
#590=B_SPLINE_CURVE_WITH_KNOTS('',3,(#20387,#20388,#20389,#20390,#20391,
#20392,#20393,#20394,#20395,#20396,#20397),.UNSPECIFIED.,.F.,.F.,(4,1,1,
1,1,1,1,1,4),(40.8407044966673,41.0328442489069,42.0193051423119,43.0057660357169,
43.9922269291219,44.9786878225269,45.9651487159319,46.9516096093369,47.1238898038469),
 .UNSPECIFIED.);
#591=B_SPLINE_CURVE_WITH_KNOTS('',3,(#20402,#20403,#20404,#20405,#20406,
#20407,#20408,#20409,#20410,#20411),.UNSPECIFIED.,.F.,.F.,(4,1,1,1,1,1,
1,4),(34.5575191894877,35.5340503040279,36.5205111974329,37.5069720908379,
38.4934329842429,39.4798938776479,40.4663547710529,40.8407044966673),
 .UNSPECIFIED.);
#592=B_SPLINE_CURVE_WITH_KNOTS('',3,(#20412,#20413,#20414,#20415,#20416,
#20417,#20418,#20419,#20420,#20421),.UNSPECIFIED.,.F.,.F.,(4,1,1,1,1,1,
1,4),(34.5575191894877,35.1140788884769,36.1005397818819,37.0870006752869,
38.0734615686919,39.0599224620969,40.0463833555019,40.8407044966673),
 .UNSPECIFIED.);
#593=B_SPLINE_CURVE_WITH_KNOTS('',3,(#20426,#20427,#20428,#20429,#20430,
#20431,#20432,#20433,#20434,#20435,#20436),.UNSPECIFIED.,.F.,.F.,(4,1,1,
1,1,1,1,1,4),(28.2743338823081,28.6288240501929,29.6152849435979,30.6017458370029,
31.5882067304079,32.5746676238129,33.5611285172179,34.5475894106229,34.5575191894877),
 .UNSPECIFIED.);
#594=B_SPLINE_CURVE_WITH_KNOTS('',3,(#20437,#20438,#20439,#20440,#20441,
#20442,#20443,#20444,#20445,#20446),.UNSPECIFIED.,.F.,.F.,(4,1,1,1,1,1,
1,4),(28.2743338823081,29.1953135280469,30.1817744214519,31.1682353148569,
32.1546962082619,33.1411571016669,34.1276179950719,34.5575191894877),
 .UNSPECIFIED.);
#595=B_SPLINE_CURVE_WITH_KNOTS('',3,(#20451,#20452,#20453,#20454,#20455,
#20456,#20457,#20458,#20459,#20460),.UNSPECIFIED.,.F.,.F.,(4,1,1,1,1,1,
1,4),(21.9911485751285,22.7100586897628,23.6965195831678,24.6829804765728,
25.6694413699778,26.6559022633828,27.6423631567879,28.2743338823081),
 .UNSPECIFIED.);
#596=B_SPLINE_CURVE_WITH_KNOTS('',3,(#20461,#20462,#20463,#20464,#20465,
#20466,#20467,#20468,#20469,#20470,#20471),.UNSPECIFIED.,.F.,.F.,(4,1,1,
1,1,1,1,1,4),(21.9911485751285,22.2900872742119,23.2765481676169,24.2630090610219,
25.2494699544269,26.2359308478319,27.2223917412369,28.2088526346419,28.2743338823081),
 .UNSPECIFIED.);
#597=B_SPLINE_CURVE_WITH_KNOTS('',3,(#20477,#20478,#20479,#20480,#20481),
 .UNSPECIFIED.,.F.,.F.,(4,1,4),(14.3984001269718,15.3848610203768,15.7079632679489),
 .UNSPECIFIED.);
#598=B_SPLINE_CURVE_WITH_KNOTS('',3,(#20484,#20485,#20486,#20487,#20488),
 .UNSPECIFIED.,.F.,.F.,(4,1,4),(13.8759337553363,14.8183715425228,15.707963267949),
 .UNSPECIFIED.);
#599=B_SPLINE_CURVE_WITH_KNOTS('',3,(#20494,#20495,#20496,#20497,#20498,
#20499,#20500,#20501),.UNSPECIFIED.,.F.,.F.,(4,1,1,1,1,4),(59.6902604182061,
60.1955726391529,61.1820335325579,62.1684944259629,63.1549553193679,64.1414162127729),
 .UNSPECIFIED.);
#600=B_SPLINE_CURVE_WITH_KNOTS('',3,(#20504,#20505,#20506,#20507,#20508,
#20509,#20510,#20511,#20512),.UNSPECIFIED.,.F.,.F.,(4,1,1,1,1,1,4),(59.6902604182061,
59.775601223602,60.762062117007,61.748523010412,62.734983903817,63.721444797222,
64.6638825844085),.UNSPECIFIED.);
#601=B_SPLINE_CURVE_WITH_KNOTS('',3,(#20517,#20518,#20519,#20520,#20521,
#20522,#20523,#20524,#20525,#20526),.UNSPECIFIED.,.F.,.F.,(4,1,1,1,1,1,
1,4),(53.4070751110265,54.2768072787229,55.2632681721279,56.2497290655329,
57.2361899589379,58.2226508523429,59.2091117457479,59.6902604182061),
 .UNSPECIFIED.);
#602=B_SPLINE_CURVE_WITH_KNOTS('',3,(#20527,#20528,#20529,#20530,#20531,
#20532,#20533,#20534,#20535,#20536),.UNSPECIFIED.,.F.,.F.,(4,1,1,1,1,1,
1,4),(53.4070751110265,53.856835863172,54.843296756577,55.829757649982,
56.816218543387,57.802679436792,58.789140330197,59.6902604182061),
 .UNSPECIFIED.);
#603=B_SPLINE_CURVE_WITH_KNOTS('',3,(#20541,#20542,#20543,#20544,#20545,
#20546,#20547,#20548,#20549,#20550,#20551),.UNSPECIFIED.,.F.,.F.,(4,1,1,
1,1,1,1,1,4),(47.1238898038469,47.3715810248879,48.3580419182929,49.3445028116979,
50.3309637051029,51.3174245985079,52.3038854919129,53.2903463853179,53.4070751110265),
 .UNSPECIFIED.);
#604=B_SPLINE_CURVE_WITH_KNOTS('',3,(#20552,#20553,#20554,#20555,#20556,
#20557,#20558,#20559,#20560,#20561),.UNSPECIFIED.,.F.,.F.,(4,1,1,1,1,1,
1,4),(47.1238898038469,47.9380705027419,48.9245313961469,49.9109922895519,
50.8974531829569,51.8839140763619,52.8703749697669,53.4070751110265),
 .UNSPECIFIED.);
#605=B_SPLINE_CURVE_WITH_KNOTS('',3,(#20566,#20567,#20568,#20569,#20570,
#20571,#20572,#20573,#20574,#20575),.UNSPECIFIED.,.F.,.F.,(4,1,1,1,1,1,
1,4),(40.8407044966673,41.4528156644579,42.4392765578629,43.4257374512679,
44.4121983446729,45.3986592380779,46.3851201314829,47.1238898038469),
 .UNSPECIFIED.);
#606=B_SPLINE_CURVE_WITH_KNOTS('',3,(#20576,#20577,#20578,#20579,#20580,
#20581,#20582,#20583,#20584,#20585,#20586),.UNSPECIFIED.,.F.,.F.,(4,1,1,
1,1,1,1,1,4),(40.8407044966673,41.0328442489069,42.0193051423119,43.0057660357169,
43.9922269291219,44.9786878225269,45.9651487159319,46.9516096093369,47.1238898038469),
 .UNSPECIFIED.);
#607=B_SPLINE_CURVE_WITH_KNOTS('',3,(#20591,#20592,#20593,#20594,#20595,
#20596,#20597,#20598,#20599,#20600),.UNSPECIFIED.,.F.,.F.,(4,1,1,1,1,1,
1,4),(34.5575191894877,35.5340503040279,36.5205111974329,37.5069720908379,
38.4934329842429,39.4798938776479,40.4663547710529,40.8407044966673),
 .UNSPECIFIED.);
#608=B_SPLINE_CURVE_WITH_KNOTS('',3,(#20601,#20602,#20603,#20604,#20605,
#20606,#20607,#20608,#20609,#20610),.UNSPECIFIED.,.F.,.F.,(4,1,1,1,1,1,
1,4),(34.5575191894877,35.1140788884769,36.1005397818819,37.0870006752869,
38.0734615686919,39.0599224620969,40.0463833555019,40.8407044966673),
 .UNSPECIFIED.);
#609=B_SPLINE_CURVE_WITH_KNOTS('',3,(#20615,#20616,#20617,#20618,#20619,
#20620,#20621,#20622,#20623,#20624,#20625),.UNSPECIFIED.,.F.,.F.,(4,1,1,
1,1,1,1,1,4),(28.2743338823081,28.6288240501928,29.6152849435978,30.6017458370028,
31.5882067304078,32.5746676238129,33.5611285172179,34.5475894106229,34.5575191894877),
 .UNSPECIFIED.);
#610=B_SPLINE_CURVE_WITH_KNOTS('',3,(#20626,#20627,#20628,#20629,#20630,
#20631,#20632,#20633,#20634,#20635),.UNSPECIFIED.,.F.,.F.,(4,1,1,1,1,1,
1,4),(28.2743338823081,29.1953135280469,30.1817744214519,31.1682353148569,
32.1546962082619,33.1411571016669,34.1276179950719,34.5575191894877),
 .UNSPECIFIED.);
#611=B_SPLINE_CURVE_WITH_KNOTS('',3,(#20640,#20641,#20642,#20643,#20644,
#20645,#20646,#20647,#20648,#20649),.UNSPECIFIED.,.F.,.F.,(4,1,1,1,1,1,
1,4),(21.9911485751285,22.7100586897628,23.6965195831678,24.6829804765728,
25.6694413699778,26.6559022633828,27.6423631567878,28.2743338823081),
 .UNSPECIFIED.);
#612=B_SPLINE_CURVE_WITH_KNOTS('',3,(#20650,#20651,#20652,#20653,#20654,
#20655,#20656,#20657,#20658,#20659,#20660),.UNSPECIFIED.,.F.,.F.,(4,1,1,
1,1,1,1,1,4),(21.9911485751285,22.2900872742119,23.2765481676169,24.2630090610219,
25.2494699544269,26.2359308478319,27.2223917412369,28.2088526346419,28.2743338823081),
 .UNSPECIFIED.);
#613=B_SPLINE_CURVE_WITH_KNOTS('',3,(#20666,#20667,#20668,#20669,#20670),
 .UNSPECIFIED.,.F.,.F.,(4,1,4),(14.3984001269718,15.3848610203768,15.7079632679489),
 .UNSPECIFIED.);
#614=B_SPLINE_CURVE_WITH_KNOTS('',3,(#20673,#20674,#20675,#20676,#20677),
 .UNSPECIFIED.,.F.,.F.,(4,1,4),(13.8759337553362,14.8183715425228,15.707963267949),
 .UNSPECIFIED.);
#615=B_SPLINE_CURVE_WITH_KNOTS('',3,(#20679,#20680,#20681,#20682,#20683,
#20684,#20685,#20686,#20687,#20688,#20689),.UNSPECIFIED.,.F.,.F.,(4,1,1,
1,1,1,1,1,4),(15.707963267949,15.8048324359278,16.7912933293328,17.7777542227378,
18.7642151161428,19.7506760095478,20.7371369029528,21.7235977963578,21.9911485751285),
 .UNSPECIFIED.);
#616=B_SPLINE_CURVE_WITH_KNOTS('',3,(#20690,#20691,#20692,#20693,#20694,
#20695,#20696,#20697,#20698,#20699),.UNSPECIFIED.,.F.,.F.,(4,1,1,1,1,1,
1,4),(15.7079632679489,16.3713219137818,17.3577828071868,18.3442437005918,
19.3307045939968,20.3171654874019,21.3036263808069,21.9911485751285),
 .UNSPECIFIED.);
#617=B_SPLINE_CURVE_WITH_KNOTS('',3,(#20924,#20925,#20926,#20927,#20928,
#20929,#20930,#20931,#20932,#20933,#20934,#20935,#20936,#20937,#20938,#20939,
#20940,#20941,#20942,#20943,#20944,#20945,#20946,#20947,#20948,#20949,#20950,
#20951,#20952,#20953,#20954,#20955,#20956,#20957,#20958,#20959,#20960,#20961,
#20962,#20963,#20964,#20965,#20966,#20967,#20968,#20969,#20970,#20971,#20972,
#20973,#20974,#20975,#20976,#20977,#20978,#20979,#20980,#20981,#20982,#20983,
#20984,#20985,#20986,#20987,#20988,#20989,#20990,#20991,#20992,#20993,#20994,
#20995,#20996,#20997,#20998,#20999,#21000,#21001,#21002,#21003,#21004,#21005,
#21006,#21007,#21008,#21009,#21010,#21011,#21012,#21013,#21014,#21015,#21016,
#21017,#21018,#21019,#21020),.UNSPECIFIED.,.F.,.F.,(4,3,3,3,3,3,3,3,3,3,
3,3,3,3,3,3,3,3,3,3,3,3,3,3,3,3,3,3,3,3,3,3,4),(0.,0.0368039760561726,0.0744333368184212,
0.113993729911609,0.148609073868149,0.155428926386467,0.160415234743925,
0.197652231831378,0.234804645306633,0.271449203389433,0.301316022933056,
0.308903620706599,0.314301810562592,0.350380482429235,0.385744360315095,
0.390916481563925,0.427339708572203,0.447829010654916,0.457282929707203,
0.462717601073039,0.49927396867586,0.535072006502099,0.570520288994985,
0.593601320607563,0.601390745293023,0.606406519246091,0.641366357839995,
0.669816903853899,0.683592867357584,0.691680491796103,0.725189672020684,
0.755168541895609,0.770777738583641),.UNSPECIFIED.);
#618=B_SPLINE_CURVE_WITH_KNOTS('',3,(#21021,#21022,#21023,#21024,#21025,
#21026,#21027,#21028,#21029,#21030,#21031,#21032,#21033,#21034,#21035,#21036,
#21037,#21038,#21039,#21040,#21041,#21042,#21043,#21044,#21045,#21046,#21047,
#21048,#21049,#21050,#21051,#21052,#21053,#21054,#21055,#21056,#21057,#21058,
#21059,#21060,#21061,#21062,#21063,#21064,#21065,#21066,#21067,#21068,#21069,
#21070,#21071,#21072,#21073,#21074,#21075,#21076,#21077,#21078,#21079,#21080,
#21081,#21082,#21083,#21084,#21085,#21086,#21087,#21088,#21089,#21090,#21091,
#21092,#21093,#21094,#21095,#21096,#21097,#21098,#21099,#21100,#21101,#21102,
#21103,#21104,#21105,#21106,#21107,#21108,#21109,#21110,#21111,#21112,#21113,
#21114),.UNSPECIFIED.,.F.,.F.,(4,3,3,3,3,3,3,3,3,3,3,3,3,3,3,3,3,3,3,3,
3,3,3,3,3,3,3,3,3,3,3,4),(0.,0.032722467477059,0.0662804545367435,0.10053688939052,
0.133256613707586,0.138568806761047,0.143645866999149,0.178633816756561,
0.214080697136686,0.251134193834276,0.278924316357469,0.285558989874725,
0.321777082201843,0.35776277380543,0.362294683927046,0.397656589907163,
0.419708610865643,0.427245995316486,0.432639299360784,0.468078725795143,
0.504737384281388,0.54174098163239,0.567834474583697,0.579481956142016,
0.584481809181592,0.622063983748247,0.654170219121896,0.668576993434055,
0.678363333947687,0.716158233455664,0.750488925242844,0.768398079192646),
 .UNSPECIFIED.);
#619=B_SPLINE_CURVE_WITH_KNOTS('',3,(#21115,#21116,#21117,#21118,#21119,
#21120,#21121,#21122,#21123,#21124,#21125,#21126,#21127,#21128,#21129,#21130,
#21131,#21132,#21133,#21134,#21135,#21136,#21137,#21138,#21139),
 .UNSPECIFIED.,.F.,.F.,(4,3,3,3,3,3,3,3,4),(-10.1321597128207,-9.86460893405003,
-8.87814804064502,-7.89168714724003,-6.90522625383502,-5.91876536043002,
-4.93230446702502,-3.94584357362001,-3.84897440564115),.UNSPECIFIED.);
#620=B_SPLINE_CURVE_WITH_KNOTS('',3,(#21364,#21365,#21366,#21367,#21368,
#21369,#21370,#21371,#21372,#21373,#21374,#21375,#21376,#21377,#21378,#21379,
#21380,#21381,#21382,#21383,#21384,#21385,#21386,#21387,#21388,#21389,#21390,
#21391,#21392,#21393,#21394,#21395,#21396,#21397,#21398,#21399,#21400,#21401,
#21402,#21403,#21404,#21405,#21406,#21407,#21408,#21409,#21410,#21411,#21412,
#21413,#21414,#21415,#21416,#21417,#21418,#21419,#21420,#21421,#21422,#21423,
#21424,#21425,#21426,#21427,#21428,#21429,#21430,#21431,#21432,#21433,#21434,
#21435,#21436,#21437,#21438,#21439,#21440,#21441,#21442,#21443,#21444,#21445,
#21446,#21447,#21448,#21449,#21450,#21451,#21452,#21453,#21454,#21455,#21456,
#21457),.UNSPECIFIED.,.F.,.F.,(4,3,3,3,3,3,3,3,3,3,3,3,3,3,3,3,3,3,3,3,
3,3,3,3,3,3,3,3,3,3,3,4),(0.,0.0327225799773267,0.0662806658545984,0.100537171029244,
0.133256860141472,0.138569969050608,0.143646002487887,0.178634022059388,
0.214080931165366,0.251134369355791,0.27892444799861,0.285558993885552,
0.321777092476967,0.357762747477908,0.362294683927068,0.397656542631737,
0.419708566544936,0.427246605750548,0.432639210952107,0.468078568034648,
0.504737197455354,0.541740788532467,0.567834305621274,0.579481260120421,
0.584480754431237,0.622062913075079,0.654169416117039,0.668576403279121,
0.678363443657298,0.716158340709877,0.750488925242921,0.768398079192729),
 .UNSPECIFIED.);
#621=B_SPLINE_CURVE_WITH_KNOTS('',3,(#21458,#21459,#21460,#21461,#21462,
#21463,#21464,#21465,#21466,#21467,#21468,#21469,#21470,#21471,#21472,#21473,
#21474,#21475,#21476,#21477,#21478,#21479,#21480,#21481,#21482),
 .UNSPECIFIED.,.F.,.F.,(4,3,3,3,3,3,3,3,4),(7.59274844815668,7.89168714724002,
8.87814804064503,9.86460893405003,10.851069827455,11.83753072086,12.823991614265,
13.81045250767,13.8759337553363),.UNSPECIFIED.);
#622=B_SPLINE_CURVE_WITH_KNOTS('',3,(#21483,#21484,#21485,#21486,#21487,
#21488,#21489,#21490,#21491,#21492,#21493,#21494,#21495,#21496,#21497,#21498,
#21499,#21500,#21501,#21502,#21503,#21504,#21505,#21506,#21507,#21508,#21509,
#21510,#21511,#21512,#21513,#21514,#21515,#21516,#21517,#21518,#21519,#21520,
#21521,#21522,#21523,#21524,#21525,#21526,#21527,#21528,#21529,#21530,#21531,
#21532,#21533,#21534,#21535,#21536,#21537,#21538,#21539,#21540,#21541,#21542,
#21543,#21544,#21545,#21546,#21547,#21548,#21549,#21550,#21551,#21552,#21553,
#21554,#21555,#21556,#21557,#21558,#21559,#21560,#21561,#21562,#21563,#21564,
#21565,#21566,#21567,#21568,#21569,#21570,#21571,#21572,#21573,#21574,#21575,
#21576,#21577,#21578,#21579),.UNSPECIFIED.,.F.,.F.,(4,3,3,3,3,3,3,3,3,3,
3,3,3,3,3,3,3,3,3,3,3,3,3,3,3,3,3,3,3,3,3,3,4),(0.,0.0368040733914109,0.0744334923513577,
0.113993866002931,0.148609192948057,0.155429662167008,0.160415950914505,
0.197652959912295,0.23480534579311,0.271449857509325,0.301316513522979,
0.308905291482282,0.314302114409216,0.350380752512021,0.385744595636286,
0.390916481563942,0.427339707606562,0.447829009749629,0.457282909273663,
0.462717595625807,0.499273963909537,0.53507200404104,0.57052027575377,0.593601309021504,
0.60139070143526,0.60640643038342,0.641366263001721,0.669816832725203,0.683592798284754,
0.691680481858046,0.725189622506651,0.755168541895646,0.770777738583679),
 .UNSPECIFIED.);
#623=B_SPLINE_CURVE_WITH_KNOTS('',3,(#21589,#21590,#21591,#21592,#21593,
#21594,#21595,#21596,#21597,#21598,#21599,#21600,#21601,#21602,#21603,#21604,
#21605,#21606,#21607,#21608,#21609,#21610,#21611,#21612,#21613,#21614,#21615,
#21616,#21617,#21618,#21619,#21620,#21621,#21622,#21623,#21624,#21625,#21626,
#21627,#21628,#21629,#21630,#21631,#21632,#21633,#21634,#21635,#21636,#21637,
#21638,#21639,#21640,#21641,#21642,#21643,#21644,#21645,#21646,#21647,#21648,
#21649,#21650,#21651,#21652,#21653,#21654,#21655,#21656,#21657,#21658,#21659,
#21660,#21661,#21662,#21663,#21664,#21665,#21666,#21667,#21668,#21669,#21670,
#21671,#21672,#21673,#21674,#21675,#21676,#21677,#21678,#21679,#21680,#21681,
#21682),.UNSPECIFIED.,.F.,.F.,(4,3,3,3,3,3,3,3,3,3,3,3,3,3,3,3,3,3,3,3,
3,3,3,3,3,3,3,3,3,3,3,4),(0.,0.0327224959120641,0.0662805079475318,0.100536960576692,
0.133256675995489,0.138569100515552,0.143645901206212,0.1786338686101,0.214080756253453,
0.251134238171856,0.278924349610658,0.285558990870915,0.321777084786821,
0.35776276714434,0.362294683927063,0.39765657796237,0.419708599667403,0.427246149485785,
0.432639276975905,0.468078685886249,0.504737337027106,0.541740932792406,
0.567834431848717,0.579481780097231,0.584481542244862,0.622063712786212,
0.654170015900382,0.6685768440841,0.678363361689231,0.716158260579035,0.750488925242892,
0.768398079192696),.UNSPECIFIED.);
#624=B_SPLINE_CURVE_WITH_KNOTS('',3,(#21683,#21684,#21685,#21686,#21687,
#21688,#21689,#21690,#21691,#21692,#21693,#21694,#21695,#21696,#21697,#21698,
#21699,#21700,#21701,#21702,#21703,#21704,#21705,#21706,#21707,#21708,#21709,
#21710,#21711,#21712,#21713,#21714,#21715,#21716,#21717,#21718,#21719,#21720,
#21721,#21722,#21723,#21724,#21725,#21726,#21727,#21728,#21729,#21730,#21731,
#21732,#21733,#21734,#21735,#21736,#21737,#21738,#21739,#21740,#21741,#21742,
#21743,#21744,#21745,#21746,#21747,#21748,#21749,#21750,#21751,#21752,#21753,
#21754,#21755,#21756,#21757,#21758,#21759,#21760,#21761,#21762,#21763,#21764,
#21765,#21766,#21767,#21768,#21769,#21770,#21771,#21772,#21773,#21774,#21775,
#21776,#21777,#21778,#21779),.UNSPECIFIED.,.F.,.F.,(4,3,3,3,3,3,3,3,3,3,
3,3,3,3,3,3,3,3,3,3,3,3,3,3,3,3,3,3,3,3,3,3,4),(0.,0.0368039914157241,0.0744333613634087,
0.113993751388472,0.148609092660403,0.155429042492168,0.160415347695229,
0.197652346662473,0.234804755786334,0.271449306551343,0.301316100304487,
0.308903884150417,0.314301858425386,0.350380524963378,0.385744397367857,
0.390916481563918,0.427339708424226,0.447829010516186,0.457282926489124,
0.462717600214839,0.499273967924932,0.53507200611566,0.570520286913965,
0.593601318786667,0.601390738323114,0.606406505217338,0.64136634286951,
0.669816892626028,0.683592856456032,0.691680490247784,0.725189664234744,
0.75516854189558,0.770777738583609),.UNSPECIFIED.);
#625=B_SPLINE_CURVE_WITH_KNOTS('',3,(#21780,#21781,#21782,#21783,#21784,
#21785,#21786,#21787,#21788,#21789,#21790,#21791,#21792,#21793,#21794,#21795,
#21796,#21797,#21798,#21799,#21800,#21801,#21802,#21803,#21804,#21805,#21806,
#21807,#21808,#21809,#21810,#21811,#21812,#21813,#21814,#21815,#21816,#21817,
#21818,#21819,#21820,#21821,#21822,#21823,#21824,#21825,#21826,#21827,#21828,
#21829,#21830,#21831,#21832,#21833,#21834,#21835,#21836,#21837,#21838,#21839,
#21840,#21841,#21842,#21843,#21844,#21845,#21846,#21847,#21848,#21849,#21850,
#21851,#21852,#21853,#21854,#21855,#21856,#21857,#21858,#21859,#21860,#21861,
#21862,#21863,#21864,#21865,#21866,#21867,#21868,#21869,#21870,#21871,#21872,
#21873),.UNSPECIFIED.,.F.,.F.,(4,3,3,3,3,3,3,3,3,3,3,3,3,3,3,3,3,3,3,3,
3,3,3,3,3,3,3,3,3,3,3,4),(0.,0.0327225294770781,0.0662805709960721,0.100537044605592,
0.133256749520777,0.138569447222746,0.143645941610917,0.17863392984422,
0.214080826059521,0.251134290526409,0.278924388876575,0.285558992053491,
0.321777087844177,0.357762759284444,0.362294683927074,0.397656563857957,
0.419708586444518,0.427246331524387,0.432639250564409,0.468078638783316,
0.50473728125208,0.541740875145429,0.567834381407617,0.579481572313244,
0.584481227357561,0.622063393148413,0.654169776172043,0.668576667903374,
0.678363394448717,0.71615829260595,0.750488925242933,0.768398079192735),
 .UNSPECIFIED.);
#626=B_SPLINE_CURVE_WITH_KNOTS('',3,(#21874,#21875,#21876,#21877,#21878,
#21879,#21880,#21881,#21882,#21883,#21884,#21885,#21886,#21887,#21888,#21889,
#21890,#21891,#21892,#21893,#21894,#21895,#21896,#21897,#21898,#21899,#21900,
#21901,#21902,#21903,#21904,#21905,#21906,#21907,#21908,#21909,#21910,#21911,
#21912,#21913,#21914,#21915,#21916,#21917,#21918,#21919,#21920,#21921,#21922,
#21923,#21924,#21925,#21926,#21927,#21928,#21929,#21930,#21931,#21932,#21933,
#21934,#21935,#21936,#21937,#21938,#21939,#21940,#21941,#21942,#21943,#21944,
#21945,#21946,#21947,#21948,#21949,#21950,#21951,#21952,#21953,#21954,#21955,
#21956,#21957,#21958,#21959,#21960,#21961,#21962,#21963,#21964,#21965,#21966,
#21967,#21968,#21969,#21970),.UNSPECIFIED.,.F.,.F.,(4,3,3,3,3,3,3,3,3,3,
3,3,3,3,3,3,3,3,3,3,3,3,3,3,3,3,3,3,3,3,3,3,4),(0.,0.0368040169038835,0.0744334020924358,
0.11399378702637,0.148609123843563,0.155429235171562,0.160415535189551,
0.197652537277058,0.234804939176668,0.271449477805488,0.301316228745094,
0.308904321525207,0.31430193792665,0.350380595626898,0.385744458930709,
0.390916481563911,0.427339708170469,0.447829010278287,0.45728292112946,
0.462717598788197,0.499273966676618,0.535072005472898,0.570520283450759,
0.593601315756361,0.601390726866048,0.606406481970154,0.641366318060403,
0.669816874019195,0.683592838382448,0.691680487645043,0.725189651274617,
0.75516854189557,0.770777738583599),.UNSPECIFIED.);
#627=B_SPLINE_CURVE_WITH_KNOTS('',3,(#21971,#21972,#21973,#21974,#21975,
#21976,#21977,#21978,#21979,#21980,#21981,#21982,#21983,#21984,#21985,#21986,
#21987,#21988,#21989,#21990,#21991,#21992,#21993,#21994,#21995,#21996,#21997,
#21998,#21999,#22000,#22001,#22002,#22003,#22004,#22005,#22006,#22007,#22008,
#22009,#22010,#22011,#22012,#22013,#22014,#22015,#22016,#22017,#22018,#22019,
#22020,#22021,#22022,#22023,#22024,#22025,#22026,#22027,#22028,#22029,#22030,
#22031,#22032,#22033,#22034,#22035,#22036,#22037,#22038,#22039,#22040,#22041,
#22042,#22043,#22044,#22045,#22046,#22047,#22048,#22049,#22050,#22051,#22052,
#22053,#22054,#22055,#22056,#22057,#22058,#22059,#22060,#22061,#22062,#22063,
#22064),.UNSPECIFIED.,.F.,.F.,(4,3,3,3,3,3,3,3,3,3,3,3,3,3,3,3,3,3,3,3,
3,3,3,3,3,3,3,3,3,3,3,4),(0.,0.0327224441775746,0.0662804107708102,0.100536831058394,
0.133256562666979,0.138568566128973,0.143645838996043,0.178633774293771,
0.214080648720454,0.251134157522108,0.278924289123348,0.285558989031475,
0.321777080052277,0.357762779229756,0.362294683927068,0.397656599693718,
0.419708620040541,0.427245869011975,0.432639317722629,0.468078758515067,
0.504737423019667,0.541741021670041,0.567834509616647,0.5794821004587,0.584482028048437,
0.622064205916635,0.6541703857482,0.668577115889702,0.678363311229139,0.716158211242659,
0.750488925242892,0.768398079192695),.UNSPECIFIED.);
#628=B_SPLINE_CURVE_WITH_KNOTS('',3,(#22065,#22066,#22067,#22068,#22069,
#22070,#22071,#22072,#22073,#22074,#22075,#22076,#22077,#22078,#22079,#22080,
#22081,#22082,#22083,#22084,#22085,#22086,#22087,#22088,#22089,#22090,#22091,
#22092,#22093,#22094,#22095,#22096,#22097,#22098,#22099,#22100,#22101,#22102,
#22103,#22104,#22105,#22106,#22107,#22108,#22109,#22110,#22111,#22112,#22113,
#22114,#22115,#22116,#22117,#22118,#22119,#22120,#22121,#22122,#22123,#22124,
#22125,#22126,#22127,#22128,#22129,#22130,#22131,#22132,#22133,#22134,#22135,
#22136,#22137,#22138,#22139,#22140,#22141,#22142,#22143,#22144,#22145,#22146,
#22147,#22148,#22149,#22150,#22151,#22152,#22153,#22154,#22155,#22156,#22157,
#22158,#22159,#22160,#22161),.UNSPECIFIED.,.F.,.F.,(4,3,3,3,3,3,3,3,3,3,
3,3,3,3,3,3,3,3,3,3,3,3,3,3,3,3,3,3,3,3,3,3,4),(0.,0.036804046830165,0.0744334499110545,
0.113993828867664,0.148609160454698,0.155429461366191,0.160415755364031,
0.197652761113477,0.234805154528782,0.271449678901402,0.301316379567035,
0.30890483519103,0.314302031357973,0.350380678677425,0.385744531292533,
0.390916481563933,0.427339707871941,0.447829009998422,0.457282914861488,
0.462717597114684,0.499273965212302,0.535072004716797,0.570520279377824,
0.59360131219255,0.601390713399489,0.606406454642536,0.641366288894707,
0.669816852144937,0.683592817141769,0.691680484574319,0.72518963603372,
0.75516854189563,0.77077773858366),.UNSPECIFIED.);
#629=B_SPLINE_CURVE_WITH_KNOTS('',3,(#22163,#22164,#22165,#22166,#22167,
#22168,#22169,#22170,#22171,#22172,#22173),.UNSPECIFIED.,.F.,.F.,(4,1,1,
1,1,1,1,1,4),(15.707963267949,15.8048324359278,16.7912933293328,17.7777542227378,
18.7642151161428,19.7506760095478,20.7371369029528,21.7235977963578,21.9911485751285),
 .UNSPECIFIED.);
#630=B_SPLINE_CURVE_WITH_KNOTS('',3,(#22174,#22175,#22176,#22177,#22178,
#22179,#22180,#22181,#22182,#22183),.UNSPECIFIED.,.F.,.F.,(4,1,1,1,1,1,
1,4),(15.7079632679489,16.3713219137818,17.3577828071869,18.3442437005919,
19.3307045939969,20.3171654874019,21.3036263808069,21.9911485751285),
 .UNSPECIFIED.);
#631=B_SPLINE_CURVE_WITH_KNOTS('',3,(#22408,#22409,#22410,#22411,#22412,
#22413,#22414,#22415,#22416,#22417,#22418,#22419,#22420,#22421,#22422,#22423,
#22424,#22425,#22426,#22427,#22428,#22429,#22430,#22431,#22432,#22433,#22434,
#22435,#22436,#22437,#22438,#22439,#22440,#22441,#22442,#22443,#22444,#22445,
#22446,#22447,#22448,#22449,#22450,#22451,#22452,#22453,#22454,#22455,#22456,
#22457,#22458,#22459,#22460,#22461,#22462,#22463,#22464,#22465,#22466,#22467,
#22468,#22469,#22470,#22471,#22472,#22473,#22474,#22475,#22476,#22477,#22478,
#22479,#22480,#22481,#22482,#22483,#22484,#22485,#22486,#22487,#22488,#22489,
#22490,#22491,#22492,#22493,#22494,#22495,#22496,#22497,#22498,#22499,#22500,
#22501,#22502,#22503,#22504),.UNSPECIFIED.,.F.,.F.,(4,3,3,3,3,3,3,3,3,3,
3,3,3,3,3,3,3,3,3,3,3,3,3,3,3,3,3,3,3,3,3,3,4),(0.,0.0368040006584821,0.0744333761311954,
0.113993764310286,0.14860910396699,0.155429112383965,0.160415415803185,
0.19765241590165,0.234804822404722,0.27144936877189,0.301316146969897,0.308904043046986,
0.314301887301155,0.350380550636825,0.385744419741531,0.39091648156392,
0.427339708332513,0.447829010430206,0.45728292453119,0.462717599696291,
0.499273967471206,0.535072005882051,0.570520285658179,0.593601317687859,
0.601390734201157,0.60640649698701,0.641366334082055,0.669816886035445,
0.683592850009941,0.691680489272535,0.725189659504915,0.755168541895614,
0.770777738583643),.UNSPECIFIED.);
#632=B_SPLINE_CURVE_WITH_KNOTS('',3,(#22505,#22506,#22507,#22508,#22509,
#22510,#22511,#22512,#22513,#22514,#22515,#22516,#22517,#22518,#22519,#22520,
#22521,#22522,#22523,#22524,#22525,#22526,#22527,#22528,#22529),
 .UNSPECIFIED.,.F.,.F.,(4,3,3,3,3,3,3,3,4),(-10.1321597128207,-9.86460893405003,
-8.87814804064502,-7.89168714724002,-6.90522625383502,-5.91876536043002,
-4.93230446702501,-3.94584357362001,-3.84897440564114),.UNSPECIFIED.);
#633=B_SPLINE_CURVE_WITH_KNOTS('',3,(#22754,#22755,#22756,#22757,#22758,
#22759,#22760,#22761,#22762,#22763,#22764,#22765,#22766,#22767,#22768,#22769,
#22770,#22771,#22772,#22773,#22774,#22775,#22776,#22777,#22778,#22779,#22780,
#22781,#22782,#22783,#22784,#22785,#22786,#22787,#22788,#22789,#22790,#22791,
#22792,#22793,#22794,#22795,#22796,#22797,#22798,#22799,#22800,#22801,#22802,
#22803,#22804,#22805,#22806,#22807,#22808,#22809,#22810,#22811,#22812,#22813,
#22814,#22815,#22816,#22817,#22818,#22819,#22820,#22821,#22822,#22823,#22824,
#22825,#22826,#22827,#22828,#22829,#22830,#22831,#22832,#22833,#22834,#22835,
#22836,#22837,#22838,#22839,#22840,#22841,#22842,#22843,#22844,#22845,#22846,
#22847),.UNSPECIFIED.,.F.,.F.,(4,3,3,3,3,3,3,3,3,3,3,3,3,3,3,3,3,3,3,3,
3,3,3,3,3,3,3,3,3,3,3,4),(0.,0.0327224852298601,0.0662804878799529,0.100536933829056,
0.133256652591307,0.138568990289855,0.143645888367285,0.178633849142766,
0.214080734056413,0.251134221524075,0.278924337124821,0.285558990484342,
0.321777083808023,0.357762769641534,0.362294683927059,0.397656582449134,
0.419708603873742,0.427246091593913,0.432639285230977,0.468078700718258,
0.504737354615871,0.541740950976496,0.567834447759792,0.579481845655055,
0.584481641657808,0.62206381370368,0.654170091588477,0.668576899729838,
0.678363351333556,0.716158250454694,0.750488925242868,0.768398079192674),
 .UNSPECIFIED.);
#634=B_SPLINE_CURVE_WITH_KNOTS('',3,(#22848,#22849,#22850,#22851,#22852,
#22853,#22854,#22855,#22856,#22857,#22858,#22859,#22860,#22861,#22862,#22863,
#22864,#22865,#22866,#22867,#22868,#22869,#22870,#22871,#22872),
 .UNSPECIFIED.,.F.,.F.,(4,3,3,3,3,3,3,3,4),(7.59274844815667,7.89168714724002,
8.87814804064502,9.86460893405003,10.851069827455,11.83753072086,12.823991614265,
13.81045250767,13.8759337553363),.UNSPECIFIED.);
#635=B_SPLINE_CURVE_WITH_KNOTS('',3,(#22874,#22875,#22876,#22877,#22878,
#22879,#22880,#22881,#22882,#22883,#22884),.UNSPECIFIED.,.F.,.F.,(4,1,1,
1,1,1,1,1,4),(15.707963267949,15.8048324359278,16.7912933293328,17.7777542227378,
18.7642151161428,19.7506760095478,20.7371369029528,21.7235977963578,21.9911485751285),
 .UNSPECIFIED.);
#636=B_SPLINE_CURVE_WITH_KNOTS('',3,(#22885,#22886,#22887,#22888,#22889,
#22890,#22891,#22892,#22893,#22894),.UNSPECIFIED.,.F.,.F.,(4,1,1,1,1,1,
1,4),(15.7079632679489,16.3713219137818,17.3577828071868,18.3442437005918,
19.3307045939968,20.3171654874019,21.3036263808069,21.9911485751285),
 .UNSPECIFIED.);
#637=B_SPLINE_CURVE_WITH_KNOTS('',3,(#23119,#23120,#23121,#23122,#23123,
#23124,#23125,#23126,#23127,#23128,#23129,#23130,#23131,#23132,#23133,#23134,
#23135,#23136,#23137,#23138,#23139,#23140,#23141,#23142,#23143,#23144,#23145,
#23146,#23147,#23148,#23149,#23150,#23151,#23152,#23153,#23154,#23155,#23156,
#23157,#23158,#23159,#23160,#23161,#23162,#23163,#23164,#23165,#23166,#23167,
#23168,#23169,#23170,#23171,#23172,#23173,#23174,#23175,#23176,#23177,#23178,
#23179,#23180,#23181,#23182,#23183,#23184,#23185,#23186,#23187,#23188,#23189,
#23190,#23191,#23192,#23193,#23194,#23195,#23196,#23197,#23198,#23199,#23200,
#23201,#23202,#23203,#23204,#23205,#23206,#23207,#23208,#23209,#23210,#23211,
#23212,#23213,#23214,#23215),.UNSPECIFIED.,.F.,.F.,(4,3,3,3,3,3,3,3,3,3,
3,3,3,3,3,3,3,3,3,3,3,3,3,3,3,3,3,3,3,3,3,3,4),(0.,0.0368039558979425,0.074433304608195,
0.113993701727663,0.148609049207197,0.155428774052918,0.160415086629183,
0.19765208124705,0.234804500431717,0.271449068097489,0.301315921464101,
0.308903275242872,0.314301747825082,0.350380426672586,0.385744311753463,
0.390916481563936,0.427339708778546,0.447829010848363,0.457282933923372,
0.462717602197838,0.49927396966006,0.535072007005015,0.570520291726377,
0.593601322997532,0.601390754314479,0.606406537654944,0.641366377472567,
0.669816918578329,0.683592881655056,0.691680493901417,0.725189682307058,
0.755168541895614,0.770777738583641),.UNSPECIFIED.);
#638=B_SPLINE_CURVE_WITH_KNOTS('',3,(#23216,#23217,#23218,#23219,#23220,
#23221,#23222,#23223,#23224,#23225,#23226,#23227,#23228,#23229,#23230,#23231,
#23232,#23233,#23234,#23235,#23236,#23237,#23238,#23239,#23240),
 .UNSPECIFIED.,.F.,.F.,(4,3,3,3,3,3,3,3,4),(-10.1321597128207,-9.86460893405003,
-8.87814804064502,-7.89168714724003,-6.90522625383502,-5.91876536043002,
-4.93230446702502,-3.94584357362001,-3.84897440564115),.UNSPECIFIED.);
#639=B_SPLINE_CURVE_WITH_KNOTS('',3,(#23465,#23466,#23467,#23468,#23469,
#23470,#23471,#23472,#23473,#23474,#23475,#23476,#23477,#23478,#23479,#23480,
#23481,#23482,#23483,#23484,#23485,#23486,#23487,#23488,#23489,#23490,#23491,
#23492,#23493,#23494,#23495,#23496,#23497,#23498,#23499,#23500,#23501,#23502,
#23503,#23504,#23505,#23506,#23507,#23508,#23509,#23510,#23511,#23512,#23513,
#23514,#23515,#23516,#23517,#23518,#23519,#23520,#23521,#23522,#23523,#23524,
#23525,#23526,#23527,#23528,#23529,#23530,#23531,#23532,#23533,#23534,#23535,
#23536,#23537,#23538,#23539,#23540,#23541,#23542,#23543,#23544,#23545,#23546,
#23547,#23548,#23549,#23550,#23551,#23552,#23553,#23554,#23555,#23556,#23557,
#23558),.UNSPECIFIED.,.F.,.F.,(4,3,3,3,3,3,3,3,3,3,3,3,3,3,3,3,3,3,3,3,
3,3,3,3,3,3,3,3,3,3,3,4),(0.,0.0327225492804934,0.0662806081929849,0.100537094180834,
0.133256792899112,0.138569651942616,0.143645965484312,0.178633966005382,
0.214080867277344,0.251134321439773,0.278924412061594,0.285558992744241,
0.321777089637378,0.35776275463403,0.362294683927058,0.397656555534726,
0.419708578641487,0.427246439006672,0.432639234997264,0.468078611004923,
0.504737248356826,0.541740841146129,0.567834351658225,0.579481449773753,
0.584481041781399,0.622063204762494,0.654169634882595,0.668576564062872,
0.678363413635591,0.716158311359956,0.750488925242897,0.768398079192707),
 .UNSPECIFIED.);
#640=B_SPLINE_CURVE_WITH_KNOTS('',3,(#23559,#23560,#23561,#23562,#23563,
#23564,#23565,#23566,#23567,#23568,#23569,#23570,#23571,#23572,#23573,#23574,
#23575,#23576,#23577,#23578,#23579,#23580,#23581,#23582,#23583),
 .UNSPECIFIED.,.F.,.F.,(4,3,3,3,3,3,3,3,4),(7.59274844815668,7.89168714724002,
8.87814804064503,9.86460893405003,10.851069827455,11.83753072086,12.823991614265,
13.81045250767,13.8759337553363),.UNSPECIFIED.);
#641=B_SPLINE_CURVE_WITH_KNOTS('',3,(#23585,#23586,#23587,#23588,#23589,
#23590,#23591,#23592,#23593,#23594,#23595),.UNSPECIFIED.,.F.,.F.,(4,1,1,
1,1,1,1,1,4),(15.7079632679489,15.8048324359278,16.7912933293328,17.7777542227378,
18.7642151161428,19.7506760095478,20.7371369029528,21.7235977963578,21.9911485751285),
 .UNSPECIFIED.);
#642=B_SPLINE_CURVE_WITH_KNOTS('',3,(#23596,#23597,#23598,#23599,#23600,
#23601,#23602,#23603,#23604,#23605),.UNSPECIFIED.,.F.,.F.,(4,1,1,1,1,1,
1,4),(15.7079632679489,16.3713219137818,17.3577828071869,18.3442437005919,
19.3307045939969,20.3171654874019,21.3036263808069,21.9911485751285),
 .UNSPECIFIED.);
#643=B_SPLINE_CURVE_WITH_KNOTS('',3,(#23830,#23831,#23832,#23833,#23834,
#23835,#23836,#23837,#23838,#23839,#23840,#23841,#23842,#23843,#23844,#23845,
#23846,#23847,#23848,#23849,#23850,#23851,#23852,#23853,#23854,#23855,#23856,
#23857,#23858,#23859,#23860,#23861,#23862,#23863,#23864,#23865,#23866,#23867,
#23868,#23869,#23870,#23871,#23872,#23873,#23874,#23875,#23876,#23877,#23878,
#23879,#23880,#23881,#23882,#23883,#23884,#23885,#23886,#23887,#23888,#23889,
#23890,#23891,#23892,#23893,#23894,#23895,#23896,#23897,#23898,#23899,#23900,
#23901,#23902,#23903,#23904,#23905,#23906,#23907,#23908,#23909,#23910,#23911,
#23912,#23913,#23914,#23915,#23916,#23917,#23918,#23919,#23920,#23921,#23922,
#23923,#23924,#23925,#23926),.UNSPECIFIED.,.F.,.F.,(4,3,3,3,3,3,3,3,3,3,
3,3,3,3,3,3,3,3,3,3,3,3,3,3,3,3,3,3,3,3,3,3,4),(0.,0.0368040296983295,0.0744334225357169,
0.113993804914242,0.148609139495452,0.155429331856321,0.160415629309949,
0.19765263296232,0.234805031233744,0.271449563770314,0.301316293218716,
0.308904541097941,0.314301977856807,0.350380631124549,0.385744489860858,
0.39091648156392,0.427339708037647,0.447829010153769,0.457282918385807,
0.462717598065727,0.499273966044462,0.535072005142963,0.570520281705417,
0.593601314229191,0.601390721049491,0.606406470197016,0.641366305496701,
0.669816864596427,0.6835928292529,0.691680486306265,0.725189644734797,0.755168541895606,
0.770777738583634),.UNSPECIFIED.);
#644=B_SPLINE_CURVE_WITH_KNOTS('',3,(#23927,#23928,#23929,#23930,#23931,
#23932,#23933,#23934,#23935,#23936,#23937,#23938,#23939,#23940,#23941,#23942,
#23943,#23944,#23945,#23946,#23947,#23948,#23949,#23950,#23951),
 .UNSPECIFIED.,.F.,.F.,(4,3,3,3,3,3,3,3,4),(-10.1321597128207,-9.86460893405003,
-8.87814804064502,-7.89168714724002,-6.90522625383502,-5.91876536043002,
-4.93230446702502,-3.94584357362001,-3.84897440564114),.UNSPECIFIED.);
#645=B_SPLINE_CURVE_WITH_KNOTS('',3,(#24176,#24177,#24178,#24179,#24180,
#24181,#24182,#24183,#24184,#24185,#24186,#24187,#24188,#24189,#24190,#24191,
#24192,#24193,#24194,#24195,#24196,#24197,#24198,#24199,#24200,#24201,#24202,
#24203,#24204,#24205,#24206,#24207,#24208,#24209,#24210,#24211,#24212,#24213,
#24214,#24215,#24216,#24217,#24218,#24219,#24220,#24221,#24222,#24223,#24224,
#24225,#24226,#24227,#24228,#24229,#24230,#24231,#24232,#24233,#24234,#24235,
#24236,#24237,#24238,#24239,#24240,#24241,#24242,#24243,#24244,#24245,#24246,
#24247,#24248,#24249,#24250,#24251,#24252,#24253,#24254,#24255,#24256,#24257,
#24258,#24259,#24260,#24261,#24262,#24263,#24264,#24265,#24266,#24267,#24268,
#24269),.UNSPECIFIED.,.F.,.F.,(4,3,3,3,3,3,3,3,3,3,3,3,3,3,3,3,3,3,3,3,
3,3,3,3,3,3,3,3,3,3,3,4),(0.,0.0327225146876364,0.0662805432171355,0.10053700758566,
0.133256717128334,0.138569294358745,0.143645923792125,0.178633902850418,
0.21408079528951,0.251134267448895,0.278924371568434,0.28555899152832,0.321777086502174,
0.357762762756158,0.36229468392705,0.397656570072467,0.419708592270616,
0.427246251204994,0.432639262274467,0.468078659615991,0.504737305906693,
0.541740900625277,0.567834403702473,0.579481664146009,0.584481366534682,
0.622063534445468,0.654169882144813,0.668576745773135,0.678363380045444,
0.716158278526066,0.750488925242846,0.768398079192654),.UNSPECIFIED.);
#646=B_SPLINE_CURVE_WITH_KNOTS('',3,(#24270,#24271,#24272,#24273,#24274,
#24275,#24276,#24277,#24278,#24279,#24280,#24281,#24282,#24283,#24284,#24285,
#24286,#24287,#24288,#24289,#24290,#24291,#24292,#24293,#24294),
 .UNSPECIFIED.,.F.,.F.,(4,3,3,3,3,3,3,3,4),(7.59274844815667,7.89168714724002,
8.87814804064502,9.86460893405002,10.851069827455,11.83753072086,12.823991614265,
13.81045250767,13.8759337553363),.UNSPECIFIED.);
#647=B_SPLINE_CURVE_WITH_KNOTS('',3,(#24322,#24323,#24324,#24325,#24326,
#24327,#24328,#24329,#24330,#24331),.UNSPECIFIED.,.F.,.F.,(4,3,3,4),(-4.09293042013064,
-3.99338989784634,-2.99504242338475,-2.06863817490912),.UNSPECIFIED.);
#648=B_SPLINE_CURVE_WITH_KNOTS('',3,(#24334,#24335,#24336,#24337,#24338,
#24339,#24340),.UNSPECIFIED.,.F.,.F.,(4,3,4),(0.,0.998805711569778,1.11730040836826),
 .UNSPECIFIED.);
#649=B_SPLINE_CURVE_WITH_KNOTS('',3,(#24345,#24346,#24347,#24348,#24349,
#24350,#24351,#24352,#24353,#24354,#24355,#24356,#24357,#24358,#24359,#24360,
#24361,#24362,#24363,#24364,#24365,#24366),.UNSPECIFIED.,.F.,.F.,(4,3,3,
3,3,3,3,4),(-10.3761157273102,-9.98347474461585,-8.98512727015427,-7.98677979569268,
-6.98843232123109,-5.99008484676951,-4.99173737230793,-4.09293042013064),
 .UNSPECIFIED.);
#650=B_SPLINE_CURVE_WITH_KNOTS('',3,(#24367,#24368,#24369,#24370,#24371,
#24372,#24373,#24374,#24375,#24376,#24377,#24378,#24379,#24380,#24381,#24382,
#24383,#24384,#24385,#24386,#24387,#24388),.UNSPECIFIED.,.F.,.F.,(4,3,3,
3,3,3,3,4),(1.11730040836826,1.99761142313956,2.99641713470934,3.99522284627912,
4.99402855784889,5.99283426941867,6.99163998098846,7.40048571554784),
 .UNSPECIFIED.);
#651=B_SPLINE_CURVE_WITH_KNOTS('',3,(#24393,#24394,#24395,#24396,#24397,
#24398,#24399,#24400,#24401,#24402,#24403,#24404,#24405,#24406,#24407,#24408,
#24409,#24410,#24411,#24412,#24413,#24414),.UNSPECIFIED.,.F.,.F.,(4,3,3,
3,3,3,3,4),(-16.6593010344898,-15.9735595913854,-14.9752121169238,-13.9768646424622,
-12.9785171680006,-11.980169693539,-10.9818222190774,-10.3761157273102),
 .UNSPECIFIED.);
#652=B_SPLINE_CURVE_WITH_KNOTS('',3,(#24415,#24416,#24417,#24418,#24419,
#24420,#24421,#24422,#24423,#24424,#24425,#24426,#24427,#24428,#24429,#24430,
#24431,#24432,#24433,#24434,#24435,#24436),.UNSPECIFIED.,.F.,.F.,(4,3,3,
3,3,3,3,4),(7.40048571554784,7.99044569255823,8.989251404128,9.98805711569777,
10.9868628272675,11.9856685388373,12.9844742504071,13.6836710227274),
 .UNSPECIFIED.);
#653=B_SPLINE_CURVE_WITH_KNOTS('',3,(#24441,#24442,#24443,#24444,#24445,
#24446,#24447,#24448,#24449,#24450,#24451,#24452,#24453,#24454,#24455,#24456,
#24457,#24458,#24459,#24460,#24461,#24462),.UNSPECIFIED.,.F.,.F.,(4,3,3,
3,3,3,3,4),(-22.9424863416694,-21.9636444381549,-20.9652969636933,-19.9669494892317,
-18.9686020147701,-17.9702545403085,-16.9719070658469,-16.6593010344898),
 .UNSPECIFIED.);
#654=B_SPLINE_CURVE_WITH_KNOTS('',3,(#24463,#24464,#24465,#24466,#24467,
#24468,#24469,#24470,#24471,#24472,#24473,#24474,#24475,#24476,#24477,#24478,
#24479,#24480,#24481,#24482,#24483,#24484),.UNSPECIFIED.,.F.,.F.,(4,3,3,
3,3,3,3,4),(13.6836710227274,13.9832799619769,14.9820856735466,15.9808913851164,
16.9796970966862,17.978502808256,18.9773085198257,19.966856329907),
 .UNSPECIFIED.);
#655=B_SPLINE_CURVE_WITH_KNOTS('',3,(#24489,#24490,#24491,#24492,#24493,
#24494,#24495,#24496,#24497,#24498,#24499,#24500,#24501,#24502,#24503,#24504,
#24505,#24506,#24507,#24508,#24509,#24510,#24511,#24512,#24513),
 .UNSPECIFIED.,.F.,.F.,(4,3,3,3,3,3,3,3,4),(-29.225671648849,-28.952076759386,
-27.9537292849244,-26.9553818104628,-25.9570343360012,-24.9586868615396,
-23.960339387078,-22.9619919126165,-22.9424863416694),.UNSPECIFIED.);
#656=B_SPLINE_CURVE_WITH_KNOTS('',3,(#24514,#24515,#24516,#24517,#24518,
#24519,#24520,#24521,#24522,#24523,#24524,#24525,#24526,#24527,#24528,#24529,
#24530,#24531,#24532,#24533,#24534,#24535,#24536,#24537,#24538),
 .UNSPECIFIED.,.F.,.F.,(4,3,3,3,3,3,3,3,4),(19.966856329907,19.9761142313955,
20.9749199429653,21.9737256545351,22.9725313661048,23.9713370776746,24.9701427892444,
25.9689485008142,26.2500416370866),.UNSPECIFIED.);
#657=B_SPLINE_CURVE_WITH_KNOTS('',3,(#24543,#24544,#24545,#24546,#24547,
#24548,#24549,#24550,#24551,#24552,#24553,#24554,#24555,#24556,#24557,#24558,
#24559,#24560,#24561,#24562,#24563,#24564),.UNSPECIFIED.,.F.,.F.,(4,3,3,
3,3,3,3,4),(-35.5088569560286,-34.9421616061555,-33.9438141316939,-32.9454666572323,
-31.9471191827707,-30.9487717083091,-29.9504242338475,-29.225671648849),
 .UNSPECIFIED.);
#658=B_SPLINE_CURVE_WITH_KNOTS('',3,(#24565,#24566,#24567,#24568,#24569,
#24570,#24571,#24572,#24573,#24574,#24575,#24576,#24577,#24578,#24579,#24580,
#24581,#24582,#24583,#24584,#24585,#24586),.UNSPECIFIED.,.F.,.F.,(4,3,3,
3,3,3,3,4),(26.2500416370866,26.9677542123839,27.9665599239537,28.9653656355235,
29.9641713470933,30.9629770586631,31.9617827702328,32.5332269442662),
 .UNSPECIFIED.);
#659=B_SPLINE_CURVE_WITH_KNOTS('',3,(#24591,#24592,#24593,#24594,#24595,
#24596,#24597,#24598,#24599,#24600,#24601,#24602,#24603,#24604,#24605,#24606,
#24607,#24608,#24609,#24610,#24611,#24612),.UNSPECIFIED.,.F.,.F.,(4,3,3,
3,3,3,3,4),(-41.7920422632082,-40.932246452925,-39.9338989784634,-38.9355515040018,
-37.9372040295402,-36.9388565550787,-35.9405090806171,-35.5088569560286),
 .UNSPECIFIED.);
#660=B_SPLINE_CURVE_WITH_KNOTS('',3,(#24613,#24614,#24615,#24616,#24617,
#24618,#24619,#24620,#24621,#24622,#24623,#24624,#24625,#24626,#24627,#24628,
#24629,#24630,#24631,#24632,#24633,#24634),.UNSPECIFIED.,.F.,.F.,(4,3,3,
3,3,3,3,4),(32.5332269442662,32.9605884818026,33.9593941933724,34.9581999049422,
35.9570056165119,36.9558113280817,37.9546170396515,38.8164122514458),
 .UNSPECIFIED.);
#661=B_SPLINE_CURVE_WITH_KNOTS('',3,(#24639,#24640,#24641,#24642,#24643,
#24644,#24645,#24646,#24647,#24648,#24649,#24650,#24651,#24652,#24653,#24654,
#24655,#24656,#24657,#24658,#24659,#24660,#24661,#24662,#24663),
 .UNSPECIFIED.,.F.,.F.,(4,3,3,3,3,3,3,3,4),(-48.0752275703878,-47.9206787741561,
-46.9223312996945,-45.9239838252329,-44.9256363507713,-43.9272888763097,
-42.9289414018482,-41.9305939273866,-41.7920422632082),.UNSPECIFIED.);
#662=B_SPLINE_CURVE_WITH_KNOTS('',3,(#24664,#24665,#24666,#24667,#24668,
#24669,#24670,#24671,#24672,#24673,#24674,#24675,#24676,#24677,#24678,#24679,
#24680,#24681,#24682,#24683,#24684,#24685,#24686,#24687,#24688),
 .UNSPECIFIED.,.F.,.F.,(4,3,3,3,3,3,3,3,4),(38.8164122514458,38.9534227512213,
39.952228462791,40.9510341743608,41.9498398859306,42.9486455975004,43.9474513090701,
44.9462570206399,45.0995975586254),.UNSPECIFIED.);
#663=B_SPLINE_CURVE_WITH_KNOTS('',3,(#24693,#24694,#24695,#24696,#24697,
#24698,#24699,#24700,#24701,#24702,#24703,#24704,#24705,#24706,#24707,#24708,
#24709,#24710,#24711,#24712,#24713,#24714),.UNSPECIFIED.,.F.,.F.,(4,3,3,
3,3,3,3,4),(-54.3584128775673,-53.9107636209256,-52.912416146464,-51.9140686720024,
-50.9157211975408,-49.9173737230793,-48.9190262486177,-48.0752275703878),
 .UNSPECIFIED.);
#664=B_SPLINE_CURVE_WITH_KNOTS('',3,(#24715,#24716,#24717,#24718,#24719,
#24720,#24721,#24722,#24723,#24724,#24725,#24726,#24727,#24728,#24729,#24730,
#24731,#24732,#24733,#24734,#24735,#24736),.UNSPECIFIED.,.F.,.F.,(4,3,3,
3,3,3,3,4),(45.0995975586254,45.9450627322097,46.9438684437795,47.9426741553493,
48.941479866919,49.9402855784888,50.9390912900586,51.382782865805),
 .UNSPECIFIED.);
#665=B_SPLINE_CURVE_WITH_KNOTS('',3,(#24741,#24742,#24743,#24744,#24745,
#24746,#24747,#24748,#24749,#24750,#24751,#24752,#24753,#24754,#24755,#24756,
#24757,#24758,#24759,#24760,#24761,#24762),.UNSPECIFIED.,.F.,.F.,(4,3,3,
3,3,3,3,4),(-60.6415981847469,-59.9008484676951,-58.9025009932335,-57.9041535187719,
-56.9058060443103,-55.9074585698488,-54.9091110953872,-54.3584128775673),
 .UNSPECIFIED.);
#666=B_SPLINE_CURVE_WITH_KNOTS('',3,(#24763,#24764,#24765,#24766,#24767,
#24768,#24769,#24770,#24771,#24772,#24773,#24774,#24775,#24776,#24777,#24778,
#24779,#24780,#24781,#24782,#24783,#24784),.UNSPECIFIED.,.F.,.F.,(4,3,3,
3,3,3,3,4),(51.382782865805,51.9378970016283,52.9367027131981,53.9355084247679,
54.9343141363377,55.9331198479074,56.9319255594772,57.6659681729846),
 .UNSPECIFIED.);
#667=B_SPLINE_CURVE_WITH_KNOTS('',3,(#24789,#24790,#24791,#24792,#24793,
#24794,#24795,#24796,#24797,#24798,#24799,#24800,#24801,#24802,#24803,#24804,
#24805,#24806,#24807,#24808,#24809,#24810,#24811,#24812,#24813),
 .UNSPECIFIED.,.F.,.F.,(4,3,3,3,3,3,3,3,4),(-66.9247834919265,-66.8892807889262,
-65.8909333144646,-64.892585840003,-63.8942383655414,-62.8958908910799,
-61.8975434166182,-60.8991959421567,-60.6415981847469),.UNSPECIFIED.);
#668=B_SPLINE_CURVE_WITH_KNOTS('',3,(#24814,#24815,#24816,#24817,#24818,
#24819,#24820,#24821,#24822,#24823,#24824,#24825,#24826,#24827,#24828,#24829,
#24830,#24831,#24832,#24833,#24834,#24835,#24836,#24837,#24838),
 .UNSPECIFIED.,.F.,.F.,(4,3,3,3,3,3,3,3,4),(57.6659681729846,57.930731271047,
58.9295369826168,59.9283426941866,60.9271484057563,61.9259541173261,62.9247598288959,
63.9235655404657,63.9491534801642),.UNSPECIFIED.);
#669=B_SPLINE_CURVE_WITH_KNOTS('',3,(#24843,#24844,#24845,#24846,#24847,
#24848,#24849,#24850,#24851,#24852,#24853,#24854,#24855,#24856,#24857,#24858,
#24859,#24860,#24861,#24862,#24863,#24864),.UNSPECIFIED.,.F.,.F.,(4,3,3,
3,3,3,3,4),(-73.2079687991061,-72.8793656356957,-71.8810181612341,-70.8826706867726,
-69.8843232123109,-68.8859757378494,-67.8876282633878,-66.9247834919265),
 .UNSPECIFIED.);
#670=B_SPLINE_CURVE_WITH_KNOTS('',3,(#24865,#24866,#24867,#24868,#24869,
#24870,#24871,#24872,#24873,#24874,#24875,#24876,#24877,#24878,#24879,#24880,
#24881,#24882,#24883,#24884,#24885,#24886),.UNSPECIFIED.,.F.,.F.,(4,3,3,
3,3,3,3,4),(63.9491534801642,64.9223712520354,65.9211769636052,66.919982675175,
67.9187883867447,68.9175940983145,69.9163998098843,70.2323387873437),
 .UNSPECIFIED.);
#671=B_SPLINE_CURVE_WITH_KNOTS('',3,(#24891,#24892,#24893,#24894,#24895,
#24896,#24897,#24898,#24899,#24900,#24901,#24902,#24903,#24904,#24905,#24906,
#24907,#24908,#24909,#24910,#24911,#24912),.UNSPECIFIED.,.F.,.F.,(4,3,3,
3,3,3,3,4),(-79.4911541062857,-78.8694504824652,-77.8711030080036,-76.8727555335421,
-75.8744080590805,-74.8760605846189,-73.8777131101573,-73.2079687991061),
 .UNSPECIFIED.);
#672=B_SPLINE_CURVE_WITH_KNOTS('',3,(#24913,#24914,#24915,#24916,#24917,
#24918,#24919,#24920,#24921,#24922,#24923,#24924,#24925,#24926,#24927,#24928,
#24929,#24930,#24931,#24932,#24933,#24934),.UNSPECIFIED.,.F.,.F.,(4,3,3,
3,3,3,3,4),(70.2323387873437,70.9152055214541,71.9140112330238,72.9128169445936,
73.9116226561634,74.9104283677332,75.909234079303,76.5155240945233),
 .UNSPECIFIED.);
#673=B_SPLINE_CURVE_WITH_KNOTS('',3,(#24939,#24940,#24941,#24942,#24943,
#24944,#24945,#24946,#24947,#24948,#24949,#24950,#24951,#24952,#24953,#24954,
#24955,#24956,#24957,#24958,#24959,#24960),.UNSPECIFIED.,.F.,.F.,(4,3,3,
3,3,3,3,4),(-85.7743394134653,-84.8595353292348,-83.8611878547731,-82.8628403803116,
-81.86449290585,-80.8661454313884,-79.8677979569268,-79.4911541062857),
 .UNSPECIFIED.);
#674=B_SPLINE_CURVE_WITH_KNOTS('',3,(#24961,#24962,#24963,#24964,#24965,
#24966,#24967,#24968,#24969,#24970,#24971,#24972,#24973,#24974,#24975,#24976,
#24977,#24978,#24979,#24980,#24981,#24982),.UNSPECIFIED.,.F.,.F.,(4,3,3,
3,3,3,3,4),(76.5155240945233,76.9080397908727,77.9068455024425,78.9056512140123,
79.9044569255821,80.9032626371518,81.9020683487216,82.7987094017029),
 .UNSPECIFIED.);
#675=B_SPLINE_CURVE_WITH_KNOTS('',3,(#24987,#24988,#24989,#24990,#24991,
#24992,#24993,#24994,#24995,#24996,#24997,#24998,#24999,#25000,#25001,#25002,
#25003,#25004,#25005,#25006,#25007,#25008,#25009,#25010,#25011),
 .UNSPECIFIED.,.F.,.F.,(4,3,3,3,3,3,3,3,4),(-92.0575247206449,-91.8479676504658,
-90.8496201760042,-89.8512727015427,-88.8529252270811,-87.8545777526195,
-86.8562302781579,-85.8578828036963,-85.7743394134653),.UNSPECIFIED.);
#676=B_SPLINE_CURVE_WITH_KNOTS('',3,(#25012,#25013,#25014,#25015,#25016,
#25017,#25018,#25019,#25020,#25021,#25022,#25023,#25024,#25025,#25026,#25027,
#25028,#25029,#25030,#25031,#25032,#25033,#25034,#25035,#25036),
 .UNSPECIFIED.,.F.,.F.,(4,3,3,3,3,3,3,3,4),(82.7987094017029,82.9008740602914,
83.8996797718612,84.8984854834309,85.8972911950007,86.8960969065705,87.8949026181403,
88.8937083297101,89.0818947088825),.UNSPECIFIED.);
#677=B_SPLINE_CURVE_WITH_KNOTS('',3,(#25041,#25042,#25043,#25044,#25045,
#25046,#25047,#25048,#25049,#25050,#25051,#25052,#25053,#25054,#25055,#25056,
#25057,#25058,#25059,#25060,#25061,#25062),.UNSPECIFIED.,.F.,.F.,(4,3,3,
3,3,3,3,4),(-98.3407100278245,-97.8380524972353,-96.8397050227737,-95.8413575483122,
-94.8430100738506,-93.844662599389,-92.8463151249274,-92.0575247206449),
 .UNSPECIFIED.);
#678=B_SPLINE_CURVE_WITH_KNOTS('',3,(#25063,#25064,#25065,#25066,#25067,
#25068,#25069,#25070,#25071,#25072,#25073,#25074,#25075,#25076,#25077,#25078,
#25079,#25080,#25081,#25082,#25083,#25084),.UNSPECIFIED.,.F.,.F.,(4,3,3,
3,3,3,3,4),(89.0818947088825,89.8925140412798,90.8913197528496,91.8901254644194,
92.8889311759891,93.8877368875589,94.8865425991287,95.3650800160621),
 .UNSPECIFIED.);
#679=B_SPLINE_CURVE_WITH_KNOTS('',3,(#25089,#25090,#25091,#25092,#25093,
#25094,#25095,#25096,#25097,#25098,#25099,#25100,#25101,#25102,#25103,#25104,
#25105,#25106,#25107,#25108,#25109,#25110),.UNSPECIFIED.,.F.,.F.,(4,3,3,
3,3,3,3,4),(-104.623895335004,-103.828137344005,-102.829789869543,-101.831442395082,
-100.83309492062,-99.8347474461585,-98.8363999716969,-98.3407100278245),
 .UNSPECIFIED.);
#680=B_SPLINE_CURVE_WITH_KNOTS('',3,(#25111,#25112,#25113,#25114,#25115,
#25116,#25117,#25118,#25119,#25120,#25121,#25122,#25123,#25124,#25125,#25126,
#25127,#25128,#25129,#25130,#25131,#25132),.UNSPECIFIED.,.F.,.F.,(4,3,3,
3,3,3,3,4),(95.3650800160621,95.8853483106984,96.8841540222682,97.882959733838,
98.8817654454078,99.8805711569776,100.879376868547,101.648265323242),
 .UNSPECIFIED.);
#681=B_SPLINE_CURVE_WITH_KNOTS('',3,(#25137,#25138,#25139,#25140,#25141,
#25142,#25143,#25144,#25145,#25146,#25147,#25148,#25149,#25150,#25151,#25152,
#25153,#25154,#25155,#25156,#25157,#25158,#25159,#25160,#25161),
 .UNSPECIFIED.,.F.,.F.,(4,3,3,3,3,3,3,3,4),(-110.907080642184,-110.816569665236,
-109.818222190774,-108.819874716313,-107.821527241851,-106.82317976739,
-105.824832292928,-104.826484818466,-104.623895335004),.UNSPECIFIED.);
#682=B_SPLINE_CURVE_WITH_KNOTS('',3,(#25162,#25163,#25164,#25165,#25166,
#25167,#25168,#25169,#25170,#25171,#25172,#25173,#25174,#25175,#25176,#25177,
#25178,#25179,#25180,#25181,#25182,#25183,#25184,#25185,#25186),
 .UNSPECIFIED.,.F.,.F.,(4,3,3,3,3,3,3,3,4),(101.648265323242,101.878182580117,
102.876988291687,103.875794003257,104.874599714826,105.873405426396,106.872211137966,
107.871016849536,107.931450630421),.UNSPECIFIED.);
#683=B_SPLINE_CURVE_WITH_KNOTS('',3,(#25191,#25192,#25193,#25194,#25195,
#25196,#25197,#25198,#25199,#25200,#25201,#25202,#25203,#25204,#25205,#25206,
#25207,#25208,#25209,#25210,#25211,#25212),.UNSPECIFIED.,.F.,.F.,(4,3,3,
3,3,3,3,4),(-117.190265949363,-116.806654512005,-115.808307037544,-114.809959563082,
-113.811612088621,-112.813264614159,-111.814917139698,-110.907080642184),
 .UNSPECIFIED.);
#684=B_SPLINE_CURVE_WITH_KNOTS('',3,(#25213,#25214,#25215,#25216,#25217,
#25218,#25219,#25220,#25221,#25222,#25223,#25224,#25225,#25226,#25227,#25228,
#25229,#25230,#25231,#25232,#25233,#25234),.UNSPECIFIED.,.F.,.F.,(4,3,3,
3,3,3,3,4),(107.931450630421,108.869822561106,109.868628272675,110.867433984245,
111.866239695815,112.865045407385,113.863851118954,114.214635937601),
 .UNSPECIFIED.);
#685=B_SPLINE_CURVE_WITH_KNOTS('',3,(#25239,#25240,#25241,#25242,#25243,
#25244,#25245,#25246,#25247,#25248,#25249,#25250,#25251,#25252,#25253,#25254,
#25255,#25256,#25257,#25258,#25259,#25260),.UNSPECIFIED.,.F.,.F.,(4,3,3,
3,3,3,3,4),(-123.473451256543,-122.796739358775,-121.798391884313,-120.800044409852,
-119.80169693539,-118.803349460929,-117.805001986467,-117.190265949363),
 .UNSPECIFIED.);
#686=B_SPLINE_CURVE_WITH_KNOTS('',3,(#25261,#25262,#25263,#25264,#25265,
#25266,#25267,#25268,#25269,#25270,#25271,#25272,#25273,#25274,#25275,#25276,
#25277,#25278,#25279,#25280,#25281,#25282),.UNSPECIFIED.,.F.,.F.,(4,3,3,
3,3,3,3,4),(114.214635937601,114.862656830524,115.861462542094,116.860268253664,
117.859073965234,118.857879676803,119.856685388373,120.49782124478),
 .UNSPECIFIED.);
#687=B_SPLINE_CURVE_WITH_KNOTS('',3,(#25287,#25288,#25289,#25290,#25291,
#25292,#25293,#25294,#25295,#25296,#25297,#25298,#25299,#25300,#25301,#25302,
#25303,#25304,#25305,#25306,#25307,#25308),.UNSPECIFIED.,.F.,.F.,(4,3,3,
3,3,3,3,4),(-129.756636563722,-128.786824205544,-127.788476731083,-126.790129256621,
-125.79178178216,-124.793434307698,-123.795086833237,-123.473451256543),
 .UNSPECIFIED.);
#688=B_SPLINE_CURVE_WITH_KNOTS('',3,(#25309,#25310,#25311,#25312,#25313,
#25314,#25315,#25316,#25317,#25318,#25319,#25320,#25321,#25322,#25323,#25324,
#25325,#25326,#25327,#25328,#25329,#25330),.UNSPECIFIED.,.F.,.F.,(4,3,3,
3,3,3,3,4),(120.49782124478,120.855491099943,121.854296811513,122.853102523082,
123.851908234652,124.850713946222,125.849519657792,126.78100655196),
 .UNSPECIFIED.);
#689=B_SPLINE_CURVE_WITH_KNOTS('',3,(#25335,#25336,#25337,#25338,#25339,
#25340,#25341,#25342,#25343,#25344,#25345,#25346,#25347,#25348,#25349,#25350,
#25351,#25352,#25353,#25354,#25355,#25356,#25357,#25358,#25359),
 .UNSPECIFIED.,.F.,.F.,(4,3,3,3,3,3,3,3,4),(-136.039821870902,-135.775256526776,
-134.776909052314,-133.778561577852,-132.780214103391,-131.781866628929,
-130.783519154468,-129.785171680006,-129.756636563722),.UNSPECIFIED.);
#690=B_SPLINE_CURVE_WITH_KNOTS('',3,(#25360,#25361,#25362,#25363,#25364,
#25365,#25366,#25367,#25368,#25369,#25370,#25371,#25372,#25373,#25374,#25375,
#25376,#25377,#25378,#25379,#25380,#25381,#25382,#25383,#25384),
 .UNSPECIFIED.,.F.,.F.,(4,3,3,3,3,3,3,3,4),(126.78100655196,126.848325369362,
127.847131080931,128.845936792501,129.844742504071,130.843548215641,131.84235392721,
132.84115963878,133.06419185914),.UNSPECIFIED.);
#691=B_SPLINE_CURVE_WITH_KNOTS('',3,(#25389,#25390,#25391,#25392,#25393,
#25394,#25395,#25396,#25397,#25398,#25399,#25400,#25401,#25402,#25403,#25404,
#25405,#25406,#25407,#25408,#25409,#25410),.UNSPECIFIED.,.F.,.F.,(4,3,3,
3,3,3,3,4),(-142.323007178082,-141.765341373545,-140.766993899083,-139.768646424622,
-138.77029895016,-137.771951475699,-136.773604001237,-136.039821870902),
 .UNSPECIFIED.);
#692=B_SPLINE_CURVE_WITH_KNOTS('',3,(#25411,#25412,#25413,#25414,#25415,
#25416,#25417,#25418,#25419,#25420,#25421,#25422,#25423,#25424,#25425,#25426,
#25427,#25428,#25429,#25430,#25431,#25432),.UNSPECIFIED.,.F.,.F.,(4,3,3,
3,3,3,3,4),(133.06419185914,133.83996535035,134.83877106192,135.83757677349,
136.836382485059,137.835188196629,138.833993908199,139.347377166319),
 .UNSPECIFIED.);
#693=B_SPLINE_CURVE_WITH_KNOTS('',3,(#25437,#25438,#25439,#25440,#25441,
#25442,#25443,#25444,#25445,#25446,#25447,#25448,#25449,#25450,#25451,#25452,
#25453,#25454,#25455,#25456,#25457,#25458),.UNSPECIFIED.,.F.,.F.,(4,3,3,
3,3,3,3,4),(-148.606192485261,-147.755426220315,-146.757078745853,-145.758731271391,
-144.76038379693,-143.762036322468,-142.763688848007,-142.323007178082),
 .UNSPECIFIED.);
#694=B_SPLINE_CURVE_WITH_KNOTS('',3,(#25459,#25460,#25461,#25462,#25463,
#25464,#25465,#25466,#25467,#25468,#25469,#25470,#25471,#25472,#25473,#25474,
#25475,#25476,#25477,#25478,#25479,#25480),.UNSPECIFIED.,.F.,.F.,(4,3,3,
3,3,3,3,4),(139.347377166319,139.832799619769,140.831605331338,141.830411042908,
142.829216754478,143.828022466048,144.826828177618,145.630562473499),
 .UNSPECIFIED.);
#695=B_SPLINE_CURVE_WITH_KNOTS('',3,(#25486,#25487,#25488,#25489,#25490,
#25491,#25492,#25493,#25494,#25495),.UNSPECIFIED.,.F.,.F.,(4,1,1,1,1,1,
1,4),(160.221225333079,160.368806542595,161.367154017056,162.365501491518,
163.363848965979,164.362196440441,165.360543914902,166.358891389364),
 .UNSPECIFIED.);
#696=B_SPLINE_CURVE_WITH_KNOTS('',3,(#25498,#25499,#25500,#25501,#25502,
#25503,#25504,#25505),.UNSPECIFIED.,.F.,.F.,(4,1,1,1,1,4),(160.221225333079,
161.124751422577,162.123557134147,163.122362845716,164.121168557286,165.119974268856),
 .UNSPECIFIED.);
#697=B_SPLINE_CURVE_WITH_KNOTS('',3,(#25510,#25511,#25512,#25513,#25514,
#25515,#25516,#25517,#25518,#25519),.UNSPECIFIED.,.F.,.F.,(4,1,1,1,1,1,
1,4),(153.9380400259,154.378721695825,155.377069170287,156.375416644748,
157.37376411921,158.372111593671,159.370459068133,160.221225333079),
 .UNSPECIFIED.);
#698=B_SPLINE_CURVE_WITH_KNOTS('',3,(#25520,#25521,#25522,#25523,#25524,
#25525,#25526,#25527,#25528,#25529,#25530),.UNSPECIFIED.,.F.,.F.,(4,1,1,
1,1,1,1,1,4),(153.9380400259,154.133111441588,155.131917153158,156.130722864728,
157.129528576298,158.128334287868,159.127139999437,160.125945711007,160.221225333079),
 .UNSPECIFIED.);
#699=B_SPLINE_CURVE_WITH_KNOTS('',3,(#25535,#25536,#25537,#25538,#25539,
#25540,#25541,#25542,#25543,#25544),.UNSPECIFIED.,.F.,.F.,(4,1,1,1,1,1,
1,4),(147.65485471872,148.388636849056,149.386984323517,150.385331797979,
151.38367927244,152.382026746902,153.380374221363,153.9380400259),
 .UNSPECIFIED.);
#700=B_SPLINE_CURVE_WITH_KNOTS('',3,(#25545,#25546,#25547,#25548,#25549,
#25550,#25551,#25552,#25553,#25554),.UNSPECIFIED.,.F.,.F.,(4,1,1,1,1,1,
1,4),(147.65485471872,148.14027717217,149.13908288374,150.137888595309,
151.136694306879,152.135500018449,153.134305730019,153.9380400259),
 .UNSPECIFIED.);
#701=B_SPLINE_CURVE_WITH_KNOTS('',3,(#25559,#25560,#25561,#25562,#25563,
#25564,#25565,#25566,#25567,#25568,#25569),.UNSPECIFIED.,.F.,.F.,(4,1,1,
1,1,1,1,1,4),(141.371669411541,141.400204527824,142.398552002286,143.396899476748,
144.395246951209,145.393594425671,146.391941900132,147.390289374594,147.65485471872),
 .UNSPECIFIED.);
#702=B_SPLINE_CURVE_WITH_KNOTS('',3,(#25570,#25571,#25572,#25573,#25574,
#25575,#25576,#25577,#25578,#25579),.UNSPECIFIED.,.F.,.F.,(4,1,1,1,1,1,
1,4),(141.371669411541,142.147442902751,143.146248614321,144.145054325891,
145.14386003746,146.14266574903,147.1414714606,147.65485471872),
 .UNSPECIFIED.);
#703=B_SPLINE_CURVE_WITH_KNOTS('',3,(#25584,#25585,#25586,#25587,#25588,
#25589,#25590,#25591,#25592,#25593),.UNSPECIFIED.,.F.,.F.,(4,1,1,1,1,1,
1,4),(135.088484104361,135.410119681055,136.408467155516,137.406814629978,
138.40516210444,139.403509578901,140.401857053363,141.371669411541),
 .UNSPECIFIED.);
#704=B_SPLINE_CURVE_WITH_KNOTS('',3,(#25594,#25595,#25596,#25597,#25598,
#25599,#25600,#25601,#25602,#25603,#25604),.UNSPECIFIED.,.F.,.F.,(4,1,1,
1,1,1,1,1,4),(135.088484104361,135.155802921763,136.154608633332,137.153414344902,
138.152220056472,139.151025768042,140.149831479612,141.148637191181,141.371669411541),
 .UNSPECIFIED.);
#705=B_SPLINE_CURVE_WITH_KNOTS('',3,(#25609,#25610,#25611,#25612,#25613,
#25614,#25615,#25616,#25617,#25618),.UNSPECIFIED.,.F.,.F.,(4,1,1,1,1,1,
1,4),(128.805298797182,129.420034834285,130.418382308747,131.416729783209,
132.41507725767,133.413424732132,134.411772206593,135.088484104361),
 .UNSPECIFIED.);
#706=B_SPLINE_CURVE_WITH_KNOTS('',3,(#25619,#25620,#25621,#25622,#25623,
#25624,#25625,#25626,#25627,#25628),.UNSPECIFIED.,.F.,.F.,(4,1,1,1,1,1,
1,4),(128.805298797182,129.162968652344,130.161774363914,131.160580075484,
132.159385787053,133.158191498623,134.156997210193,135.088484104361),
 .UNSPECIFIED.);
#707=B_SPLINE_CURVE_WITH_KNOTS('',3,(#25633,#25634,#25635,#25636,#25637,
#25638,#25639,#25640,#25641,#25642),.UNSPECIFIED.,.F.,.F.,(4,1,1,1,1,1,
1,4),(122.522113490002,123.429949987516,124.428297461977,125.426644936439,
126.424992410901,127.423339885362,128.421687359824,128.805298797182),
 .UNSPECIFIED.);
#708=B_SPLINE_CURVE_WITH_KNOTS('',3,(#25643,#25644,#25645,#25646,#25647,
#25648,#25649,#25650,#25651,#25652),.UNSPECIFIED.,.F.,.F.,(4,1,1,1,1,1,
1,4),(122.522113490002,123.170134382925,124.168940094495,125.167745806065,
126.166551517635,127.165357229204,128.164162940774,128.805298797182),
 .UNSPECIFIED.);
#709=B_SPLINE_CURVE_WITH_KNOTS('',3,(#25657,#25658,#25659,#25660,#25661,
#25662,#25663,#25664,#25665,#25666,#25667),.UNSPECIFIED.,.F.,.F.,(4,1,1,
1,1,1,1,1,4),(116.238928182822,116.441517666285,117.439865140746,118.438212615208,
119.43656008967,120.434907564131,121.433255038593,122.431602513054,122.522113490002),
 .UNSPECIFIED.);
#710=B_SPLINE_CURVE_WITH_KNOTS('',3,(#25668,#25669,#25670,#25671,#25672,
#25673,#25674,#25675,#25676,#25677),.UNSPECIFIED.,.F.,.F.,(4,1,1,1,1,1,
1,4),(116.238928182822,117.177300113507,118.176105825076,119.174911536646,
120.173717248216,121.172522959786,122.171328671356,122.522113490002),
 .UNSPECIFIED.);
#711=B_SPLINE_CURVE_WITH_KNOTS('',3,(#25682,#25683,#25684,#25685,#25686,
#25687,#25688,#25689,#25690,#25691),.UNSPECIFIED.,.F.,.F.,(4,1,1,1,1,1,
1,4),(109.955742875643,110.451432819515,111.449780293977,112.448127768438,
113.4464752429,114.444822717362,115.443170191823,116.238928182822),
 .UNSPECIFIED.);
#712=B_SPLINE_CURVE_WITH_KNOTS('',3,(#25692,#25693,#25694,#25695,#25696,
#25697,#25698,#25699,#25700,#25701,#25702),.UNSPECIFIED.,.F.,.F.,(4,1,1,
1,1,1,1,1,4),(109.955742875643,110.185660132518,111.184465844088,112.183271555658,
113.182077267228,114.180882978797,115.179688690367,116.178494401937,116.238928182822),
 .UNSPECIFIED.);
#713=B_SPLINE_CURVE_WITH_KNOTS('',3,(#25707,#25708,#25709,#25710,#25711,
#25712,#25713,#25714,#25715,#25716),.UNSPECIFIED.,.F.,.F.,(4,1,1,1,1,1,
1,4),(103.672557568463,104.461347972746,105.459695447207,106.458042921669,
107.456390396131,108.454737870592,109.453085345054,109.955742875643),
 .UNSPECIFIED.);
#714=B_SPLINE_CURVE_WITH_KNOTS('',3,(#25717,#25718,#25719,#25720,#25721,
#25722,#25723,#25724,#25725,#25726),.UNSPECIFIED.,.F.,.F.,(4,1,1,1,1,1,
1,4),(103.672557568463,104.1928258631,105.191631574669,106.190437286239,
107.189242997809,108.188048709379,109.186854420948,109.955742875643),
 .UNSPECIFIED.);
#715=B_SPLINE_CURVE_WITH_KNOTS('',3,(#25731,#25732,#25733,#25734,#25735,
#25736,#25737,#25738,#25739,#25740,#25741),.UNSPECIFIED.,.F.,.F.,(4,1,1,
1,1,1,1,1,4),(97.3893722612837,97.4729156515147,98.4712631259763,99.4696106004379,
100.467958074899,101.466305549361,102.464653023823,103.463000498284,103.672557568463),
 .UNSPECIFIED.);
#716=B_SPLINE_CURVE_WITH_KNOTS('',3,(#25742,#25743,#25744,#25745,#25746,
#25747,#25748,#25749,#25750,#25751),.UNSPECIFIED.,.F.,.F.,(4,1,1,1,1,1,
1,4),(97.3893722612837,98.199991593681,99.1987973052507,100.197603016821,
101.19640872839,102.19521443996,103.19402015153,103.672557568463),
 .UNSPECIFIED.);
#717=B_SPLINE_CURVE_WITH_KNOTS('',3,(#25756,#25757,#25758,#25759,#25760,
#25761,#25762,#25763,#25764,#25765),.UNSPECIFIED.,.F.,.F.,(4,1,1,1,1,1,
1,4),(91.1061869541041,91.4828308047452,92.4811782792068,93.4795257536684,
94.4778732281299,95.4762207025915,96.4745681770531,97.3893722612837),
 .UNSPECIFIED.);
#718=B_SPLINE_CURVE_WITH_KNOTS('',3,(#25766,#25767,#25768,#25769,#25770,
#25771,#25772,#25773,#25774,#25775,#25776),.UNSPECIFIED.,.F.,.F.,(4,1,1,
1,1,1,1,1,4),(91.1061869541041,91.2083516126925,92.2071573242623,93.2059630358321,
94.2047687474019,95.2035744589716,96.2023801705414,97.2011858821112,97.3893722612837),
 .UNSPECIFIED.);
#719=B_SPLINE_CURVE_WITH_KNOTS('',3,(#25781,#25782,#25783,#25784,#25785,
#25786,#25787,#25788,#25789,#25790),.UNSPECIFIED.,.F.,.F.,(4,1,1,1,1,1,
1,4),(84.8230016469245,85.4927459579757,86.4910934324373,87.4894409068988,
88.4877883813604,89.486135855822,90.4844833302836,91.1061869541041),
 .UNSPECIFIED.);
#720=B_SPLINE_CURVE_WITH_KNOTS('',3,(#25791,#25792,#25793,#25794,#25795,
#25796,#25797,#25798,#25799,#25800),.UNSPECIFIED.,.F.,.F.,(4,1,1,1,1,1,
1,4),(84.8230016469245,85.2155173432739,86.2143230548436,87.2131287664134,
88.2119344779832,89.210740189553,90.2095459011228,91.1061869541041),
 .UNSPECIFIED.);
#721=B_SPLINE_CURVE_WITH_KNOTS('',3,(#25805,#25806,#25807,#25808,#25809,
#25810,#25811,#25812,#25813,#25814),.UNSPECIFIED.,.F.,.F.,(4,1,1,1,1,1,
1,4),(78.5398163397449,79.5026611112062,80.5010085856677,81.4993560601293,
82.4977035345909,83.4960510090525,84.4943984835141,84.8230016469245),
 .UNSPECIFIED.);
#722=B_SPLINE_CURVE_WITH_KNOTS('',3,(#25815,#25816,#25817,#25818,#25819,
#25820,#25821,#25822,#25823,#25824),.UNSPECIFIED.,.F.,.F.,(4,1,1,1,1,1,
1,4),(78.5398163397449,79.2226830738552,80.221488785425,81.2202944969948,
82.2191002085646,83.2179059201343,84.2167116317041,84.8230016469245),
 .UNSPECIFIED.);
#723=B_SPLINE_CURVE_WITH_KNOTS('',3,(#25829,#25830,#25831,#25832,#25833,
#25834,#25835,#25836,#25837,#25838,#25839),.UNSPECIFIED.,.F.,.F.,(4,1,1,
1,1,1,1,1,4),(72.2566310325653,72.5142287899751,73.5125762644366,74.5109237388982,
75.5092712133598,76.5076186878214,77.505966162283,78.5043136367446,78.5398163397449),
 .UNSPECIFIED.);
#724=B_SPLINE_CURVE_WITH_KNOTS('',3,(#25840,#25841,#25842,#25843,#25844,
#25845,#25846,#25847,#25848,#25849),.UNSPECIFIED.,.F.,.F.,(4,1,1,1,1,1,
1,4),(72.2566310325653,73.2298488044366,74.2286545160063,75.2274602275761,
76.2262659391459,77.2250716507157,78.2238773622854,78.5398163397449),
 .UNSPECIFIED.);
#725=B_SPLINE_CURVE_WITH_KNOTS('',3,(#25854,#25855,#25856,#25857,#25858,
#25859,#25860,#25861,#25862,#25863),.UNSPECIFIED.,.F.,.F.,(4,1,1,1,1,1,
1,4),(65.9734457253857,66.5241439432056,67.5224914176671,68.5208388921287,
69.5191863665903,70.5175338410519,71.5158813155135,72.2566310325653),
 .UNSPECIFIED.);
#726=B_SPLINE_CURVE_WITH_KNOTS('',3,(#25864,#25865,#25866,#25867,#25868,
#25869,#25870,#25871,#25872,#25873,#25874),.UNSPECIFIED.,.F.,.F.,(4,1,1,
1,1,1,1,1,4),(65.9734457253857,66.2382088234481,67.2370145350179,68.2358202465877,
69.2346259581575,70.2334316697272,71.232237381297,72.2310430928668,72.2566310325653),
 .UNSPECIFIED.);
#727=B_SPLINE_CURVE_WITH_KNOTS('',3,(#25879,#25880,#25881,#25882,#25883,
#25884,#25885,#25886,#25887,#25888),.UNSPECIFIED.,.F.,.F.,(4,1,1,1,1,1,
1,4),(59.6902604182061,60.534059096436,61.5324065708976,62.5307540453592,
63.5291015198208,64.5274489942824,65.525796468744,65.9734457253857),
 .UNSPECIFIED.);
#728=B_SPLINE_CURVE_WITH_KNOTS('',3,(#25889,#25890,#25891,#25892,#25893,
#25894,#25895,#25896,#25897,#25898),.UNSPECIFIED.,.F.,.F.,(4,1,1,1,1,1,
1,4),(59.6902604182061,60.2453745540295,61.2441802655993,62.242985977169,
63.2417916887388,64.2405974003086,65.2394031118784,65.9734457253857),
 .UNSPECIFIED.);
#729=B_SPLINE_CURVE_WITH_KNOTS('',3,(#25903,#25904,#25905,#25906,#25907,
#25908,#25909,#25910,#25911,#25912,#25913),.UNSPECIFIED.,.F.,.F.,(4,1,1,
1,1,1,1,1,4),(53.4070751110265,53.545626775205,54.5439742496665,55.5423217241281,
56.5406691985897,57.5390166730513,58.5373641475129,59.5357116219745,59.6902604182061),
 .UNSPECIFIED.);
#730=B_SPLINE_CURVE_WITH_KNOTS('',3,(#25914,#25915,#25916,#25917,#25918,
#25919,#25920,#25921,#25922,#25923),.UNSPECIFIED.,.F.,.F.,(4,1,1,1,1,1,
1,4),(53.4070751110265,54.2525402846108,55.2513459961806,56.2501517077504,
57.2489574193202,58.2477631308899,59.2465688424597,59.6902604182061),
 .UNSPECIFIED.);
#731=B_SPLINE_CURVE_WITH_KNOTS('',3,(#25928,#25929,#25930,#25931,#25932,
#25933,#25934,#25935,#25936,#25937),.UNSPECIFIED.,.F.,.F.,(4,1,1,1,1,1,
1,4),(47.1238898038469,47.5555419284354,48.553889402897,49.5522368773586,
50.5505843518202,51.5489318262818,52.5472793007434,53.4070751110265),
 .UNSPECIFIED.);
#732=B_SPLINE_CURVE_WITH_KNOTS('',3,(#25938,#25939,#25940,#25941,#25942,
#25943,#25944,#25945,#25946,#25947,#25948),.UNSPECIFIED.,.F.,.F.,(4,1,1,
1,1,1,1,1,4),(47.1238898038469,47.2609003036224,48.2597060151922,49.258511726762,
50.2573174383317,51.2561231499015,52.2549288614713,53.2537345730411,53.4070751110265),
 .UNSPECIFIED.);
#733=B_SPLINE_CURVE_WITH_KNOTS('',3,(#25953,#25954,#25955,#25956,#25957,
#25958,#25959,#25960,#25961,#25962),.UNSPECIFIED.,.F.,.F.,(4,1,1,1,1,1,
1,4),(40.8407044966673,41.5654570816659,42.5638045561275,43.5621520305891,
44.5604995050507,45.5588469795123,46.5571944539738,47.1238898038469),
 .UNSPECIFIED.);
#734=B_SPLINE_CURVE_WITH_KNOTS('',3,(#25963,#25964,#25965,#25966,#25967,
#25968,#25969,#25970,#25971,#25972),.UNSPECIFIED.,.F.,.F.,(4,1,1,1,1,1,
1,4),(40.8407044966673,41.2680660342037,42.2668717457735,43.2656774573433,
44.2644831689131,45.2632888804829,46.2620945920526,47.1238898038469),
 .UNSPECIFIED.);
#735=B_SPLINE_CURVE_WITH_KNOTS('',3,(#25977,#25978,#25979,#25980,#25981,
#25982,#25983,#25984,#25985,#25986,#25987),.UNSPECIFIED.,.F.,.F.,(4,1,1,
1,1,1,1,1,4),(34.5575191894877,34.5770247604348,35.5753722348964,36.573719709358,
37.5720671838196,38.5704146582812,39.5687621327428,40.5671096072043,40.8407044966673),
 .UNSPECIFIED.);
#736=B_SPLINE_CURVE_WITH_KNOTS('',3,(#25988,#25989,#25990,#25991,#25992,
#25993,#25994,#25995,#25996,#25997),.UNSPECIFIED.,.F.,.F.,(4,1,1,1,1,1,
1,4),(34.5575191894877,35.2752317647851,36.2740374763549,37.2728431879246,
38.2716488994944,39.2704546110642,40.269260322634,40.8407044966673),
 .UNSPECIFIED.);
#737=B_SPLINE_CURVE_WITH_KNOTS('',3,(#26002,#26003,#26004,#26005,#26006,
#26007,#26008,#26009,#26010,#26011),.UNSPECIFIED.,.F.,.F.,(4,1,1,1,1,1,
1,4),(28.2743338823082,28.5869399136653,29.5852873881269,30.5836348625885,
31.5819823370501,32.5803298115117,33.5786772859732,34.5575191894877),
 .UNSPECIFIED.);
#738=B_SPLINE_CURVE_WITH_KNOTS('',3,(#26012,#26013,#26014,#26015,#26016,
#26017,#26018,#26019,#26020,#26021,#26022),.UNSPECIFIED.,.F.,.F.,(4,1,1,
1,1,1,1,1,4),(28.2743338823082,28.2835917837967,29.2823974953664,30.2812032069362,
31.280008918506,32.2788146300758,33.2776203416455,34.2764260532153,34.5575191894877),
 .UNSPECIFIED.);
#739=B_SPLINE_CURVE_WITH_KNOTS('',3,(#26027,#26028,#26029,#26030,#26031,
#26032,#26033,#26034,#26035,#26036),.UNSPECIFIED.,.F.,.F.,(4,1,1,1,1,1,
1,4),(21.9911485751286,22.5968550668958,23.5952025413574,24.593550015819,
25.5918974902806,26.5902449647422,27.5885924392037,28.2743338823082),
 .UNSPECIFIED.);
#740=B_SPLINE_CURVE_WITH_KNOTS('',3,(#26037,#26038,#26039,#26040,#26041,
#26042,#26043,#26044,#26045,#26046),.UNSPECIFIED.,.F.,.F.,(4,1,1,1,1,1,
1,4),(21.9911485751286,22.290757514378,23.2895632259478,24.2883689375176,
25.2871746490873,26.2859803606571,27.2847860722269,28.2743338823082),
 .UNSPECIFIED.);
#741=B_SPLINE_CURVE_WITH_KNOTS('',3,(#26051,#26052,#26053,#26054,#26055,
#26056,#26057,#26058,#26059,#26060),.UNSPECIFIED.,.F.,.F.,(4,1,1,1,1,1,
1,4),(15.707963267949,16.6067702201263,17.6051176945879,18.6034651690495,
19.6018126435111,20.6001601179726,21.5985075924342,21.9911485751286),
 .UNSPECIFIED.);
#742=B_SPLINE_CURVE_WITH_KNOTS('',3,(#26061,#26062,#26063,#26064,#26065,
#26066,#26067,#26068,#26069,#26070),.UNSPECIFIED.,.F.,.F.,(4,1,1,1,1,1,
1,4),(15.707963267949,16.2979232449593,17.2967289565291,18.2955346680989,
19.2943403796687,20.2931460912385,21.2919518028082,21.9911485751286),
 .UNSPECIFIED.);
#743=B_SPLINE_CURVE_WITH_KNOTS('',3,(#26073,#26074,#26075,#26076,#26077,
#26078,#26079,#26080,#26081,#26082,#26083,#26084,#26085,#26086,#26087,#26088,
#26089,#26090,#26091,#26092,#26093,#26094,#26095,#26096,#26097,#26098,#26099,
#26100,#26101,#26102,#26103,#26104,#26105,#26106,#26107,#26108,#26109,#26110,
#26111,#26112,#26113,#26114,#26115,#26116,#26117,#26118,#26119,#26120,#26121,
#26122,#26123,#26124,#26125,#26126,#26127,#26128,#26129,#26130,#26131,#26132,
#26133,#26134,#26135,#26136,#26137,#26138,#26139,#26140,#26141,#26142,#26143,
#26144,#26145,#26146,#26147,#26148,#26149,#26150,#26151,#26152,#26153,#26154,
#26155,#26156,#26157,#26158,#26159,#26160,#26161,#26162,#26163,#26164,#26165,
#26166,#26167,#26168,#26169,#26170,#26171,#26172,#26173,#26174,#26175,#26176,
#26177,#26178,#26179,#26180,#26181,#26182,#26183,#26184,#26185,#26186,#26187,
#26188,#26189,#26190,#26191,#26192,#26193,#26194,#26195,#26196,#26197,#26198,
#26199,#26200,#26201,#26202,#26203,#26204,#26205,#26206,#26207,#26208,#26209,
#26210,#26211,#26212,#26213,#26214,#26215,#26216,#26217,#26218,#26219,#26220,
#26221,#26222,#26223,#26224,#26225,#26226,#26227,#26228,#26229,#26230,#26231,
#26232,#26233,#26234,#26235,#26236,#26237,#26238,#26239,#26240,#26241,#26242,
#26243,#26244,#26245,#26246,#26247,#26248,#26249,#26250,#26251,#26252,#26253,
#26254,#26255,#26256,#26257,#26258,#26259,#26260,#26261,#26262,#26263,#26264,
#26265,#26266,#26267,#26268,#26269,#26270,#26271,#26272,#26273,#26274,#26275,
#26276,#26277,#26278,#26279,#26280,#26281,#26282,#26283,#26284,#26285,#26286,
#26287,#26288,#26289,#26290,#26291,#26292,#26293,#26294,#26295,#26296,#26297,
#26298,#26299,#26300,#26301,#26302,#26303,#26304),.UNSPECIFIED.,.F.,.F.,
(4,3,3,3,3,3,3,3,3,3,3,3,3,3,3,3,3,3,3,3,3,3,3,3,3,3,3,3,3,3,3,3,3,3,3,
3,3,3,3,3,3,3,3,3,3,3,3,3,3,3,3,3,3,3,3,3,3,3,3,3,3,3,3,3,3,3,3,3,3,3,3,
3,3,3,3,3,3,4),(-2.07787844821581,-2.04563640817454,-2.01260600406739,-1.99390262471517,
-1.97880815407869,-1.97343611688677,-1.93978265453417,-1.90587423526444,
-1.88438455677208,-1.87589993511254,-1.87071648916707,-1.83652656870669,
-1.80253536734925,-1.7682460873374,-1.75110144733148,-1.74333138277347,
-1.73705920337893,-1.73395680732556,-1.70122489773177,-1.66760788468754,
-1.63163034935991,-1.61589017765406,-1.60492981834386,-1.60020318232811,
-1.56577415958123,-1.53098947454713,-1.49635100238812,-1.4672101523077,
-1.46216466120046,-1.42716054566692,-1.39267814268788,-1.37978760206645,
-1.34531390132733,-1.33245646351828,-1.32592267957129,-1.32082668753048,
-1.28679878189102,-1.2516716099619,-1.21635641577775,-1.19129075085948,
-1.18499879133774,-1.18014246087519,-1.1446795062145,-1.10922024591651,
-1.07424600071327,-1.04503854857244,-1.03811338002803,-1.0158310964316,
-0.981392848951218,-0.946133107350497,-0.910369520876374,-0.899628872347486,
-0.89368994999567,-0.857962841308724,-0.82181130706931,-0.785718553763474,
-0.767732714465289,-0.754402261382112,-0.748013249342093,-0.711600160631613,
-0.675777877337977,-0.641831839377992,-0.620163722971144,-0.609175591942721,
-0.603763283335243,-0.56872451739821,-0.532416642828612,-0.495724942594248,
-0.470652071878519,-0.458093605572563,-0.451831603827856,-0.415093157349795,
-0.378123471546787,-0.341518871530435,-0.318330424199427,-0.308274893383926,
-0.301672805800084,-0.295141976868419),.UNSPECIFIED.);
#744=B_SPLINE_CURVE_WITH_KNOTS('',3,(#26306,#26307,#26308,#26309,#26310,
#26311,#26312,#26313,#26314,#26315,#26316,#26317,#26318,#26319,#26320,#26321,
#26322,#26323,#26324,#26325,#26326,#26327,#26328,#26329,#26330,#26331,#26332,
#26333,#26334,#26335,#26336,#26337,#26338,#26339,#26340,#26341,#26342,#26343,
#26344,#26345,#26346,#26347,#26348,#26349,#26350,#26351,#26352,#26353,#26354,
#26355,#26356,#26357,#26358,#26359,#26360,#26361,#26362,#26363,#26364,#26365,
#26366,#26367,#26368,#26369,#26370,#26371,#26372),.UNSPECIFIED.,.F.,.F.,
(4,3,3,3,3,3,3,3,3,3,3,3,3,3,3,3,3,3,3,3,3,3,4),(-0.560387248253829,-0.523489675423405,
-0.486909280826814,-0.451409765500931,-0.428581929912694,-0.422644096024468,
-0.417538776764712,-0.382486843658728,-0.360098423147984,-0.324342694600126,
-0.288456460870319,-0.277039646852259,-0.272658549855339,-0.23782854730266,
-0.202954723102529,-0.168490668078001,-0.147429334568251,-0.135539740506508,
-0.130645012249701,-0.0971180289394068,-0.0640503905793665,-0.0319885771286076,
0.),.UNSPECIFIED.);
#745=B_SPLINE_CURVE_WITH_KNOTS('',3,(#26375,#26376,#26377,#26378,#26379,
#26380,#26381,#26382,#26383,#26384,#26385,#26386,#26387,#26388,#26389,#26390,
#26391,#26392,#26393,#26394,#26395,#26396,#26397,#26398,#26399,#26400,#26401,
#26402,#26403,#26404,#26405),.UNSPECIFIED.,.F.,.F.,(4,3,3,3,3,3,3,3,3,3,
4),(-0.295141976868419,-0.258118008913044,-0.221832521729933,-0.184905796964689,
-0.161792572344103,-0.155196944416255,-0.149950158553442,-0.112462618915081,
-0.0749997768837546,-0.0374998884418773,0.),.UNSPECIFIED.);
#746=B_SPLINE_CURVE_WITH_KNOTS('',3,(#27042,#27043,#27044,#27045,#27046,
#27047,#27048,#27049),.UNSPECIFIED.,.F.,.F.,(4,1,1,1,1,4),(11.6150328478184,
12.61338032228,13.6117277967416,14.6100752712031,15.6084227456647,15.707963267949),
 .UNSPECIFIED.);
#747=B_SPLINE_CURVE_WITH_KNOTS('',3,(#27050,#27051,#27052,#27053,#27054,
#27055,#27056,#27057,#27058,#27059,#27060,#27061,#27062,#27063,#27064,#27065,
#27066,#27067,#27068,#27069,#27070,#27071,#27072,#27073,#27074,#27075,#27076,
#27077,#27078,#27079,#27080,#27081,#27082,#27083,#27084,#27085,#27086,#27087,
#27088,#27089,#27090,#27091,#27092,#27093,#27094,#27095,#27096,#27097,#27098,
#27099,#27100,#27101,#27102,#27103,#27104,#27105,#27106,#27107,#27108,#27109,
#27110,#27111,#27112,#27113,#27114,#27115,#27116,#27117,#27118,#27119,#27120,
#27121,#27122,#27123,#27124,#27125,#27126,#27127,#27128,#27129,#27130,#27131,
#27132,#27133,#27134,#27135,#27136,#27137,#27138,#27139,#27140,#27141,#27142,
#27143,#27144,#27145,#27146),.UNSPECIFIED.,.F.,.F.,(4,3,3,3,3,3,3,3,3,3,
3,3,3,3,3,3,3,3,3,3,3,3,3,3,3,3,3,3,3,3,3,3,4),(-0.75940314415766,-0.731099230044352,
-0.694405090916541,-0.673021753795954,-0.659792230351525,-0.653579099280099,
-0.615915673993481,-0.58296017686769,-0.568542146875157,-0.56016187063185,
-0.554528541316208,-0.518574457756444,-0.482794928028838,-0.44802285832865,
-0.424085067993276,-0.41225754927003,-0.407433722504049,-0.373002009397425,
-0.352271696987154,-0.317344582417244,-0.282174956583422,-0.274866834214802,
-0.269904808501567,-0.23562822660491,-0.201185303792214,-0.167047167238569,
-0.146166271333748,-0.135071182701311,-0.130169248221992,-0.0967451917617864,
-0.0637506042838665,-0.03178494031496,0.),.UNSPECIFIED.);
#748=B_SPLINE_CURVE_WITH_KNOTS('',3,(#27147,#27148,#27149,#27150,#27151,
#27152,#27153,#27154,#27155,#27156,#27157,#27158,#27159,#27160,#27161,#27162,
#27163,#27164,#27165),.UNSPECIFIED.,.F.,.F.,(4,3,3,3,3,3,4),(-153.229510295036,
-152.747163592623,-151.748816118161,-150.750468643699,-149.752121169238,
-148.753773694776,-148.606192485261),.UNSPECIFIED.);
#749=B_SPLINE_CURVE_WITH_KNOTS('',3,(#27168,#27169,#27170,#27171,#27172,
#27173,#27174,#27175,#27176),.UNSPECIFIED.,.F.,.F.,(4,1,1,1,1,1,4),(10.3761157273103,
11.3038946871105,12.3027003986802,13.30150611025,14.3003118218198,15.2991175333896,
15.707963267949),.UNSPECIFIED.);
#750=B_SPLINE_CURVE_WITH_KNOTS('',3,(#27818,#27819,#27820,#27821,#27822,
#27823,#27824,#27825,#27826,#27827,#27828,#27829,#27830,#27831,#27832,#27833,
#27834,#27835,#27836,#27837,#27838,#27839),.UNSPECIFIED.,.F.,.F.,(4,3,3,
3,3,3,3,4),(145.630562473499,145.825633889187,146.824439600757,147.823245312327,
148.822051023897,149.820856735466,150.819662447036,151.160872120127),
 .UNSPECIFIED.);
#751=B_SPLINE_CURVE_WITH_KNOTS('',3,(#27840,#27841,#27842,#27843,#27844,
#27845,#27846,#27847,#27848,#27849,#27850,#27851,#27852,#27853,#27854,#27855,
#27856,#27857,#27858,#27859,#27860,#27861,#27862,#27863,#27864,#27865,#27866,
#27867,#27868,#27869,#27870,#27871,#27872,#27873,#27874,#27875,#27876,#27877,
#27878,#27879,#27880,#27881,#27882,#27883,#27884,#27885,#27886,#27887,#27888,
#27889,#27890,#27891,#27892,#27893,#27894,#27895,#27896,#27897,#27898,#27899,
#27900,#27901,#27902,#27903,#27904,#27905,#27906,#27907,#27908,#27909,#27910,
#27911,#27912,#27913,#27914,#27915,#27916,#27917,#27918,#27919,#27920,#27921,
#27922,#27923,#27924,#27925,#27926,#27927,#27928,#27929,#27930,#27931,#27932,
#27933,#27934,#27935,#27936),.UNSPECIFIED.,.F.,.F.,(4,3,3,3,3,3,3,3,3,3,
3,3,3,3,3,3,3,3,3,3,3,3,3,3,3,3,3,3,3,3,3,3,4),(-0.761903739928579,-0.737714840814909,
-0.705408016786385,-0.685226614670373,-0.676627161339419,-0.668738660960247,
-0.635678094311993,-0.604031530389268,-0.590186158673076,-0.583843379993958,
-0.578312161070379,-0.543995147795815,-0.509206617715678,-0.474634013675463,
-0.451601905989146,-0.445054542245308,-0.439067220218037,-0.403526955466083,
-0.382505582930195,-0.348068670802762,-0.312989133154698,-0.301425205487243,
-0.296110141258073,-0.261171717718659,-0.225140081955213,-0.188826370911274,
-0.165223074547365,-0.15245028863213,-0.147771515823046,-0.110734161208511,
-0.0736990584503352,-0.0368495292251676,0.),.UNSPECIFIED.);
#752=B_SPLINE_CURVE_WITH_KNOTS('',3,(#28046,#28047,#28048,#28049,#28050,
#28051,#28052),.UNSPECIFIED.,.F.,.F.,(4,3,4),(158.388651680658,158.598858328231,
159.096033432709),.UNSPECIFIED.);
#753=B_SPLINE_CURVE_WITH_KNOTS('',3,(#28060,#28061,#28062,#28063,#28064,
#28065,#28066,#28067,#28068,#28069,#28070,#28071,#28072,#28073,#28074,#28075),
 .UNSPECIFIED.,.F.,.F.,(4,3,3,3,3,4),(-157.079632679489,-156.610157910323,
-156.112982805845,-155.615807701368,-155.118632596891,-154.645421777951),
 .UNSPECIFIED.);
#754=B_SPLINE_CURVE_WITH_KNOTS('',3,(#28080,#28081,#28082,#28083,#28084,
#28085,#28086,#28087,#28088,#28089,#28090,#28091,#28092,#28093,#28094,#28095,
#28096,#28097,#28098,#28099,#28100,#28101,#28102,#28103,#28104,#28105,#28106,
#28107,#28108,#28109,#28110,#28111,#28112,#28113,#28114,#28115,#28116,#28117,
#28118,#28119,#28120,#28121,#28122),.UNSPECIFIED.,.F.,.F.,(4,3,3,3,3,3,
3,3,3,3,3,3,3,3,4),(152.105466373478,152.135581970028,152.632757074505,
153.129932178982,153.627107283459,154.124282387936,154.621457492414,155.118632596891,
155.615807701368,156.112982805845,156.610157910323,157.1073330148,157.604508119277,
158.101683223754,158.388651680658),.UNSPECIFIED.);
#755=B_SPLINE_CURVE_WITH_KNOTS('',3,(#28123,#28124,#28125,#28126,#28127,
#28128,#28129,#28130,#28131,#28132,#28133,#28134,#28135,#28136,#28137,#28138,
#28139,#28140,#28141,#28142,#28143,#28144,#28145,#28146,#28147,#28148,#28149,
#28150,#28151,#28152,#28153,#28154,#28155,#28156,#28157,#28158,#28159,#28160,
#28161,#28162,#28163,#28164,#28165),.UNSPECIFIED.,.F.,.F.,(4,3,3,3,3,3,
3,3,3,3,3,3,3,3,4),(-154.645421777951,-154.621457492414,-154.124282387936,
-153.627107283459,-153.129932178982,-152.632757074505,-152.135581970028,
-151.63840686555,-151.141231761073,-150.644056656596,-150.146881552119,
-149.649706447642,-149.152531343164,-148.655356238687,-148.362236470772),
 .UNSPECIFIED.);
#756=B_SPLINE_CURVE_WITH_KNOTS('',3,(#28170,#28171,#28172,#28173,#28174,
#28175,#28176,#28177,#28178,#28179,#28180,#28181,#28182,#28183,#28184,#28185,
#28186,#28187,#28188,#28189,#28190,#28191,#28192,#28193,#28194,#28195,#28196,
#28197,#28198,#28199,#28200,#28201,#28202,#28203,#28204,#28205,#28206,#28207,
#28208,#28209),.UNSPECIFIED.,.F.,.F.,(4,3,3,3,3,3,3,3,3,3,3,3,3,4),(145.822281066299,
146.169480716301,146.666655820778,147.163830925255,147.661006029733,148.15818113421,
148.655356238687,149.152531343164,149.649706447642,150.146881552119,150.644056656596,
151.141231761073,151.63840686555,152.105466373478),.UNSPECIFIED.);
#757=B_SPLINE_CURVE_WITH_KNOTS('',3,(#28210,#28211,#28212,#28213,#28214,
#28215,#28216,#28217,#28218,#28219,#28220,#28221,#28222,#28223,#28224,#28225,
#28226,#28227,#28228,#28229,#28230,#28231,#28232,#28233,#28234,#28235,#28236,
#28237,#28238,#28239,#28240,#28241,#28242,#28243,#28244,#28245,#28246,#28247,
#28248,#28249,#28250,#28251,#28252),.UNSPECIFIED.,.F.,.F.,(4,3,3,3,3,3,
3,3,3,3,3,3,3,3,4),(-148.362236470772,-148.15818113421,-147.661006029733,
-147.163830925255,-146.666655820778,-146.169480716301,-145.672305611824,
-145.175130507347,-144.677955402869,-144.180780298392,-143.683605193915,
-143.186430089438,-142.689254984961,-142.192079880483,-142.079051163592),
 .UNSPECIFIED.);
#758=B_SPLINE_CURVE_WITH_KNOTS('',3,(#28257,#28258,#28259,#28260,#28261,
#28262,#28263,#28264,#28265,#28266,#28267,#28268,#28269,#28270,#28271,#28272,
#28273,#28274,#28275,#28276,#28277,#28278,#28279,#28280,#28281,#28282,#28283,
#28284,#28285,#28286,#28287,#28288,#28289,#28290,#28291,#28292,#28293,#28294,
#28295,#28296,#28297,#28298,#28299),.UNSPECIFIED.,.F.,.F.,(4,3,3,3,3,3,
3,3,3,3,3,3,3,3,4),(139.539095759119,139.706204358097,140.203379462574,
140.700554567052,141.197729671529,141.694904776006,142.192079880483,142.689254984961,
143.186430089438,143.683605193915,144.180780298392,144.677955402869,145.175130507347,
145.672305611824,145.822281066299),.UNSPECIFIED.);
#759=B_SPLINE_CURVE_WITH_KNOTS('',3,(#28300,#28301,#28302,#28303,#28304,
#28305,#28306,#28307,#28308,#28309,#28310,#28311,#28312,#28313,#28314,#28315,
#28316,#28317,#28318,#28319,#28320,#28321,#28322,#28323,#28324,#28325,#28326,
#28327,#28328,#28329,#28330,#28331,#28332,#28333,#28334,#28335,#28336,#28337,
#28338,#28339),.UNSPECIFIED.,.F.,.F.,(4,3,3,3,3,3,3,3,3,3,3,3,3,4),(-142.079051163592,
-141.694904776006,-141.197729671529,-140.700554567052,-140.203379462574,
-139.706204358097,-139.20902925362,-138.711854149143,-138.214679044666,
-137.717503940188,-137.220328835711,-136.723153731234,-136.225978626757,
-135.795865856412),.UNSPECIFIED.);
#760=B_SPLINE_CURVE_WITH_KNOTS('',3,(#28344,#28345,#28346,#28347,#28348,
#28349,#28350,#28351,#28352,#28353,#28354,#28355,#28356,#28357,#28358,#28359,
#28360,#28361,#28362,#28363,#28364,#28365,#28366,#28367,#28368,#28369,#28370,
#28371,#28372,#28373,#28374,#28375,#28376,#28377,#28378,#28379,#28380,#28381,
#28382,#28383),.UNSPECIFIED.,.F.,.F.,(4,3,3,3,3,3,3,3,3,3,3,3,3,4),(133.255910451939,
133.740103104371,134.237278208848,134.734453313325,135.231628417802,135.72880352228,
136.225978626757,136.723153731234,137.220328835711,137.717503940188,138.214679044666,
138.711854149143,139.20902925362,139.539095759119),.UNSPECIFIED.);
#761=B_SPLINE_CURVE_WITH_KNOTS('',3,(#28384,#28385,#28386,#28387,#28388,
#28389,#28390,#28391,#28392,#28393,#28394,#28395,#28396,#28397,#28398,#28399,
#28400,#28401,#28402,#28403,#28404,#28405,#28406,#28407,#28408,#28409,#28410,
#28411,#28412,#28413,#28414,#28415,#28416,#28417,#28418,#28419,#28420,#28421,
#28422,#28423,#28424,#28425,#28426),.UNSPECIFIED.,.F.,.F.,(4,3,3,3,3,3,
3,3,3,3,3,3,3,3,4),(-135.795865856412,-135.72880352228,-135.231628417802,
-134.734453313325,-134.237278208848,-133.740103104371,-133.242927999893,
-132.745752895416,-132.248577790939,-131.751402686462,-131.254227581985,
-130.757052477507,-130.25987737303,-129.762702268553,-129.512680549233),
 .UNSPECIFIED.);
#762=B_SPLINE_CURVE_WITH_KNOTS('',3,(#28431,#28432,#28433,#28434,#28435,
#28436,#28437,#28438,#28439,#28440,#28441,#28442,#28443,#28444,#28445,#28446,
#28447,#28448,#28449,#28450,#28451,#28452,#28453,#28454,#28455,#28456,#28457,
#28458,#28459,#28460,#28461,#28462,#28463,#28464,#28465,#28466,#28467,#28468,
#28469,#28470,#28471,#28472,#28473),.UNSPECIFIED.,.F.,.F.,(4,3,3,3,3,3,
3,3,3,3,3,3,3,3,4),(126.97272514476,127.276826746167,127.774001850644,128.271176955121,
128.768352059598,129.265527164076,129.762702268553,130.25987737303,130.757052477507,
131.254227581985,131.751402686462,132.248577790939,132.745752895416,133.242927999893,
133.255910451939),.UNSPECIFIED.);
#763=B_SPLINE_CURVE_WITH_KNOTS('',3,(#28474,#28475,#28476,#28477,#28478,
#28479,#28480,#28481,#28482,#28483,#28484,#28485,#28486,#28487,#28488,#28489,
#28490,#28491,#28492,#28493,#28494,#28495,#28496,#28497,#28498,#28499,#28500,
#28501,#28502,#28503,#28504,#28505,#28506,#28507,#28508,#28509,#28510,#28511,
#28512,#28513,#28514,#28515,#28516),.UNSPECIFIED.,.F.,.F.,(4,3,3,3,3,3,
3,3,3,3,3,3,3,3,4),(-129.512680549233,-129.265527164076,-128.768352059599,
-128.271176955121,-127.774001850644,-127.276826746167,-126.77965164169,
-126.282476537213,-125.785301432735,-125.288126328258,-124.790951223781,
-124.293776119304,-123.796601014826,-123.299425910349,-123.229495242054),
 .UNSPECIFIED.);
#764=B_SPLINE_CURVE_WITH_KNOTS('',3,(#28521,#28522,#28523,#28524,#28525,
#28526,#28527,#28528,#28529,#28530,#28531,#28532,#28533,#28534,#28535,#28536,
#28537,#28538,#28539,#28540,#28541,#28542,#28543,#28544,#28545,#28546,#28547,
#28548,#28549,#28550,#28551,#28552,#28553,#28554,#28555,#28556,#28557,#28558,
#28559,#28560,#28561,#28562,#28563),.UNSPECIFIED.,.F.,.F.,(4,3,3,3,3,3,
3,3,3,3,3,3,3,3,4),(120.68953983758,120.813550387963,121.31072549244,121.807900596918,
122.305075701395,122.802250805872,123.299425910349,123.796601014826,124.293776119304,
124.790951223781,125.288126328258,125.785301432735,126.282476537212,126.77965164169,
126.97272514476),.UNSPECIFIED.);
#765=B_SPLINE_CURVE_WITH_KNOTS('',3,(#28564,#28565,#28566,#28567,#28568,
#28569,#28570,#28571,#28572,#28573,#28574,#28575,#28576,#28577,#28578,#28579,
#28580,#28581,#28582,#28583,#28584,#28585,#28586,#28587,#28588,#28589,#28590,
#28591,#28592,#28593,#28594,#28595,#28596,#28597,#28598,#28599,#28600,#28601,
#28602,#28603),.UNSPECIFIED.,.F.,.F.,(4,3,3,3,3,3,3,3,3,3,3,3,3,4),(-123.229495242054,
-122.802250805872,-122.305075701395,-121.807900596918,-121.31072549244,
-120.813550387963,-120.316375283486,-119.819200179009,-119.322025074531,
-118.824849970054,-118.327674865577,-117.8304997611,-117.333324656623,-116.946309934874),
 .UNSPECIFIED.);
#766=B_SPLINE_CURVE_WITH_KNOTS('',3,(#28608,#28609,#28610,#28611,#28612,
#28613,#28614,#28615,#28616,#28617,#28618,#28619,#28620,#28621,#28622,#28623,
#28624,#28625,#28626,#28627,#28628,#28629,#28630,#28631,#28632,#28633,#28634,
#28635,#28636,#28637,#28638,#28639,#28640,#28641,#28642,#28643,#28644,#28645,
#28646,#28647),.UNSPECIFIED.,.F.,.F.,(4,3,3,3,3,3,3,3,3,3,3,3,3,4),(114.406354530401,
114.847449134237,115.344624238714,115.841799343191,116.338974447668,116.836149552145,
117.333324656623,117.8304997611,118.327674865577,118.824849970054,119.322025074531,
119.819200179009,120.316375283486,120.68953983758),.UNSPECIFIED.);
#767=B_SPLINE_CURVE_WITH_KNOTS('',3,(#28648,#28649,#28650,#28651,#28652,
#28653,#28654,#28655,#28656,#28657,#28658,#28659,#28660,#28661,#28662,#28663,
#28664,#28665,#28666,#28667,#28668,#28669,#28670,#28671,#28672,#28673,#28674,
#28675,#28676,#28677,#28678,#28679,#28680,#28681,#28682,#28683,#28684,#28685,
#28686,#28687,#28688,#28689,#28690),.UNSPECIFIED.,.F.,.F.,(4,3,3,3,3,3,
3,3,3,3,3,3,3,3,4),(-116.946309934874,-116.836149552145,-116.338974447668,
-115.841799343191,-115.344624238714,-114.847449134237,-114.350274029759,
-113.853098925282,-113.355923820805,-112.858748716328,-112.36157361185,
-111.864398507373,-111.367223402896,-110.870048298419,-110.663124627694),
 .UNSPECIFIED.);
#768=B_SPLINE_CURVE_WITH_KNOTS('',3,(#28695,#28696,#28697,#28698,#28699,
#28700,#28701,#28702,#28703,#28704,#28705,#28706,#28707,#28708,#28709,#28710,
#28711,#28712,#28713,#28714,#28715,#28716,#28717,#28718,#28719,#28720,#28721,
#28722,#28723,#28724,#28725,#28726,#28727,#28728,#28729,#28730,#28731,#28732,
#28733,#28734,#28735,#28736,#28737),.UNSPECIFIED.,.F.,.F.,(4,3,3,3,3,3,
3,3,3,3,3,3,3,3,4),(108.123169223221,108.384172776033,108.88134788051,109.378522984987,
109.875698089464,110.372873193942,110.870048298419,111.367223402896,111.864398507373,
112.36157361185,112.858748716328,113.355923820805,113.853098925282,114.350274029759,
114.406354530401),.UNSPECIFIED.);
#769=B_SPLINE_CURVE_WITH_KNOTS('',3,(#28738,#28739,#28740,#28741,#28742,
#28743,#28744,#28745,#28746,#28747,#28748,#28749,#28750,#28751,#28752,#28753,
#28754,#28755,#28756,#28757,#28758,#28759,#28760,#28761,#28762,#28763,#28764,
#28765,#28766,#28767,#28768,#28769,#28770,#28771,#28772,#28773,#28774,#28775,
#28776,#28777,#28778,#28779,#28780),.UNSPECIFIED.,.F.,.F.,(4,3,3,3,3,3,
3,3,3,3,3,3,3,3,4),(-110.663124627694,-110.372873193942,-109.875698089464,
-109.378522984987,-108.88134788051,-108.384172776033,-107.886997671556,
-107.389822567078,-106.892647462601,-106.395472358124,-105.898297253647,
-105.401122149169,-104.903947044692,-104.406771940215,-104.379939320514),
 .UNSPECIFIED.);
#770=B_SPLINE_CURVE_WITH_KNOTS('',3,(#28785,#28786,#28787,#28788,#28789,
#28790,#28791,#28792,#28793,#28794,#28795,#28796,#28797,#28798,#28799,#28800,
#28801,#28802,#28803,#28804,#28805,#28806,#28807,#28808,#28809,#28810,#28811,
#28812,#28813,#28814,#28815,#28816,#28817,#28818,#28819,#28820,#28821,#28822,
#28823,#28824,#28825,#28826,#28827),.UNSPECIFIED.,.F.,.F.,(4,3,3,3,3,3,
3,3,3,3,3,3,3,3,4),(101.839983916041,101.920896417829,102.418071522306,
102.915246626783,103.412421731261,103.909596835738,104.406771940215,104.903947044692,
105.401122149169,105.898297253647,106.395472358124,106.892647462601,107.389822567078,
107.886997671556,108.123169223221),.UNSPECIFIED.);
#771=B_SPLINE_CURVE_WITH_KNOTS('',3,(#28828,#28829,#28830,#28831,#28832,
#28833,#28834,#28835,#28836,#28837,#28838,#28839,#28840,#28841,#28842,#28843,
#28844,#28845,#28846,#28847,#28848,#28849,#28850,#28851,#28852,#28853,#28854,
#28855,#28856,#28857,#28858,#28859,#28860,#28861,#28862,#28863,#28864,#28865,
#28866,#28867),.UNSPECIFIED.,.F.,.F.,(4,3,3,3,3,3,3,3,3,3,3,3,3,4),(-104.379939320514,
-103.909596835738,-103.412421731261,-102.915246626783,-102.418071522306,
-101.920896417829,-101.423721313352,-100.926546208875,-100.429371104397,
-99.9321959999201,-99.4350208954429,-98.9378457909657,-98.4406706864885,
-98.0967540133348),.UNSPECIFIED.);
#772=B_SPLINE_CURVE_WITH_KNOTS('',3,(#28872,#28873,#28874,#28875,#28876,
#28877,#28878,#28879,#28880,#28881,#28882,#28883,#28884,#28885,#28886,#28887,
#28888,#28889,#28890,#28891,#28892,#28893,#28894,#28895,#28896,#28897,#28898,
#28899,#28900,#28901,#28902,#28903,#28904,#28905,#28906,#28907,#28908,#28909,
#28910,#28911),.UNSPECIFIED.,.F.,.F.,(4,3,3,3,3,3,3,3,3,3,3,3,3,4),(95.5567986088618,
95.9547951641024,96.4519702685796,96.9491453730568,97.446320477534,97.9434955820112,
98.4406706864884,98.9378457909657,99.4350208954429,99.9321959999201,100.429371104397,
100.926546208875,101.423721313352,101.839983916041),.UNSPECIFIED.);
#773=B_SPLINE_CURVE_WITH_KNOTS('',3,(#28912,#28913,#28914,#28915,#28916,
#28917,#28918,#28919,#28920,#28921,#28922,#28923,#28924,#28925,#28926,#28927,
#28928,#28929,#28930,#28931,#28932,#28933,#28934,#28935,#28936,#28937,#28938,
#28939,#28940,#28941,#28942,#28943,#28944,#28945,#28946,#28947,#28948,#28949,
#28950,#28951,#28952,#28953,#28954),.UNSPECIFIED.,.F.,.F.,(4,3,3,3,3,3,
3,3,3,3,3,3,3,3,4),(-98.0967540133348,-97.9434955820113,-97.446320477534,
-96.9491453730568,-96.4519702685796,-95.9547951641024,-95.4576200596252,
-94.960444955148,-94.4632698506707,-93.9660947461935,-93.4689196417163,
-92.9717445372391,-92.4745694327619,-91.9773943282847,-91.8135687061551),
 .UNSPECIFIED.);
#774=B_SPLINE_CURVE_WITH_KNOTS('',3,(#28959,#28960,#28961,#28962,#28963,
#28964,#28965,#28966,#28967,#28968,#28969,#28970,#28971,#28972,#28973,#28974,
#28975,#28976,#28977,#28978,#28979,#28980,#28981,#28982,#28983,#28984,#28985,
#28986,#28987,#28988,#28989,#28990,#28991,#28992,#28993,#28994,#28995,#28996,
#28997,#28998,#28999,#29000,#29001),.UNSPECIFIED.,.F.,.F.,(4,3,3,3,3,3,
3,3,3,3,3,3,3,3,4),(89.2736133016821,89.4915188058986,89.9886939103758,
90.485869014853,90.9830441193302,91.4802192238075,91.9773943282847,92.4745694327619,
92.9717445372391,93.4689196417163,93.9660947461935,94.4632698506707,94.9604449551479,
95.4576200596252,95.5567986088618),.UNSPECIFIED.);
#775=B_SPLINE_CURVE_WITH_KNOTS('',3,(#29002,#29003,#29004,#29005,#29006,
#29007,#29008,#29009,#29010,#29011,#29012,#29013,#29014,#29015,#29016,#29017,
#29018,#29019,#29020,#29021,#29022,#29023,#29024,#29025,#29026,#29027,#29028,
#29029,#29030,#29031,#29032,#29033,#29034,#29035,#29036,#29037,#29038,#29039,
#29040,#29041),.UNSPECIFIED.,.F.,.F.,(4,3,3,3,3,3,3,3,3,3,3,3,3,4),(-91.8135687061551,
-91.4802192238075,-90.9830441193302,-90.485869014853,-89.9886939103758,
-89.4915188058986,-88.9943437014214,-88.4971685969442,-87.9999934924669,
-87.5028183879897,-87.0056432835125,-86.5084681790353,-86.0112930745581,
-85.5303833989759),.UNSPECIFIED.);
#776=B_SPLINE_CURVE_WITH_KNOTS('',3,(#29046,#29047,#29048,#29049,#29050,
#29051,#29052,#29053,#29054,#29055,#29056,#29057,#29058,#29059,#29060,#29061,
#29062,#29063,#29064,#29065,#29066,#29067,#29068,#29069,#29070,#29071,#29072,
#29073,#29074,#29075,#29076,#29077,#29078,#29079,#29080,#29081,#29082,#29083,
#29084,#29085,#29086,#29087,#29088),.UNSPECIFIED.,.F.,.F.,(4,3,3,3,3,3,
3,3,3,3,3,3,3,3,4),(82.9904279945029,83.0282424476948,83.525417552172,84.0225926566493,
84.5197677611265,85.0169428656037,85.5141179700809,86.0112930745581,86.5084681790353,
87.0056432835125,87.5028183879897,87.9999934924669,88.4971685969441,88.9943437014214,
89.2736133016821),.UNSPECIFIED.);
#777=B_SPLINE_CURVE_WITH_KNOTS('',3,(#29089,#29090,#29091,#29092,#29093,
#29094,#29095,#29096,#29097,#29098,#29099,#29100,#29101,#29102,#29103,#29104,
#29105,#29106,#29107,#29108,#29109,#29110,#29111,#29112,#29113,#29114,#29115,
#29116,#29117,#29118,#29119,#29120,#29121,#29122,#29123,#29124,#29125,#29126,
#29127,#29128,#29129,#29130,#29131),.UNSPECIFIED.,.F.,.F.,(4,3,3,3,3,3,
3,3,3,3,3,3,3,3,4),(-85.5303833989759,-85.5141179700809,-85.0169428656037,
-84.5197677611264,-84.0225926566492,-83.525417552172,-83.0282424476948,
-82.5310673432176,-82.0338922387404,-81.5367171342632,-81.039542029786,
-80.5423669253087,-80.0451918208315,-79.5480167163543,-79.2471980917962),
 .UNSPECIFIED.);
#778=B_SPLINE_CURVE_WITH_KNOTS('',3,(#29136,#29137,#29138,#29139,#29140,
#29141,#29142,#29143,#29144,#29145,#29146,#29147,#29148,#29149,#29150,#29151,
#29152,#29153,#29154,#29155,#29156,#29157,#29158,#29159,#29160,#29161,#29162,
#29163,#29164,#29165,#29166,#29167,#29168,#29169,#29170,#29171,#29172,#29173,
#29174,#29175),.UNSPECIFIED.,.F.,.F.,(4,3,3,3,3,3,3,3,3,3,3,3,3,4),(76.7072426873232,
77.0621411939682,77.5593162984454,78.0564914029227,78.5536665073999,79.0508416118771,
79.5480167163543,80.0451918208315,80.5423669253087,81.0395420297859,81.5367171342632,
82.0338922387404,82.5310673432176,82.9904279945029),.UNSPECIFIED.);
#779=B_SPLINE_CURVE_WITH_KNOTS('',3,(#29176,#29177,#29178,#29179,#29180,
#29181,#29182,#29183,#29184,#29185,#29186,#29187,#29188,#29189,#29190,#29191,
#29192,#29193,#29194,#29195,#29196,#29197,#29198,#29199,#29200,#29201,#29202,
#29203,#29204,#29205,#29206,#29207,#29208,#29209,#29210,#29211,#29212,#29213,
#29214,#29215,#29216,#29217,#29218),.UNSPECIFIED.,.F.,.F.,(4,3,3,3,3,3,
3,3,3,3,3,3,3,3,4),(-79.2471980917962,-79.0508416118771,-78.5536665073999,
-78.0564914029227,-77.5593162984455,-77.0621411939683,-76.564966089491,
-76.0677909850138,-75.5706158805366,-75.0734407760594,-74.5762656715822,
-74.079090567105,-73.5819154626277,-73.0847403581505,-72.9640127846165),
 .UNSPECIFIED.);
#780=B_SPLINE_CURVE_WITH_KNOTS('',3,(#29223,#29224,#29225,#29226,#29227,
#29228,#29229,#29230,#29231,#29232,#29233,#29234,#29235,#29236,#29237,#29238,
#29239,#29240,#29241,#29242,#29243,#29244,#29245,#29246,#29247,#29248,#29249,
#29250,#29251,#29252,#29253,#29254,#29255,#29256,#29257,#29258,#29259,#29260,
#29261,#29262,#29263,#29264,#29265),.UNSPECIFIED.,.F.,.F.,(4,3,3,3,3,3,
3,3,3,3,3,3,3,3,4),(70.4240573801435,70.5988648357644,71.0960399402417,
71.5932150447189,72.0903901491961,72.5875652536733,73.0847403581505,73.5819154626277,
74.0790905671049,74.5762656715822,75.0734407760594,75.5706158805366,76.0677909850138,
76.564966089491,76.7072426873232),.UNSPECIFIED.);
#781=B_SPLINE_CURVE_WITH_KNOTS('',3,(#29266,#29267,#29268,#29269,#29270,
#29271,#29272,#29273,#29274,#29275,#29276,#29277,#29278,#29279,#29280,#29281,
#29282,#29283,#29284,#29285,#29286,#29287,#29288,#29289,#29290,#29291,#29292,
#29293,#29294,#29295,#29296,#29297,#29298,#29299,#29300,#29301,#29302,#29303,
#29304,#29305),.UNSPECIFIED.,.F.,.F.,(4,3,3,3,3,3,3,3,3,3,3,3,3,4),(-72.9640127846165,
-72.5875652536733,-72.0903901491961,-71.5932150447189,-71.0960399402417,
-70.5988648357645,-70.1016897312873,-69.60451462681,-69.1073395223328,-68.6101644178556,
-68.1129893133784,-67.6158142089012,-67.1186391044239,-66.6808274774369),
 .UNSPECIFIED.);
#782=B_SPLINE_CURVE_WITH_KNOTS('',3,(#29310,#29311,#29312,#29313,#29314,
#29315,#29316,#29317,#29318,#29319,#29320,#29321,#29322,#29323,#29324,#29325,
#29326,#29327,#29328,#29329,#29330,#29331,#29332,#29333,#29334,#29335,#29336,
#29337,#29338,#29339,#29340,#29341,#29342,#29343,#29344,#29345,#29346,#29347,
#29348,#29349),.UNSPECIFIED.,.F.,.F.,(4,3,3,3,3,3,3,3,3,3,3,3,3,4),(64.1408720729639,
64.6327635820379,65.1299386865151,65.6271137909923,66.1242888954695,66.6214639999467,
67.1186391044239,67.6158142089012,68.1129893133784,68.6101644178556,69.1073395223328,
69.60451462681,70.1016897312872,70.4240573801435),.UNSPECIFIED.);
#783=B_SPLINE_CURVE_WITH_KNOTS('',3,(#29350,#29351,#29352,#29353,#29354,
#29355,#29356,#29357,#29358,#29359,#29360,#29361,#29362,#29363,#29364,#29365,
#29366,#29367,#29368,#29369,#29370,#29371,#29372,#29373,#29374,#29375,#29376,
#29377,#29378,#29379,#29380,#29381,#29382,#29383,#29384,#29385,#29386,#29387,
#29388,#29389,#29390,#29391,#29392),.UNSPECIFIED.,.F.,.F.,(4,3,3,3,3,3,
3,3,3,3,3,3,3,3,4),(-66.6808274774369,-66.6214639999467,-66.1242888954695,
-65.6271137909923,-65.1299386865151,-64.6327635820379,-64.1355884775607,
-63.6384133730835,-63.1412382686062,-62.644063164129,-62.1468880596518,
-61.6497129551746,-61.1525378506974,-60.6553627462202,-60.3976421702572),
 .UNSPECIFIED.);
#784=B_SPLINE_CURVE_WITH_KNOTS('',3,(#29397,#29398,#29399,#29400,#29401,
#29402,#29403,#29404,#29405,#29406,#29407,#29408,#29409,#29410,#29411,#29412,
#29413,#29414,#29415,#29416,#29417,#29418,#29419,#29420,#29421,#29422,#29423,
#29424,#29425,#29426,#29427,#29428,#29429,#29430,#29431,#29432,#29433,#29434,
#29435,#29436,#29437,#29438,#29439),.UNSPECIFIED.,.F.,.F.,(4,3,3,3,3,3,
3,3,3,3,3,3,3,3,4),(57.8576867657842,58.1694872238341,58.6666623283113,
59.1638374327885,59.6610125372657,60.1581876417429,60.6553627462201,61.1525378506974,
61.6497129551746,62.1468880596518,62.644063164129,63.1412382686062,63.6384133730835,
64.1355884775607,64.1408720729639),.UNSPECIFIED.);
#785=B_SPLINE_CURVE_WITH_KNOTS('',3,(#29440,#29441,#29442,#29443,#29444,
#29445,#29446,#29447,#29448,#29449,#29450,#29451,#29452,#29453,#29454,#29455,
#29456,#29457,#29458,#29459,#29460,#29461,#29462,#29463,#29464,#29465,#29466,
#29467,#29468,#29469,#29470,#29471,#29472,#29473,#29474,#29475,#29476,#29477,
#29478,#29479,#29480,#29481,#29482),.UNSPECIFIED.,.F.,.F.,(4,3,3,3,3,3,
3,3,3,3,3,3,3,3,4),(-60.3976421702572,-60.158187641743,-59.6610125372657,
-59.1638374327885,-58.6666623283113,-58.1694872238341,-57.6723121193569,
-57.1751370148797,-56.6779619104025,-56.1807868059252,-55.683611701448,
-55.1864365969708,-54.6892614924936,-54.1920863880164,-54.114456863078),
 .UNSPECIFIED.);
#786=B_SPLINE_CURVE_WITH_KNOTS('',3,(#29487,#29488,#29489,#29490,#29491,
#29492,#29493,#29494,#29495,#29496,#29497,#29498,#29499,#29500,#29501,#29502,
#29503,#29504,#29505,#29506,#29507,#29508,#29509,#29510,#29511,#29512,#29513,
#29514,#29515,#29516,#29517,#29518,#29519,#29520,#29521,#29522,#29523,#29524,
#29525,#29526,#29527,#29528,#29529),.UNSPECIFIED.,.F.,.F.,(4,3,3,3,3,3,
3,3,3,3,3,3,3,3,4),(51.5745014586045,51.7062108656303,52.2033859701075,
52.7005610745847,53.1977361790619,53.6949112835391,54.1920863880164,54.6892614924936,
55.1864365969708,55.683611701448,56.1807868059252,56.6779619104024,57.1751370148797,
57.6723121193569,57.8576867657842),.UNSPECIFIED.);
#787=B_SPLINE_CURVE_WITH_KNOTS('',3,(#29530,#29531,#29532,#29533,#29534,
#29535,#29536,#29537,#29538,#29539,#29540,#29541,#29542,#29543,#29544,#29545,
#29546,#29547,#29548,#29549,#29550,#29551,#29552,#29553,#29554,#29555,#29556,
#29557,#29558,#29559,#29560,#29561,#29562,#29563,#29564,#29565,#29566,#29567,
#29568,#29569),.UNSPECIFIED.,.F.,.F.,(4,3,3,3,3,3,3,3,3,3,3,3,3,4),(-54.114456863078,
-53.6949112835392,-53.197736179062,-52.7005610745847,-52.2033859701075,
-51.7062108656303,-51.2090357611531,-50.7118606566759,-50.2146855521987,
-49.7175104477215,-49.2203353432442,-48.723160238767,-48.2259851342898,
-47.8312715558983),.UNSPECIFIED.);
#788=B_SPLINE_CURVE_WITH_KNOTS('',3,(#29574,#29575,#29576,#29577,#29578,
#29579,#29580,#29581,#29582,#29583,#29584,#29585,#29586,#29587,#29588,#29589,
#29590,#29591,#29592,#29593,#29594,#29595,#29596,#29597,#29598,#29599,#29600,
#29601,#29602,#29603,#29604,#29605,#29606,#29607,#29608,#29609,#29610,#29611,
#29612,#29613),.UNSPECIFIED.,.F.,.F.,(4,3,3,3,3,3,3,3,3,3,3,3,3,4),(45.2913161514253,
45.7401096119037,46.2372847163809,46.7344598208582,47.2316349253354,47.7288100298126,
48.2259851342898,48.723160238767,49.2203353432442,49.7175104477214,50.2146855521987,
50.7118606566759,51.2090357611531,51.5745014586045),.UNSPECIFIED.);
#789=B_SPLINE_CURVE_WITH_KNOTS('',3,(#29614,#29615,#29616,#29617,#29618,
#29619,#29620,#29621,#29622,#29623,#29624,#29625,#29626,#29627,#29628,#29629,
#29630,#29631,#29632,#29633,#29634,#29635,#29636,#29637,#29638,#29639,#29640,
#29641,#29642,#29643,#29644,#29645,#29646,#29647,#29648,#29649,#29650,#29651,
#29652,#29653,#29654,#29655,#29656),.UNSPECIFIED.,.F.,.F.,(4,3,3,3,3,3,
3,3,3,3,3,3,3,3,4),(-47.8312715558983,-47.7288100298126,-47.2316349253354,
-46.7344598208582,-46.2372847163809,-45.7401096119037,-45.2429345074265,
-44.7457594029493,-44.2485842984721,-43.7514091939949,-43.2542340895177,
-42.7570589850404,-42.2598838805632,-41.762708776086,-41.5480862487186),
 .UNSPECIFIED.);
#790=B_SPLINE_CURVE_WITH_KNOTS('',3,(#29661,#29662,#29663,#29664,#29665,
#29666,#29667,#29668,#29669,#29670,#29671,#29672,#29673,#29674,#29675,#29676,
#29677,#29678,#29679,#29680,#29681,#29682,#29683,#29684,#29685,#29686,#29687,
#29688,#29689,#29690,#29691,#29692,#29693,#29694,#29695,#29696,#29697,#29698,
#29699,#29700,#29701,#29702,#29703),.UNSPECIFIED.,.F.,.F.,(4,3,3,3,3,3,
3,3,3,3,3,3,3,3,4),(39.0081308442456,39.2768332536999,39.7740083581771,
40.2711834626544,40.7683585671316,41.2655336716088,41.762708776086,42.2598838805632,
42.7570589850404,43.2542340895177,43.7514091939949,44.2485842984721,44.7457594029493,
45.2429345074265,45.2913161514253),.UNSPECIFIED.);
#791=B_SPLINE_CURVE_WITH_KNOTS('',3,(#29704,#29705,#29706,#29707,#29708,
#29709,#29710,#29711,#29712,#29713,#29714,#29715,#29716,#29717,#29718,#29719,
#29720,#29721,#29722,#29723,#29724,#29725,#29726,#29727,#29728,#29729,#29730,
#29731,#29732,#29733,#29734,#29735,#29736,#29737,#29738,#29739,#29740,#29741,
#29742,#29743,#29744,#29745,#29746),.UNSPECIFIED.,.F.,.F.,(4,3,3,3,3,3,
3,3,3,3,3,3,3,3,4),(-41.5480862487186,-41.2655336716088,-40.7683585671316,
-40.2711834626544,-39.7740083581772,-39.2768332536999,-38.7796581492227,
-38.2824830447455,-37.7853079402683,-37.2881328357911,-36.7909577313139,
-36.2937826268367,-35.7966075223594,-35.2994324178822,-35.2649009415389),
 .UNSPECIFIED.);
#792=B_SPLINE_CURVE_WITH_KNOTS('',3,(#29751,#29752,#29753,#29754,#29755,
#29756,#29757,#29758,#29759,#29760,#29761,#29762,#29763,#29764,#29765,#29766,
#29767,#29768,#29769,#29770,#29771,#29772,#29773,#29774,#29775,#29776,#29777,
#29778,#29779,#29780,#29781,#29782,#29783,#29784,#29785,#29786,#29787,#29788,
#29789,#29790,#29791,#29792,#29793),.UNSPECIFIED.,.F.,.F.,(4,3,3,3,3,3,
3,3,3,3,3,3,3,3,4),(32.7249455370659,32.8135568954961,33.3107319999734,
33.8079071044506,34.3050822089278,34.802257313405,35.2994324178822,35.7966075223594,
36.2937826268367,36.7909577313139,37.2881328357911,37.7853079402683,38.2824830447455,
38.7796581492227,39.0081308442456),.UNSPECIFIED.);
#793=B_SPLINE_CURVE_WITH_KNOTS('',3,(#29794,#29795,#29796,#29797,#29798,
#29799,#29800,#29801,#29802,#29803,#29804,#29805,#29806,#29807,#29808,#29809,
#29810,#29811,#29812,#29813,#29814,#29815,#29816,#29817,#29818,#29819,#29820,
#29821,#29822,#29823,#29824,#29825,#29826,#29827,#29828,#29829,#29830,#29831,
#29832,#29833),.UNSPECIFIED.,.F.,.F.,(4,3,3,3,3,3,3,3,3,3,3,3,3,4),(-35.2649009415389,
-34.802257313405,-34.3050822089278,-33.8079071044506,-33.3107319999734,
-32.8135568954962,-32.3163817910189,-31.8192066865417,-31.3220315820645,
-30.8248564775873,-30.3276813731101,-29.8305062686329,-29.3333311641557,
-28.9817156343593),.UNSPECIFIED.);
#794=B_SPLINE_CURVE_WITH_KNOTS('',3,(#29838,#29839,#29840,#29841,#29842,
#29843,#29844,#29845,#29846,#29847,#29848,#29849,#29850,#29851,#29852,#29853,
#29854,#29855,#29856,#29857,#29858,#29859,#29860,#29861,#29862,#29863,#29864,
#29865,#29866,#29867,#29868,#29869,#29870,#29871,#29872,#29873,#29874,#29875,
#29876,#29877),.UNSPECIFIED.,.F.,.F.,(4,3,3,3,3,3,3,3,3,3,3,3,3,4),(26.4417602298863,
26.8474556417696,27.3446307462468,27.841805850724,28.3389809552012,28.8361560596784,
29.3333311641556,29.8305062686329,30.3276813731101,30.8248564775873,31.3220315820645,
31.8192066865417,32.3163817910189,32.7249455370659),.UNSPECIFIED.);
#795=B_SPLINE_CURVE_WITH_KNOTS('',3,(#29878,#29879,#29880,#29881,#29882,
#29883,#29884,#29885,#29886,#29887,#29888,#29889,#29890,#29891,#29892,#29893,
#29894,#29895,#29896,#29897,#29898,#29899,#29900,#29901,#29902,#29903,#29904,
#29905,#29906,#29907,#29908,#29909,#29910,#29911,#29912,#29913,#29914,#29915,
#29916,#29917,#29918,#29919,#29920),.UNSPECIFIED.,.F.,.F.,(4,3,3,3,3,3,
3,3,3,3,3,3,3,3,4),(-28.9817156343593,-28.8361560596784,-28.3389809552012,
-27.841805850724,-27.3446307462468,-26.8474556417696,-26.3502805372924,
-25.8531054328152,-25.3559303283379,-24.8587552238607,-24.3615801193835,
-23.8644050149063,-23.3672299104291,-22.8700548059519,-22.69853032718),
 .UNSPECIFIED.);
#796=B_SPLINE_CURVE_WITH_KNOTS('',3,(#29925,#29926,#29927,#29928,#29929,
#29930,#29931,#29932,#29933,#29934,#29935,#29936,#29937,#29938,#29939,#29940,
#29941,#29942,#29943,#29944,#29945,#29946,#29947,#29948,#29949,#29950,#29951,
#29952,#29953,#29954,#29955,#29956,#29957,#29958,#29959,#29960,#29961,#29962,
#29963,#29964,#29965,#29966,#29967),.UNSPECIFIED.,.F.,.F.,(4,3,3,3,3,3,
3,3,3,3,3,3,3,3,4),(20.1585749227066,20.3841792835658,20.881354388043,21.3785294925202,
21.8757045969974,22.3728797014746,22.8700548059519,23.3672299104291,23.8644050149063,
24.3615801193835,24.8587552238607,25.3559303283379,25.8531054328151,26.3502805372924,
26.4417602298863),.UNSPECIFIED.);
#797=B_SPLINE_CURVE_WITH_KNOTS('',3,(#29968,#29969,#29970,#29971,#29972,
#29973,#29974,#29975,#29976,#29977,#29978,#29979,#29980,#29981,#29982,#29983,
#29984,#29985,#29986,#29987,#29988,#29989,#29990,#29991,#29992,#29993,#29994,
#29995,#29996,#29997,#29998,#29999,#30000,#30001,#30002,#30003,#30004,#30005,
#30006,#30007),.UNSPECIFIED.,.F.,.F.,(4,3,3,3,3,3,3,3,3,3,3,3,3,4),(-22.69853032718,
-22.3728797014747,-21.8757045969974,-21.3785294925202,-20.881354388043,
-20.3841792835658,-19.8870041790886,-19.3898290746114,-18.8926539701342,
-18.3954788656569,-17.8983037611797,-17.4011286567025,-16.9039535522253,
-16.4153450200004),.UNSPECIFIED.);
#798=B_SPLINE_CURVE_WITH_KNOTS('',3,(#30012,#30013,#30014,#30015,#30016,
#30017,#30018,#30019,#30020,#30021,#30022,#30023,#30024,#30025,#30026,#30027,
#30028,#30029,#30030,#30031,#30032,#30033,#30034,#30035,#30036,#30037,#30038,
#30039,#30040,#30041,#30042,#30043,#30044,#30045,#30046,#30047,#30048,#30049,
#30050,#30051,#30052,#30053,#30054),.UNSPECIFIED.,.F.,.F.,(4,3,3,3,3,3,
3,3,3,3,3,3,3,3,4),(13.8753896155273,13.920902925362,14.4180780298392,14.9152531343164,
15.4124282387936,15.9096033432709,16.4067784477481,16.9039535522253,17.4011286567025,
17.8983037611797,18.3954788656569,18.8926539701341,19.3898290746114,19.8870041790886,
20.1585749227066),.UNSPECIFIED.);
#799=B_SPLINE_CURVE_WITH_KNOTS('',3,(#30055,#30056,#30057,#30058,#30059,
#30060,#30061,#30062,#30063,#30064,#30065,#30066,#30067,#30068,#30069,#30070,
#30071,#30072,#30073,#30074,#30075,#30076,#30077,#30078,#30079,#30080,#30081,
#30082,#30083,#30084,#30085,#30086,#30087,#30088,#30089,#30090,#30091,#30092,
#30093,#30094,#30095,#30096,#30097),.UNSPECIFIED.,.F.,.F.,(4,3,3,3,3,3,
3,3,3,3,3,3,3,3,4),(-16.4153450200004,-16.4067784477481,-15.9096033432709,
-15.4124282387936,-14.9152531343164,-14.4180780298392,-13.920902925362,
-13.4237278208848,-12.9265527164076,-12.4293776119304,-11.9322025074531,
-11.4350274029759,-10.9378522984987,-10.4406771940215,-10.1321597128207),
 .UNSPECIFIED.);
#800=B_SPLINE_CURVE_WITH_KNOTS('',3,(#30103,#30104,#30105,#30106,#30107,
#30108,#30109,#30110,#30111,#30112,#30113,#30114,#30115,#30116,#30117,#30118,
#30119,#30120,#30121,#30122,#30123,#30124,#30125,#30126,#30127),
 .UNSPECIFIED.,.F.,.F.,(4,3,3,3,3,3,3,3,4),(-3.848974405641,-3.4802257313405,
-2.98305062686329,-2.48587552238607,-1.98870041790886,-1.49152531343164,
-0.99435020895443,-0.497175104477215,0.),.UNSPECIFIED.);
#801=B_SPLINE_CURVE_WITH_KNOTS('',3,(#30130,#30131,#30132,#30133,#30134,
#30135,#30136,#30137,#30138,#30139,#30140,#30141,#30142,#30143,#30144,#30145,
#30146,#30147,#30148,#30149,#30150,#30151,#30152,#30153,#30154,#30155,#30156,
#30157,#30158,#30159,#30160,#30161,#30162,#30163,#30164,#30165,#30166),
 .UNSPECIFIED.,.F.,.F.,(4,3,3,3,3,3,3,3,3,3,3,3,4),(2.01640075321939,2.48587552238607,
2.98305062686328,3.4802257313405,3.97740083581771,4.47457594029493,4.97175104477214,
5.46892614924935,5.96610125372657,6.46327635820378,6.960451462681,7.45762656715821,
7.59220430834767),.UNSPECIFIED.);
#802=B_SPLINE_CURVE_WITH_KNOTS('',3,(#30172,#30173,#30174,#30175,#30176,
#30177,#30178,#30179,#30180,#30181,#30182,#30183),.UNSPECIFIED.,.F.,.F.,
(4,1,1,1,1,1,1,1,1,4),(166.504410640259,166.977621459199,167.474796563676,
167.971971668153,168.46914677263,168.966321877108,169.463496981585,169.960672086062,
170.457847190539,170.955022295017),.UNSPECIFIED.);
#803=B_SPLINE_CURVE_WITH_KNOTS('',3,(#30186,#30187,#30188,#30189,#30190,
#30191,#30192,#30193,#30194,#30195,#30196,#30197,#30198,#30199),
 .UNSPECIFIED.,.F.,.F.,(4,1,1,1,1,1,1,1,1,1,1,4),(166.504410640259,166.534526236809,
167.031701341286,167.528876445763,168.02605155024,168.523226654717,169.020401759195,
169.517576863672,170.014751968149,170.511927072626,171.009102177104,171.47857694627),
 .UNSPECIFIED.);
#804=B_SPLINE_CURVE_WITH_KNOTS('',3,(#30204,#30205,#30206,#30207,#30208,
#30209,#30210,#30211,#30212,#30213,#30214,#30215,#30216,#30217,#30218,#30219,
#30220),.UNSPECIFIED.,.F.,.F.,(4,1,1,1,1,1,1,1,1,1,1,1,1,1,4),(160.22122533308,
160.514345100995,161.011520205472,161.508695309949,162.005870414427,162.503045518904,
163.000220623381,163.497395727858,163.994570832336,164.491745936813,164.98892104129,
165.486096145767,165.983271250244,166.480446354722,166.504410640259),
 .UNSPECIFIED.);
#805=B_SPLINE_CURVE_WITH_KNOTS('',3,(#30221,#30222,#30223,#30224,#30225,
#30226,#30227,#30228,#30229,#30230,#30231,#30232,#30233,#30234,#30235,#30236),
 .UNSPECIFIED.,.F.,.F.,(4,1,1,1,1,1,1,1,1,1,1,1,1,4),(160.22122533308,160.568424983082,
161.065600087559,161.562775192036,162.059950296514,162.557125400991,163.054300505468,
163.551475609945,164.048650714422,164.5458258189,165.043000923377,165.540176027854,
166.037351132331,166.504410640259),.UNSPECIFIED.);
#806=B_SPLINE_CURVE_WITH_KNOTS('',3,(#30241,#30242,#30243,#30244,#30245,
#30246,#30247,#30248,#30249,#30250,#30251,#30252,#30253,#30254,#30255,#30256,
#30257),.UNSPECIFIED.,.F.,.F.,(4,1,1,1,1,1,1,1,1,1,1,1,1,1,4),(153.9380400259,
154.051068742791,154.548243847269,155.045418951746,155.542594056223,156.0397691607,
156.536944265177,157.034119369655,157.531294474132,158.028469578609,158.525644683086,
159.022819787563,159.519994892041,160.017169996518,160.22122533308),
 .UNSPECIFIED.);
#807=B_SPLINE_CURVE_WITH_KNOTS('',3,(#30258,#30259,#30260,#30261,#30262,
#30263,#30264,#30265,#30266,#30267,#30268,#30269,#30270,#30271,#30272,#30273,
#30274),.UNSPECIFIED.,.F.,.F.,(4,1,1,1,1,1,1,1,1,1,1,1,1,1,4),(153.9380400259,
154.105148624878,154.602323729355,155.099498833833,155.59667393831,156.093849042787,
156.591024147264,157.088199251742,157.585374356219,158.082549460696,158.579724565173,
159.07689966965,159.574074774128,160.071249878605,160.22122533308),
 .UNSPECIFIED.);
#808=B_SPLINE_CURVE_WITH_KNOTS('',3,(#30279,#30280,#30281,#30282,#30283,
#30284,#30285,#30286,#30287,#30288,#30289,#30290,#30291,#30292,#30293,#30294),
 .UNSPECIFIED.,.F.,.F.,(4,1,1,1,1,1,1,1,1,1,1,1,1,4),(147.65485471872,148.084967489065,
148.582142593542,149.079317698019,149.576492802496,150.073667906974,150.570843011451,
151.068018115928,151.565193220405,152.062368324882,152.55954342936,153.056718533837,
153.553893638314,153.9380400259),.UNSPECIFIED.);
#809=B_SPLINE_CURVE_WITH_KNOTS('',3,(#30295,#30296,#30297,#30298,#30299,
#30300,#30301,#30302,#30303,#30304,#30305,#30306,#30307,#30308,#30309,#30310),
 .UNSPECIFIED.,.F.,.F.,(4,1,1,1,1,1,1,1,1,1,1,1,1,4),(147.65485471872,148.139047371152,
148.636222475629,149.133397580106,149.630572684583,150.12774778906,150.624922893538,
151.122097998015,151.619273102492,152.116448206969,152.613623311447,153.110798415924,
153.607973520401,153.9380400259),.UNSPECIFIED.);
#810=B_SPLINE_CURVE_WITH_KNOTS('',3,(#30315,#30316,#30317,#30318,#30319,
#30320,#30321,#30322,#30323,#30324,#30325,#30326,#30327,#30328,#30329,#30330,
#30331),.UNSPECIFIED.,.F.,.F.,(4,1,1,1,1,1,1,1,1,1,1,1,1,1,4),(141.371669411541,
141.621691130861,142.118866235338,142.616041339815,143.113216444293,143.61039154877,
144.107566653247,144.604741757724,145.101916862201,145.599091966679,146.096267071156,
146.593442175633,147.09061728011,147.587792384587,147.65485471872),
 .UNSPECIFIED.);
#811=B_SPLINE_CURVE_WITH_KNOTS('',3,(#30332,#30333,#30334,#30335,#30336,
#30337,#30338,#30339,#30340,#30341,#30342,#30343,#30344,#30345,#30346,#30347,
#30348),.UNSPECIFIED.,.F.,.F.,(4,1,1,1,1,1,1,1,1,1,1,1,1,1,4),(141.371669411541,
141.675771012948,142.172946117425,142.670121221902,143.167296326379,143.664471430857,
144.161646535334,144.658821639811,145.155996744288,145.653171848766,146.150346953243,
146.64752205772,147.144697162197,147.641872266674,147.65485471872),
 .UNSPECIFIED.);
#812=B_SPLINE_CURVE_WITH_KNOTS('',3,(#30353,#30354,#30355,#30356,#30357,
#30358,#30359,#30360,#30361,#30362,#30363,#30364,#30365,#30366,#30367,#30368,
#30369),.UNSPECIFIED.,.F.,.F.,(4,1,1,1,1,1,1,1,1,1,1,1,1,1,4),(135.088484104361,
135.158414772657,135.655589877134,136.152764981612,136.649940086089,137.147115190566,
137.644290295043,138.14146539952,138.638640503998,139.135815608475,139.632990712952,
140.130165817429,140.627340921906,141.124516026384,141.371669411541),
 .UNSPECIFIED.);
#813=B_SPLINE_CURVE_WITH_KNOTS('',3,(#30370,#30371,#30372,#30373,#30374,
#30375,#30376,#30377,#30378,#30379,#30380,#30381,#30382,#30383,#30384,#30385,
#30386),.UNSPECIFIED.,.F.,.F.,(4,1,1,1,1,1,1,1,1,1,1,1,1,1,4),(135.088484104361,
135.212494654744,135.709669759221,136.206844863698,136.704019968176,137.201195072653,
137.69837017713,138.195545281607,138.692720386085,139.189895490562,139.687070595039,
140.184245699516,140.681420803993,141.178595908471,141.371669411541),
 .UNSPECIFIED.);
#814=B_SPLINE_CURVE_WITH_KNOTS('',3,(#30391,#30392,#30393,#30394,#30395,
#30396,#30397,#30398,#30399,#30400,#30401,#30402,#30403,#30404,#30405,#30406),
 .UNSPECIFIED.,.F.,.F.,(4,1,1,1,1,1,1,1,1,1,1,1,1,4),(128.805298797182,
129.192313518931,129.689488623408,130.186663727885,130.683838832362,131.181013936839,
131.678189041317,132.175364145794,132.672539250271,133.169714354748,133.666889459226,
134.164064563703,134.66123966818,135.088484104361),.UNSPECIFIED.);
#815=B_SPLINE_CURVE_WITH_KNOTS('',3,(#30407,#30408,#30409,#30410,#30411,
#30412,#30413,#30414,#30415,#30416,#30417,#30418,#30419,#30420,#30421,#30422),
 .UNSPECIFIED.,.F.,.F.,(4,1,1,1,1,1,1,1,1,1,1,1,1,4),(128.805298797182,
129.246393401017,129.743568505495,130.240743609972,130.737918714449,131.235093818926,
131.732268923404,132.229444027881,132.726619132358,133.223794236835,133.720969341312,
134.21814444579,134.715319550267,135.088484104361),.UNSPECIFIED.);
#816=B_SPLINE_CURVE_WITH_KNOTS('',3,(#30427,#30428,#30429,#30430,#30431,
#30432,#30433,#30434,#30435,#30436,#30437,#30438,#30439,#30440,#30441,#30442,
#30443),.UNSPECIFIED.,.F.,.F.,(4,1,1,1,1,1,1,1,1,1,1,1,1,1,4),(122.522113490002,
122.729037160727,123.226212265204,123.723387369681,124.220562474158,124.717737578636,
125.214912683113,125.71208778759,126.209262892067,126.706437996544,127.203613101022,
127.700788205499,128.197963309976,128.695138414453,128.805298797182),
 .UNSPECIFIED.);
#817=B_SPLINE_CURVE_WITH_KNOTS('',3,(#30444,#30445,#30446,#30447,#30448,
#30449,#30450,#30451,#30452,#30453,#30454,#30455,#30456,#30457,#30458,#30459,
#30460),.UNSPECIFIED.,.F.,.F.,(4,1,1,1,1,1,1,1,1,1,1,1,1,1,4),(122.522113490002,
122.783117042814,123.280292147291,123.777467251768,124.274642356245,124.771817460723,
125.2689925652,125.766167669677,126.263342774154,126.760517878631,127.257692983109,
127.754868087586,128.252043192063,128.74921829654,128.805298797182),
 .UNSPECIFIED.);
#818=B_SPLINE_CURVE_WITH_KNOTS('',3,(#30465,#30466,#30467,#30468,#30469,
#30470,#30471,#30472,#30473,#30474,#30475,#30476,#30477,#30478,#30479,#30480,
#30481),.UNSPECIFIED.,.F.,.F.,(4,1,1,1,1,1,1,1,1,1,1,1,1,1,4),(116.238928182822,
116.265760802523,116.762935907,117.260111011477,117.757286115955,118.254461220432,
118.751636324909,119.248811429386,119.745986533863,120.243161638341,120.740336742818,
121.237511847295,121.734686951772,122.23186205625,122.522113490002),
 .UNSPECIFIED.);
#819=B_SPLINE_CURVE_WITH_KNOTS('',3,(#30482,#30483,#30484,#30485,#30486,
#30487,#30488,#30489,#30490,#30491,#30492,#30493,#30494,#30495,#30496,#30497,
#30498),.UNSPECIFIED.,.F.,.F.,(4,1,1,1,1,1,1,1,1,1,1,1,1,1,4),(116.238928182822,
116.31984068461,116.817015789087,117.314190893564,117.811365998042,118.308541102519,
118.805716206996,119.302891311473,119.80006641595,120.297241520428,120.794416624905,
121.291591729382,121.788766833859,122.285941938336,122.522113490002),
 .UNSPECIFIED.);
#820=B_SPLINE_CURVE_WITH_KNOTS('',3,(#30503,#30504,#30505,#30506,#30507,
#30508,#30509,#30510,#30511,#30512,#30513,#30514,#30515,#30516,#30517,#30518),
 .UNSPECIFIED.,.F.,.F.,(4,1,1,1,1,1,1,1,1,1,1,1,1,4),(109.955742875643,
110.299659548796,110.796834653274,111.294009757751,111.791184862228,112.288359966705,
112.785535071182,113.28271017566,113.779885280137,114.277060384614,114.774235489091,
115.271410593569,115.768585698046,116.238928182822),.UNSPECIFIED.);
#821=B_SPLINE_CURVE_WITH_KNOTS('',3,(#30519,#30520,#30521,#30522,#30523,
#30524,#30525,#30526,#30527,#30528,#30529,#30530,#30531,#30532,#30533,#30534),
 .UNSPECIFIED.,.F.,.F.,(4,1,1,1,1,1,1,1,1,1,1,1,1,4),(109.955742875643,
110.353739430883,110.850914535361,111.348089639838,111.845264744315,112.342439848792,
112.839614953269,113.336790057747,113.833965162224,114.331140266701,114.828315371178,
115.325490475655,115.822665580133,116.238928182822),.UNSPECIFIED.);
#822=B_SPLINE_CURVE_WITH_KNOTS('',3,(#30539,#30540,#30541,#30542,#30543,
#30544,#30545,#30546,#30547,#30548,#30549,#30550,#30551,#30552,#30553,#30554,
#30555),.UNSPECIFIED.,.F.,.F.,(4,1,1,1,1,1,1,1,1,1,1,1,1,1,4),(103.672557568463,
103.836383190593,104.33355829507,104.830733399547,105.327908504024,105.825083608501,
106.322258712979,106.819433817456,107.316608921933,107.81378402641,108.310959130888,
108.808134235365,109.305309339842,109.802484444319,109.955742875643),
 .UNSPECIFIED.);
#823=B_SPLINE_CURVE_WITH_KNOTS('',3,(#30556,#30557,#30558,#30559,#30560,
#30561,#30562,#30563,#30564,#30565,#30566,#30567,#30568,#30569,#30570,#30571,
#30572),.UNSPECIFIED.,.F.,.F.,(4,1,1,1,1,1,1,1,1,1,1,1,1,1,4),(103.672557568463,
103.89046307268,104.387638177157,104.884813281634,105.381988386111,105.879163490588,
106.376338595066,106.873513699543,107.37068880402,107.867863908497,108.365039012974,
108.862214117452,109.359389221929,109.856564326406,109.955742875643),
 .UNSPECIFIED.);
#824=B_SPLINE_CURVE_WITH_KNOTS('',3,(#30577,#30578,#30579,#30580,#30581,
#30582,#30583,#30584,#30585,#30586,#30587,#30588,#30589,#30590,#30591,#30592),
 .UNSPECIFIED.,.F.,.F.,(4,1,1,1,1,1,1,1,1,1,1,1,1,4),(97.3893722612839,
97.870281936866,98.3674570413433,98.8646321458205,99.3618072502977,99.8589823547749,
100.356157459252,100.853332563729,101.350507668207,101.847682772684,102.344857877161,
102.842032981638,103.339208086115,103.672557568463),.UNSPECIFIED.);
#825=B_SPLINE_CURVE_WITH_KNOTS('',3,(#30593,#30594,#30595,#30596,#30597,
#30598,#30599,#30600,#30601,#30602,#30603,#30604,#30605,#30606,#30607,#30608,
#30609),.UNSPECIFIED.,.F.,.F.,(4,1,1,1,1,1,1,1,1,1,1,1,1,1,4),(97.3893722612839,
97.4271867144758,97.924361818953,98.4215369234302,98.9187120279074,99.4158871323846,
99.9130622368618,100.410237341339,100.907412445816,101.404587550293,101.901762654771,
102.398937759248,102.896112863725,103.393287968202,103.672557568463),
 .UNSPECIFIED.);
#826=B_SPLINE_CURVE_WITH_KNOTS('',3,(#30614,#30615,#30616,#30617,#30618,
#30619,#30620,#30621,#30622,#30623,#30624,#30625,#30626,#30627,#30628,#30629,
#30630),.UNSPECIFIED.,.F.,.F.,(4,1,1,1,1,1,1,1,1,1,1,1,1,1,4),(91.1061869541042,
91.4070055786623,91.9041806831395,92.4013557876167,92.8985308920939,93.3957059965711,
93.8928811010483,94.3900562055255,94.8872313100028,95.38440641448,95.8815815189572,
96.3787566234344,96.8759317279116,97.3731068323888,97.3893722612839),
 .UNSPECIFIED.);
#827=B_SPLINE_CURVE_WITH_KNOTS('',3,(#30631,#30632,#30633,#30634,#30635,
#30636,#30637,#30638,#30639,#30640,#30641,#30642,#30643,#30644,#30645,#30646),
 .UNSPECIFIED.,.F.,.F.,(4,1,1,1,1,1,1,1,1,1,1,1,1,4),(91.1061869541042,
91.4610854607492,91.9582605652264,92.4554356697036,92.9526107741808,93.449785878658,
93.9469609831353,94.4441360876125,94.9413111920897,95.4384862965669,95.9356614010441,
96.4328365055213,96.9300116099986,97.3893722612839),.UNSPECIFIED.);
#828=B_SPLINE_CURVE_WITH_KNOTS('',3,(#30651,#30652,#30653,#30654,#30655,
#30656,#30657,#30658,#30659,#30660,#30661,#30662,#30663,#30664,#30665,#30666,
#30667),.UNSPECIFIED.,.F.,.F.,(4,1,1,1,1,1,1,1,1,1,1,1,1,1,4),(84.8230016469245,
84.9437292204585,85.4409043249357,85.9380794294129,86.4352545338901,86.9324296383673,
87.4296047428445,87.9267798473217,88.423954951799,88.9211300562762,89.4183051607534,
89.9154802652306,90.4126553697078,90.909830474185,91.1061869541042),
 .UNSPECIFIED.);
#829=B_SPLINE_CURVE_WITH_KNOTS('',3,(#30668,#30669,#30670,#30671,#30672,
#30673,#30674,#30675,#30676,#30677,#30678,#30679,#30680,#30681,#30682,#30683,
#30684),.UNSPECIFIED.,.F.,.F.,(4,1,1,1,1,1,1,1,1,1,1,1,1,1,4),(84.8230016469245,
84.9978091025454,85.4949842070226,85.9921593114998,86.4893344159771,86.9865095204543,
87.4836846249315,87.9808597294087,88.4780348338859,88.9752099383631,89.4723850428403,
89.9695601473175,90.4667352517948,90.963910356272,91.1061869541042),
 .UNSPECIFIED.);
#830=B_SPLINE_CURVE_WITH_KNOTS('',3,(#30689,#30690,#30691,#30692,#30693,
#30694,#30695,#30696,#30697,#30698,#30699,#30700,#30701,#30702,#30703,#30704),
 .UNSPECIFIED.,.F.,.F.,(4,1,1,1,1,1,1,1,1,1,1,1,1,4),(78.5398163397448,
78.9776279667319,79.4748030712091,79.9719781756863,80.4691532801635,80.9663283846407,
81.463503489118,81.9606785935952,82.4578536980724,82.9550288025496,83.4522039070268,
83.949379011504,84.4465541159813,84.8230016469245),.UNSPECIFIED.);
#831=B_SPLINE_CURVE_WITH_KNOTS('',3,(#30705,#30706,#30707,#30708,#30709,
#30710,#30711,#30712,#30713,#30714,#30715,#30716,#30717,#30718,#30719,#30720),
 .UNSPECIFIED.,.F.,.F.,(4,1,1,1,1,1,1,1,1,1,1,1,1,4),(78.5398163397448,
79.0317078488188,79.528882953296,80.0260580577733,80.5232331622505,81.0204082667277,
81.5175833712049,82.0147584756821,82.5119335801593,83.0091086846365,83.5062837891138,
84.003458893591,84.5006339980682,84.8230016469245),.UNSPECIFIED.);
#832=B_SPLINE_CURVE_WITH_KNOTS('',3,(#30725,#30726,#30727,#30728,#30729,
#30730,#30731,#30732,#30733,#30734,#30735,#30736,#30737,#30738,#30739,#30740,
#30741),.UNSPECIFIED.,.F.,.F.,(4,1,1,1,1,1,1,1,1,1,1,1,1,1,4),(72.2566310325651,
72.5143516085281,73.0115267130053,73.5087018174825,74.0058769219598,74.503052026437,
75.0002271309142,75.4974022353914,75.9945773398686,76.4917524443458,76.988927548823,
77.4861026533003,77.9832777577775,78.4804528622547,78.5398163397448),
 .UNSPECIFIED.);
#833=B_SPLINE_CURVE_WITH_KNOTS('',3,(#30742,#30743,#30744,#30745,#30746,
#30747,#30748,#30749,#30750,#30751,#30752,#30753,#30754,#30755,#30756,#30757,
#30758),.UNSPECIFIED.,.F.,.F.,(4,1,1,1,1,1,1,1,1,1,1,1,1,1,4),(72.2566310325651,
72.568431490615,73.0656065950923,73.5627816995695,74.0599568040467,74.5571319085239,
75.0543070130011,75.5514821174783,76.0486572219556,76.5458323264328,77.04300743091,
77.5401825353872,78.0373576398644,78.5345327443416,78.5398163397448),
 .UNSPECIFIED.);
#834=B_SPLINE_CURVE_WITH_KNOTS('',3,(#30763,#30764,#30765,#30766,#30767,
#30768,#30769,#30770,#30771,#30772,#30773,#30774,#30775,#30776,#30777,#30778,
#30779),.UNSPECIFIED.,.F.,.F.,(4,1,1,1,1,1,1,1,1,1,1,1,1,1,4),(65.9734457253859,
66.0510752503243,66.5482503548015,67.0454254592788,67.542600563756,68.0397756682332,
68.5369507727104,69.0341258771876,69.5313009816648,70.028476086142,70.5256511906192,
71.0228262950965,71.5200013995737,72.0171765040509,72.2566310325651),
 .UNSPECIFIED.);
#835=B_SPLINE_CURVE_WITH_KNOTS('',3,(#30780,#30781,#30782,#30783,#30784,
#30785,#30786,#30787,#30788,#30789,#30790,#30791,#30792,#30793,#30794,#30795,
#30796),.UNSPECIFIED.,.F.,.F.,(4,1,1,1,1,1,1,1,1,1,1,1,1,1,4),(65.9734457253859,
66.1051551324113,66.6023302368885,67.0995053413657,67.5966804458429,68.0938555503201,
68.5910306547973,69.0882057592745,69.5853808637518,70.082555968229,70.5797310727062,
71.0769061771834,71.5740812816606,72.0712563861378,72.2566310325651),
 .UNSPECIFIED.);
#836=B_SPLINE_CURVE_WITH_KNOTS('',3,(#30801,#30802,#30803,#30804,#30805,
#30806,#30807,#30808,#30809,#30810,#30811,#30812,#30813,#30814,#30815,#30816),
 .UNSPECIFIED.,.F.,.F.,(4,1,1,1,1,1,1,1,1,1,1,1,1,4),(59.6902604182062,
60.0849739965977,60.582149101075,61.0793242055522,61.5764993100294,62.0736744145066,
62.5708495189838,63.068024623461,63.5651997279382,64.0623748324155,64.5595499368927,
65.0567250413699,65.5539001458471,65.9734457253859),.UNSPECIFIED.);
#837=B_SPLINE_CURVE_WITH_KNOTS('',3,(#30817,#30818,#30819,#30820,#30821,
#30822,#30823,#30824,#30825,#30826,#30827,#30828,#30829,#30830,#30831,#30832),
 .UNSPECIFIED.,.F.,.F.,(4,1,1,1,1,1,1,1,1,1,1,1,1,4),(59.6902604182062,
60.1390538786847,60.6362289831619,61.1334040876391,61.6305791921163,62.1277542965935,
62.6249294010708,63.122104505548,63.6192796100252,64.1164547145024,64.6136298189796,
65.1108049234568,65.607980027934,65.9734457253859),.UNSPECIFIED.);
#838=B_SPLINE_CURVE_WITH_KNOTS('',3,(#30837,#30838,#30839,#30840,#30841,
#30842,#30843,#30844,#30845,#30846,#30847,#30848,#30849,#30850,#30851,#30852,
#30853),.UNSPECIFIED.,.F.,.F.,(4,1,1,1,1,1,1,1,1,1,1,1,1,1,4),(53.4070751110266,
53.621697638394,54.1188727428712,54.6160478473484,55.1132229518256,55.6103980563028,
56.10757316078,56.6047482652572,57.1019233697345,57.5990984742117,58.0962735786889,
58.5934486831661,59.0906237876433,59.5877988921205,59.6902604182062),
 .UNSPECIFIED.);
#839=B_SPLINE_CURVE_WITH_KNOTS('',3,(#30854,#30855,#30856,#30857,#30858,
#30859,#30860,#30861,#30862,#30863,#30864,#30865,#30866,#30867,#30868,#30869,
#30870),.UNSPECIFIED.,.F.,.F.,(4,1,1,1,1,1,1,1,1,1,1,1,1,1,4),(53.4070751110266,
53.6757775204809,54.1729526249581,54.6701277294353,55.1673028339125,55.6644779383898,
56.161653042867,56.6588281473442,57.1560032518214,57.6531783562986,58.1503534607758,
58.647528565253,59.1447036697303,59.6418787742075,59.6902604182062),
 .UNSPECIFIED.);
#840=B_SPLINE_CURVE_WITH_KNOTS('',3,(#30875,#30876,#30877,#30878,#30879,
#30880,#30881,#30882,#30883,#30884,#30885,#30886,#30887,#30888,#30889,#30890,
#30891),.UNSPECIFIED.,.F.,.F.,(4,1,1,1,1,1,1,1,1,1,1,1,1,1,4),(47.1238898038469,
47.1584212801902,47.6555963846674,48.1527714891446,48.6499465936218,49.147121698099,
49.6442968025762,50.1414719070535,50.6386470115307,51.1358221160079,51.6329972204851,
52.1301723249623,52.6273474294395,53.1245225339167,53.4070751110266),
 .UNSPECIFIED.);
#841=B_SPLINE_CURVE_WITH_KNOTS('',3,(#30892,#30893,#30894,#30895,#30896,
#30897,#30898,#30899,#30900,#30901,#30902,#30903,#30904,#30905,#30906,#30907,
#30908),.UNSPECIFIED.,.F.,.F.,(4,1,1,1,1,1,1,1,1,1,1,1,1,1,4),(47.1238898038469,
47.2125011622771,47.7096762667543,48.2068513712315,48.7040264757088,49.201201580186,
49.6983766846632,50.1955517891404,50.6927268936176,51.1899019980948,51.687077102572,
52.1842522070493,52.6814273115265,53.1786024160037,53.4070751110266),
 .UNSPECIFIED.);
#842=B_SPLINE_CURVE_WITH_KNOTS('',3,(#30913,#30914,#30915,#30916,#30917,
#30918,#30919,#30920,#30921,#30922,#30923,#30924,#30925,#30926,#30927,#30928),
 .UNSPECIFIED.,.F.,.F.,(4,1,1,1,1,1,1,1,1,1,1,1,1,4),(40.8407044966672,
41.1923200264636,41.6894951309408,42.186670235418,42.6838453398952,43.1810204443725,
43.6781955488497,44.1753706533269,44.6725457578041,45.1697208622813,45.6668959667585,
46.1640710712357,46.661246175713,47.1238898038469),.UNSPECIFIED.);
#843=B_SPLINE_CURVE_WITH_KNOTS('',3,(#30929,#30930,#30931,#30932,#30933,
#30934,#30935,#30936,#30937,#30938,#30939,#30940,#30941,#30942,#30943,#30944),
 .UNSPECIFIED.,.F.,.F.,(4,1,1,1,1,1,1,1,1,1,1,1,1,4),(40.8407044966672,
41.2463999085505,41.7435750130278,42.240750117505,42.7379252219822,43.2351003264594,
43.7322754309366,44.2294505354138,44.726625639891,45.2238007443683,45.7209758488455,
46.2181509533227,46.7153260577999,47.1238898038469),.UNSPECIFIED.);
#844=B_SPLINE_CURVE_WITH_KNOTS('',3,(#30949,#30950,#30951,#30952,#30953,
#30954,#30955,#30956,#30957,#30958,#30959,#30960,#30961,#30962,#30963,#30964,
#30965),.UNSPECIFIED.,.F.,.F.,(4,1,1,1,1,1,1,1,1,1,1,1,1,1,4),(34.557519189488,
34.7290436682598,35.226218772737,35.7233938772142,36.2205689816915,36.7177440861687,
37.2149191906459,37.7120942951231,38.2092693996003,38.7064445040775,39.2036196085547,
39.700794713032,40.1979698175092,40.6951449219864,40.8407044966672),
 .UNSPECIFIED.);
#845=B_SPLINE_CURVE_WITH_KNOTS('',3,(#30966,#30967,#30968,#30969,#30970,
#30971,#30972,#30973,#30974,#30975,#30976,#30977,#30978,#30979,#30980,#30981,
#30982),.UNSPECIFIED.,.F.,.F.,(4,1,1,1,1,1,1,1,1,1,1,1,1,1,4),(34.557519189488,
34.7831235503468,35.280298654824,35.7774737593012,36.2746488637784,36.7718239682556,
37.2689990727328,37.76617417721,38.2633492816873,38.7605243861645,39.2576994906417,
39.7548745951189,40.2520496995961,40.7492248040733,40.8407044966672),
 .UNSPECIFIED.);
#846=B_SPLINE_CURVE_WITH_KNOTS('',3,(#30987,#30988,#30989,#30990,#30991,
#30992,#30993,#30994,#30995,#30996,#30997,#30998,#30999,#31000,#31001,#31002),
 .UNSPECIFIED.,.F.,.F.,(4,1,1,1,1,1,1,1,1,1,1,1,1,4),(28.2743338823083,
28.7629424145332,29.2601175190104,29.7572926234877,30.2544677279649,30.7516428324421,
31.2488179369193,31.7459930413965,32.2431681458737,32.7403432503509,33.2375183548282,
33.7346934593054,34.2318685637826,34.557519189488),.UNSPECIFIED.);
#847=B_SPLINE_CURVE_WITH_KNOTS('',3,(#31003,#31004,#31005,#31006,#31007,
#31008,#31009,#31010,#31011,#31012,#31013,#31014,#31015,#31016,#31017,#31018,
#31019),.UNSPECIFIED.,.F.,.F.,(4,1,1,1,1,1,1,1,1,1,1,1,1,1,4),(28.2743338823083,
28.319847192143,28.8170222966202,29.3141974010974,29.8113725055746,30.3085476100518,
30.805722714529,31.3028978190063,31.8000729234835,32.2972480279607,32.7944231324379,
33.2915982369151,33.7887733413923,34.2859484458695,34.557519189488),
 .UNSPECIFIED.);
#848=B_SPLINE_CURVE_WITH_KNOTS('',3,(#31024,#31025,#31026,#31027,#31028,
#31029,#31030,#31031,#31032,#31033,#31034,#31035,#31036,#31037,#31038,#31039,
#31040),.UNSPECIFIED.,.F.,.F.,(4,1,1,1,1,1,1,1,1,1,1,1,1,1,4),(21.9911485751286,
22.2996660563294,22.7968411608067,23.2940162652839,23.7911913697611,24.2883664742383,
24.7855415787155,25.2827166831927,25.7798917876699,26.2770668921472,26.7742419966244,
27.2714171011016,27.7685922055788,28.265767310056,28.2743338823083),
 .UNSPECIFIED.);
#849=B_SPLINE_CURVE_WITH_KNOTS('',3,(#31041,#31042,#31043,#31044,#31045,
#31046,#31047,#31048,#31049,#31050,#31051,#31052,#31053,#31054,#31055,#31056),
 .UNSPECIFIED.,.F.,.F.,(4,1,1,1,1,1,1,1,1,1,1,1,1,4),(21.9911485751286,
22.3537459384164,22.8509210428936,23.3480961473708,23.845271251848,24.3424463563253,
24.8396214608025,25.3367965652797,25.8339716697569,26.3311467742341,26.8283218787113,
27.3254969831885,27.8226720876658,28.2743338823083),.UNSPECIFIED.);
#850=B_SPLINE_CURVE_WITH_KNOTS('',3,(#31062,#31063,#31064,#31065,#31066,
#31067),.UNSPECIFIED.,.F.,.F.,(4,1,1,4),(14.398944266781,14.8961193712582,
15.3932944757354,15.707963267949),.UNSPECIFIED.);
#851=B_SPLINE_CURVE_WITH_KNOTS('',3,(#31070,#31071,#31072,#31073,#31074,
#31075,#31076),.UNSPECIFIED.,.F.,.F.,(4,1,1,1,4),(13.8753896155273,14.344864384694,
14.8420394891712,15.3392145936484,15.707963267949),.UNSPECIFIED.);
#852=B_SPLINE_CURVE_WITH_KNOTS('',3,(#31082,#31083,#31084,#31085,#31086,
#31087,#31088),.UNSPECIFIED.,.F.,.F.,(4,3,4),(252.636431288351,252.845104747016,
253.343813040403),.UNSPECIFIED.);
#853=B_SPLINE_CURVE_WITH_KNOTS('',3,(#31096,#31097,#31098,#31099,#31100,
#31101,#31102,#31103,#31104,#31105,#31106,#31107,#31108,#31109,#31110,#31111),
 .UNSPECIFIED.,.F.,.F.,(4,3,3,3,3,4),(-251.327412287183,-250.85027157347,
-250.351563280083,-249.852854986696,-249.35414669331,-248.893201385645),
 .UNSPECIFIED.);
#854=B_SPLINE_CURVE_WITH_KNOTS('',3,(#31116,#31117,#31118,#31119,#31120,
#31121,#31122,#31123,#31124,#31125,#31126,#31127,#31128,#31129,#31130,#31131,
#31132,#31133,#31134,#31135,#31136,#31137,#31138,#31139,#31140,#31141,#31142,
#31143,#31144,#31145,#31146,#31147,#31148,#31149,#31150,#31151,#31152,#31153,
#31154,#31155,#31156,#31157,#31158),.UNSPECIFIED.,.F.,.F.,(4,3,3,3,3,3,
3,3,3,3,3,3,3,3,4),(246.353245981172,246.36189693299,246.860605226377,247.359313519763,
247.85802181315,248.356730106537,248.855438399923,249.35414669331,249.852854986696,
250.351563280083,250.85027157347,251.348979866856,251.847688160243,252.346396453629,
252.636431288351),.UNSPECIFIED.);
#855=B_SPLINE_CURVE_WITH_KNOTS('',3,(#31159,#31160,#31161,#31162,#31163,
#31164,#31165,#31166,#31167,#31168,#31169,#31170,#31171,#31172,#31173,#31174,
#31175,#31176,#31177,#31178,#31179,#31180,#31181,#31182,#31183,#31184,#31185,
#31186,#31187,#31188,#31189,#31190,#31191,#31192,#31193,#31194,#31195,#31196,
#31197,#31198,#31199,#31200,#31201),.UNSPECIFIED.,.F.,.F.,(4,3,3,3,3,3,
3,3,3,3,3,3,3,3,4),(-248.893201385645,-248.855438399923,-248.356730106536,
-247.85802181315,-247.359313519763,-246.860605226377,-246.36189693299,-245.863188639603,
-245.364480346217,-244.86577205283,-244.367063759444,-243.868355466057,
-243.36964717267,-242.870938879284,-242.610016078465),.UNSPECIFIED.);
#856=B_SPLINE_CURVE_WITH_KNOTS('',3,(#31206,#31207,#31208,#31209,#31210,
#31211,#31212,#31213,#31214,#31215,#31216,#31217,#31218,#31219,#31220,#31221,
#31222,#31223,#31224,#31225,#31226,#31227,#31228,#31229,#31230,#31231,#31232,
#31233,#31234,#31235,#31236,#31237,#31238,#31239,#31240,#31241,#31242,#31243,
#31244,#31245),.UNSPECIFIED.,.F.,.F.,(4,3,3,3,3,3,3,3,3,3,3,3,3,4),(240.070060673992,
240.377397412351,240.876105705737,241.374813999124,241.873522292511,242.372230585897,
242.870938879284,243.36964717267,243.868355466057,244.367063759444,244.86577205283,
245.364480346217,245.863188639603,246.353245981172),.UNSPECIFIED.);
#857=B_SPLINE_CURVE_WITH_KNOTS('',3,(#31246,#31247,#31248,#31249,#31250,
#31251,#31252,#31253,#31254,#31255,#31256,#31257,#31258,#31259,#31260,#31261,
#31262,#31263,#31264,#31265,#31266,#31267,#31268,#31269,#31270,#31271,#31272,
#31273,#31274,#31275,#31276,#31277,#31278,#31279,#31280,#31281,#31282,#31283,
#31284,#31285,#31286,#31287,#31288),.UNSPECIFIED.,.F.,.F.,(4,3,3,3,3,3,
3,3,3,3,3,3,3,3,4),(-242.610016078465,-242.372230585897,-241.87352229251,
-241.374813999124,-240.876105705737,-240.377397412351,-239.878689118964,
-239.379980825577,-238.881272532191,-238.382564238804,-237.883855945417,
-237.385147652031,-236.886439358644,-236.387731065258,-236.326830771286),
 .UNSPECIFIED.);
#858=B_SPLINE_CURVE_WITH_KNOTS('',3,(#31293,#31294,#31295,#31296,#31297,
#31298,#31299,#31300,#31301,#31302,#31303,#31304,#31305,#31306,#31307,#31308,
#31309,#31310,#31311,#31312,#31313,#31314,#31315,#31316,#31317,#31318,#31319,
#31320,#31321,#31322,#31323,#31324,#31325,#31326,#31327,#31328,#31329,#31330,
#31331,#31332,#31333,#31334,#31335),.UNSPECIFIED.,.F.,.F.,(4,3,3,3,3,3,
3,3,3,3,3,3,3,3,4),(233.786875366813,233.894189598325,234.392897891711,
234.891606185098,235.390314478484,235.889022771871,236.387731065258,236.886439358644,
237.385147652031,237.883855945418,238.382564238804,238.881272532191,239.379980825577,
239.878689118964,240.070060673992),.UNSPECIFIED.);
#859=B_SPLINE_CURVE_WITH_KNOTS('',3,(#31336,#31337,#31338,#31339,#31340,
#31341,#31342,#31343,#31344,#31345,#31346,#31347,#31348,#31349,#31350,#31351,
#31352,#31353,#31354,#31355,#31356,#31357,#31358,#31359,#31360,#31361,#31362,
#31363,#31364,#31365,#31366,#31367,#31368,#31369,#31370,#31371,#31372,#31373,
#31374,#31375),.UNSPECIFIED.,.F.,.F.,(4,3,3,3,3,3,3,3,3,3,3,3,3,4),(-236.326830771286,
-235.889022771871,-235.390314478484,-234.891606185098,-234.392897891711,
-233.894189598325,-233.395481304938,-232.896773011551,-232.398064718165,
-231.899356424778,-231.400648131391,-230.901939838005,-230.403231544618,
-230.043645464106),.UNSPECIFIED.);
#860=B_SPLINE_CURVE_WITH_KNOTS('',3,(#31380,#31381,#31382,#31383,#31384,
#31385,#31386,#31387,#31388,#31389,#31390,#31391,#31392,#31393,#31394,#31395,
#31396,#31397,#31398,#31399,#31400,#31401,#31402,#31403,#31404,#31405,#31406,
#31407,#31408,#31409,#31410,#31411,#31412,#31413,#31414,#31415,#31416,#31417,
#31418,#31419),.UNSPECIFIED.,.F.,.F.,(4,3,3,3,3,3,3,3,3,3,3,3,3,4),(227.503690059633,
227.909690077685,228.408398371072,228.907106664458,229.405814957845,229.904523251232,
230.403231544618,230.901939838005,231.400648131391,231.899356424778,232.398064718165,
232.896773011551,233.395481304938,233.786875366813),.UNSPECIFIED.);
#861=B_SPLINE_CURVE_WITH_KNOTS('',3,(#31420,#31421,#31422,#31423,#31424,
#31425,#31426,#31427,#31428,#31429,#31430,#31431,#31432,#31433,#31434,#31435,
#31436,#31437,#31438,#31439,#31440,#31441,#31442,#31443,#31444,#31445,#31446,
#31447,#31448,#31449,#31450,#31451,#31452,#31453,#31454,#31455,#31456,#31457,
#31458,#31459,#31460,#31461,#31462),.UNSPECIFIED.,.F.,.F.,(4,3,3,3,3,3,
3,3,3,3,3,3,3,3,4),(-230.043645464106,-229.904523251232,-229.405814957845,
-228.907106664458,-228.408398371072,-227.909690077685,-227.410981784298,
-226.912273490912,-226.413565197525,-225.914856904139,-225.416148610752,
-224.917440317365,-224.418732023979,-223.920023730592,-223.760460156926),
 .UNSPECIFIED.);
#862=B_SPLINE_CURVE_WITH_KNOTS('',3,(#31467,#31468,#31469,#31470,#31471,
#31472,#31473,#31474,#31475,#31476,#31477,#31478,#31479,#31480,#31481,#31482,
#31483,#31484,#31485,#31486,#31487,#31488,#31489,#31490,#31491,#31492,#31493,
#31494,#31495,#31496,#31497,#31498,#31499,#31500,#31501,#31502,#31503,#31504,
#31505,#31506,#31507,#31508,#31509),.UNSPECIFIED.,.F.,.F.,(4,3,3,3,3,3,
3,3,3,3,3,3,3,3,4),(221.220504752453,221.426482263659,221.925190557046,
222.423898850432,222.922607143819,223.421315437206,223.920023730592,224.418732023979,
224.917440317365,225.416148610752,225.914856904139,226.413565197525,226.912273490912,
227.410981784299,227.503690059633),.UNSPECIFIED.);
#863=B_SPLINE_CURVE_WITH_KNOTS('',3,(#31510,#31511,#31512,#31513,#31514,
#31515,#31516,#31517,#31518,#31519,#31520,#31521,#31522,#31523,#31524,#31525,
#31526,#31527,#31528,#31529,#31530,#31531,#31532,#31533,#31534,#31535,#31536,
#31537,#31538,#31539,#31540,#31541,#31542,#31543,#31544,#31545,#31546,#31547,
#31548,#31549),.UNSPECIFIED.,.F.,.F.,(4,3,3,3,3,3,3,3,3,3,3,3,3,4),(-223.760460156926,
-223.421315437206,-222.922607143819,-222.423898850432,-221.925190557046,
-221.426482263659,-220.927773970272,-220.429065676886,-219.930357383499,
-219.431649090113,-218.932940796726,-218.434232503339,-217.935524209953,
-217.477274849747),.UNSPECIFIED.);
#864=B_SPLINE_CURVE_WITH_KNOTS('',3,(#31554,#31555,#31556,#31557,#31558,
#31559,#31560,#31561,#31562,#31563,#31564,#31565,#31566,#31567,#31568,#31569,
#31570,#31571,#31572,#31573,#31574,#31575,#31576,#31577,#31578,#31579,#31580,
#31581,#31582,#31583,#31584,#31585,#31586,#31587,#31588,#31589,#31590,#31591,
#31592,#31593,#31594,#31595,#31596),.UNSPECIFIED.,.F.,.F.,(4,3,3,3,3,3,
3,3,3,3,3,3,3,3,4),(214.937319445274,214.943274449633,215.44198274302,215.940691036406,
216.439399329793,216.93810762318,217.436815916566,217.935524209953,218.434232503339,
218.932940796726,219.431649090113,219.930357383499,220.429065676886,220.927773970272,
221.220504752453),.UNSPECIFIED.);
#865=B_SPLINE_CURVE_WITH_KNOTS('',3,(#31597,#31598,#31599,#31600,#31601,
#31602,#31603,#31604,#31605,#31606,#31607,#31608,#31609,#31610,#31611,#31612,
#31613,#31614,#31615,#31616,#31617,#31618,#31619,#31620,#31621,#31622,#31623,
#31624,#31625,#31626,#31627,#31628,#31629,#31630,#31631,#31632,#31633,#31634,
#31635,#31636,#31637,#31638,#31639),.UNSPECIFIED.,.F.,.F.,(4,3,3,3,3,3,
3,3,3,3,3,3,3,3,4),(-217.477274849747,-217.436815916566,-216.938107623179,
-216.439399329793,-215.940691036406,-215.44198274302,-214.943274449633,
-214.444566156246,-213.94585786286,-213.447149569473,-212.948441276087,
-212.4497329827,-211.951024689313,-211.452316395927,-211.194089542567),
 .UNSPECIFIED.);
#866=B_SPLINE_CURVE_WITH_KNOTS('',3,(#31644,#31645,#31646,#31647,#31648,
#31649,#31650,#31651,#31652,#31653,#31654,#31655,#31656,#31657,#31658,#31659,
#31660,#31661,#31662,#31663,#31664,#31665,#31666,#31667,#31668,#31669,#31670,
#31671,#31672,#31673,#31674,#31675,#31676,#31677,#31678,#31679,#31680,#31681,
#31682,#31683),.UNSPECIFIED.,.F.,.F.,(4,3,3,3,3,3,3,3,3,3,3,3,3,4),(208.654134138094,
208.958774928994,209.45748322238,209.956191515767,210.454899809153,210.95360810254,
211.452316395927,211.951024689313,212.4497329827,212.948441276087,213.447149569473,
213.94585786286,214.444566156246,214.937319445274),.UNSPECIFIED.);
#867=B_SPLINE_CURVE_WITH_KNOTS('',3,(#31684,#31685,#31686,#31687,#31688,
#31689,#31690,#31691,#31692,#31693,#31694,#31695,#31696,#31697,#31698,#31699,
#31700,#31701,#31702,#31703,#31704,#31705,#31706,#31707,#31708,#31709,#31710,
#31711,#31712,#31713,#31714,#31715,#31716,#31717,#31718,#31719,#31720,#31721,
#31722,#31723,#31724,#31725,#31726),.UNSPECIFIED.,.F.,.F.,(4,3,3,3,3,3,
3,3,3,3,3,3,3,3,4),(-211.194089542567,-210.95360810254,-210.454899809153,
-209.956191515767,-209.45748322238,-208.958774928994,-208.460066635607,
-207.96135834222,-207.462650048834,-206.963941755447,-206.46523346206,-205.966525168674,
-205.467816875287,-204.969108581901,-204.910904235388),.UNSPECIFIED.);
#868=B_SPLINE_CURVE_WITH_KNOTS('',3,(#31731,#31732,#31733,#31734,#31735,
#31736,#31737,#31738,#31739,#31740,#31741,#31742,#31743,#31744,#31745,#31746,
#31747,#31748,#31749,#31750,#31751,#31752,#31753,#31754,#31755,#31756,#31757,
#31758,#31759,#31760,#31761,#31762,#31763,#31764,#31765,#31766,#31767,#31768,
#31769,#31770,#31771,#31772,#31773),.UNSPECIFIED.,.F.,.F.,(4,3,3,3,3,3,
3,3,3,3,3,3,3,3,4),(202.370948830915,202.475567114968,202.974275408354,
203.472983701741,203.971691995127,204.470400288514,204.969108581901,205.467816875287,
205.966525168674,206.46523346206,206.963941755447,207.462650048834,207.96135834222,
208.460066635607,208.654134138094),.UNSPECIFIED.);
#869=B_SPLINE_CURVE_WITH_KNOTS('',3,(#31774,#31775,#31776,#31777,#31778,
#31779,#31780,#31781,#31782,#31783,#31784,#31785,#31786,#31787,#31788,#31789,
#31790,#31791,#31792,#31793,#31794,#31795,#31796,#31797,#31798,#31799,#31800,
#31801,#31802,#31803,#31804,#31805,#31806,#31807,#31808,#31809,#31810,#31811,
#31812,#31813),.UNSPECIFIED.,.F.,.F.,(4,3,3,3,3,3,3,3,3,3,3,3,3,4),(-204.910904235388,
-204.470400288514,-203.971691995127,-203.472983701741,-202.974275408354,
-202.475567114968,-201.976858821581,-201.478150528194,-200.979442234808,
-200.480733941421,-199.982025648034,-199.483317354648,-198.984609061261,
-198.627718928208),.UNSPECIFIED.);
#870=B_SPLINE_CURVE_WITH_KNOTS('',3,(#31818,#31819,#31820,#31821,#31822,
#31823,#31824,#31825,#31826,#31827,#31828,#31829,#31830,#31831,#31832,#31833,
#31834,#31835,#31836,#31837,#31838,#31839,#31840,#31841,#31842,#31843,#31844,
#31845,#31846,#31847,#31848,#31849,#31850,#31851,#31852,#31853,#31854,#31855,
#31856,#31857),.UNSPECIFIED.,.F.,.F.,(4,3,3,3,3,3,3,3,3,3,3,3,3,4),(196.087763523735,
196.491067594328,196.989775887715,197.488484181101,197.987192474488,198.485900767875,
198.984609061261,199.483317354648,199.982025648034,200.480733941421,200.979442234808,
201.478150528194,201.976858821581,202.370948830915),.UNSPECIFIED.);
#871=B_SPLINE_CURVE_WITH_KNOTS('',3,(#31858,#31859,#31860,#31861,#31862,
#31863,#31864,#31865,#31866,#31867,#31868,#31869,#31870,#31871,#31872,#31873,
#31874,#31875,#31876,#31877,#31878,#31879,#31880,#31881,#31882,#31883,#31884,
#31885,#31886,#31887,#31888,#31889,#31890,#31891,#31892,#31893,#31894,#31895,
#31896,#31897,#31898,#31899,#31900),.UNSPECIFIED.,.F.,.F.,(4,3,3,3,3,3,
3,3,3,3,3,3,3,3,4),(-198.627718928208,-198.485900767875,-197.987192474488,
-197.488484181101,-196.989775887715,-196.491067594328,-195.992359300941,
-195.493651007555,-194.994942714168,-194.496234420782,-193.997526127395,
-193.498817834008,-193.000109540622,-192.501401247235,-192.344533621029),
 .UNSPECIFIED.);
#872=B_SPLINE_CURVE_WITH_KNOTS('',3,(#31905,#31906,#31907,#31908,#31909,
#31910,#31911,#31912,#31913,#31914,#31915,#31916,#31917,#31918,#31919,#31920,
#31921,#31922,#31923,#31924,#31925,#31926,#31927,#31928,#31929,#31930,#31931,
#31932,#31933,#31934,#31935,#31936,#31937,#31938,#31939,#31940,#31941,#31942,
#31943,#31944,#31945,#31946,#31947),.UNSPECIFIED.,.F.,.F.,(4,3,3,3,3,3,
3,3,3,3,3,3,3,3,4),(189.804578216556,190.007859780302,190.506568073689,
191.005276367075,191.503984660462,192.002692953849,192.501401247235,193.000109540622,
193.498817834008,193.997526127395,194.496234420782,194.994942714168,195.493651007555,
195.992359300941,196.087763523735),.UNSPECIFIED.);
#873=B_SPLINE_CURVE_WITH_KNOTS('',3,(#31948,#31949,#31950,#31951,#31952,
#31953,#31954,#31955,#31956,#31957,#31958,#31959,#31960,#31961,#31962,#31963,
#31964,#31965,#31966,#31967,#31968,#31969,#31970,#31971,#31972,#31973,#31974,
#31975,#31976,#31977,#31978,#31979,#31980,#31981,#31982,#31983,#31984,#31985,
#31986,#31987),.UNSPECIFIED.,.F.,.F.,(4,3,3,3,3,3,3,3,3,3,3,3,3,4),(-192.344533621029,
-192.002692953848,-191.503984660462,-191.005276367075,-190.506568073689,
-190.007859780302,-189.509151486915,-189.010443193529,-188.511734900142,
-188.013026606756,-187.514318313369,-187.015610019982,-186.516901726596,
-186.061348313849),.UNSPECIFIED.);
#874=B_SPLINE_CURVE_WITH_KNOTS('',3,(#31992,#31993,#31994,#31995,#31996,
#31997,#31998,#31999,#32000,#32001,#32002,#32003,#32004,#32005,#32006,#32007,
#32008,#32009,#32010,#32011,#32012,#32013,#32014,#32015,#32016,#32017,#32018,
#32019,#32020,#32021,#32022,#32023,#32024,#32025,#32026,#32027,#32028,#32029,
#32030,#32031,#32032,#32033,#32034),.UNSPECIFIED.,.F.,.F.,(4,3,3,3,3,3,
3,3,3,3,3,3,3,3,4),(183.521392909376,183.524651966276,184.023360259663,
184.522068553049,185.020776846436,185.519485139823,186.018193433209,186.516901726596,
187.015610019982,187.514318313369,188.013026606756,188.511734900142,189.010443193529,
189.509151486915,189.804578216556),.UNSPECIFIED.);
#875=B_SPLINE_CURVE_WITH_KNOTS('',3,(#32035,#32036,#32037,#32038,#32039,
#32040,#32041,#32042,#32043,#32044,#32045,#32046,#32047,#32048,#32049,#32050,
#32051,#32052,#32053,#32054,#32055,#32056,#32057,#32058,#32059,#32060,#32061,
#32062,#32063,#32064,#32065,#32066,#32067,#32068,#32069,#32070,#32071,#32072,
#32073,#32074,#32075,#32076,#32077),.UNSPECIFIED.,.F.,.F.,(4,3,3,3,3,3,
3,3,3,3,3,3,3,3,4),(-186.061348313849,-186.018193433209,-185.519485139822,
-185.020776846436,-184.522068553049,-184.023360259663,-183.524651966276,
-183.025943672889,-182.527235379503,-182.028527086116,-181.529818792729,
-181.031110499343,-180.532402205956,-180.03369391257,-179.77816300667),
 .UNSPECIFIED.);
#876=B_SPLINE_CURVE_WITH_KNOTS('',3,(#32082,#32083,#32084,#32085,#32086,
#32087,#32088,#32089,#32090,#32091,#32092,#32093,#32094,#32095,#32096,#32097,
#32098,#32099,#32100,#32101,#32102,#32103,#32104,#32105,#32106,#32107,#32108,
#32109,#32110,#32111,#32112,#32113,#32114,#32115,#32116,#32117,#32118,#32119,
#32120,#32121),.UNSPECIFIED.,.F.,.F.,(4,3,3,3,3,3,3,3,3,3,3,3,3,4),(177.238207602196,
177.540152445637,178.038860739023,178.53756903241,179.036277325796,179.534985619183,
180.03369391257,180.532402205956,181.031110499343,181.52981879273,182.028527086116,
182.527235379503,183.025943672889,183.521392909376),.UNSPECIFIED.);
#877=B_SPLINE_CURVE_WITH_KNOTS('',3,(#32122,#32123,#32124,#32125,#32126,
#32127,#32128,#32129,#32130,#32131,#32132,#32133,#32134,#32135,#32136,#32137,
#32138,#32139,#32140,#32141,#32142,#32143,#32144,#32145,#32146,#32147,#32148,
#32149,#32150,#32151,#32152,#32153,#32154,#32155,#32156,#32157,#32158,#32159,
#32160,#32161,#32162,#32163,#32164),.UNSPECIFIED.,.F.,.F.,(4,3,3,3,3,3,
3,3,3,3,3,3,3,3,4),(-179.77816300667,-179.534985619183,-179.036277325796,
-178.53756903241,-178.038860739023,-177.540152445637,-177.04144415225,-176.542735858863,
-176.044027565477,-175.54531927209,-175.046610978703,-174.547902685317,
-174.04919439193,-173.550486098544,-173.49497769949),.UNSPECIFIED.);
#878=B_SPLINE_CURVE_WITH_KNOTS('',3,(#32169,#32170,#32171,#32172,#32173,
#32174,#32175,#32176,#32177,#32178,#32179,#32180,#32181,#32182,#32183,#32184,
#32185,#32186,#32187,#32188,#32189,#32190,#32191,#32192,#32193,#32194,#32195,
#32196,#32197,#32198,#32199,#32200,#32201,#32202,#32203,#32204,#32205,#32206,
#32207,#32208,#32209,#32210,#32211),.UNSPECIFIED.,.F.,.F.,(4,3,3,3,3,3,
3,3,3,3,3,3,3,3,4),(170.955022295017,171.056944631611,171.555652924997,
172.054361218384,172.55306951177,173.051777805157,173.550486098544,174.04919439193,
174.547902685317,175.046610978703,175.54531927209,176.044027565477,176.542735858863,
177.04144415225,177.238207602196),.UNSPECIFIED.);
#879=B_SPLINE_CURVE_WITH_KNOTS('',3,(#32212,#32213,#32214,#32215,#32216,
#32217,#32218,#32219,#32220,#32221,#32222,#32223,#32224,#32225,#32226,#32227,
#32228,#32229,#32230,#32231,#32232,#32233,#32234,#32235,#32236,#32237,#32238,
#32239,#32240,#32241,#32242,#32243,#32244,#32245,#32246,#32247,#32248,#32249,
#32250,#32251),.UNSPECIFIED.,.F.,.F.,(4,3,3,3,3,3,3,3,3,3,3,3,3,4),(-173.49497769949,
-173.051777805157,-172.55306951177,-172.054361218384,-171.555652924997,
-171.05694463161,-170.558236338224,-170.059528044837,-169.560819751451,
-169.062111458064,-168.563403164677,-168.064694871291,-167.565986577904,
-167.21179239231),.UNSPECIFIED.);
#880=B_SPLINE_CURVE_WITH_KNOTS('',3,(#32256,#32257,#32258,#32259,#32260,
#32261,#32262,#32263,#32264,#32265,#32266,#32267,#32268,#32269,#32270,#32271,
#32272,#32273,#32274,#32275,#32276,#32277,#32278,#32279,#32280,#32281,#32282,
#32283,#32284,#32285,#32286,#32287,#32288,#32289,#32290,#32291,#32292,#32293,
#32294,#32295),.UNSPECIFIED.,.F.,.F.,(4,3,3,3,3,3,3,3,3,3,3,3,3,4),(164.671836987837,
165.072445110971,165.571153404358,166.069861697744,166.568569991131,167.067278284518,
167.565986577904,168.064694871291,168.563403164677,169.062111458064,169.560819751451,
170.059528044837,170.558236338224,170.955022295017),.UNSPECIFIED.);
#881=B_SPLINE_CURVE_WITH_KNOTS('',3,(#32296,#32297,#32298,#32299,#32300,
#32301,#32302,#32303,#32304,#32305,#32306,#32307,#32308,#32309,#32310,#32311,
#32312,#32313,#32314,#32315,#32316,#32317,#32318,#32319,#32320,#32321,#32322,
#32323,#32324,#32325,#32326,#32327,#32328,#32329,#32330,#32331,#32332,#32333,
#32334,#32335,#32336,#32337,#32338),.UNSPECIFIED.,.F.,.F.,(4,3,3,3,3,3,
3,3,3,3,3,3,3,3,4),(-167.21179239231,-167.067278284517,-166.568569991131,
-166.069861697744,-165.571153404358,-165.072445110971,-164.573736817584,
-164.075028524198,-163.576320230811,-163.077611937425,-162.578903644038,
-162.080195350651,-161.581487057265,-161.082778763878,-160.928607085131),
 .UNSPECIFIED.);
#882=B_SPLINE_CURVE_WITH_KNOTS('',3,(#32343,#32344,#32345,#32346,#32347,
#32348,#32349,#32350,#32351,#32352,#32353,#32354,#32355,#32356,#32357,#32358,
#32359,#32360,#32361,#32362,#32363,#32364,#32365,#32366,#32367,#32368,#32369,
#32370,#32371,#32372,#32373,#32374,#32375,#32376,#32377,#32378,#32379,#32380,
#32381,#32382,#32383,#32384,#32385),.UNSPECIFIED.,.F.,.F.,(4,3,3,3,3,3,
3,3,3,3,3,3,3,3,4),(158.388651680658,158.589237296945,159.087945590332,
159.586653883718,160.085362177105,160.584070470491,161.082778763878,161.581487057265,
162.080195350651,162.578903644038,163.077611937425,163.576320230811,164.075028524198,
164.573736817584,164.671836987837),.UNSPECIFIED.);
#883=B_SPLINE_CURVE_WITH_KNOTS('',3,(#32386,#32387,#32388,#32389,#32390,
#32391,#32392,#32393,#32394,#32395,#32396,#32397,#32398,#32399,#32400,#32401,
#32402,#32403,#32404,#32405,#32406,#32407,#32408,#32409,#32410,#32411,#32412,
#32413,#32414,#32415,#32416,#32417,#32418,#32419,#32420,#32421,#32422,#32423,
#32424,#32425),.UNSPECIFIED.,.F.,.F.,(4,3,3,3,3,3,3,3,3,3,3,3,3,4),(-160.928607085131,
-160.584070470491,-160.085362177105,-159.586653883718,-159.087945590332,
-158.589237296945,-158.090529003558,-157.591820710172,-157.093112416785,
-156.594404123399,-156.095695830012,-155.596987536625,-155.098279243239,
-154.645421777951),.UNSPECIFIED.);
#884=B_SPLINE_CURVE_WITH_KNOTS('',3,(#32430,#32431,#32432,#32433,#32434,
#32435,#32436,#32437,#32438,#32439,#32440,#32441,#32442,#32443,#32444,#32445,
#32446,#32447,#32448,#32449,#32450,#32451,#32452,#32453,#32454,#32455,#32456,
#32457,#32458,#32459,#32460,#32461,#32462,#32463,#32464,#32465,#32466,#32467,
#32468,#32469),.UNSPECIFIED.,.F.,.F.,(4,3,3,3,3,3,3,3,3,3,3,3,3,4),(152.105466373478,
152.604737776306,153.103446069692,153.602154363079,154.100862656465,154.599570949852,
155.098279243239,155.596987536625,156.095695830012,156.594404123399,157.093112416785,
157.591820710172,158.090529003558,158.388651680658),.UNSPECIFIED.);
#885=B_SPLINE_CURVE_WITH_KNOTS('',3,(#32470,#32471,#32472,#32473,#32474,
#32475,#32476,#32477,#32478,#32479,#32480,#32481,#32482,#32483,#32484,#32485,
#32486,#32487,#32488,#32489,#32490,#32491,#32492,#32493,#32494,#32495,#32496,
#32497,#32498,#32499,#32500,#32501,#32502,#32503,#32504,#32505,#32506,#32507,
#32508,#32509,#32510,#32511,#32512),.UNSPECIFIED.,.F.,.F.,(4,3,3,3,3,3,
3,3,3,3,3,3,3,3,4),(-154.645421777951,-154.599570949852,-154.100862656465,
-153.602154363079,-153.103446069692,-152.604737776306,-152.106029482919,
-151.607321189532,-151.108612896146,-150.609904602759,-150.111196309372,
-149.612488015986,-149.113779722599,-148.615071429213,-148.362236470772),
 .UNSPECIFIED.);
#886=B_SPLINE_CURVE_WITH_KNOTS('',3,(#32517,#32518,#32519,#32520,#32521,
#32522,#32523,#32524,#32525,#32526,#32527,#32528,#32529,#32530,#32531,#32532,
#32533,#32534,#32535,#32536,#32537,#32538,#32539,#32540,#32541,#32542,#32543,
#32544,#32545,#32546,#32547,#32548,#32549,#32550,#32551,#32552,#32553,#32554,
#32555,#32556),.UNSPECIFIED.,.F.,.F.,(4,3,3,3,3,3,3,3,3,3,3,3,3,4),(145.822281066299,
146.121529962279,146.620238255666,147.118946549053,147.617654842439,148.116363135826,
148.615071429213,149.113779722599,149.612488015986,150.111196309372,150.609904602759,
151.108612896146,151.607321189532,152.105466373478),.UNSPECIFIED.);
#887=B_SPLINE_CURVE_WITH_KNOTS('',3,(#32557,#32558,#32559,#32560,#32561,
#32562,#32563,#32564,#32565,#32566,#32567,#32568,#32569,#32570,#32571,#32572,
#32573,#32574,#32575,#32576,#32577,#32578,#32579,#32580,#32581,#32582,#32583,
#32584,#32585,#32586,#32587,#32588,#32589,#32590,#32591,#32592,#32593,#32594,
#32595,#32596,#32597,#32598,#32599),.UNSPECIFIED.,.F.,.F.,(4,3,3,3,3,3,
3,3,3,3,3,3,3,3,4),(-148.362236470772,-148.116363135826,-147.617654842439,
-147.118946549053,-146.620238255666,-146.12152996228,-145.622821668893,
-145.124113375506,-144.62540508212,-144.126696788733,-143.627988495346,
-143.12928020196,-142.630571908573,-142.131863615187,-142.079051163592),
 .UNSPECIFIED.);
#888=B_SPLINE_CURVE_WITH_KNOTS('',3,(#32604,#32605,#32606,#32607,#32608,
#32609,#32610,#32611,#32612,#32613,#32614,#32615,#32616,#32617,#32618,#32619,
#32620,#32621,#32622,#32623,#32624,#32625,#32626,#32627,#32628,#32629,#32630,
#32631,#32632,#32633,#32634,#32635,#32636,#32637,#32638,#32639,#32640,#32641,
#32642,#32643,#32644,#32645,#32646),.UNSPECIFIED.,.F.,.F.,(4,3,3,3,3,3,
3,3,3,3,3,3,3,3,4),(139.539095759119,139.638322148253,140.13703044164,140.635738735027,
141.134447028413,141.6331553218,142.131863615187,142.630571908573,143.12928020196,
143.627988495346,144.126696788733,144.62540508212,145.124113375506,145.622821668893,
145.822281066299),.UNSPECIFIED.);
#889=B_SPLINE_CURVE_WITH_KNOTS('',3,(#32647,#32648,#32649,#32650,#32651,
#32652,#32653,#32654,#32655,#32656,#32657,#32658,#32659,#32660,#32661,#32662,
#32663,#32664,#32665,#32666,#32667,#32668,#32669,#32670,#32671,#32672,#32673,
#32674,#32675,#32676,#32677,#32678,#32679,#32680,#32681,#32682,#32683,#32684,
#32685,#32686),.UNSPECIFIED.,.F.,.F.,(4,3,3,3,3,3,3,3,3,3,3,3,3,4),(-142.079051163592,
-141.6331553218,-141.134447028413,-140.635738735027,-140.13703044164,-139.638322148253,
-139.139613854867,-138.64090556148,-138.142197268094,-137.643488974707,
-137.14478068132,-136.646072387934,-136.147364094547,-135.795865856413),
 .UNSPECIFIED.);
#890=B_SPLINE_CURVE_WITH_KNOTS('',3,(#32691,#32692,#32693,#32694,#32695,
#32696,#32697,#32698,#32699,#32700,#32701,#32702,#32703,#32704,#32705,#32706,
#32707,#32708,#32709,#32710,#32711,#32712,#32713,#32714,#32715,#32716,#32717,
#32718,#32719,#32720,#32721,#32722,#32723,#32724,#32725,#32726,#32727,#32728,
#32729,#32730),.UNSPECIFIED.,.F.,.F.,(4,3,3,3,3,3,3,3,3,3,3,3,3,4),(133.25591045194,
133.653822627614,134.152530921001,134.651239214387,135.149947507774,135.648655801161,
136.147364094547,136.646072387934,137.14478068132,137.643488974707,138.142197268094,
138.64090556148,139.139613854867,139.539095759119),.UNSPECIFIED.);
#891=B_SPLINE_CURVE_WITH_KNOTS('',3,(#32731,#32732,#32733,#32734,#32735,
#32736,#32737,#32738,#32739,#32740,#32741,#32742,#32743,#32744,#32745,#32746,
#32747,#32748,#32749,#32750,#32751,#32752,#32753,#32754,#32755,#32756,#32757,
#32758,#32759,#32760,#32761),.UNSPECIFIED.,.F.,.F.,(4,3,3,3,3,3,3,3,3,3,
4),(-135.795865856413,-135.648655801161,-135.149947507774,-134.651239214387,
-134.152530921001,-133.653822627614,-132.656406040841,-131.658989454068,
-130.661572867294,-129.664156280521,-129.512680549233),.UNSPECIFIED.);
#892=B_SPLINE_CURVE_WITH_KNOTS('',3,(#32766,#32767,#32768,#32769,#32770,
#32771,#32772,#32773,#32774,#32775,#32776,#32777,#32778,#32779,#32780,#32781,
#32782,#32783,#32784,#32785,#32786,#32787),.UNSPECIFIED.,.F.,.F.,(4,3,3,
3,3,3,3,4),(126.97272514476,127.669323106975,128.666739693748,129.664156280521,
130.661572867294,131.658989454068,132.656406040841,133.25591045194),
 .UNSPECIFIED.);
#893=B_SPLINE_CURVE_WITH_KNOTS('',3,(#32788,#32789,#32790,#32791,#32792,
#32793,#32794,#32795,#32796,#32797,#32798,#32799,#32800,#32801,#32802,#32803,
#32804,#32805,#32806,#32807,#32808,#32809),.UNSPECIFIED.,.F.,.F.,(4,3,3,
3,3,3,3,4),(-129.512680549233,-128.666739693748,-127.669323106975,-126.671906520201,
-125.674489933428,-124.677073346655,-123.679656759882,-123.229495242053),
 .UNSPECIFIED.);
#894=B_SPLINE_CURVE_WITH_KNOTS('',3,(#32814,#32815,#32816,#32817,#32818,
#32819,#32820,#32821,#32822,#32823,#32824,#32825,#32826,#32827,#32828,#32829,
#32830,#32831,#32832,#32833,#32834,#32835),.UNSPECIFIED.,.F.,.F.,(4,3,3,
3,3,3,3,4),(120.68953983758,121.684823586335,122.682240173108,123.679656759882,
124.677073346655,125.674489933428,126.671906520201,126.97272514476),
 .UNSPECIFIED.);
#895=B_SPLINE_CURVE_WITH_KNOTS('',3,(#32836,#32837,#32838,#32839,#32840,
#32841,#32842,#32843,#32844,#32845,#32846,#32847,#32848,#32849,#32850,#32851,
#32852,#32853,#32854,#32855,#32856,#32857,#32858,#32859,#32860,#32861,#32862,
#32863,#32864,#32865,#32866),.UNSPECIFIED.,.F.,.F.,(4,3,3,3,3,3,3,3,3,3,
4),(-123.229495242053,-122.682240173108,-121.684823586335,-120.687406999562,
-119.689990412789,-119.191282119402,-118.692573826015,-118.193865532629,
-117.695157239242,-117.196448945856,-116.946309934874),.UNSPECIFIED.);
#896=B_SPLINE_CURVE_WITH_KNOTS('',3,(#32871,#32872,#32873,#32874,#32875,
#32876,#32877,#32878,#32879,#32880,#32881,#32882,#32883,#32884,#32885,#32886,
#32887,#32888,#32889,#32890,#32891,#32892,#32893,#32894,#32895,#32896,#32897,
#32898,#32899,#32900,#32901,#32902,#32903,#32904,#32905,#32906,#32907,#32908,
#32909,#32910),.UNSPECIFIED.,.F.,.F.,(4,3,3,3,3,3,3,3,3,3,3,3,3,4),(114.406354530401,
114.702907478922,115.201615772309,115.700324065696,116.199032359082,116.697740652469,
117.196448945856,117.695157239242,118.193865532629,118.692573826015,119.191282119402,
119.689990412789,120.687406999562,120.68953983758),.UNSPECIFIED.);
#897=B_SPLINE_CURVE_WITH_KNOTS('',3,(#32911,#32912,#32913,#32914,#32915,
#32916,#32917,#32918,#32919,#32920,#32921,#32922,#32923,#32924,#32925,#32926,
#32927,#32928,#32929,#32930,#32931,#32932,#32933,#32934,#32935,#32936,#32937,
#32938,#32939,#32940,#32941,#32942,#32943,#32944,#32945,#32946,#32947,#32948,
#32949,#32950,#32951,#32952,#32953),.UNSPECIFIED.,.F.,.F.,(4,3,3,3,3,3,
3,3,3,3,3,3,3,3,4),(-116.946309934874,-116.697740652469,-116.199032359082,
-115.700324065696,-115.201615772309,-114.702907478922,-114.204199185536,
-113.705490892149,-113.206782598763,-112.708074305376,-112.209366011989,
-111.710657718603,-111.211949425216,-110.71324113183,-110.663124627694),
 .UNSPECIFIED.);
#898=B_SPLINE_CURVE_WITH_KNOTS('',3,(#32958,#32959,#32960,#32961,#32962,
#32963,#32964,#32965,#32966,#32967,#32968,#32969,#32970,#32971,#32972,#32973,
#32974,#32975,#32976,#32977,#32978,#32979,#32980,#32981,#32982,#32983,#32984,
#32985,#32986,#32987,#32988,#32989,#32990,#32991,#32992,#32993,#32994,#32995,
#32996,#32997,#32998,#32999,#33000),.UNSPECIFIED.,.F.,.F.,(4,3,3,3,3,3,
3,3,3,3,3,3,3,3,4),(108.123169223221,108.219699664896,108.718407958283,
109.21711625167,109.715824545056,110.214532838443,110.71324113183,111.211949425216,
111.710657718603,112.209366011989,112.708074305376,113.206782598763,113.705490892149,
114.204199185536,114.406354530401),.UNSPECIFIED.);
#899=B_SPLINE_CURVE_WITH_KNOTS('',3,(#33001,#33002,#33003,#33004,#33005,
#33006,#33007,#33008,#33009,#33010,#33011,#33012,#33013,#33014,#33015,#33016,
#33017,#33018,#33019,#33020,#33021,#33022,#33023,#33024,#33025,#33026,#33027,
#33028,#33029,#33030,#33031,#33032,#33033,#33034,#33035,#33036,#33037,#33038,
#33039,#33040),.UNSPECIFIED.,.F.,.F.,(4,3,3,3,3,3,3,3,3,3,3,3,3,4),(-110.663124627694,
-110.214532838443,-109.715824545056,-109.21711625167,-108.718407958283,
-108.219699664896,-107.72099137151,-107.222283078123,-106.723574784737,
-106.22486649135,-105.726158197963,-105.227449904577,-104.72874161119,-104.379939320515),
 .UNSPECIFIED.);
#900=B_SPLINE_CURVE_WITH_KNOTS('',3,(#33045,#33046,#33047,#33048,#33049,
#33050,#33051,#33052,#33053,#33054,#33055,#33056,#33057,#33058,#33059,#33060,
#33061,#33062,#33063,#33064,#33065,#33066,#33067,#33068,#33069,#33070,#33071,
#33072,#33073,#33074,#33075,#33076,#33077,#33078,#33079,#33080,#33081,#33082,
#33083,#33084),.UNSPECIFIED.,.F.,.F.,(4,3,3,3,3,3,3,3,3,3,3,3,3,4),(101.839983916042,
102.235200144257,102.733908437644,103.23261673103,103.731325024417,104.230033317804,
104.72874161119,105.227449904577,105.726158197963,106.22486649135,106.723574784737,
107.222283078123,107.72099137151,108.123169223221),.UNSPECIFIED.);
#901=B_SPLINE_CURVE_WITH_KNOTS('',3,(#33085,#33086,#33087,#33088,#33089,
#33090,#33091,#33092,#33093,#33094,#33095,#33096,#33097,#33098,#33099,#33100,
#33101,#33102,#33103,#33104,#33105,#33106,#33107,#33108,#33109,#33110,#33111,
#33112,#33113,#33114,#33115,#33116,#33117,#33118,#33119,#33120,#33121,#33122,
#33123,#33124,#33125,#33126,#33127),.UNSPECIFIED.,.F.,.F.,(4,3,3,3,3,3,
3,3,3,3,3,3,3,3,4),(-104.379939320515,-104.230033317803,-103.731325024417,
-103.23261673103,-102.733908437644,-102.235200144257,-101.73649185087,-101.237783557484,
-100.739075264097,-100.24036697071,-99.7416586773239,-99.2429503839373,
-98.7442420905506,-98.245533797164,-98.096754013335),.UNSPECIFIED.);
#902=B_SPLINE_CURVE_WITH_KNOTS('',3,(#33132,#33133,#33134,#33135,#33136,
#33137,#33138,#33139,#33140,#33141,#33142,#33143,#33144,#33145,#33146,#33147,
#33148,#33149,#33150,#33151,#33152,#33153,#33154,#33155,#33156,#33157,#33158,
#33159,#33160,#33161,#33162,#33163,#33164,#33165,#33166,#33167,#33168,#33169,
#33170,#33171,#33172,#33173,#33174),.UNSPECIFIED.,.F.,.F.,(4,3,3,3,3,3,
3,3,3,3,3,3,3,3,4),(95.556798608862,95.751992330231,96.2507006236176,96.7494089170042,
97.2481172103908,97.7468255037774,98.2455337971641,98.7442420905507,99.2429503839373,
99.7416586773239,100.240366970711,100.739075264097,101.237783557484,101.73649185087,
101.839983916042),.UNSPECIFIED.);
#903=B_SPLINE_CURVE_WITH_KNOTS('',3,(#33175,#33176,#33177,#33178,#33179,
#33180,#33181,#33182,#33183,#33184,#33185,#33186,#33187,#33188,#33189,#33190,
#33191,#33192,#33193,#33194,#33195,#33196,#33197,#33198,#33199,#33200,#33201,
#33202,#33203,#33204,#33205,#33206,#33207,#33208,#33209,#33210,#33211,#33212,
#33213,#33214),.UNSPECIFIED.,.F.,.F.,(4,3,3,3,3,3,3,3,3,3,3,3,3,4),(-98.096754013335,
-97.7468255037774,-97.2481172103908,-96.7494089170042,-96.2507006236176,
-95.7519923302309,-95.2532840368443,-94.7545757434577,-94.2558674500711,
-93.7571591566845,-93.2584508632978,-92.7597425699112,-92.2610342765246,
-91.8135687061554),.UNSPECIFIED.);
#904=B_SPLINE_CURVE_WITH_KNOTS('',3,(#33219,#33220,#33221,#33222,#33223,
#33224,#33225,#33226,#33227,#33228,#33229,#33230,#33231,#33232,#33233,#33234,
#33235,#33236,#33237,#33238,#33239,#33240,#33241,#33242,#33243,#33244,#33245,
#33246,#33247,#33248,#33249,#33250,#33251,#33252,#33253,#33254,#33255,#33256,
#33257,#33258),.UNSPECIFIED.,.F.,.F.,(4,3,3,3,3,3,3,3,3,3,3,3,3,4),(89.2736133016824,
89.7674928095915,90.2662011029781,90.7649093963648,91.2636176897514,91.762325983138,
92.2610342765246,92.7597425699113,93.2584508632979,93.7571591566845,94.2558674500711,
94.7545757434577,95.2532840368443,95.556798608862),.UNSPECIFIED.);
#905=B_SPLINE_CURVE_WITH_KNOTS('',3,(#33259,#33260,#33261,#33262,#33263,
#33264,#33265,#33266,#33267,#33268,#33269,#33270,#33271,#33272,#33273,#33274,
#33275,#33276,#33277,#33278,#33279,#33280,#33281,#33282,#33283,#33284,#33285,
#33286,#33287,#33288,#33289,#33290,#33291,#33292,#33293,#33294,#33295,#33296,
#33297,#33298,#33299,#33300,#33301),.UNSPECIFIED.,.F.,.F.,(4,3,3,3,3,3,
3,3,3,3,3,3,3,3,4),(-91.8135687061554,-91.762325983138,-91.2636176897513,
-90.7649093963647,-90.2662011029781,-89.7674928095915,-89.2687845162049,
-88.7700762228182,-88.2713679294316,-87.772659636045,-87.2739513426584,
-86.7752430492718,-86.2765347558852,-85.7778264624986,-85.5303833989758),
 .UNSPECIFIED.);
#906=B_SPLINE_CURVE_WITH_KNOTS('',3,(#33306,#33307,#33308,#33309,#33310,
#33311,#33312,#33313,#33314,#33315,#33316,#33317,#33318,#33319,#33320,#33321,
#33322,#33323,#33324,#33325,#33326,#33327,#33328,#33329,#33330,#33331,#33332,
#33333,#33334,#33335,#33336,#33337,#33338,#33339,#33340,#33341,#33342,#33343,
#33344,#33345,#33346,#33347,#33348),.UNSPECIFIED.,.F.,.F.,(4,3,3,3,3,3,
3,3,3,3,3,3,3,3,4),(82.9904279945028,83.2842849955655,83.7829932889521,
84.2817015823387,84.7804098757253,85.279118169112,85.7778264624986,86.2765347558852,
86.7752430492718,87.2739513426584,87.772659636045,88.2713679294317,88.7700762228183,
89.2687845162049,89.2736133016824),.UNSPECIFIED.);
#907=B_SPLINE_CURVE_WITH_KNOTS('',3,(#33349,#33350,#33351,#33352,#33353,
#33354,#33355,#33356,#33357,#33358,#33359,#33360,#33361,#33362,#33363,#33364,
#33365,#33366,#33367,#33368,#33369,#33370,#33371,#33372,#33373,#33374,#33375,
#33376,#33377,#33378,#33379,#33380,#33381,#33382,#33383,#33384,#33385,#33386,
#33387,#33388,#33389,#33390,#33391),.UNSPECIFIED.,.F.,.F.,(4,3,3,3,3,3,
3,3,3,3,3,3,3,3,4),(-85.5303833989758,-85.2791181691119,-84.7804098757253,
-84.2817015823387,-83.7829932889521,-83.2842849955654,-82.7855767021788,
-82.2868684087922,-81.7881601154056,-81.289451822019,-80.7907435286323,
-80.2920352352457,-79.7933269418591,-79.2946186484725,-79.2471980917962),
 .UNSPECIFIED.);
#908=B_SPLINE_CURVE_WITH_KNOTS('',3,(#33396,#33397,#33398,#33399,#33400,
#33401,#33402,#33403,#33404,#33405,#33406,#33407,#33408,#33409,#33410,#33411,
#33412,#33413,#33414,#33415,#33416,#33417,#33418,#33419,#33420,#33421,#33422,
#33423,#33424,#33425,#33426,#33427,#33428,#33429,#33430,#33431,#33432,#33433,
#33434,#33435,#33436,#33437,#33438),.UNSPECIFIED.,.F.,.F.,(4,3,3,3,3,3,
3,3,3,3,3,3,3,3,4),(76.7072426873232,76.8010771815394,77.299785474926,77.7984937683127,
78.2972020616993,78.7959103550859,79.2946186484725,79.7933269418591,80.2920352352457,
80.7907435286324,81.289451822019,81.7881601154056,82.2868684087922,82.7855767021789,
82.9904279945028),.UNSPECIFIED.);
#909=B_SPLINE_CURVE_WITH_KNOTS('',3,(#33439,#33440,#33441,#33442,#33443,
#33444,#33445,#33446,#33447,#33448,#33449,#33450,#33451,#33452,#33453,#33454,
#33455,#33456,#33457,#33458,#33459,#33460,#33461,#33462,#33463,#33464,#33465,
#33466,#33467,#33468,#33469,#33470,#33471,#33472,#33473,#33474,#33475,#33476,
#33477,#33478),.UNSPECIFIED.,.F.,.F.,(4,3,3,3,3,3,3,3,3,3,3,3,3,4),(-79.2471980917962,
-78.7959103550859,-78.2972020616993,-77.7984937683126,-77.299785474926,
-76.8010771815394,-76.3023688881528,-75.8036605947662,-75.3049523013795,
-74.8062440079929,-74.3075357146063,-73.8088274212197,-73.3101191278331,
-72.9640127846166),.UNSPECIFIED.);
#910=B_SPLINE_CURVE_WITH_KNOTS('',3,(#33483,#33484,#33485,#33486,#33487,
#33488,#33489,#33490,#33491,#33492,#33493,#33494,#33495,#33496,#33497,#33498,
#33499,#33500,#33501,#33502,#33503,#33504,#33505,#33506,#33507,#33508,#33509,
#33510,#33511,#33512,#33513,#33514,#33515,#33516,#33517,#33518,#33519,#33520,
#33521,#33522),.UNSPECIFIED.,.F.,.F.,(4,3,3,3,3,3,3,3,3,3,3,3,3,4),(70.4240573801436,
70.8165776609,71.3152859542866,71.8139942476732,72.3127025410598,72.8114108344465,
73.3101191278331,73.8088274212197,74.3075357146063,74.8062440079929,75.3049523013796,
75.8036605947662,76.3023688881528,76.7072426873232),.UNSPECIFIED.);
#911=B_SPLINE_CURVE_WITH_KNOTS('',3,(#33523,#33524,#33525,#33526,#33527,
#33528,#33529,#33530,#33531,#33532,#33533,#33534,#33535,#33536,#33537,#33538,
#33539,#33540,#33541,#33542,#33543,#33544,#33545,#33546,#33547,#33548,#33549,
#33550,#33551,#33552,#33553,#33554,#33555,#33556,#33557,#33558,#33559,#33560,
#33561,#33562,#33563,#33564,#33565),.UNSPECIFIED.,.F.,.F.,(4,3,3,3,3,3,
3,3,3,3,3,3,3,3,4),(-72.9640127846166,-72.8114108344464,-72.3127025410598,
-71.8139942476732,-71.3152859542866,-70.8165776609,-70.3178693675133,-69.8191610741267,
-69.3204527807401,-68.8217444873535,-68.3230361939669,-67.8243279005802,
-67.3256196071936,-66.826911313807,-66.680827477437),.UNSPECIFIED.);
#912=B_SPLINE_CURVE_WITH_KNOTS('',3,(#33570,#33571,#33572,#33573,#33574,
#33575,#33576,#33577,#33578,#33579,#33580,#33581,#33582,#33583,#33584,#33585,
#33586,#33587,#33588,#33589,#33590,#33591,#33592,#33593,#33594,#33595,#33596,
#33597,#33598,#33599,#33600,#33601,#33602,#33603,#33604,#33605,#33606,#33607,
#33608,#33609,#33610,#33611,#33612),.UNSPECIFIED.,.F.,.F.,(4,3,3,3,3,3,
3,3,3,3,3,3,3,3,4),(64.140872072964,64.3333698468739,64.8320781402605,65.3307864336472,
65.8294947270338,66.3282030204204,66.826911313807,67.3256196071937,67.8243279005803,
68.3230361939669,68.8217444873535,69.3204527807401,69.8191610741268,70.3178693675134,
70.4240573801436),.UNSPECIFIED.);
#913=B_SPLINE_CURVE_WITH_KNOTS('',3,(#33613,#33614,#33615,#33616,#33617,
#33618,#33619,#33620,#33621,#33622,#33623,#33624,#33625,#33626,#33627,#33628,
#33629,#33630,#33631,#33632,#33633,#33634,#33635,#33636,#33637,#33638,#33639,
#33640,#33641,#33642,#33643,#33644,#33645,#33646,#33647,#33648,#33649,#33650,
#33651,#33652),.UNSPECIFIED.,.F.,.F.,(4,3,3,3,3,3,3,3,3,3,3,3,3,4),(-66.680827477437,
-66.3282030204204,-65.8294947270337,-65.3307864336471,-64.8320781402605,
-64.3333698468739,-63.8346615534873,-63.3359532601007,-62.837244966714,
-62.3385366733274,-61.8398283799408,-61.3411200865542,-60.8424117931676,
-60.3976421702575),.UNSPECIFIED.);
#914=B_SPLINE_CURVE_WITH_KNOTS('',3,(#33657,#33658,#33659,#33660,#33661,
#33662,#33663,#33664,#33665,#33666,#33667,#33668,#33669,#33670,#33671,#33672,
#33673,#33674,#33675,#33676,#33677,#33678,#33679,#33680,#33681,#33682,#33683,
#33684,#33685,#33686,#33687,#33688,#33689,#33690,#33691,#33692,#33693,#33694,
#33695,#33696),.UNSPECIFIED.,.F.,.F.,(4,3,3,3,3,3,3,3,3,3,3,3,3,4),(57.8576867657844,
58.3488703262345,58.8475786196211,59.3462869130077,59.8449952063944,60.343703499781,
60.8424117931676,61.3411200865542,61.8398283799408,62.3385366733274,62.8372449667141,
63.3359532601007,63.8346615534873,64.140872072964),.UNSPECIFIED.);
#915=B_SPLINE_CURVE_WITH_KNOTS('',3,(#33697,#33698,#33699,#33700,#33701,
#33702,#33703,#33704,#33705,#33706,#33707,#33708,#33709,#33710,#33711,#33712,
#33713,#33714,#33715,#33716,#33717,#33718,#33719,#33720,#33721,#33722,#33723,
#33724,#33725,#33726,#33727,#33728,#33729,#33730,#33731,#33732,#33733,#33734,
#33735,#33736,#33737,#33738,#33739),.UNSPECIFIED.,.F.,.F.,(4,3,3,3,3,3,
3,3,3,3,3,3,3,3,4),(-60.3976421702575,-60.3437034997809,-59.8449952063943,
-59.3462869130077,-58.8475786196211,-58.3488703262345,-57.8501620328479,
-57.3514537394612,-56.8527454460746,-56.354037152688,-55.8553288593014,
-55.3566205659148,-54.8579122725281,-54.3592039791415,-54.1144568630779),
 .UNSPECIFIED.);
#916=B_SPLINE_CURVE_WITH_KNOTS('',3,(#33744,#33745,#33746,#33747,#33748,
#33749,#33750,#33751,#33752,#33753,#33754,#33755,#33756,#33757,#33758,#33759,
#33760,#33761,#33762,#33763,#33764,#33765,#33766,#33767,#33768,#33769,#33770,
#33771,#33772,#33773,#33774,#33775,#33776,#33777,#33778,#33779,#33780,#33781,
#33782,#33783,#33784,#33785,#33786),.UNSPECIFIED.,.F.,.F.,(4,3,3,3,3,3,
3,3,3,3,3,3,3,3,4),(51.5745014586048,51.8656625122084,52.3643708055951,
52.8630790989817,53.3617873923683,53.8604956857549,54.3592039791415,54.8579122725282,
55.3566205659148,55.8553288593014,56.354037152688,56.8527454460746,57.3514537394612,
57.8501620328479,57.8576867657844),.UNSPECIFIED.);
#917=B_SPLINE_CURVE_WITH_KNOTS('',3,(#33787,#33788,#33789,#33790,#33791,
#33792,#33793,#33794,#33795,#33796,#33797,#33798,#33799,#33800,#33801,#33802,
#33803,#33804,#33805,#33806,#33807,#33808,#33809,#33810,#33811,#33812,#33813,
#33814,#33815,#33816,#33817,#33818,#33819,#33820,#33821,#33822,#33823,#33824,
#33825,#33826,#33827,#33828,#33829),.UNSPECIFIED.,.F.,.F.,(4,3,3,3,3,3,
3,3,3,3,3,3,3,3,4),(-54.1144568630779,-53.8604956857549,-53.3617873923683,
-52.8630790989817,-52.3643708055951,-51.8656625122084,-51.3669542188218,
-50.8682459254352,-50.3695376320486,-49.8708293386619,-49.3721210452753,
-48.8734127518887,-48.3747044585021,-47.8759961651155,-47.8312715558983),
 .UNSPECIFIED.);
#918=B_SPLINE_CURVE_WITH_KNOTS('',3,(#33834,#33835,#33836,#33837,#33838,
#33839,#33840,#33841,#33842,#33843,#33844,#33845,#33846,#33847,#33848,#33849,
#33850,#33851,#33852,#33853,#33854,#33855,#33856,#33857,#33858,#33859,#33860,
#33861,#33862,#33863,#33864,#33865,#33866,#33867,#33868,#33869,#33870,#33871,
#33872,#33873,#33874,#33875,#33876),.UNSPECIFIED.,.F.,.F.,(4,3,3,3,3,3,
3,3,3,3,3,3,3,3,4),(45.2913161514252,45.3824546981824,45.881162991569,46.3798712849556,
46.8785795783422,47.3772878717289,47.8759961651155,48.3747044585021,48.8734127518887,
49.3721210452753,49.870829338662,50.3695376320486,50.8682459254352,51.3669542188218,
51.5745014586048),.UNSPECIFIED.);
#919=B_SPLINE_CURVE_WITH_KNOTS('',3,(#33877,#33878,#33879,#33880,#33881,
#33882,#33883,#33884,#33885,#33886,#33887,#33888,#33889,#33890,#33891,#33892,
#33893,#33894,#33895,#33896,#33897,#33898,#33899,#33900,#33901,#33902,#33903,
#33904,#33905,#33906,#33907,#33908,#33909,#33910,#33911,#33912,#33913,#33914,
#33915,#33916),.UNSPECIFIED.,.F.,.F.,(4,3,3,3,3,3,3,3,3,3,3,3,3,4),(-47.8312715558983,
-47.3772878717289,-46.8785795783422,-46.3798712849556,-45.881162991569,
-45.3824546981824,-44.8837464047958,-44.3850381114091,-43.8863298180225,
-43.3876215246359,-42.8889132312493,-42.3902049378627,-41.891496644476,
-41.5480862487187),.UNSPECIFIED.);
#920=B_SPLINE_CURVE_WITH_KNOTS('',3,(#33921,#33922,#33923,#33924,#33925,
#33926,#33927,#33928,#33929,#33930,#33931,#33932,#33933,#33934,#33935,#33936,
#33937,#33938,#33939,#33940,#33941,#33942,#33943,#33944,#33945,#33946,#33947,
#33948,#33949,#33950,#33951,#33952,#33953,#33954,#33955,#33956,#33957,#33958,
#33959,#33960),.UNSPECIFIED.,.F.,.F.,(4,3,3,3,3,3,3,3,3,3,3,3,3,4),(39.0081308442456,
39.3979551775429,39.8966634709296,40.3953717643162,40.8940800577028,41.3927883510894,
41.891496644476,42.3902049378627,42.8889132312493,43.3876215246359,43.8863298180225,
44.3850381114091,44.8837464047958,45.2913161514252),.UNSPECIFIED.);
#921=B_SPLINE_CURVE_WITH_KNOTS('',3,(#33961,#33962,#33963,#33964,#33965,
#33966,#33967,#33968,#33969,#33970,#33971,#33972,#33973,#33974,#33975,#33976,
#33977,#33978,#33979,#33980,#33981,#33982,#33983,#33984,#33985,#33986,#33987,
#33988,#33989,#33990,#33991,#33992,#33993,#33994,#33995,#33996,#33997,#33998,
#33999,#34000,#34001,#34002,#34003),.UNSPECIFIED.,.F.,.F.,(4,3,3,3,3,3,
3,3,3,3,3,3,3,3,4),(-41.5480862487187,-41.3927883510894,-40.8940800577028,
-40.3953717643162,-39.8966634709296,-39.3979551775429,-38.8992468841563,
-38.4005385907697,-37.9018302973831,-37.4031220039965,-36.9044137106098,
-36.4057054172232,-35.9069971238366,-35.40828883045,-35.2649009415391),
 .UNSPECIFIED.);
#922=B_SPLINE_CURVE_WITH_KNOTS('',3,(#34008,#34009,#34010,#34011,#34012,
#34013,#34014,#34015,#34016,#34017,#34018,#34019,#34020,#34021,#34022,#34023,
#34024,#34025,#34026,#34027,#34028,#34029,#34030,#34031,#34032,#34033,#34034,
#34035,#34036,#34037,#34038,#34039,#34040,#34041,#34042,#34043,#34044,#34045,
#34046,#34047,#34048,#34049,#34050),.UNSPECIFIED.,.F.,.F.,(4,3,3,3,3,3,
3,3,3,3,3,3,3,3,4),(32.7249455370661,32.9147473635169,33.4134556569035,
33.9121639502901,34.4108722436767,34.9095805370634,35.40828883045,35.9069971238366,
36.4057054172232,36.9044137106099,37.4031220039965,37.9018302973831,38.4005385907697,
38.8992468841563,39.0081308442456),.UNSPECIFIED.);
#923=B_SPLINE_CURVE_WITH_KNOTS('',3,(#34051,#34052,#34053,#34054,#34055,
#34056,#34057,#34058,#34059,#34060,#34061,#34062,#34063,#34064,#34065,#34066,
#34067,#34068,#34069,#34070,#34071,#34072,#34073,#34074,#34075,#34076,#34077,
#34078,#34079,#34080,#34081,#34082,#34083,#34084,#34085,#34086,#34087,#34088,
#34089,#34090),.UNSPECIFIED.,.F.,.F.,(4,3,3,3,3,3,3,3,3,3,3,3,3,4),(-35.2649009415391,
-34.9095805370634,-34.4108722436767,-33.9121639502901,-33.4134556569035,
-32.9147473635169,-32.4160390701303,-31.9173307767436,-31.418622483357,
-30.9199141899704,-30.4212058965838,-29.9224976031972,-29.4237893098105,
-28.9817156343595),.UNSPECIFIED.);
#924=B_SPLINE_CURVE_WITH_KNOTS('',3,(#34095,#34096,#34097,#34098,#34099,
#34100,#34101,#34102,#34103,#34104,#34105,#34106,#34107,#34108,#34109,#34110,
#34111,#34112,#34113,#34114,#34115,#34116,#34117,#34118,#34119,#34120,#34121,
#34122,#34123,#34124,#34125,#34126,#34127,#34128,#34129,#34130,#34131,#34132,
#34133,#34134),.UNSPECIFIED.,.F.,.F.,(4,3,3,3,3,3,3,3,3,3,3,3,3,4),(26.4417602298865,
26.9302478428775,27.4289561362641,27.9276644296507,28.4263727230373,28.9250810164239,
29.4237893098106,29.9224976031972,30.4212058965838,30.9199141899704,31.418622483357,
31.9173307767437,32.4160390701303,32.7249455370661),.UNSPECIFIED.);
#925=B_SPLINE_CURVE_WITH_KNOTS('',3,(#34135,#34136,#34137,#34138,#34139,
#34140,#34141,#34142,#34143,#34144,#34145,#34146,#34147,#34148,#34149,#34150,
#34151,#34152,#34153,#34154,#34155,#34156,#34157,#34158,#34159,#34160,#34161,
#34162,#34163,#34164,#34165,#34166,#34167,#34168,#34169,#34170,#34171,#34172,
#34173,#34174,#34175,#34176,#34177),.UNSPECIFIED.,.F.,.F.,(4,3,3,3,3,3,
3,3,3,3,3,3,3,3,4),(-28.9817156343595,-28.9250810164239,-28.4263727230373,
-27.9276644296507,-27.4289561362641,-26.9302478428774,-26.4315395494908,
-25.9328312561042,-25.4341229627176,-24.935414669331,-24.4367063759443,
-23.9379980825577,-23.4392897891711,-22.9405814957845,-22.6985303271799),
 .UNSPECIFIED.);
#926=B_SPLINE_CURVE_WITH_KNOTS('',3,(#34182,#34183,#34184,#34185,#34186,
#34187,#34188,#34189,#34190,#34191,#34192,#34193,#34194,#34195,#34196,#34197,
#34198,#34199,#34200,#34201,#34202,#34203,#34204,#34205,#34206,#34207,#34208,
#34209,#34210,#34211,#34212,#34213,#34214,#34215,#34216,#34217,#34218,#34219,
#34220,#34221,#34222,#34223,#34224),.UNSPECIFIED.,.F.,.F.,(4,3,3,3,3,3,
3,3,3,3,3,3,3,3,4),(20.1585749227069,20.4470400288514,20.945748322238,21.4444566156246,
21.9431649090113,22.4418732023979,22.9405814957845,23.4392897891711,23.9379980825577,
24.4367063759444,24.935414669331,25.4341229627176,25.9328312561042,26.4315395494908,
26.4417602298865),.UNSPECIFIED.);
#927=B_SPLINE_CURVE_WITH_KNOTS('',3,(#34225,#34226,#34227,#34228,#34229,
#34230,#34231,#34232,#34233,#34234,#34235,#34236,#34237,#34238,#34239,#34240,
#34241,#34242,#34243,#34244,#34245,#34246,#34247,#34248,#34249,#34250,#34251,
#34252,#34253,#34254,#34255,#34256,#34257,#34258,#34259,#34260,#34261,#34262,
#34263,#34264,#34265,#34266,#34267),.UNSPECIFIED.,.F.,.F.,(4,3,3,3,3,3,
3,3,3,3,3,3,3,3,4),(-22.6985303271799,-22.4418732023979,-21.9431649090112,
-21.4444566156246,-20.945748322238,-20.4470400288514,-19.9483317354648,
-19.4496234420782,-18.9509151486915,-18.4522068553049,-17.9534985619183,
-17.4547902685317,-16.9560819751451,-16.4573736817584,-16.4153450200003),
 .UNSPECIFIED.);
#928=B_SPLINE_CURVE_WITH_KNOTS('',3,(#34272,#34273,#34274,#34275,#34276,
#34277,#34278,#34279,#34280,#34281,#34282,#34283,#34284,#34285,#34286,#34287,
#34288,#34289,#34290,#34291,#34292,#34293,#34294,#34295,#34296,#34297,#34298,
#34299,#34300,#34301,#34302,#34303,#34304,#34305,#34306,#34307,#34308,#34309,
#34310,#34311,#34312,#34313,#34314),.UNSPECIFIED.,.F.,.F.,(4,3,3,3,3,3,
3,3,3,3,3,3,3,3,4),(13.8753896155273,13.9638322148253,14.462540508212,14.9612488015986,
15.4599570949852,15.9586653883718,16.4573736817584,16.9560819751451,17.4547902685317,
17.9534985619183,18.4522068553049,18.9509151486915,19.4496234420782,19.9483317354648,
20.1585749227069),.UNSPECIFIED.);
#929=B_SPLINE_CURVE_WITH_KNOTS('',3,(#34315,#34316,#34317,#34318,#34319,
#34320,#34321,#34322,#34323,#34324,#34325,#34326,#34327,#34328,#34329,#34330,
#34331,#34332,#34333,#34334,#34335,#34336,#34337,#34338,#34339,#34340,#34341,
#34342,#34343,#34344,#34345,#34346,#34347,#34348,#34349,#34350,#34351,#34352,
#34353,#34354),.UNSPECIFIED.,.F.,.F.,(4,3,3,3,3,3,3,3,3,3,3,3,3,4),(-16.4153450200003,
-15.9586653883718,-15.4599570949852,-14.9612488015986,-14.462540508212,
-13.9638322148253,-13.4651239214387,-12.9664156280521,-12.4677073346655,
-11.9689990412789,-11.4702907478922,-10.9715824545056,-10.472874161119,
-10.1321597128207),.UNSPECIFIED.);
#930=B_SPLINE_CURVE_WITH_KNOTS('',3,(#34360,#34361,#34362,#34363,#34364,
#34365,#34366,#34367,#34368,#34369,#34370,#34371,#34372,#34373,#34374,#34375,
#34376,#34377,#34378,#34379,#34380,#34381,#34382,#34383,#34384),
 .UNSPECIFIED.,.F.,.F.,(4,3,3,3,3,3,3,3,4),(-3.84897440564115,-3.49095805370634,
-2.99224976031972,-2.4935414669331,-1.99483317354648,-1.49612488015986,
-0.997416586773239,-0.49870829338662,0.),.UNSPECIFIED.);
#931=B_SPLINE_CURVE_WITH_KNOTS('',3,(#34387,#34388,#34389,#34390,#34391,
#34392,#34393,#34394,#34395,#34396,#34397,#34398,#34399,#34400,#34401,#34402,
#34403,#34404,#34405,#34406,#34407,#34408,#34409,#34410,#34411,#34412,#34413,
#34414,#34415,#34416,#34417,#34418,#34419,#34420,#34421,#34422,#34423),
 .UNSPECIFIED.,.F.,.F.,(4,3,3,3,3,3,3,3,3,3,3,3,4),(2.01640075321917,2.4935414669331,
2.99224976031972,3.49095805370634,3.98966634709296,4.48837464047958,4.9870829338662,
5.48579122725282,5.98449952063944,6.48320781402605,6.98191610741268,7.48062440079929,
7.59220430834772),.UNSPECIFIED.);
#932=B_SPLINE_CURVE_WITH_KNOTS('',3,(#34429,#34430,#34431,#34432,#34433,
#34434,#34435,#34436,#34437,#34438,#34439,#34440),.UNSPECIFIED.,.F.,.F.,
(4,1,1,1,1,1,1,1,1,4),(260.752190247953,261.213135555618,261.711843849004,
262.210552142391,262.709260435778,263.207968729164,263.706677022551,264.205385315938,
264.704093609324,265.202801902711),.UNSPECIFIED.);
#933=B_SPLINE_CURVE_WITH_KNOTS('',3,(#34443,#34444,#34445,#34446,#34447,
#34448,#34449,#34450,#34451,#34452,#34453,#34454,#34455,#34456),
 .UNSPECIFIED.,.F.,.F.,(4,1,1,1,1,1,1,1,1,1,1,4),(260.752190247953,260.760841199772,
261.259549493158,261.758257786545,262.256966079931,262.755674373318,263.254382666705,
263.753090960091,264.251799253478,264.750507546865,265.249215840251,265.726356553965),
 .UNSPECIFIED.);
#934=B_SPLINE_CURVE_WITH_KNOTS('',3,(#34461,#34462,#34463,#34464,#34465,
#34466,#34467,#34468,#34469,#34470,#34471,#34472,#34473,#34474,#34475,#34476,
#34477),.UNSPECIFIED.,.F.,.F.,(4,1,1,1,1,1,1,1,1,1,1,1,1,1,4),(254.469004940773,
254.729927741592,255.228636034978,255.727344328365,256.226052621752,256.724760915138,
257.223469208525,257.722177501912,258.220885795298,258.719594088685,259.218302382071,
259.717010675458,260.215718968845,260.714427262231,260.752190247953),
 .UNSPECIFIED.);
#935=B_SPLINE_CURVE_WITH_KNOTS('',3,(#34478,#34479,#34480,#34481,#34482,
#34483,#34484,#34485,#34486,#34487,#34488,#34489,#34490,#34491,#34492,#34493),
 .UNSPECIFIED.,.F.,.F.,(4,1,1,1,1,1,1,1,1,1,1,1,1,4),(254.469004940773,
254.776341679132,255.275049972519,255.773758265905,256.272466559292,256.771174852679,
257.269883146065,257.768591439452,258.267299732838,258.766008026225,259.264716319612,
259.763424612998,260.262132906385,260.752190247953),.UNSPECIFIED.);
#936=B_SPLINE_CURVE_WITH_KNOTS('',3,(#34498,#34499,#34500,#34501,#34502,
#34503,#34504,#34505,#34506,#34507,#34508,#34509,#34510,#34511,#34512,#34513,
#34514),.UNSPECIFIED.,.F.,.F.,(4,1,1,1,1,1,1,1,1,1,1,1,1,1,4),(248.185819633594,
248.246719927566,248.745428220952,249.244136514339,249.742844807726,250.241553101112,
250.740261394499,251.238969687886,251.737677981272,252.236386274659,252.735094568045,
253.233802861432,253.732511154819,254.231219448205,254.469004940773),
 .UNSPECIFIED.);
#937=B_SPLINE_CURVE_WITH_KNOTS('',3,(#34515,#34516,#34517,#34518,#34519,
#34520,#34521,#34522,#34523,#34524,#34525,#34526,#34527,#34528,#34529,#34530,
#34531),.UNSPECIFIED.,.F.,.F.,(4,1,1,1,1,1,1,1,1,1,1,1,1,1,4),(248.185819633594,
248.293133865106,248.791842158493,249.290550451879,249.789258745266,250.287967038653,
250.786675332039,251.285383625426,251.784091918812,252.282800212199,252.781508505586,
253.280216798972,253.778925092359,254.277633385745,254.469004940773),
 .UNSPECIFIED.);
#938=B_SPLINE_CURVE_WITH_KNOTS('',3,(#34536,#34537,#34538,#34539,#34540,
#34541,#34542,#34543,#34544,#34545,#34546,#34547,#34548,#34549,#34550,#34551),
 .UNSPECIFIED.,.F.,.F.,(4,1,1,1,1,1,1,1,1,1,1,1,1,4),(241.902634326414,
242.262220406926,242.760928700313,243.2596369937,243.758345287086,244.257053580473,
244.755761873859,245.254470167246,245.753178460633,246.251886754019,246.750595047406,
247.249303340793,247.748011634179,248.185819633594),.UNSPECIFIED.);
#939=B_SPLINE_CURVE_WITH_KNOTS('',3,(#34552,#34553,#34554,#34555,#34556,
#34557,#34558,#34559,#34560,#34561,#34562,#34563,#34564,#34565,#34566,#34567),
 .UNSPECIFIED.,.F.,.F.,(4,1,1,1,1,1,1,1,1,1,1,1,1,4),(241.902634326414,
242.308634344467,242.807342637853,243.30605093124,243.804759224626,244.303467518013,
244.8021758114,245.300884104786,245.799592398173,246.29830069156,246.797008984946,
247.295717278333,247.794425571719,248.185819633594),.UNSPECIFIED.);
#940=B_SPLINE_CURVE_WITH_KNOTS('',3,(#34572,#34573,#34574,#34575,#34576,
#34577,#34578,#34579,#34580,#34581,#34582,#34583,#34584,#34585,#34586,#34587,
#34588),.UNSPECIFIED.,.F.,.F.,(4,1,1,1,1,1,1,1,1,1,1,1,1,1,4),(235.619449019235,
235.7790125929,236.277720886287,236.776429179674,237.27513747306,237.773845766447,
238.272554059833,238.77126235322,239.269970646607,239.768678939993,240.26738723338,
240.766095526767,241.264803820153,241.76351211354,241.902634326414),
 .UNSPECIFIED.);
#941=B_SPLINE_CURVE_WITH_KNOTS('',3,(#34589,#34590,#34591,#34592,#34593,
#34594,#34595,#34596,#34597,#34598,#34599,#34600,#34601,#34602,#34603,#34604,
#34605),.UNSPECIFIED.,.F.,.F.,(4,1,1,1,1,1,1,1,1,1,1,1,1,1,4),(235.619449019235,
235.825426530441,236.324134823827,236.822843117214,237.3215514106,237.820259703987,
238.318967997374,238.81767629076,239.316384584147,239.815092877534,240.31380117092,
240.812509464307,241.311217757693,241.80992605108,241.902634326414),
 .UNSPECIFIED.);
#942=B_SPLINE_CURVE_WITH_KNOTS('',3,(#34610,#34611,#34612,#34613,#34614,
#34615,#34616,#34617,#34618,#34619,#34620,#34621,#34622,#34623,#34624,#34625),
 .UNSPECIFIED.,.F.,.F.,(4,1,1,1,1,1,1,1,1,1,1,1,1,4),(229.336263712055,
229.794513072261,230.293221365647,230.791929659034,231.290637952421,231.789346245807,
232.288054539194,232.786762832581,233.285471125967,233.784179419354,234.28288771274,
234.781596006127,235.280304299514,235.619449019235),.UNSPECIFIED.);
#943=B_SPLINE_CURVE_WITH_KNOTS('',3,(#34626,#34627,#34628,#34629,#34630,
#34631,#34632,#34633,#34634,#34635,#34636,#34637,#34638,#34639,#34640,#34641,
#34642),.UNSPECIFIED.,.F.,.F.,(4,1,1,1,1,1,1,1,1,1,1,1,1,1,4),(229.336263712055,
229.342218716414,229.840927009801,230.339635303188,230.838343596574,231.337051889961,
231.835760183348,232.334468476734,232.833176770121,233.331885063507,233.830593356894,
234.329301650281,234.828009943667,235.326718237054,235.619449019235),
 .UNSPECIFIED.);
#944=B_SPLINE_CURVE_WITH_KNOTS('',3,(#34647,#34648,#34649,#34650,#34651,
#34652,#34653,#34654,#34655,#34656,#34657,#34658,#34659,#34660,#34661,#34662,
#34663),.UNSPECIFIED.,.F.,.F.,(4,1,1,1,1,1,1,1,1,1,1,1,1,1,4),(223.053078404875,
223.311305258235,223.810013551621,224.308721845008,224.807430138395,225.306138431781,
225.804846725168,226.303555018555,226.802263311941,227.300971605328,227.799679898714,
228.298388192101,228.797096485488,229.295804778874,229.336263712055),
 .UNSPECIFIED.);
#945=B_SPLINE_CURVE_WITH_KNOTS('',3,(#34664,#34665,#34666,#34667,#34668,
#34669,#34670,#34671,#34672,#34673,#34674,#34675,#34676,#34677,#34678,#34679),
 .UNSPECIFIED.,.F.,.F.,(4,1,1,1,1,1,1,1,1,1,1,1,1,4),(223.053078404875,
223.357719195775,223.856427489162,224.355135782548,224.853844075935,225.352552369322,
225.851260662708,226.349968956095,226.848677249481,227.347385542868,227.846093836255,
228.344802129641,228.843510423028,229.336263712055),.UNSPECIFIED.);
#946=B_SPLINE_CURVE_WITH_KNOTS('',3,(#34684,#34685,#34686,#34687,#34688,
#34689,#34690,#34691,#34692,#34693,#34694,#34695,#34696,#34697,#34698,#34699,
#34700),.UNSPECIFIED.,.F.,.F.,(4,1,1,1,1,1,1,1,1,1,1,1,1,1,4),(216.769893097696,
216.828097444209,217.326805737595,217.825514030982,218.324222324369,218.822930617755,
219.321638911142,219.820347204529,220.319055497915,220.817763791302,221.316472084688,
221.815180378075,222.313888671462,222.812596964848,223.053078404875),
 .UNSPECIFIED.);
#947=B_SPLINE_CURVE_WITH_KNOTS('',3,(#34701,#34702,#34703,#34704,#34705,
#34706,#34707,#34708,#34709,#34710,#34711,#34712,#34713,#34714,#34715,#34716,
#34717),.UNSPECIFIED.,.F.,.F.,(4,1,1,1,1,1,1,1,1,1,1,1,1,1,4),(216.769893097696,
216.874511381749,217.373219675136,217.871927968522,218.370636261909,218.869344555295,
219.368052848682,219.866761142069,220.365469435455,220.864177728842,221.362886022229,
221.861594315615,222.360302609002,222.859010902388,223.053078404875),
 .UNSPECIFIED.);
#948=B_SPLINE_CURVE_WITH_KNOTS('',3,(#34722,#34723,#34724,#34725,#34726,
#34727,#34728,#34729,#34730,#34731,#34732,#34733,#34734,#34735,#34736,#34737),
 .UNSPECIFIED.,.F.,.F.,(4,1,1,1,1,1,1,1,1,1,1,1,1,4),(210.486707790516,
210.843597923569,211.342306216956,211.841014510343,212.339722803729,212.838431097116,
213.337139390502,213.835847683889,214.334555977276,214.833264270662,215.331972564049,
215.830680857436,216.329389150822,216.769893097696),.UNSPECIFIED.);
#949=B_SPLINE_CURVE_WITH_KNOTS('',3,(#34738,#34739,#34740,#34741,#34742,
#34743,#34744,#34745,#34746,#34747,#34748,#34749,#34750,#34751,#34752,#34753),
 .UNSPECIFIED.,.F.,.F.,(4,1,1,1,1,1,1,1,1,1,1,1,1,4),(210.486707790516,
210.89001186111,211.388720154496,211.887428447883,212.386136741269,212.884845034656,
213.383553328043,213.882261621429,214.380969914816,214.879678208203,215.378386501589,
215.877094794976,216.375803088362,216.769893097696),.UNSPECIFIED.);
#950=B_SPLINE_CURVE_WITH_KNOTS('',3,(#34758,#34759,#34760,#34761,#34762,
#34763,#34764,#34765,#34766,#34767,#34768,#34769,#34770,#34771,#34772,#34773,
#34774),.UNSPECIFIED.,.F.,.F.,(4,1,1,1,1,1,1,1,1,1,1,1,1,1,4),(204.203522483337,
204.360390109543,204.85909840293,205.357806696317,205.856514989703,206.35522328309,
206.853931576476,207.352639869863,207.85134816325,208.350056456636,208.848764750023,
209.347473043409,209.846181336796,210.344889630183,210.486707790516),
 .UNSPECIFIED.);
#951=B_SPLINE_CURVE_WITH_KNOTS('',3,(#34775,#34776,#34777,#34778,#34779,
#34780,#34781,#34782,#34783,#34784,#34785,#34786,#34787,#34788,#34789,#34790,
#34791),.UNSPECIFIED.,.F.,.F.,(4,1,1,1,1,1,1,1,1,1,1,1,1,1,4),(204.203522483337,
204.406804047084,204.90551234047,205.404220633857,205.902928927243,206.40163722063,
206.900345514017,207.399053807403,207.89776210079,208.396470394177,208.895178687563,
209.39388698095,209.892595274336,210.391303567723,210.486707790516),
 .UNSPECIFIED.);
#952=B_SPLINE_CURVE_WITH_KNOTS('',3,(#34796,#34797,#34798,#34799,#34800,
#34801,#34802,#34803,#34804,#34805,#34806,#34807,#34808,#34809,#34810,#34811),
 .UNSPECIFIED.,.F.,.F.,(4,1,1,1,1,1,1,1,1,1,1,1,1,4),(197.920337176157,
198.375890588904,198.87459888229,199.373307175677,199.872015469064,200.37072376245,
200.869432055837,201.368140349224,201.86684864261,202.365556935997,202.864265229383,
203.36297352277,203.861681816157,204.203522483337),.UNSPECIFIED.);
#953=B_SPLINE_CURVE_WITH_KNOTS('',3,(#34812,#34813,#34814,#34815,#34816,
#34817,#34818,#34819,#34820,#34821,#34822,#34823,#34824,#34825,#34826,#34827,
#34828),.UNSPECIFIED.,.F.,.F.,(4,1,1,1,1,1,1,1,1,1,1,1,1,1,4),(197.920337176157,
197.923596233057,198.422304526444,198.921012819831,199.419721113217,199.918429406604,
200.417137699991,200.915845993377,201.414554286764,201.91326258015,202.411970873537,
202.910679166924,203.40938746031,203.908095753697,204.203522483337),
 .UNSPECIFIED.);
#954=B_SPLINE_CURVE_WITH_KNOTS('',3,(#34833,#34834,#34835,#34836,#34837,
#34838,#34839,#34840,#34841,#34842,#34843,#34844,#34845,#34846,#34847,#34848,
#34849),.UNSPECIFIED.,.F.,.F.,(4,1,1,1,1,1,1,1,1,1,1,1,1,1,4),(191.637151868978,
191.892682774878,192.391391068264,192.890099361651,193.388807655038,193.887515948424,
194.386224241811,194.884932535198,195.383640828584,195.882349121971,196.381057415357,
196.879765708744,197.378474002131,197.877182295517,197.920337176157),
 .UNSPECIFIED.);
#955=B_SPLINE_CURVE_WITH_KNOTS('',3,(#34850,#34851,#34852,#34853,#34854,
#34855,#34856,#34857,#34858,#34859,#34860,#34861,#34862,#34863,#34864,#34865),
 .UNSPECIFIED.,.F.,.F.,(4,1,1,1,1,1,1,1,1,1,1,1,1,4),(191.637151868978,
191.939096712418,192.437805005805,192.936513299191,193.435221592578,193.933929885965,
194.432638179351,194.931346472738,195.430054766124,195.928763059511,196.427471352898,
196.926179646284,197.424887939671,197.920337176157),.UNSPECIFIED.);
#956=B_SPLINE_CURVE_WITH_KNOTS('',3,(#34870,#34871,#34872,#34873,#34874,
#34875,#34876,#34877,#34878,#34879,#34880,#34881,#34882,#34883,#34884,#34885,
#34886),.UNSPECIFIED.,.F.,.F.,(4,1,1,1,1,1,1,1,1,1,1,1,1,1,4),(185.353966561798,
185.409474960852,185.908183254238,186.406891547625,186.905599841012,187.404308134398,
187.903016427785,188.401724721171,188.900433014558,189.399141307945,189.897849601331,
190.396557894718,190.895266188105,191.393974481491,191.637151868978),
 .UNSPECIFIED.);
#957=B_SPLINE_CURVE_WITH_KNOTS('',3,(#34887,#34888,#34889,#34890,#34891,
#34892,#34893,#34894,#34895,#34896,#34897,#34898,#34899,#34900,#34901,#34902,
#34903),.UNSPECIFIED.,.F.,.F.,(4,1,1,1,1,1,1,1,1,1,1,1,1,1,4),(185.353966561798,
185.455888898392,185.954597191779,186.453305485165,186.952013778552,187.450722071938,
187.949430365325,188.448138658712,188.946846952098,189.445555245485,189.944263538872,
190.442971832258,190.941680125645,191.440388419031,191.637151868978),
 .UNSPECIFIED.);
#958=B_SPLINE_CURVE_WITH_KNOTS('',3,(#34908,#34909,#34910,#34911,#34912,
#34913,#34914,#34915,#34916,#34917,#34918,#34919,#34920,#34921,#34922,#34923),
 .UNSPECIFIED.,.F.,.F.,(4,1,1,1,1,1,1,1,1,1,1,1,1,4),(179.070781254618,
179.424975440212,179.923683733599,180.422392026986,180.921100320372,181.419808613759,
181.918516907145,182.417225200532,182.915933493919,183.414641787305,183.913350080692,
184.412058374079,184.910766667465,185.353966561798),.UNSPECIFIED.);
#959=B_SPLINE_CURVE_WITH_KNOTS('',3,(#34924,#34925,#34926,#34927,#34928,
#34929,#34930,#34931,#34932,#34933,#34934,#34935,#34936,#34937,#34938,#34939),
 .UNSPECIFIED.,.F.,.F.,(4,1,1,1,1,1,1,1,1,1,1,1,1,4),(179.070781254618,
179.471389377753,179.970097671139,180.468805964526,180.967514257912,181.466222551299,
181.964930844686,182.463639138072,182.962347431459,183.461055724845,183.959764018232,
184.458472311619,184.957180605005,185.353966561798),.UNSPECIFIED.);
#960=B_SPLINE_CURVE_WITH_KNOTS('',3,(#34944,#34945,#34946,#34947,#34948,
#34949,#34950,#34951,#34952,#34953,#34954,#34955,#34956,#34957,#34958,#34959,
#34960),.UNSPECIFIED.,.F.,.F.,(4,1,1,1,1,1,1,1,1,1,1,1,1,1,4),(172.787595947439,
172.941767626186,173.440475919573,173.93918421296,174.437892506346,174.936600799733,
175.435309093119,175.934017386506,176.432725679893,176.931433973279,177.430142266666,
177.928850560052,178.427558853439,178.926267146826,179.070781254618),
 .UNSPECIFIED.);
#961=B_SPLINE_CURVE_WITH_KNOTS('',3,(#34961,#34962,#34963,#34964,#34965,
#34966,#34967,#34968,#34969,#34970,#34971,#34972,#34973,#34974,#34975,#34976,
#34977),.UNSPECIFIED.,.F.,.F.,(4,1,1,1,1,1,1,1,1,1,1,1,1,1,4),(172.787595947439,
172.988181563726,173.486889857113,173.9855981505,174.484306443886,174.983014737273,
175.48172303066,175.980431324046,176.479139617433,176.977847910819,177.476556204206,
177.975264497593,178.473972790979,178.972681084366,179.070781254618),
 .UNSPECIFIED.);
#962=B_SPLINE_CURVE_WITH_KNOTS('',3,(#34982,#34983,#34984,#34985,#34986,
#34987,#34988,#34989,#34990,#34991,#34992,#34993,#34994,#34995,#34996,#34997),
 .UNSPECIFIED.,.F.,.F.,(4,1,1,1,1,1,1,1,1,1,1,1,1,4),(166.504410640259,
166.957268105547,167.455976398933,167.95468469232,168.453392985707,168.952101279093,
169.45080957248,169.949517865867,170.448226159253,170.94693445264,171.445642746026,
171.944351039413,172.4430593328,172.787595947439),.UNSPECIFIED.);
#963=B_SPLINE_CURVE_WITH_KNOTS('',3,(#34998,#34999,#35000,#35001,#35002,
#35003,#35004,#35005,#35006,#35007,#35008,#35009,#35010,#35011,#35012,#35013,
#35014),.UNSPECIFIED.,.F.,.F.,(4,1,1,1,1,1,1,1,1,1,1,1,1,1,4),(166.504410640259,
166.5049737497,167.003682043087,167.502390336474,168.00109862986,168.499806923247,
168.998515216634,169.49722351002,169.995931803407,170.494640096793,170.99334839018,
171.492056683567,171.990764976953,172.48947327034,172.787595947439),
 .UNSPECIFIED.);
#964=B_SPLINE_CURVE_WITH_KNOTS('',3,(#35019,#35020,#35021,#35022,#35023,
#35024,#35025,#35026,#35027,#35028,#35029,#35030,#35031,#35032,#35033,#35034,
#35035),.UNSPECIFIED.,.F.,.F.,(4,1,1,1,1,1,1,1,1,1,1,1,1,1,4),(160.22122533308,
160.474060291521,160.972768584907,161.471476878294,161.970185171681,162.468893465067,
162.967601758454,163.466310051841,163.965018345227,164.463726638614,164.962434932,
165.461143225387,165.959851518774,166.45855981216,166.504410640259),
 .UNSPECIFIED.);
#965=B_SPLINE_CURVE_WITH_KNOTS('',3,(#35036,#35037,#35038,#35039,#35040,
#35041,#35042,#35043,#35044,#35045,#35046,#35047,#35048,#35049,#35050,#35051),
 .UNSPECIFIED.,.F.,.F.,(4,1,1,1,1,1,1,1,1,1,1,1,1,4),(160.22122533308,160.520474229061,
161.019182522448,161.517890815834,162.016599109221,162.515307402608,163.014015695994,
163.512723989381,164.011432282767,164.510140576154,165.008848869541,165.507557162927,
166.006265456314,166.504410640259),.UNSPECIFIED.);
#966=B_SPLINE_CURVE_WITH_KNOTS('',3,(#35056,#35057,#35058,#35059,#35060,
#35061,#35062,#35063,#35064,#35065,#35066,#35067,#35068,#35069,#35070,#35071,
#35072),.UNSPECIFIED.,.F.,.F.,(4,1,1,1,1,1,1,1,1,1,1,1,1,1,4),(153.9380400259,
153.990852477495,154.489560770881,154.988269064268,155.486977357655,155.985685651041,
156.484393944428,156.983102237814,157.481810531201,157.980518824588,158.479227117974,
158.977935411361,159.476643704748,159.975351998134,160.22122533308),
 .UNSPECIFIED.);
#967=B_SPLINE_CURVE_WITH_KNOTS('',3,(#35073,#35074,#35075,#35076,#35077,
#35078,#35079,#35080,#35081,#35082,#35083,#35084,#35085,#35086,#35087,#35088,
#35089),.UNSPECIFIED.,.F.,.F.,(4,1,1,1,1,1,1,1,1,1,1,1,1,1,4),(153.9380400259,
154.037266415035,154.535974708422,155.034683001808,155.533391295195,156.032099588581,
156.530807881968,157.029516175355,157.528224468741,158.026932762128,158.525641055515,
159.024349348901,159.523057642288,160.021765935674,160.22122533308),
 .UNSPECIFIED.);
#968=B_SPLINE_CURVE_WITH_KNOTS('',3,(#35094,#35095,#35096,#35097,#35098,
#35099,#35100,#35101,#35102,#35103,#35104,#35105,#35106,#35107,#35108,#35109),
 .UNSPECIFIED.,.F.,.F.,(4,1,1,1,1,1,1,1,1,1,1,1,1,4),(147.654854718721,
148.006352956855,148.505061250242,149.003769543629,149.502477837015,150.001186130402,
150.499894423788,150.998602717175,151.497311010562,151.996019303948,152.494727597335,
152.993435890721,153.492144184108,153.9380400259),.UNSPECIFIED.);
#969=B_SPLINE_CURVE_WITH_KNOTS('',3,(#35110,#35111,#35112,#35113,#35114,
#35115,#35116,#35117,#35118,#35119,#35120,#35121,#35122,#35123,#35124,#35125),
 .UNSPECIFIED.,.F.,.F.,(4,1,1,1,1,1,1,1,1,1,1,1,1,4),(147.654854718721,
148.052766894396,148.551475187782,149.050183481169,149.548891774555,150.047600067942,
150.546308361329,151.045016654715,151.543724948102,152.042433241488,152.541141534875,
153.039849828262,153.538558121648,153.9380400259),.UNSPECIFIED.);
#970=B_SPLINE_CURVE_WITH_KNOTS('',3,(#35130,#35131,#35132,#35133,#35134,
#35135,#35136,#35137,#35138,#35139,#35140,#35141,#35142),.UNSPECIFIED.,
 .F.,.F.,(4,1,1,1,1,1,1,1,1,1,4),(141.371669411541,141.523145142829,142.520561729602,
143.517978316376,144.515394903149,145.512811489922,146.011519783309,146.510228076695,
147.008936370082,147.507644663469,147.654854718721),.UNSPECIFIED.);
#971=B_SPLINE_CURVE_WITH_KNOTS('',3,(#35143,#35144,#35145,#35146,#35147,
#35148,#35149,#35150,#35151,#35152),.UNSPECIFIED.,.F.,.F.,(4,1,1,1,1,1,
1,4),(141.371669411541,142.068267373756,143.065683960529,144.063100547303,
145.060517134076,146.057933720849,147.055350307622,147.654854718721),
 .UNSPECIFIED.);
#972=B_SPLINE_CURVE_WITH_KNOTS('',3,(#35157,#35158,#35159,#35160,#35161,
#35162,#35163,#35164,#35165,#35166),.UNSPECIFIED.,.F.,.F.,(4,1,1,1,1,1,
1,4),(135.088484104362,135.53864562219,136.536062208963,137.533478795736,
138.53089538251,139.528311969283,140.525728556056,141.371669411541),
 .UNSPECIFIED.);
#973=B_SPLINE_CURVE_WITH_KNOTS('',3,(#35167,#35168,#35169,#35170,#35171,
#35172,#35173,#35174,#35175,#35176),.UNSPECIFIED.,.F.,.F.,(4,1,1,1,1,1,
1,4),(135.088484104362,136.083767853117,137.08118443989,138.078601026663,
139.076017613436,140.07343420021,141.070850786983,141.371669411541),
 .UNSPECIFIED.);
#974=B_SPLINE_CURVE_WITH_KNOTS('',3,(#35181,#35182,#35183,#35184,#35185,
#35186,#35187,#35188,#35189,#35190,#35191,#35192,#35193),.UNSPECIFIED.,
 .F.,.F.,(4,1,1,1,1,1,1,1,1,1,4),(128.805298797182,129.055437808164,129.55414610155,
130.052854394937,130.551562688324,131.05027098171,131.548979275097,132.54639586187,
133.543812448643,134.541229035417,135.088484104362),.UNSPECIFIED.);
#975=B_SPLINE_CURVE_WITH_KNOTS('',3,(#35194,#35195,#35196,#35197,#35198,
#35199,#35200,#35201,#35202,#35203,#35204,#35205,#35206,#35207,#35208,#35209),
 .UNSPECIFIED.,.F.,.F.,(4,1,1,1,1,1,1,1,1,1,1,1,1,4),(128.805298797182,
129.101851745704,129.600560039091,130.099268332477,130.597976625864,131.09668491925,
131.595393212637,132.094101506024,132.59280979941,133.091518092797,133.590226386184,
134.08893467957,135.086351266343,135.088484104362),.UNSPECIFIED.);
#976=B_SPLINE_CURVE_WITH_KNOTS('',3,(#35214,#35215,#35216,#35217,#35218,
#35219,#35220,#35221,#35222,#35223,#35224,#35225,#35226,#35227,#35228,#35229,
#35230),.UNSPECIFIED.,.F.,.F.,(4,1,1,1,1,1,1,1,1,1,1,1,1,1,4),(122.522113490002,
122.572229994138,123.070938287524,123.569646580911,124.068354874298,124.567063167684,
125.065771461071,125.564479754457,126.063188047844,126.561896341231,127.060604634617,
127.559312928004,128.058021221391,128.556729514777,128.805298797182),
 .UNSPECIFIED.);
#977=B_SPLINE_CURVE_WITH_KNOTS('',3,(#35231,#35232,#35233,#35234,#35235,
#35236,#35237,#35238,#35239,#35240,#35241,#35242,#35243,#35244,#35245,#35246,
#35247),.UNSPECIFIED.,.F.,.F.,(4,1,1,1,1,1,1,1,1,1,1,1,1,1,4),(122.522113490002,
122.618643931678,123.117352225065,123.616060518451,124.114768811838,124.613477105224,
125.112185398611,125.610893691998,126.109601985384,126.608310278771,127.107018572158,
127.605726865544,128.104435158931,128.603143452317,128.805298797182),
 .UNSPECIFIED.);
#978=B_SPLINE_CURVE_WITH_KNOTS('',3,(#35252,#35253,#35254,#35255,#35256,
#35257,#35258,#35259,#35260,#35261,#35262,#35263,#35264,#35265,#35266,#35267),
 .UNSPECIFIED.,.F.,.F.,(4,1,1,1,1,1,1,1,1,1,1,1,1,4),(116.238928182823,
116.587730473498,117.086438766885,117.585147060271,118.083855353658,118.582563647045,
119.081271940431,119.579980233818,120.078688527205,120.577396820591,121.076105113978,
121.574813407364,122.073521700751,122.522113490002),.UNSPECIFIED.);
#979=B_SPLINE_CURVE_WITH_KNOTS('',3,(#35268,#35269,#35270,#35271,#35272,
#35273,#35274,#35275,#35276,#35277,#35278,#35279,#35280,#35281,#35282,#35283),
 .UNSPECIFIED.,.F.,.F.,(4,1,1,1,1,1,1,1,1,1,1,1,1,4),(116.238928182823,
116.634144411039,117.132852704425,117.631560997812,118.130269291198,118.628977584585,
119.127685877972,119.626394171358,120.125102464745,120.623810758131,121.122519051518,
121.621227344905,122.119935638291,122.522113490002),.UNSPECIFIED.);
#980=B_SPLINE_CURVE_WITH_KNOTS('',3,(#35288,#35289,#35290,#35291,#35292,
#35293,#35294,#35295,#35296,#35297,#35298,#35299,#35300,#35301,#35302,#35303,
#35304),.UNSPECIFIED.,.F.,.F.,(4,1,1,1,1,1,1,1,1,1,1,1,1,1,4),(109.955742875643,
110.104522659472,110.603230952859,111.101939246245,111.600647539632,112.099355833019,
112.598064126405,113.096772419792,113.595480713179,114.094189006565,114.592897299952,
115.091605593338,115.590313886725,116.089022180112,116.238928182823),
 .UNSPECIFIED.);
#981=B_SPLINE_CURVE_WITH_KNOTS('',3,(#35305,#35306,#35307,#35308,#35309,
#35310,#35311,#35312,#35313,#35314,#35315,#35316,#35317,#35318,#35319,#35320,
#35321),.UNSPECIFIED.,.F.,.F.,(4,1,1,1,1,1,1,1,1,1,1,1,1,1,4),(109.955742875643,
110.150936597012,110.649644890399,111.148353183786,111.647061477172,112.145769770559,
112.644478063946,113.143186357332,113.641894650719,114.140602944105,114.639311237492,
115.138019530879,115.636727824265,116.135436117652,116.238928182823),
 .UNSPECIFIED.);
#982=B_SPLINE_CURVE_WITH_KNOTS('',3,(#35326,#35327,#35328,#35329,#35330,
#35331,#35332,#35333,#35334,#35335,#35336,#35337,#35338,#35339,#35340,#35341),
 .UNSPECIFIED.,.F.,.F.,(4,1,1,1,1,1,1,1,1,1,1,1,1,4),(103.672557568464,
104.120023138833,104.618731432219,105.117439725606,105.616148018993,106.114856312379,
106.613564605766,107.112272899152,107.610981192539,108.109689485926,108.608397779312,
109.107106072699,109.605814366086,109.955742875643),.UNSPECIFIED.);
#983=B_SPLINE_CURVE_WITH_KNOTS('',3,(#35342,#35343,#35344,#35345,#35346,
#35347,#35348,#35349,#35350,#35351,#35352,#35353,#35354,#35355,#35356,#35357),
 .UNSPECIFIED.,.F.,.F.,(4,1,1,1,1,1,1,1,1,1,1,1,1,4),(103.672557568464,
104.166437076373,104.66514536976,105.163853663146,105.662561956533,106.161270249919,
106.659978543306,107.158686836693,107.657395130079,108.156103423466,108.654811716853,
109.153520010239,109.652228303626,109.955742875643),.UNSPECIFIED.);
#984=B_SPLINE_CURVE_WITH_KNOTS('',3,(#35362,#35363,#35364,#35365,#35366,
#35367,#35368,#35369,#35370,#35371,#35372,#35373,#35374,#35375,#35376,#35377,
#35378),.UNSPECIFIED.,.F.,.F.,(4,1,1,1,1,1,1,1,1,1,1,1,1,1,4),(97.389372261284,
97.6368153248067,98.1355236181933,98.63423191158,99.1329402049666,99.6316484983532,
100.13035679174,100.629065085126,101.127773378513,101.6264816719,102.125189965286,
102.623898258673,103.12260655206,103.621314845446,103.672557568464),
 .UNSPECIFIED.);
#985=B_SPLINE_CURVE_WITH_KNOTS('',3,(#35379,#35380,#35381,#35382,#35383,
#35384,#35385,#35386,#35387,#35388,#35389,#35390,#35391,#35392,#35393,#35394,
#35395),.UNSPECIFIED.,.F.,.F.,(4,1,1,1,1,1,1,1,1,1,1,1,1,1,4),(97.389372261284,
97.683229262347,98.1819375557336,98.6806458491202,99.1793541425068,99.6780624358935,
100.17677072928,100.675479022667,101.174187316053,101.67289560944,102.171603902827,
102.670312196213,103.1690204896,103.667728782986,103.672557568464),
 .UNSPECIFIED.);
#986=B_SPLINE_CURVE_WITH_KNOTS('',3,(#35400,#35401,#35402,#35403,#35404,
#35405,#35406,#35407,#35408,#35409,#35410,#35411,#35412,#35413,#35414,#35415,
#35416),.UNSPECIFIED.,.F.,.F.,(4,1,1,1,1,1,1,1,1,1,1,1,1,1,4),(91.1061869541044,
91.1536075107807,91.6523158041673,92.1510240975539,92.6497323909405,93.1484406843271,
93.6471489777138,94.1458572711004,94.644565564487,95.1432738578736,95.6419821512603,
96.1406904446469,96.6393987380335,97.1381070314201,97.389372261284),
 .UNSPECIFIED.);
#987=B_SPLINE_CURVE_WITH_KNOTS('',3,(#35417,#35418,#35419,#35420,#35421,
#35422,#35423,#35424,#35425,#35426,#35427,#35428,#35429,#35430,#35431,#35432,
#35433),.UNSPECIFIED.,.F.,.F.,(4,1,1,1,1,1,1,1,1,1,1,1,1,1,4),(91.1061869541044,
91.2000214483209,91.6987297417075,92.1974380350942,92.6961463284808,93.1948546218674,
93.693562915254,94.1922712086406,94.6909795020272,95.1896877954139,95.6883960888005,
96.1871043821871,96.6858126755737,97.1845209689603,97.389372261284),
 .UNSPECIFIED.);
#988=B_SPLINE_CURVE_WITH_KNOTS('',3,(#35438,#35439,#35440,#35441,#35442,
#35443,#35444,#35445,#35446,#35447,#35448,#35449,#35450,#35451,#35452,#35453),
 .UNSPECIFIED.,.F.,.F.,(4,1,1,1,1,1,1,1,1,1,1,1,1,4),(84.8230016469248,
85.1691079901412,85.6678162835279,86.1665245769145,86.6652328703011,87.1639411636877,
87.6626494570743,88.161357750461,88.6600660438476,89.1587743372342,89.6574826306208,
90.1561909240074,90.654899217394,91.1061869541044),.UNSPECIFIED.);
#989=B_SPLINE_CURVE_WITH_KNOTS('',3,(#35454,#35455,#35456,#35457,#35458,
#35459,#35460,#35461,#35462,#35463,#35464,#35465,#35466,#35467,#35468,#35469),
 .UNSPECIFIED.,.F.,.F.,(4,1,1,1,1,1,1,1,1,1,1,1,1,4),(84.8230016469248,
85.2155219276815,85.7142302210681,86.2129385144547,86.7116468078413,87.2103551012279,
87.7090633946146,88.2077716880012,88.7064799813878,89.2051882747744,89.703896568161,
90.2026048615477,90.7013131549343,91.1061869541044),.UNSPECIFIED.);
#990=B_SPLINE_CURVE_WITH_KNOTS('',3,(#35474,#35475,#35476,#35477,#35478,
#35479,#35480,#35481,#35482,#35483,#35484,#35485,#35486,#35487,#35488,#35489,
#35490),.UNSPECIFIED.,.F.,.F.,(4,1,1,1,1,1,1,1,1,1,1,1,1,1,4),(78.5398163397452,
78.6859001761152,79.1846084695018,79.6833167628884,80.1820250562751,80.6807333496617,
81.1794416430483,81.6781499364349,82.1768582298215,82.6755665232081,83.1742748165948,
83.6729831099814,84.171691403368,84.6703996967546,84.8230016469248),
 .UNSPECIFIED.);
#991=B_SPLINE_CURVE_WITH_KNOTS('',3,(#35491,#35492,#35493,#35494,#35495,
#35496,#35497,#35498,#35499,#35500,#35501,#35502,#35503,#35504,#35505,#35506,
#35507),.UNSPECIFIED.,.F.,.F.,(4,1,1,1,1,1,1,1,1,1,1,1,1,1,4),(78.5398163397452,
78.7323141136554,79.231022407042,79.7297307004287,80.2284389938153,80.7271472872019,
81.2258555805885,81.7245638739751,82.2232721673618,82.7219804607484,83.220688754135,
83.7193970475216,84.2181053409082,84.7168136342949,84.8230016469248),
 .UNSPECIFIED.);
#992=B_SPLINE_CURVE_WITH_KNOTS('',3,(#35512,#35513,#35514,#35515,#35516,
#35517,#35518,#35519,#35520,#35521,#35522,#35523,#35524,#35525,#35526,#35527),
 .UNSPECIFIED.,.F.,.F.,(4,1,1,1,1,1,1,1,1,1,1,1,1,4),(72.2566310325657,
72.7014006554758,73.2001089488624,73.698817242249,74.1975255356356,74.6962338290222,
75.1949421224089,75.6936504157955,76.1923587091821,76.6910670025687,77.1897752959553,
77.6884835893419,78.1871918827286,78.5398163397452),.UNSPECIFIED.);
#993=B_SPLINE_CURVE_WITH_KNOTS('',3,(#35528,#35529,#35530,#35531,#35532,
#35533,#35534,#35535,#35536,#35537,#35538,#35539,#35540,#35541,#35542,#35543),
 .UNSPECIFIED.,.F.,.F.,(4,1,1,1,1,1,1,1,1,1,1,1,1,4),(72.2566310325657,
72.747814593016,73.2465228864026,73.7452311797892,74.2439394731758,74.7426477665625,
75.2413560599491,75.7400643533357,76.2387726467223,76.7374809401089,77.2361892334956,
77.7348975268822,78.2336058202688,78.5398163397452),.UNSPECIFIED.);
#994=B_SPLINE_CURVE_WITH_KNOTS('',3,(#35548,#35549,#35550,#35551,#35552,
#35553,#35554,#35555,#35556,#35557,#35558,#35559,#35560,#35561,#35562,#35563,
#35564),.UNSPECIFIED.,.F.,.F.,(4,1,1,1,1,1,1,1,1,1,1,1,1,1,4),(65.973445725386,
66.2181928414497,66.7169011348363,67.2156094282229,67.7143177216096,68.2130260149962,
68.7117343083828,69.2104426017694,69.709150895156,70.2078591885427,70.7065674819293,
71.2052757753159,71.7039840687025,72.2026923620891,72.2566310325657),
 .UNSPECIFIED.);
#995=B_SPLINE_CURVE_WITH_KNOTS('',3,(#35565,#35566,#35567,#35568,#35569,
#35570,#35571,#35572,#35573,#35574,#35575,#35576,#35577,#35578,#35579,#35580,
#35581),.UNSPECIFIED.,.F.,.F.,(4,1,1,1,1,1,1,1,1,1,1,1,1,1,4),(65.973445725386,
66.2646067789899,66.7633150723765,67.2620233657632,67.7607316591498,68.2594399525364,
68.758148245923,69.2568565393096,69.7555648326963,70.2542731260829,70.7529814194695,
71.2516897128561,71.7503980062427,72.2491062996294,72.2566310325657),
 .UNSPECIFIED.);
#996=B_SPLINE_CURVE_WITH_KNOTS('',3,(#35586,#35587,#35588,#35589,#35590,
#35591,#35592,#35593,#35594,#35595,#35596,#35597,#35598,#35599,#35600,#35601,
#35602),.UNSPECIFIED.,.F.,.F.,(4,1,1,1,1,1,1,1,1,1,1,1,1,1,4),(59.6902604182065,
59.7349850274237,60.2336933208103,60.7324016141969,61.2311099075835,61.7298182009701,
62.2285264943567,62.7272347877434,63.22594308113,63.7246513745166,64.2233596679032,
64.7220679612898,65.2207762546765,65.7194845480631,65.973445725386),
 .UNSPECIFIED.);
#997=B_SPLINE_CURVE_WITH_KNOTS('',3,(#35603,#35604,#35605,#35606,#35607,
#35608,#35609,#35610,#35611,#35612,#35613,#35614,#35615,#35616,#35617,#35618,
#35619),.UNSPECIFIED.,.F.,.F.,(4,1,1,1,1,1,1,1,1,1,1,1,1,1,4),(59.6902604182065,
59.7813989649639,60.2801072583505,60.7788155517371,61.2775238451237,61.7762321385104,
62.274940431897,62.7736487252836,63.2723570186702,63.7710653120568,64.2697736054434,
64.7684818988301,65.2671901922167,65.7658984856033,65.973445725386),
 .UNSPECIFIED.);
#998=B_SPLINE_CURVE_WITH_KNOTS('',3,(#35624,#35625,#35626,#35627,#35628,
#35629,#35630,#35631,#35632,#35633,#35634,#35635,#35636,#35637,#35638,#35639),
 .UNSPECIFIED.,.F.,.F.,(4,1,1,1,1,1,1,1,1,1,1,1,1,4),(53.4070751110269,
53.7504855067842,54.2491938001708,54.7479020935575,55.2466103869441,55.7453186803307,
56.2440269737173,56.7427352671039,57.2414435604906,57.7401518538772,58.2388601472638,
58.7375684406504,59.236276734037,59.6902604182065),.UNSPECIFIED.);
#999=B_SPLINE_CURVE_WITH_KNOTS('',3,(#35640,#35641,#35642,#35643,#35644,
#35645,#35646,#35647,#35648,#35649,#35650,#35651,#35652,#35653,#35654,#35655),
 .UNSPECIFIED.,.F.,.F.,(4,1,1,1,1,1,1,1,1,1,1,1,1,4),(53.4070751110269,
53.7968994443244,54.2956077377111,54.7943160310977,55.2930243244843,55.7917326178709,
56.2904409112575,56.7891492046442,57.2878574980308,57.7865657914174,58.285274084804,
58.7839823781906,59.2826906715772,59.6902604182065),.UNSPECIFIED.);
#1000=B_SPLINE_CURVE_WITH_KNOTS('',3,(#35660,#35661,#35662,#35663,#35664,
#35665,#35666,#35667,#35668,#35669,#35670,#35671,#35672,#35673,#35674,#35675,
#35676),.UNSPECIFIED.,.F.,.F.,(4,1,1,1,1,1,1,1,1,1,1,1,1,1,4),(47.1238898038473,
47.2672776927582,47.7659859861448,48.2646942795314,48.763402572918,49.2621108663046,
49.7608191596913,50.2595274530779,50.7582357464645,51.2569440398511,51.7556523332377,
52.2543606266244,52.753068920011,53.2517772133976,53.4070751110269),
 .UNSPECIFIED.);
#1001=B_SPLINE_CURVE_WITH_KNOTS('',3,(#35677,#35678,#35679,#35680,#35681,
#35682,#35683,#35684,#35685,#35686,#35687,#35688,#35689,#35690,#35691,#35692,
#35693),.UNSPECIFIED.,.F.,.F.,(4,1,1,1,1,1,1,1,1,1,1,1,1,1,4),(47.1238898038473,
47.3136916302984,47.812399923685,48.3111082170716,48.8098165104582,49.3085248038449,
49.8072330972315,50.3059413906181,50.8046496840047,51.3033579773913,51.802066270778,
52.3007745641646,52.7994828575512,53.2981911509378,53.4070751110269),
 .UNSPECIFIED.);
#1002=B_SPLINE_CURVE_WITH_KNOTS('',3,(#35698,#35699,#35700,#35701,#35702,
#35703,#35704,#35705,#35706,#35707,#35708,#35709,#35710,#35711,#35712,#35713),
 .UNSPECIFIED.,.F.,.F.,(4,1,1,1,1,1,1,1,1,1,1,1,1,4),(40.8407044966677,
41.2827781721187,41.7814864655054,42.280194758892,42.7789030522786,43.2776113456652,
43.7763196390518,44.2750279324384,44.7737362258251,45.2724445192117,45.7711528125983,
46.2698611059849,46.7685693993716,47.1238898038473),.UNSPECIFIED.);
#1003=B_SPLINE_CURVE_WITH_KNOTS('',3,(#35714,#35715,#35716,#35717,#35718,
#35719,#35720,#35721,#35722,#35723,#35724,#35725,#35726,#35727,#35728,#35729),
 .UNSPECIFIED.,.F.,.F.,(4,1,1,1,1,1,1,1,1,1,1,1,1,4),(40.8407044966677,
41.3291921096589,41.8279004030456,42.3266086964322,42.8253169898188,43.3240252832054,
43.822733576592,44.3214418699787,44.8201501633653,45.3188584567519,45.8175667501385,
46.3162750435251,46.8149833369118,47.1238898038473),.UNSPECIFIED.);
#1004=B_SPLINE_CURVE_WITH_KNOTS('',3,(#35734,#35735,#35736,#35737,#35738,
#35739,#35740,#35741,#35742,#35743,#35744,#35745,#35746,#35747,#35748,#35749,
#35750),.UNSPECIFIED.,.F.,.F.,(4,1,1,1,1,1,1,1,1,1,1,1,1,1,4),(34.5575191894881,
34.7995703580927,35.2982786514793,35.7969869448659,36.2956952382525,36.7944035316392,
37.2931118250258,37.7918201184124,38.290528411799,38.7892367051856,39.2879449985723,
39.7866532919589,40.2853615853455,40.7840698787321,40.8407044966677),
 .UNSPECIFIED.);
#1005=B_SPLINE_CURVE_WITH_KNOTS('',3,(#35751,#35752,#35753,#35754,#35755,
#35756,#35757,#35758,#35759,#35760,#35761,#35762,#35763,#35764,#35765,#35766,
#35767),.UNSPECIFIED.,.F.,.F.,(4,1,1,1,1,1,1,1,1,1,1,1,1,1,4),(34.5575191894881,
34.8459842956329,35.3446925890195,35.8434008824061,36.3421091757927,36.8408174691794,
37.339525762566,37.8382340559526,38.3369423493392,38.8356506427259,39.3343589361125,
39.8330672294991,40.3317755228857,40.8304838162723,40.8407044966677),
 .UNSPECIFIED.);
#1006=B_SPLINE_CURVE_WITH_KNOTS('',3,(#35772,#35773,#35774,#35775,#35776,
#35777,#35778,#35779,#35780,#35781,#35782,#35783,#35784,#35785,#35786,#35787,
#35788),.UNSPECIFIED.,.F.,.F.,(4,1,1,1,1,1,1,1,1,1,1,1,1,1,4),(28.2743338823085,
28.3163625440666,28.8150708374532,29.3137791308399,29.8124874242265,30.3111957176131,
30.8099040109997,31.3086123043863,31.807320597773,32.3060288911596,32.8047371845462,
33.3034454779328,33.8021537713194,34.3008620647061,34.5575191894881),
 .UNSPECIFIED.);
#1007=B_SPLINE_CURVE_WITH_KNOTS('',3,(#35789,#35790,#35791,#35792,#35793,
#35794,#35795,#35796,#35797,#35798,#35799,#35800,#35801,#35802,#35803,#35804,
#35805),.UNSPECIFIED.,.F.,.F.,(4,1,1,1,1,1,1,1,1,1,1,1,1,1,4),(28.2743338823085,
28.3627764816068,28.8614847749935,29.3601930683801,29.8589013617667,30.3576096551533,
30.8563179485399,31.3550262419266,31.8537345353132,32.3524428286998,32.8511511220864,
33.349859415473,33.8485677088597,34.3472760022463,34.5575191894881),
 .UNSPECIFIED.);
#1008=B_SPLINE_CURVE_WITH_KNOTS('',3,(#35810,#35811,#35812,#35813,#35814,
#35815,#35816,#35817,#35818,#35819,#35820,#35821,#35822,#35823,#35824,#35825),
 .UNSPECIFIED.,.F.,.F.,(4,1,1,1,1,1,1,1,1,1,1,1,1,4),(21.9911485751289,
22.3318630234272,22.8305713168138,23.3292796102004,23.8279879035871,24.3266961969737,
24.8254044903603,25.3241127837469,25.8228210771335,26.3215293705201,26.8202376639068,
27.3189459572934,27.81765425068,28.2743338823085),.UNSPECIFIED.);
#1009=B_SPLINE_CURVE_WITH_KNOTS('',3,(#35826,#35827,#35828,#35829,#35830,
#35831,#35832,#35833,#35834,#35835,#35836,#35837,#35838,#35839,#35840,#35841),
 .UNSPECIFIED.,.F.,.F.,(4,1,1,1,1,1,1,1,1,1,1,1,1,4),(21.9911485751289,
22.3782769609674,22.876985254354,23.3756935477406,23.8744018411273,24.3731101345139,
24.8718184279005,25.3705267212871,25.8692350146737,26.3679433080604,26.866651601447,
27.3653598948336,27.8640681882202,28.2743338823085),.UNSPECIFIED.);
#1010=B_SPLINE_CURVE_WITH_KNOTS('',3,(#35847,#35848,#35849,#35850,#35851,
#35852),.UNSPECIFIED.,.F.,.F.,(4,1,1,4),(14.3989442667815,14.8976525601681,
15.3963608535547,15.7079632679493),.UNSPECIFIED.);
#1011=B_SPLINE_CURVE_WITH_KNOTS('',3,(#35855,#35856,#35857,#35858,#35859,
#35860,#35861),.UNSPECIFIED.,.F.,.F.,(4,1,1,1,4),(13.8753896155274,14.3525303292413,
14.8512386226279,15.3499469160145,15.7079632679493),.UNSPECIFIED.);
#1012=B_SPLINE_CURVE_WITH_KNOTS('',3,(#35863,#35864,#35865,#35866,#35867,
#35868,#35869,#35870,#35871,#35872,#35873,#35874,#35875,#35876,#35877,#35878,
#35879,#35880,#35881,#35882,#35883,#35884,#35885,#35886,#35887,#35888,#35889,
#35890,#35891,#35892,#35893,#35894,#35895,#35896,#35897,#35898,#35899,#35900,
#35901,#35902,#35903,#35904,#35905,#35906,#35907,#35908,#35909,#35910,#35911,
#35912,#35913,#35914,#35915,#35916,#35917,#35918,#35919,#35920,#35921,#35922,
#35923,#35924,#35925,#35926,#35927,#35928,#35929,#35930,#35931,#35932,#35933,
#35934,#35935,#35936,#35937,#35938,#35939,#35940,#35941,#35942,#35943,#35944,
#35945,#35946,#35947,#35948,#35949,#35950,#35951,#35952,#35953,#35954,#35955,
#35956,#35957,#35958,#35959,#35960,#35961,#35962,#35963,#35964,#35965,#35966,
#35967,#35968),.UNSPECIFIED.,.F.,.F.,(4,3,3,3,3,3,3,3,3,3,3,3,3,3,3,3,3,
3,3,3,3,3,3,3,3,3,3,3,3,3,3,3,3,3,3,4),(-0.972375876542216,-0.931557379101648,
-0.890218542042487,-0.869392708916521,-0.861677237530619,-0.819813801882793,
-0.781167845425456,-0.769475619651221,-0.760546025724648,-0.754411794373795,
-0.74252188896812,-0.700976733031894,-0.65877791376378,-0.616292150528589,
-0.588572673703484,-0.579879678859757,-0.574332463387633,-0.531223905437004,
-0.505414243228169,-0.462559206201071,-0.419378313085458,-0.399643768345371,
-0.391565714980685,-0.383732909736738,-0.340135839018284,-0.296193649678293,
-0.261501955164762,-0.217668074296404,-0.204748702273309,-0.197210738162037,
-0.192140598791969,-0.1468449795757,-0.102253744983165,-0.0566059334550285,
-0.0109581219268922,0.),.UNSPECIFIED.);
#1013=B_SPLINE_CURVE_WITH_KNOTS('',3,(#35969,#35970,#35971,#35972,#35973,
#35974,#35975,#35976,#35977,#35978,#35979,#35980,#35981,#35982,#35983,#35984,
#35985,#35986,#35987,#35988,#35989,#35990,#35991,#35992,#35993,#35994,#35995,
#35996,#35997,#35998,#35999,#36000,#36001,#36002,#36003,#36004,#36005,#36006,
#36007,#36008,#36009,#36010,#36011,#36012,#36013,#36014,#36015,#36016,#36017,
#36018,#36019,#36020,#36021,#36022,#36023,#36024,#36025,#36026,#36027,#36028,
#36029,#36030,#36031,#36032,#36033,#36034,#36035,#36036,#36037,#36038,#36039,
#36040,#36041,#36042,#36043,#36044,#36045,#36046,#36047,#36048,#36049,#36050,
#36051,#36052,#36053,#36054,#36055,#36056,#36057,#36058,#36059,#36060,#36061,
#36062,#36063,#36064,#36065,#36066,#36067,#36068,#36069,#36070,#36071),
 .UNSPECIFIED.,.F.,.F.,(4,3,3,3,3,3,3,3,3,3,3,3,3,3,3,3,3,3,3,3,3,3,3,3,
3,3,3,3,3,3,3,3,3,3,4),(-0.970006587573357,-0.925489021709122,-0.880831606117785,
-0.860106336836479,-0.852213503588024,-0.808023919462815,-0.764142093829507,
-0.741127929891385,-0.732995659095006,-0.720260268196198,-0.676886083169421,
-0.633189091074775,-0.58989356338977,-0.561603730397805,-0.548456029491321,
-0.542926374323804,-0.500045602531121,-0.476734231421911,-0.433752968122039,
-0.390893110149348,-0.372012672166435,-0.363955407652349,-0.356648068723258,
-0.314412819484753,-0.272458136815843,-0.239849606286048,-0.197688110523089,
-0.185715478561588,-0.179206252930902,-0.173732780061183,-0.132200928727762,
-0.0907046629355285,-0.0499294541163457,-0.00977294415302305,0.),
 .UNSPECIFIED.);
#1014=B_SPLINE_CURVE_WITH_KNOTS('',3,(#36073,#36074,#36075,#36076,#36077,
#36078,#36079,#36080,#36081,#36082,#36083,#36084,#36085,#36086,#36087,#36088,
#36089),.UNSPECIFIED.,.F.,.F.,(4,1,1,1,1,1,1,1,1,1,1,1,1,1,4),(15.7079632679493,
15.8486552094011,16.3473635027878,16.8460717961744,17.344780089561,17.8434883829476,
18.3421966763342,18.8409049697209,19.3396132631075,19.8383215564941,20.3370298498807,
20.8357381432673,21.334446436654,21.8331547300406,21.9911485751289),
 .UNSPECIFIED.);
#1015=B_SPLINE_CURVE_WITH_KNOTS('',3,(#36090,#36091,#36092,#36093,#36094,
#36095,#36096,#36097,#36098,#36099,#36100,#36101,#36102,#36103,#36104,#36105,
#36106),.UNSPECIFIED.,.F.,.F.,(4,1,1,1,1,1,1,1,1,1,1,1,1,1,4),(15.7079632679493,
15.8950691469414,16.393777440328,16.8924857337146,17.3911940271012,17.8899023204878,
18.3886106138744,18.8873189072611,19.3860272006477,19.8847354940343,20.3834437874209,
20.8821520808075,21.3808603741942,21.8795686675808,21.9911485751289),
 .UNSPECIFIED.);
#1016=B_SPLINE_CURVE_WITH_KNOTS('',3,(#38095,#38096,#38097,#38098,#38099,
#38100,#38101,#38102,#38103,#38104,#38105,#38106,#38107,#38108,#38109,#38110,
#38111,#38112,#38113,#38114,#38115,#38116,#38117,#38118,#38119,#38120,#38121,
#38122,#38123,#38124,#38125,#38126,#38127,#38128,#38129,#38130,#38131,#38132,
#38133,#38134,#38135,#38136,#38137,#38138,#38139,#38140,#38141,#38142,#38143,
#38144,#38145,#38146,#38147,#38148,#38149,#38150,#38151,#38152,#38153,#38154,
#38155,#38156,#38157,#38158,#38159,#38160,#38161,#38162,#38163,#38164,#38165,
#38166,#38167,#38168,#38169,#38170,#38171,#38172,#38173,#38174,#38175,#38176,
#38177,#38178,#38179,#38180,#38181,#38182,#38183,#38184,#38185,#38186,#38187,
#38188,#38189,#38190,#38191,#38192,#38193,#38194,#38195,#38196,#38197,#38198,
#38199,#38200),.UNSPECIFIED.,.F.,.F.,(4,3,3,3,3,3,3,3,3,3,3,3,3,3,3,3,3,
3,3,3,3,3,3,3,3,3,3,3,3,3,3,3,3,3,3,4),(0.,0.040424976116911,0.081552621191953,
0.123116379418818,0.164484386952486,0.177258002125512,0.182429040513286,
0.224585211732574,0.229750939065668,0.271485437391992,0.313663426362065,
0.351832391899687,0.358992185792409,0.364434825962351,0.407093430609824,
0.45008484068709,0.466339288512555,0.509174339674324,0.534227886997736,
0.545013114142881,0.550666578456316,0.593964513128218,0.637614398405316,
0.68114810979745,0.709602718261623,0.725600523556765,0.736529828545389,
0.743509911151027,0.78723345430323,0.830193673824424,0.848440235266336,
0.858098500020291,0.902703209392534,0.947246712359152,0.959074332388006,
0.970006587573436),.UNSPECIFIED.);
#1017=B_SPLINE_CURVE_WITH_KNOTS('',3,(#38201,#38202,#38203,#38204,#38205,
#38206,#38207,#38208,#38209,#38210,#38211,#38212,#38213,#38214,#38215,#38216,
#38217,#38218,#38219,#38220,#38221,#38222,#38223,#38224,#38225,#38226,#38227,
#38228,#38229,#38230,#38231,#38232,#38233,#38234,#38235,#38236,#38237,#38238,
#38239,#38240,#38241,#38242,#38243),.UNSPECIFIED.,.F.,.F.,(4,3,3,3,3,3,
3,3,3,3,3,3,3,3,4),(-10.1321597128207,-9.97416586773239,-9.47545757434577,
-8.97674928095915,-8.47804098757253,-7.97933269418591,-7.48062440079929,
-6.98191610741267,-6.48320781402605,-5.98449952063943,-5.48579122725281,
-4.98708293386619,-4.48837464047957,-3.98966634709295,-3.84897440564115),
 .UNSPECIFIED.);
#1018=B_SPLINE_CURVE_WITH_KNOTS('',3,(#40232,#40233,#40234,#40235,#40236,
#40237,#40238,#40239,#40240,#40241,#40242,#40243,#40244,#40245,#40246,#40247,
#40248,#40249,#40250,#40251,#40252,#40253,#40254,#40255,#40256,#40257,#40258,
#40259,#40260,#40261,#40262,#40263,#40264,#40265,#40266,#40267,#40268,#40269,
#40270,#40271),.UNSPECIFIED.,.F.,.F.,(4,3,3,3,3,3,3,3,3,3,3,3,3,4),(7.59220430834772,
7.97933269418591,8.47804098757253,8.97674928095915,9.47545757434577,9.97416586773239,
10.472874161119,10.9715824545056,11.4702907478922,11.9689990412789,12.4677073346655,
12.9664156280521,13.4651239214387,13.8753896155273),.UNSPECIFIED.);
#1019=B_SPLINE_CURVE_WITH_KNOTS('',3,(#40272,#40273,#40274,#40275,#40276,
#40277,#40278,#40279,#40280,#40281,#40282,#40283,#40284,#40285,#40286,#40287,
#40288,#40289,#40290,#40291,#40292,#40293,#40294,#40295,#40296,#40297,#40298,
#40299,#40300,#40301,#40302,#40303,#40304,#40305,#40306,#40307,#40308,#40309,
#40310,#40311,#40312,#40313,#40314,#40315,#40316,#40317,#40318,#40319,#40320,
#40321,#40322,#40323,#40324,#40325,#40326,#40327,#40328,#40329,#40330,#40331,
#40332,#40333,#40334,#40335,#40336,#40337,#40338,#40339,#40340,#40341,#40342,
#40343,#40344,#40345,#40346,#40347,#40348,#40349,#40350,#40351,#40352,#40353,
#40354,#40355,#40356,#40357,#40358,#40359,#40360,#40361,#40362,#40363,#40364,
#40365,#40366,#40367,#40368,#40369,#40370,#40371,#40372,#40373,#40374,#40375,
#40376,#40377),.UNSPECIFIED.,.F.,.F.,(4,3,3,3,3,3,3,3,3,3,3,3,3,3,3,3,3,
3,3,3,3,3,3,3,3,3,3,3,3,3,3,3,3,3,3,4),(0.,0.0441576970943254,0.088758491595093,
0.133154322886181,0.177017836347152,0.193697049021019,0.19965188566726,
0.243475277581627,0.250795014009384,0.294669452308725,0.338569619728244,
0.37767568962022,0.38721824859893,0.393275053464473,0.436458598855563,0.479377262352089,
0.494993899296151,0.538189921814499,0.562468636762688,0.572092716170009,
0.579226787127647,0.621711263641225,0.664154373258728,0.70594102510778,
0.732419641400012,0.748330061688134,0.757222465646011,0.763401818269173,
0.80529293424602,0.844615778238015,0.861173358979439,0.871344162504664,
0.912748133225373,0.953576775379504,0.962584310214001,0.972375876542313),
 .UNSPECIFIED.);
#1020=B_SPLINE_CURVE_WITH_KNOTS('',3,(#40383,#40384,#40385,#40386,#40387,
#40388,#40389,#40390,#40391,#40392,#40393,#40394,#40395,#40396,#40397,#40398,
#40399,#40400,#40401,#40402,#40403,#40404,#40405,#40406,#40407,#40408,#40409,
#40410,#40411,#40412,#40413,#40414,#40415,#40416,#40417,#40418,#40419,#40420,
#40421,#40422,#40423,#40424,#40425,#40426,#40427,#40428,#40429,#40430,#40431,
#40432,#40433,#40434,#40435,#40436,#40437,#40438,#40439,#40440,#40441,#40442,
#40443,#40444,#40445,#40446,#40447,#40448,#40449,#40450,#40451,#40452,#40453,
#40454,#40455,#40456,#40457,#40458,#40459,#40460,#40461,#40462,#40463,#40464,
#40465,#40466,#40467,#40468,#40469,#40470,#40471,#40472,#40473,#40474,#40475,
#40476,#40477,#40478,#40479,#40480,#40481,#40482,#40483,#40484,#40485),
 .UNSPECIFIED.,.F.,.F.,(4,3,3,3,3,3,3,3,3,3,3,3,3,3,3,3,3,3,3,3,3,3,3,3,
3,3,3,3,3,3,3,3,3,3,4),(-0.972375876542414,-0.931565253728255,-0.890231005347033,
-0.869571408761885,-0.861266125665987,-0.819404433385386,-0.781321836236662,
-0.759040374121689,-0.752934683192443,-0.743239239087938,-0.701695078724687,
-0.659497058703992,-0.617009387497169,-0.589480672868744,-0.57644702705794,
-0.5714452780933,-0.528325351620324,-0.506894528983471,-0.464054318866617,
-0.420876860304666,-0.401240281040809,-0.388666227231065,-0.383537192824514,
-0.339939758883143,-0.295998103578765,-0.263784226193809,-0.219954566467475,
-0.204809517925579,-0.197308554950036,-0.192241015625869,-0.147699202975487,
-0.103111401264591,-0.0585925831444644,-0.0140737650243382,0.),
 .UNSPECIFIED.);
#1021=B_SPLINE_CURVE_WITH_KNOTS('',3,(#40486,#40487,#40488,#40489,#40490,
#40491,#40492,#40493,#40494,#40495,#40496,#40497,#40498,#40499,#40500,#40501,
#40502,#40503,#40504,#40505,#40506,#40507,#40508,#40509,#40510,#40511,#40512,
#40513,#40514,#40515,#40516,#40517,#40518,#40519,#40520,#40521,#40522,#40523,
#40524,#40525,#40526,#40527,#40528,#40529,#40530,#40531,#40532,#40533,#40534,
#40535,#40536,#40537,#40538,#40539,#40540,#40541,#40542,#40543,#40544,#40545,
#40546,#40547,#40548,#40549,#40550,#40551,#40552,#40553,#40554,#40555,#40556,
#40557,#40558,#40559,#40560,#40561,#40562,#40563,#40564,#40565,#40566,#40567,
#40568,#40569,#40570,#40571,#40572,#40573,#40574,#40575,#40576,#40577,#40578,
#40579,#40580,#40581,#40582,#40583,#40584,#40585,#40586,#40587,#40588),
 .UNSPECIFIED.,.F.,.F.,(4,3,3,3,3,3,3,3,3,3,3,3,3,3,3,3,3,3,3,3,3,3,3,3,
3,3,3,3,3,3,3,3,3,3,4),(-0.97000658757332,-0.925493326456513,-0.880835987444213,
-0.86024842639854,-0.852333874766883,-0.808142692209155,-0.764580356539862,
-0.742334794451242,-0.733010188832428,-0.721018020870569,-0.677646574841948,
-0.633950360266973,-0.590648734368262,-0.562539792613221,-0.550153753024242,
-0.542978093928587,-0.50009796533363,-0.478212967348099,-0.435235450336473,
-0.392367497022972,-0.373572235159268,-0.361228651726056,-0.355614322341834,
-0.313378921971217,-0.271427075980555,-0.242005402113342,-0.199831951142943,
-0.186315085816715,-0.179649707786883,-0.174232916759018,-0.132703725702247,
-0.0912075908119877,-0.0504161836307489,-0.0125558726020182,0.),
 .UNSPECIFIED.);
#1022=B_SPLINE_CURVE_WITH_KNOTS('',3,(#40590,#40591,#40592,#40593,#40594,
#40595,#40596,#40597,#40598,#40599,#40600,#40601,#40602,#40603,#40604,#40605,
#40606),.UNSPECIFIED.,.F.,.F.,(4,1,1,1,1,1,1,1,1,1,1,1,1,1,4),(15.707963267949,
15.8363896981257,16.3335648026029,16.8307399070801,17.3279150115573,17.8250901160345,
18.3222652205117,18.8194403249889,19.3166154294662,19.8137905339434,20.3109656384206,
20.8081407428978,21.305315847375,21.8024909518522,21.9911485751286),
 .UNSPECIFIED.);
#1023=B_SPLINE_CURVE_WITH_KNOTS('',3,(#40607,#40608,#40609,#40610,#40611,
#40612,#40613,#40614,#40615,#40616,#40617,#40618,#40619,#40620,#40621,#40622,
#40623),.UNSPECIFIED.,.F.,.F.,(4,1,1,1,1,1,1,1,1,1,1,1,1,1,4),(15.707963267949,
15.8904695802126,16.3876446846898,16.884819789167,17.3819948936443,17.8791699981215,
18.3763451025987,18.8735202070759,19.3706953115531,19.8678704160303,20.3650455205075,
20.8622206249848,21.359395729462,21.8565708339392,21.9911485751286),
 .UNSPECIFIED.);
#1024=B_SPLINE_CURVE_WITH_KNOTS('',3,(#41916,#41917,#41918,#41919,#41920,
#41921,#41922,#41923,#41924,#41925,#41926,#41927,#41928,#41929,#41930,#41931,
#41932,#41933,#41934,#41935,#41936,#41937,#41938,#41939,#41940,#41941,#41942,
#41943,#41944,#41945,#41946,#41947,#41948,#41949,#41950,#41951,#41952,#41953,
#41954,#41955,#41956,#41957,#41958,#41959,#41960,#41961,#41962,#41963,#41964,
#41965,#41966,#41967,#41968,#41969,#41970,#41971,#41972,#41973,#41974,#41975,
#41976,#41977,#41978,#41979,#41980,#41981,#41982,#41983,#41984,#41985,#41986,
#41987,#41988,#41989,#41990,#41991,#41992,#41993,#41994,#41995,#41996,#41997,
#41998,#41999,#42000,#42001,#42002,#42003,#42004,#42005,#42006,#42007,#42008,
#42009,#42010,#42011,#42012,#42013,#42014,#42015,#42016,#42017,#42018,#42019,
#42020,#42021),.UNSPECIFIED.,.F.,.F.,(4,3,3,3,3,3,3,3,3,3,3,3,3,3,3,3,3,
3,3,3,3,3,3,3,3,3,3,3,3,3,3,3,3,3,3,4),(0.,0.0404156030320338,0.0815364170314856,
0.123099442202208,0.164471164259153,0.177417333177223,0.182894508577368,
0.225046885757466,0.229033692090525,0.270767557602402,0.312945697761686,
0.350924838148176,0.357993918766748,0.363846074008531,0.406502560546029,
0.449493818503337,0.464862259307647,0.507689818261392,0.532644888553053,
0.54674918267878,0.552366866895522,0.595682545020243,0.639338821245014,
0.682868010841828,0.707330380594682,0.725816624679753,0.736955855775304,
0.74358314378864,0.787317407834192,0.829479796072424,0.846856648451819,
0.854114186312316,0.898699022066203,0.94326334774114,0.955966960787121,
0.97000658757331),.UNSPECIFIED.);
#1025=B_SPLINE_CURVE_WITH_KNOTS('',3,(#42022,#42023,#42024,#42025,#42026,
#42027,#42028,#42029,#42030,#42031,#42032,#42033,#42034,#42035,#42036,#42037,
#42038,#42039,#42040,#42041,#42042,#42043,#42044,#42045,#42046,#42047,#42048,
#42049,#42050,#42051,#42052,#42053,#42054,#42055,#42056,#42057,#42058,#42059,
#42060,#42061,#42062,#42063,#42064),.UNSPECIFIED.,.F.,.F.,(4,3,3,3,3,3,
3,3,3,3,3,3,3,3,4),(-10.1321597128207,-9.94350208954429,-9.44632698506708,
-8.94915188058987,-8.45197677611265,-7.95480167163544,-7.45762656715822,
-6.96045146268101,-6.46327635820379,-5.96610125372657,-5.46892614924936,
-4.97175104477214,-4.47457594029493,-3.97740083581771,-3.848974405641),
 .UNSPECIFIED.);
#1026=B_SPLINE_CURVE_WITH_KNOTS('',3,(#43357,#43358,#43359,#43360,#43361,
#43362,#43363,#43364,#43365,#43366,#43367,#43368,#43369,#43370,#43371,#43372,
#43373,#43374,#43375,#43376,#43377,#43378,#43379,#43380,#43381,#43382,#43383,
#43384,#43385,#43386,#43387,#43388,#43389,#43390,#43391,#43392,#43393,#43394,
#43395,#43396),.UNSPECIFIED.,.F.,.F.,(4,3,3,3,3,3,3,3,3,3,3,3,3,4),(7.59220430834767,
7.95480167163543,8.45197677611264,8.94915188058986,9.44632698506707,9.94350208954429,
10.4406771940215,10.9378522984987,11.4350274029759,11.9322025074531,12.4293776119304,
12.9265527164076,13.4237278208848,13.8753896155273),.UNSPECIFIED.);
#1027=B_SPLINE_CURVE_WITH_KNOTS('',3,(#43397,#43398,#43399,#43400,#43401,
#43402,#43403,#43404,#43405,#43406,#43407,#43408,#43409,#43410,#43411,#43412,
#43413,#43414,#43415,#43416,#43417,#43418,#43419,#43420,#43421,#43422,#43423,
#43424,#43425,#43426,#43427,#43428,#43429,#43430,#43431,#43432,#43433,#43434,
#43435,#43436,#43437,#43438,#43439,#43440,#43441,#43442,#43443,#43444,#43445,
#43446,#43447,#43448,#43449,#43450,#43451,#43452,#43453,#43454,#43455,#43456,
#43457,#43458,#43459,#43460,#43461,#43462,#43463,#43464,#43465,#43466,#43467,
#43468,#43469,#43470,#43471,#43472,#43473,#43474,#43475,#43476,#43477,#43478,
#43479,#43480,#43481,#43482,#43483,#43484,#43485,#43486,#43487,#43488,#43489,
#43490,#43491,#43492,#43493,#43494,#43495,#43496,#43497,#43498,#43499,#43500,
#43501,#43502),.UNSPECIFIED.,.F.,.F.,(4,3,3,3,3,3,3,3,3,3,3,3,3,3,3,3,3,
3,3,3,3,3,3,3,3,3,3,3,3,3,3,3,3,3,3,4),(0.,0.044150773052086,0.0887487507111273,
0.133148741969068,0.177019043965151,0.193023436662248,0.199907412815446,
0.24373234733986,0.250033573379215,0.293906609053928,0.337808296166161,
0.376734021006827,0.385567082155686,0.391401994113249,0.434581851246655,
0.477513379513922,0.493511195528826,0.53671130462677,0.560905212030567,
0.574207000071321,0.579201605029167,0.62168463125547,0.664125603281933,
0.705919109414855,0.730262563857148,0.748325604460628,0.757394747707568,
0.762943677116111,0.804834492856293,0.843575066915537,0.859283154994003,
0.866889043776386,0.908311110283104,0.949189929713081,0.959796789093269,
0.972375876542504),.UNSPECIFIED.);
#1028=B_SPLINE_CURVE_WITH_KNOTS('',3,(#44037,#44038,#44039,#44040,#44041,
#44042,#44043,#44044,#44045,#44046),.UNSPECIFIED.,.F.,.F.,(4,3,3,4),(-4.09293042013065,
-3.97826971642971,-2.98370228732228,-2.06773127522702),.UNSPECIFIED.);
#1029=B_SPLINE_CURVE_WITH_KNOTS('',3,(#44049,#44050,#44051,#44052,#44053,
#44054,#44055,#44056,#44057,#44058),.UNSPECIFIED.,.F.,.F.,(4,3,3,4),(0.,
0.49759560509741,0.995191210194833,1.11639350868605),.UNSPECIFIED.);
#1030=B_SPLINE_CURVE_WITH_KNOTS('',3,(#44063,#44064,#44065,#44066,#44067,
#44068,#44069,#44070,#44071,#44072,#44073,#44074,#44075,#44076,#44077,#44078,
#44079,#44080,#44081,#44082,#44083,#44084),.UNSPECIFIED.,.F.,.F.,(4,3,3,
3,3,3,3,4),(-10.3761157273102,-9.94567429107427,-8.95110686196684,-7.95653943285942,
-6.96197200375199,-5.96740457464456,-4.97283714553713,-4.09293042013065),
 .UNSPECIFIED.);
#1031=B_SPLINE_CURVE_WITH_KNOTS('',3,(#44085,#44086,#44087,#44088,#44089,
#44090,#44091,#44092,#44093,#44094,#44095,#44096,#44097,#44098,#44099,#44100,
#44101,#44102,#44103,#44104,#44105,#44106),.UNSPECIFIED.,.F.,.F.,(4,3,3,
3,3,3,3,4),(1.11639350868605,1.99038242038966,2.98557363058448,3.9807648407793,
4.97595605097413,5.97114726116895,6.96633847136377,7.39957881586564),
 .UNSPECIFIED.);
#1032=B_SPLINE_CURVE_WITH_KNOTS('',3,(#44111,#44112,#44113,#44114,#44115,
#44116,#44117,#44118,#44119,#44120,#44121,#44122,#44123,#44124,#44125,#44126,
#44127,#44128,#44129,#44130,#44131,#44132),.UNSPECIFIED.,.F.,.F.,(4,3,3,
3,3,3,3,4),(-16.6593010344898,-15.9130788657188,-14.9185114366114,-13.923944007504,
-12.9293765783965,-11.9348091492891,-10.9402417201817,-10.3761157273102),
 .UNSPECIFIED.);
#1033=B_SPLINE_CURVE_WITH_KNOTS('',3,(#44133,#44134,#44135,#44136,#44137,
#44138,#44139,#44140,#44141,#44142,#44143,#44144,#44145,#44146,#44147,#44148,
#44149,#44150,#44151,#44152,#44153,#44154),.UNSPECIFIED.,.F.,.F.,(4,3,3,
3,3,3,3,4),(7.39957881586564,7.9615296815586,8.95672089175343,9.95191210194825,
10.9471033121431,11.9422945223379,12.9374857325327,13.6827641230452),
 .UNSPECIFIED.);
#1034=B_SPLINE_CURVE_WITH_KNOTS('',3,(#44159,#44160,#44161,#44162,#44163,
#44164,#44165,#44166,#44167,#44168,#44169,#44170,#44171,#44172,#44173,#44174,
#44175,#44176,#44177,#44178,#44179,#44180,#44181,#44182,#44183),
 .UNSPECIFIED.,.F.,.F.,(4,3,3,3,3,3,3,3,4),(-22.9424863416694,-22.8750508694708,
-21.8804834403634,-20.885916011256,-19.8913485821485,-18.8967811530411,
-17.9022137239337,-16.9076462948263,-16.6593010344898),.UNSPECIFIED.);
#1035=B_SPLINE_CURVE_WITH_KNOTS('',3,(#44184,#44185,#44186,#44187,#44188,
#44189,#44190,#44191,#44192,#44193,#44194,#44195,#44196,#44197,#44198,#44199,
#44200,#44201,#44202,#44203,#44204,#44205,#44206,#44207,#44208),
 .UNSPECIFIED.,.F.,.F.,(4,3,3,3,3,3,3,3,4),(13.6827641230452,13.9326769427276,
14.9278681529224,15.9230593631172,16.918250573312,17.9134417835069,18.9086329937017,
19.9038242038965,19.9659494302248),.UNSPECIFIED.);
#1036=B_SPLINE_CURVE_WITH_KNOTS('',3,(#44213,#44214,#44215,#44216,#44217,
#44218,#44219,#44220,#44221,#44222,#44223,#44224,#44225,#44226,#44227,#44228,
#44229,#44230,#44231,#44232,#44233,#44234),.UNSPECIFIED.,.F.,.F.,(4,3,3,
3,3,3,3,4),(-29.225671648849,-28.8424554441154,-27.847888015008,-26.8533205859005,
-25.8587531567931,-24.8641857276857,-23.8696182985782,-22.9424863416694),
 .UNSPECIFIED.);
#1037=B_SPLINE_CURVE_WITH_KNOTS('',3,(#44235,#44236,#44237,#44238,#44239,
#44240,#44241,#44242,#44243,#44244,#44245,#44246,#44247,#44248,#44249,#44250,
#44251,#44252,#44253,#44254,#44255,#44256),.UNSPECIFIED.,.F.,.F.,(4,3,3,
3,3,3,3,4),(19.9659494302248,20.8990154140913,21.8942066242861,22.889397834481,
23.8845890446758,24.8797802548706,25.8749714650654,26.2491347374044),
 .UNSPECIFIED.);
#1038=B_SPLINE_CURVE_WITH_KNOTS('',3,(#44261,#44262,#44263,#44264,#44265,
#44266,#44267,#44268,#44269,#44270,#44271,#44272,#44273,#44274,#44275,#44276,
#44277,#44278,#44279,#44280,#44281,#44282),.UNSPECIFIED.,.F.,.F.,(4,3,3,
3,3,3,3,4),(-35.5088569560286,-34.8098600187599,-33.8152925896525,-32.8207251605451,
-31.8261577314377,-30.8315903023302,-29.8370228732228,-29.225671648849),
 .UNSPECIFIED.);
#1039=B_SPLINE_CURVE_WITH_KNOTS('',3,(#44283,#44284,#44285,#44286,#44287,
#44288,#44289,#44290,#44291,#44292,#44293,#44294,#44295,#44296,#44297,#44298,
#44299,#44300,#44301,#44302,#44303,#44304),.UNSPECIFIED.,.F.,.F.,(4,3,3,
3,3,3,3,4),(26.2491347374044,26.8701626752603,27.8653538854551,28.8605450956499,
29.8557363058448,30.8509275160396,31.8461187262344,32.532320044584),
 .UNSPECIFIED.);
#1040=B_SPLINE_CURVE_WITH_KNOTS('',3,(#44309,#44310,#44311,#44312,#44313,
#44314,#44315,#44316,#44317,#44318,#44319,#44320,#44321,#44322,#44323,#44324,
#44325,#44326,#44327,#44328,#44329,#44330,#44331,#44332,#44333),
 .UNSPECIFIED.,.F.,.F.,(4,3,3,3,3,3,3,3,4),(-41.7920422632082,-41.7718320225119,
-40.7772645934045,-39.7826971642971,-38.7881297351896,-37.7935623060822,
-36.7989948769748,-35.8044274478674,-35.5088569560286),.UNSPECIFIED.);
#1041=B_SPLINE_CURVE_WITH_KNOTS('',3,(#44334,#44335,#44336,#44337,#44338,
#44339,#44340,#44341,#44342,#44343,#44344,#44345,#44346,#44347,#44348,#44349,
#44350,#44351,#44352,#44353,#44354,#44355,#44356,#44357,#44358),
 .UNSPECIFIED.,.F.,.F.,(4,3,3,3,3,3,3,3,4),(32.532320044584,32.8413099364292,
33.8365011466241,34.8316923568189,35.8268835670137,36.8220747772085,37.8172659874034,
38.8124571975982,38.8155053517636),.UNSPECIFIED.);
#1042=B_SPLINE_CURVE_WITH_KNOTS('',3,(#44363,#44364,#44365,#44366,#44367,
#44368,#44369,#44370,#44371,#44372,#44373,#44374,#44375,#44376,#44377,#44378,
#44379,#44380,#44381,#44382,#44383,#44384),.UNSPECIFIED.,.F.,.F.,(4,3,3,
3,3,3,3,4),(-48.0752275703878,-47.7392365971565,-46.7446691680491,-45.7501017389416,
-44.7555343098342,-43.7609668807268,-42.7663994516193,-41.7920422632082),
 .UNSPECIFIED.);
#1043=B_SPLINE_CURVE_WITH_KNOTS('',3,(#44385,#44386,#44387,#44388,#44389,
#44390,#44391,#44392,#44393,#44394,#44395,#44396,#44397,#44398,#44399,#44400,
#44401,#44402,#44403,#44404,#44405,#44406),.UNSPECIFIED.,.F.,.F.,(4,3,3,
3,3,3,3,4),(38.8155053517636,39.807648407793,40.8028396179878,41.7980308281826,
42.7932220383775,43.7884132485723,44.7836044587671,45.0986906589432),
 .UNSPECIFIED.);
#1044=B_SPLINE_CURVE_WITH_KNOTS('',3,(#44411,#44412,#44413,#44414,#44415,
#44416,#44417,#44418,#44419,#44420,#44421,#44422,#44423,#44424,#44425,#44426,
#44427,#44428,#44429,#44430,#44431,#44432),.UNSPECIFIED.,.F.,.F.,(4,3,3,
3,3,3,3,4),(-54.3584128775674,-53.7066411718011,-52.7120737426936,-51.7175063135862,
-50.7229388844788,-49.7283714553713,-48.7338040262639,-48.0752275703878),
 .UNSPECIFIED.);
#1045=B_SPLINE_CURVE_WITH_KNOTS('',3,(#44433,#44434,#44435,#44436,#44437,
#44438,#44439,#44440,#44441,#44442,#44443,#44444,#44445,#44446,#44447,#44448,
#44449,#44450,#44451,#44452,#44453,#44454),.UNSPECIFIED.,.F.,.F.,(4,3,3,
3,3,3,3,4),(45.0986906589432,45.7787956689619,46.7739868791568,47.7691780893516,
48.7643692995464,49.7595605097412,50.7547517199361,51.3818759661228),
 .UNSPECIFIED.);
#1046=B_SPLINE_CURVE_WITH_KNOTS('',3,(#44459,#44460,#44461,#44462,#44463,
#44464,#44465,#44466,#44467,#44468,#44469,#44470,#44471,#44472,#44473,#44474,
#44475,#44476,#44477,#44478,#44479,#44480),.UNSPECIFIED.,.F.,.F.,(4,3,3,
3,3,3,3,4),(-60.641598184747,-59.6740457464456,-58.6794783173382,-57.6849108882308,
-56.6903434591233,-55.6957760300159,-54.7012086009085,-54.3584128775674),
 .UNSPECIFIED.);
#1047=B_SPLINE_CURVE_WITH_KNOTS('',3,(#44481,#44482,#44483,#44484,#44485,
#44486,#44487,#44488,#44489,#44490,#44491,#44492,#44493,#44494,#44495,#44496,
#44497,#44498,#44499,#44500,#44501,#44502),.UNSPECIFIED.,.F.,.F.,(4,3,3,
3,3,3,3,4),(51.3818759661228,51.7499429301309,52.7451341403257,53.7403253505205,
54.7355165607154,55.7307077709102,56.725898981105,57.6650612733024),
 .UNSPECIFIED.);
#1048=B_SPLINE_CURVE_WITH_KNOTS('',3,(#44507,#44508,#44509,#44510,#44511,
#44512,#44513,#44514,#44515,#44516,#44517,#44518,#44519,#44520,#44521,#44522,
#44523,#44524,#44525,#44526,#44527,#44528,#44529,#44530,#44531),
 .UNSPECIFIED.,.F.,.F.,(4,3,3,3,3,3,3,3,4),(-66.9247834919265,-66.6360177501976,
-65.6414503210902,-64.6468828919827,-63.6523154628753,-62.6577480337679,
-61.6631806046605,-60.668613175553,-60.641598184747),.UNSPECIFIED.);
#1049=B_SPLINE_CURVE_WITH_KNOTS('',3,(#44532,#44533,#44534,#44535,#44536,
#44537,#44538,#44539,#44540,#44541,#44542,#44543,#44544,#44545,#44546,#44547,
#44548,#44549,#44550,#44551,#44552,#44553,#44554,#44555,#44556),
 .UNSPECIFIED.,.F.,.F.,(4,3,3,3,3,3,3,3,4),(57.6650612733024,57.7210901912998,
58.7162814014946,59.7114726116895,60.7066638218843,61.7018550320791,62.697046242274,
63.6922374524688,63.9482465804819),.UNSPECIFIED.);
#1050=B_SPLINE_CURVE_WITH_KNOTS('',3,(#44561,#44562,#44563,#44564,#44565,
#44566,#44567,#44568,#44569,#44570,#44571,#44572,#44573,#44574,#44575,#44576,
#44577,#44578,#44579,#44580,#44581,#44582),.UNSPECIFIED.,.F.,.F.,(4,3,3,
3,3,3,3,4),(-73.2079687991061,-72.6034223248422,-71.6088548957347,-70.6142874666273,
-69.6197200375199,-68.6251526084124,-67.630585179305,-66.9247834919265),
 .UNSPECIFIED.);
#1051=B_SPLINE_CURVE_WITH_KNOTS('',3,(#44583,#44584,#44585,#44586,#44587,
#44588,#44589,#44590,#44591,#44592,#44593,#44594,#44595,#44596,#44597,#44598,
#44599,#44600,#44601,#44602,#44603,#44604),.UNSPECIFIED.,.F.,.F.,(4,3,3,
3,3,3,3,4),(63.9482465804819,64.6874286626636,65.6826198728584,66.6778110830533,
67.6730022932481,68.6681935034429,69.6633847136378,70.2314318876615),
 .UNSPECIFIED.);
#1052=B_SPLINE_CURVE_WITH_KNOTS('',3,(#44609,#44610,#44611,#44612,#44613,
#44614,#44615,#44616,#44617,#44618,#44619,#44620,#44621,#44622,#44623,#44624,
#44625,#44626,#44627,#44628,#44629,#44630),.UNSPECIFIED.,.F.,.F.,(4,3,3,
3,3,3,3,4),(-79.4911541062857,-78.5708268994867,-77.5762594703793,-76.5816920412719,
-75.5871246121644,-74.592557183057,-73.5979897539496,-73.2079687991061),
 .UNSPECIFIED.);
#1053=B_SPLINE_CURVE_WITH_KNOTS('',3,(#44631,#44632,#44633,#44634,#44635,
#44636,#44637,#44638,#44639,#44640,#44641,#44642,#44643,#44644,#44645,#44646,
#44647,#44648,#44649,#44650,#44651,#44652),.UNSPECIFIED.,.F.,.F.,(4,3,3,
3,3,3,3,4),(70.2314318876615,70.6585759238326,71.6537671340274,72.6489583442222,
73.644149554417,74.6393407646119,75.6345319748067,76.5146171948411),
 .UNSPECIFIED.);
#1054=B_SPLINE_CURVE_WITH_KNOTS('',3,(#44657,#44658,#44659,#44660,#44661,
#44662,#44663,#44664,#44665,#44666,#44667,#44668,#44669,#44670,#44671,#44672,
#44673,#44674,#44675,#44676,#44677,#44678,#44679,#44680,#44681),
 .UNSPECIFIED.,.F.,.F.,(4,3,3,3,3,3,3,3,4),(-85.7743394134653,-85.5327989032387,
-84.5382314741313,-83.5436640450238,-82.5490966159164,-81.554529186809,
-80.5599617577016,-79.5653943285942,-79.4911541062857),.UNSPECIFIED.);
#1055=B_SPLINE_CURVE_WITH_KNOTS('',3,(#44682,#44683,#44684,#44685,#44686,
#44687,#44688,#44689,#44690,#44691,#44692,#44693,#44694,#44695,#44696,#44697,
#44698,#44699,#44700,#44701,#44702,#44703,#44704,#44705,#44706),
 .UNSPECIFIED.,.F.,.F.,(4,3,3,3,3,3,3,3,4),(76.5146171948411,76.6297231850015,
77.6249143951963,78.6201056053912,79.615296815586,80.6104880257808,81.6056792359756,
82.6008704461705,82.7978025020207),.UNSPECIFIED.);
#1056=B_SPLINE_CURVE_WITH_KNOTS('',3,(#44711,#44712,#44713,#44714,#44715,
#44716,#44717,#44718,#44719,#44720,#44721,#44722,#44723,#44724,#44725,#44726,
#44727,#44728,#44729,#44730,#44731,#44732),.UNSPECIFIED.,.F.,.F.,(4,3,3,
3,3,3,3,4),(-92.0575247206449,-91.5002034778833,-90.5056360487758,-89.5110686196684,
-88.516501190561,-87.5219337614536,-86.5273663323461,-85.7743394134653),
 .UNSPECIFIED.);
#1057=B_SPLINE_CURVE_WITH_KNOTS('',3,(#44733,#44734,#44735,#44736,#44737,
#44738,#44739,#44740,#44741,#44742,#44743,#44744,#44745,#44746,#44747,#44748,
#44749,#44750,#44751,#44752,#44753,#44754),.UNSPECIFIED.,.F.,.F.,(4,3,3,
3,3,3,3,4),(82.7978025020207,83.5960616563653,84.5912528665601,85.5864440767549,
86.5816352869498,87.5768264971446,88.5720177073394,89.0809878092003),
 .UNSPECIFIED.);
#1058=B_SPLINE_CURVE_WITH_KNOTS('',3,(#44759,#44760,#44761,#44762,#44763,
#44764,#44765,#44766,#44767,#44768,#44769,#44770,#44771,#44772,#44773,#44774,
#44775,#44776,#44777,#44778,#44779,#44780),.UNSPECIFIED.,.F.,.F.,(4,3,3,
3,3,3,3,4),(-98.3407100278245,-97.4676080525278,-96.4730406234204,-95.478473194313,
-94.4839057652055,-93.4893383360981,-92.4947709069907,-92.0575247206449),
 .UNSPECIFIED.);
#1059=B_SPLINE_CURVE_WITH_KNOTS('',3,(#44781,#44782,#44783,#44784,#44785,
#44786,#44787,#44788,#44789,#44790,#44791,#44792,#44793,#44794,#44795,#44796,
#44797,#44798,#44799,#44800,#44801,#44802),.UNSPECIFIED.,.F.,.F.,(4,3,3,
3,3,3,3,4),(89.0809878092003,89.5672089175342,90.5624001277291,91.5575913379239,
92.5527825481187,93.5479737583135,94.5431649685084,95.3641731163799),
 .UNSPECIFIED.);
#1060=B_SPLINE_CURVE_WITH_KNOTS('',3,(#44807,#44808,#44809,#44810,#44811,
#44812,#44813,#44814,#44815,#44816,#44817,#44818,#44819,#44820,#44821,#44822,
#44823,#44824,#44825,#44826,#44827,#44828,#44829,#44830,#44831),
 .UNSPECIFIED.,.F.,.F.,(4,3,3,3,3,3,3,3,4),(-104.623895335004,-104.42958005628,
-103.435012627172,-102.440445198065,-101.445877768958,-100.45131033985,
-99.4567429107427,-98.4621754816353,-98.3407100278245),.UNSPECIFIED.);
#1061=B_SPLINE_CURVE_WITH_KNOTS('',3,(#44832,#44833,#44834,#44835,#44836,
#44837,#44838,#44839,#44840,#44841,#44842,#44843,#44844,#44845,#44846,#44847,
#44848,#44849,#44850,#44851,#44852,#44853,#44854,#44855,#44856),
 .UNSPECIFIED.,.F.,.F.,(4,3,3,3,3,3,3,3,4),(95.3641731163799,95.5383561787032,
96.533547388898,97.5287385990929,98.5239298092877,99.5191210194825,100.514312229677,
101.509503439872,101.64735842356),.UNSPECIFIED.);
#1062=B_SPLINE_CURVE_WITH_KNOTS('',3,(#44861,#44862,#44863,#44864,#44865,
#44866,#44867,#44868,#44869,#44870,#44871,#44872,#44873,#44874,#44875,#44876,
#44877,#44878,#44879,#44880,#44881,#44882),.UNSPECIFIED.,.F.,.F.,(4,3,3,
3,3,3,3,4),(-110.907080642184,-110.396984630924,-109.402417201817,-108.40784977271,
-107.413282343602,-106.418714914495,-105.424147485387,-104.623895335004),
 .UNSPECIFIED.);
#1063=B_SPLINE_CURVE_WITH_KNOTS('',3,(#44883,#44884,#44885,#44886,#44887,
#44888,#44889,#44890,#44891,#44892,#44893,#44894,#44895,#44896,#44897,#44898,
#44899,#44900,#44901,#44902,#44903,#44904),.UNSPECIFIED.,.F.,.F.,(4,3,3,
3,3,3,3,4),(101.64735842356,102.504694650067,103.499885860262,104.495077070457,
105.490268280651,106.485459490846,107.480650701041,107.930543730739),
 .UNSPECIFIED.);
#1064=B_SPLINE_CURVE_WITH_KNOTS('',3,(#44909,#44910,#44911,#44912,#44913,
#44914,#44915,#44916,#44917,#44918,#44919,#44920,#44921,#44922,#44923,#44924,
#44925,#44926,#44927,#44928,#44929,#44930),.UNSPECIFIED.,.F.,.F.,(4,3,3,
3,3,3,3,4),(-117.190265949363,-116.364389205569,-115.369821776462,-114.375254347354,
-113.380686918247,-112.386119489139,-111.391552060032,-110.907080642184),
 .UNSPECIFIED.);
#1065=B_SPLINE_CURVE_WITH_KNOTS('',3,(#44931,#44932,#44933,#44934,#44935,
#44936,#44937,#44938,#44939,#44940,#44941,#44942,#44943,#44944,#44945,#44946,
#44947,#44948,#44949,#44950,#44951,#44952),.UNSPECIFIED.,.F.,.F.,(4,3,3,
3,3,3,3,4),(107.930543730739,108.475841911236,109.471033121431,110.466224331626,
111.46141554182,112.456606752015,113.45179796221,114.213729037919),
 .UNSPECIFIED.);
#1066=B_SPLINE_CURVE_WITH_KNOTS('',3,(#44958,#44959,#44960,#44961,#44962,
#44963,#44964,#44965,#44966,#44967,#44968),.UNSPECIFIED.,.F.,.F.,(4,1,1,
1,1,1,1,1,4),(128.805298797182,128.973989482495,129.968556911602,130.963124340709,
131.957691769817,132.952259198924,133.946826628032,134.444110342585,134.941394057139),
 .UNSPECIFIED.);
#1067=B_SPLINE_CURVE_WITH_KNOTS('',3,(#44971,#44972,#44973,#44974,#44975,
#44976,#44977,#44978,#44979),.UNSPECIFIED.,.F.,.F.,(4,1,1,1,1,1,4),(128.805298797182,
129.721712095852,130.716903306047,131.712094516241,132.707285726436,133.204881331534,
133.702476936631),.UNSPECIFIED.);
#1068=B_SPLINE_CURVE_WITH_KNOTS('',3,(#44984,#44985,#44986,#44987,#44988,
#44989,#44990,#44991,#44992,#44993),.UNSPECIFIED.,.F.,.F.,(4,1,1,1,1,1,
1,4),(122.522113490002,123.00658490785,124.001152336957,124.995719766065,
125.990287195172,126.98485462428,127.979422053387,128.805298797182),
 .UNSPECIFIED.);
#1069=B_SPLINE_CURVE_WITH_KNOTS('',3,(#44994,#44995,#44996,#44997,#44998,
#44999,#45000,#45001,#45002,#45003,#45004),.UNSPECIFIED.,.F.,.F.,(4,1,1,
1,1,1,1,1,4),(122.522113490002,122.755373624488,123.750564834683,124.745756044878,
125.740947255072,126.736138465267,127.731329675462,128.726520885657,128.805298797182),
 .UNSPECIFIED.);
#1070=B_SPLINE_CURVE_WITH_KNOTS('',3,(#45009,#45010,#45011,#45012,#45013,
#45014,#45015,#45016,#45017,#45018),.UNSPECIFIED.,.F.,.F.,(4,1,1,1,1,1,
1,4),(116.238928182822,117.039180333205,118.033747762313,119.02831519142,
120.022882620528,121.017450049635,122.012017478743,122.522113490002),
 .UNSPECIFIED.);
#1071=B_SPLINE_CURVE_WITH_KNOTS('',3,(#45019,#45020,#45021,#45022,#45023,
#45024,#45025,#45026,#45027,#45028),.UNSPECIFIED.,.F.,.F.,(4,1,1,1,1,1,
1,4),(116.238928182822,116.784226363319,117.779417573514,118.774608783709,
119.769799993904,120.764991204098,121.760182414293,122.522113490002),
 .UNSPECIFIED.);
#1072=B_SPLINE_CURVE_WITH_KNOTS('',3,(#45033,#45034,#45035,#45036,#45037,
#45038,#45039,#45040,#45041,#45042,#45043),.UNSPECIFIED.,.F.,.F.,(4,1,1,
1,1,1,1,1,4),(109.955742875643,110.077208329453,111.071775758561,112.066343187668,
113.060910616776,114.055478045883,115.050045474991,116.044612904098,116.238928182822),
 .UNSPECIFIED.);
#1073=B_SPLINE_CURVE_WITH_KNOTS('',3,(#45044,#45045,#45046,#45047,#45048,
#45049,#45050,#45051,#45052,#45053),.UNSPECIFIED.,.F.,.F.,(4,1,1,1,1,1,
1,4),(109.955742875643,110.81307910215,111.808270312345,112.80346152254,
113.798652732735,114.793843942929,115.789035153124,116.238928182822),
 .UNSPECIFIED.);
#1074=B_SPLINE_CURVE_WITH_KNOTS('',3,(#45058,#45059,#45060,#45061,#45062,
#45063,#45064,#45065,#45066,#45067),.UNSPECIFIED.,.F.,.F.,(4,1,1,1,1,1,
1,4),(103.672557568463,104.109803754809,105.104371183916,106.098938613024,
107.093506042131,108.088073471239,109.082640900346,109.955742875643),
 .UNSPECIFIED.);
#1075=B_SPLINE_CURVE_WITH_KNOTS('',3,(#45068,#45069,#45070,#45071,#45072,
#45073,#45074,#45075,#45076,#45077,#45078),.UNSPECIFIED.,.F.,.F.,(4,1,1,
1,1,1,1,1,4),(103.672557568463,103.846740630786,104.841931840981,105.837123051176,
106.832314261371,107.827505471566,108.82269668176,109.817887891955,109.955742875643),
 .UNSPECIFIED.);
#1076=B_SPLINE_CURVE_WITH_KNOTS('',3,(#45083,#45084,#45085,#45086,#45087,
#45088,#45089,#45090,#45091,#45092),.UNSPECIFIED.,.F.,.F.,(4,1,1,1,1,1,
1,4),(97.3893722612836,98.1423991801644,99.1369666092718,100.131534038379,
101.126101467487,102.120668896594,103.115236325701,103.672557568463),
 .UNSPECIFIED.);
#1077=B_SPLINE_CURVE_WITH_KNOTS('',3,(#45093,#45094,#45095,#45096,#45097,
#45098,#45099,#45100,#45101,#45102),.UNSPECIFIED.,.F.,.F.,(4,1,1,1,1,1,
1,4),(97.3893722612835,97.8755933696174,98.8707845798122,99.865975790007,
100.861167000202,101.856358210397,102.851549420591,103.672557568463),
 .UNSPECIFIED.);
#1078=B_SPLINE_CURVE_WITH_KNOTS('',3,(#45107,#45108,#45109,#45110,#45111,
#45112,#45113,#45114,#45115,#45116,#45117),.UNSPECIFIED.,.F.,.F.,(4,1,1,
1,1,1,1,1,4),(91.106186954104,91.1804271764124,92.1749946055198,93.1695620346272,
94.1641294637347,95.1586968928421,96.1532643219495,97.1478317510569,97.3893722612836),
 .UNSPECIFIED.);
#1079=B_SPLINE_CURVE_WITH_KNOTS('',3,(#45118,#45119,#45120,#45121,#45122,
#45123,#45124,#45125,#45126,#45127),.UNSPECIFIED.,.F.,.F.,(4,1,1,1,1,1,
1,4),(91.106186954104,91.9044461084484,92.8996373186432,93.8948285288381,
94.8900197390329,95.8852109492277,96.8804021594225,97.3893722612835),
 .UNSPECIFIED.);
#1080=B_SPLINE_CURVE_WITH_KNOTS('',3,(#45132,#45133,#45134,#45135,#45136,
#45137,#45138,#45139,#45140,#45141),.UNSPECIFIED.,.F.,.F.,(4,1,1,1,1,1,
1,4),(84.8230016469244,85.2130226017678,86.2075900308752,87.2021574599827,
88.1967248890901,89.1912923181975,90.1858597473049,91.106186954104),
 .UNSPECIFIED.);
#1081=B_SPLINE_CURVE_WITH_KNOTS('',3,(#45142,#45143,#45144,#45145,#45146,
#45147,#45148,#45149,#45150,#45151,#45152),.UNSPECIFIED.,.F.,.F.,(4,1,1,
1,1,1,1,1,4),(84.8230016469244,84.9381076370846,85.9332988472795,86.9284900574743,
87.9236812676691,88.9188724778639,89.9140636880588,90.9092548982536,91.106186954104),
 .UNSPECIFIED.);
#1082=B_SPLINE_CURVE_WITH_KNOTS('',3,(#45157,#45158,#45159,#45160,#45161,
#45162,#45163,#45164,#45165,#45166),.UNSPECIFIED.,.F.,.F.,(4,1,1,1,1,1,
1,4),(78.5398163397448,79.2456180271232,80.2401854562307,81.2347528853381,
82.2293203144455,83.223887743553,84.2184551726604,84.8230016469244),
 .UNSPECIFIED.);
#1083=B_SPLINE_CURVE_WITH_KNOTS('',3,(#45167,#45168,#45169,#45170,#45171,
#45172,#45173,#45174,#45175,#45176),.UNSPECIFIED.,.F.,.F.,(4,1,1,1,1,1,
1,4),(78.5398163397448,78.9669603759157,79.9621515861105,80.9573427963053,
81.9525340065002,82.947725216695,83.9429164268898,84.8230016469244),
 .UNSPECIFIED.);
#1084=B_SPLINE_CURVE_WITH_KNOTS('',3,(#45181,#45182,#45183,#45184,#45185,
#45186,#45187,#45188,#45189,#45190,#45191),.UNSPECIFIED.,.F.,.F.,(4,1,1,
1,1,1,1,1,4),(72.2566310325652,72.2836460233713,73.2782134524787,74.2727808815861,
75.2673483106935,76.261915739801,77.2564831689084,78.2510505980158,78.5398163397448),
 .UNSPECIFIED.);
#1085=B_SPLINE_CURVE_WITH_KNOTS('',3,(#45192,#45193,#45194,#45195,#45196,
#45197,#45198,#45199,#45200,#45201),.UNSPECIFIED.,.F.,.F.,(4,1,1,1,1,1,
1,4),(72.2566310325652,72.9958131147467,73.9910043249416,74.9861955351364,
75.9813867453312,76.976577955526,77.9717691657209,78.5398163397448),
 .UNSPECIFIED.);
#1086=B_SPLINE_CURVE_WITH_KNOTS('',3,(#45206,#45207,#45208,#45209,#45210,
#45211,#45212,#45213,#45214,#45215),.UNSPECIFIED.,.F.,.F.,(4,1,1,1,1,1,
1,4),(65.9734457253856,66.3162414487267,67.3108088778341,68.3053763069416,
69.299943736049,70.2945111651564,71.2890785942638,72.2566310325652),
 .UNSPECIFIED.);
#1087=B_SPLINE_CURVE_WITH_KNOTS('',3,(#45216,#45217,#45218,#45219,#45220,
#45221,#45222,#45223,#45224,#45225,#45226),.UNSPECIFIED.,.F.,.F.,(4,1,1,
1,1,1,1,1,4),(65.9734457253856,66.029474643383,67.0246658535778,68.0198570637726,
69.0150482739674,70.0102394841623,71.0054306943571,72.0006219045519,72.2566310325652),
 .UNSPECIFIED.);
#1088=B_SPLINE_CURVE_WITH_KNOTS('',3,(#45231,#45232,#45233,#45234,#45235,
#45236,#45237,#45238,#45239,#45240),.UNSPECIFIED.,.F.,.F.,(4,1,1,1,1,1,
1,4),(59.690260418206,60.3488368740821,61.3434043031896,62.337971732297,
63.3325391614044,64.3271065905118,65.3216740196193,65.9734457253856),
 .UNSPECIFIED.);
#1089=B_SPLINE_CURVE_WITH_KNOTS('',3,(#45241,#45242,#45243,#45244,#45245,
#45246,#45247,#45248,#45249,#45250),.UNSPECIFIED.,.F.,.F.,(4,1,1,1,1,1,
1,4),(59.690260418206,60.058327382214,61.0535185924088,62.0487098026037,
63.0439010127985,64.0390922229933,65.0342834331881,65.9734457253856),
 .UNSPECIFIED.);
#1090=B_SPLINE_CURVE_WITH_KNOTS('',3,(#45255,#45256,#45257,#45258,#45259,
#45260,#45261,#45262,#45263,#45264),.UNSPECIFIED.,.F.,.F.,(4,1,1,1,1,1,
1,4),(53.4070751110264,54.3814322994376,55.375999728545,56.3705671576524,
57.3651345867599,58.3597020158673,59.3542694449747,59.690260418206),
 .UNSPECIFIED.);
#1091=B_SPLINE_CURVE_WITH_KNOTS('',3,(#45265,#45266,#45267,#45268,#45269,
#45270,#45271,#45272,#45273,#45274),.UNSPECIFIED.,.F.,.F.,(4,1,1,1,1,1,
1,4),(53.4070751110264,54.0871801210451,55.0823713312399,56.0775625414347,
57.0727537516295,58.0679449618244,59.0631361720192,59.690260418206),
 .UNSPECIFIED.);
#1092=B_SPLINE_CURVE_WITH_KNOTS('',3,(#45279,#45280,#45281,#45282,#45283,
#45284,#45285,#45286,#45287,#45288,#45289),.UNSPECIFIED.,.F.,.F.,(4,1,1,
1,1,1,1,1,4),(47.1238898038468,47.4194602956856,48.414027724793,49.4085951539004,
50.4031625830079,51.3977300121153,52.3922974412227,53.3868648703302,53.4070751110264),
 .UNSPECIFIED.);
#1093=B_SPLINE_CURVE_WITH_KNOTS('',3,(#45290,#45291,#45292,#45293,#45294,
#45295,#45296,#45297,#45298,#45299),.UNSPECIFIED.,.F.,.F.,(4,1,1,1,1,1,
1,4),(47.1238898038468,48.1160328598761,49.1112240700709,50.1064152802658,
51.1016064904606,52.0967977006554,53.0919889108502,53.4070751110264),
 .UNSPECIFIED.);
#1094=B_SPLINE_CURVE_WITH_KNOTS('',3,(#45304,#45305,#45306,#45307,#45308,
#45309,#45310,#45311,#45312,#45313),.UNSPECIFIED.,.F.,.F.,(4,1,1,1,1,1,
1,4),(40.8407044966672,41.452055721041,42.4466231501485,43.4411905792559,
44.4357580083633,45.4303254374707,46.4248928665782,47.1238898038468),
 .UNSPECIFIED.);
#1095=B_SPLINE_CURVE_WITH_KNOTS('',3,(#45314,#45315,#45316,#45317,#45318,
#45319,#45320,#45321,#45322,#45323,#45324),.UNSPECIFIED.,.F.,.F.,(4,1,1,
1,1,1,1,1,4),(40.8407044966672,41.1496943885123,42.1448855987072,43.140076808902,
44.1352680190968,45.1304592292916,46.1256504394865,47.1208416496813,47.1238898038468),
 .UNSPECIFIED.);
#1096=B_SPLINE_CURVE_WITH_KNOTS('',3,(#45329,#45330,#45331,#45332,#45333,
#45334,#45335,#45336,#45337,#45338),.UNSPECIFIED.,.F.,.F.,(4,1,1,1,1,1,
1,4),(34.5575191894876,35.4846511463965,36.4792185755039,37.4737860046113,
38.4683534337187,39.4629208628262,40.4574882919336,40.8407044966672),
 .UNSPECIFIED.);
#1097=B_SPLINE_CURVE_WITH_KNOTS('',3,(#45339,#45340,#45341,#45342,#45343,
#45344,#45345,#45346,#45347,#45348),.UNSPECIFIED.,.F.,.F.,(4,1,1,1,1,1,
1,4),(34.5575191894876,35.1785471273434,36.1737383375382,37.168929547733,
38.1641207579279,39.1593119681227,40.1545031783175,40.8407044966672),
 .UNSPECIFIED.);
#1098=B_SPLINE_CURVE_WITH_KNOTS('',3,(#45353,#45354,#45355,#45356,#45357,
#45358,#45359,#45360,#45361,#45362,#45363),.UNSPECIFIED.,.F.,.F.,(4,1,1,
1,1,1,1,1,4),(28.274333882308,28.5226791426445,29.5172465717519,30.5118140008593,
31.5063814299668,32.5009488590742,33.4955162881816,34.490083717289,34.5575191894876),
 .UNSPECIFIED.);
#1099=B_SPLINE_CURVE_WITH_KNOTS('',3,(#45364,#45365,#45366,#45367,#45368,
#45369,#45370,#45371,#45372,#45373),.UNSPECIFIED.,.F.,.F.,(4,1,1,1,1,1,
1,4),(28.274333882308,29.2073998661744,30.2025910763693,31.1977822865641,
32.1929734967589,33.1881647069537,34.1833559171486,34.5575191894876),
 .UNSPECIFIED.);
#1100=B_SPLINE_CURVE_WITH_KNOTS('',3,(#45378,#45379,#45380,#45381,#45382,
#45383,#45384,#45385,#45386,#45387),.UNSPECIFIED.,.F.,.F.,(4,1,1,1,1,1,
1,4),(21.9911485751285,22.5552745679999,23.5498419971074,24.5444094262148,
25.5389768553222,26.5335442844296,27.5281117135371,28.274333882308),
 .UNSPECIFIED.);
#1101=B_SPLINE_CURVE_WITH_KNOTS('',3,(#45388,#45389,#45390,#45391,#45392,
#45393,#45394,#45395,#45396,#45397,#45398),.UNSPECIFIED.,.F.,.F.,(4,1,1,
1,1,1,1,1,4),(21.9911485751285,22.2410613948107,23.2362526050055,24.2314438152003,
25.2266350253952,26.22182623559,27.2170174457848,28.2122086559796,28.274333882308),
 .UNSPECIFIED.);
#1102=B_SPLINE_CURVE_WITH_KNOTS('',3,(#45403,#45404,#45405,#45406,#45407,
#45408,#45409,#45410,#45411,#45412),.UNSPECIFIED.,.F.,.F.,(4,1,1,1,1,1,
1,4),(15.7079632679489,16.5878699933554,17.5824374224628,18.5770048515702,
19.5715722806776,20.5661397097851,21.5607071388925,21.9911485751285),
 .UNSPECIFIED.);
#1103=B_SPLINE_CURVE_WITH_KNOTS('',3,(#45413,#45414,#45415,#45416,#45417,
#45418,#45419,#45420,#45421,#45422),.UNSPECIFIED.,.F.,.F.,(4,1,1,1,1,1,
1,4),(15.7079632679489,16.2699141336417,17.2651053438366,18.2602965540314,
19.2554877642262,20.250678974421,21.2458701846159,21.9911485751285),
 .UNSPECIFIED.);
#1104=B_SPLINE_CURVE_WITH_KNOTS('',3,(#45425,#45426,#45427,#45428,#45429,
#45430,#45431,#45432,#45433,#45434,#45435,#45436,#45437,#45438,#45439,#45440,
#45441,#45442,#45443,#45444,#45445,#45446,#45447,#45448,#45449,#45450,#45451,
#45452,#45453,#45454,#45455,#45456,#45457,#45458,#45459,#45460,#45461,#45462,
#45463,#45464,#45465,#45466,#45467,#45468,#45469,#45470,#45471,#45472,#45473,
#45474,#45475,#45476,#45477,#45478,#45479,#45480,#45481,#45482,#45483,#45484,
#45485,#45486,#45487,#45488,#45489,#45490,#45491,#45492,#45493,#45494,#45495,
#45496,#45497,#45498,#45499,#45500,#45501,#45502,#45503,#45504,#45505,#45506,
#45507,#45508,#45509,#45510,#45511,#45512,#45513,#45514,#45515,#45516,#45517,
#45518,#45519,#45520,#45521,#45522,#45523,#45524,#45525,#45526,#45527,#45528,
#45529,#45530,#45531,#45532,#45533,#45534,#45535,#45536,#45537,#45538,#45539,
#45540,#45541,#45542,#45543,#45544,#45545,#45546,#45547,#45548,#45549,#45550,
#45551,#45552,#45553,#45554,#45555,#45556,#45557,#45558,#45559,#45560,#45561,
#45562,#45563,#45564,#45565,#45566,#45567,#45568,#45569,#45570,#45571,#45572,
#45573,#45574,#45575,#45576,#45577,#45578,#45579,#45580,#45581,#45582,#45583,
#45584,#45585,#45586,#45587,#45588,#45589,#45590,#45591,#45592,#45593,#45594,
#45595,#45596,#45597,#45598,#45599,#45600,#45601,#45602,#45603,#45604,#45605,
#45606,#45607,#45608,#45609,#45610,#45611,#45612,#45613,#45614,#45615,#45616,
#45617,#45618,#45619,#45620,#45621,#45622,#45623,#45624,#45625,#45626,#45627,
#45628,#45629,#45630,#45631,#45632,#45633,#45634,#45635,#45636,#45637,#45638,
#45639,#45640,#45641,#45642,#45643,#45644,#45645,#45646,#45647,#45648,#45649,
#45650,#45651,#45652,#45653,#45654,#45655,#45656,#45657,#45658,#45659,#45660,
#45661,#45662,#45663,#45664,#45665,#45666,#45667,#45668),.UNSPECIFIED.,
 .F.,.F.,(4,3,3,3,3,3,3,3,3,3,3,3,3,3,3,3,3,3,3,3,3,3,3,3,3,3,3,3,3,3,3,
3,3,3,3,3,3,3,3,3,3,3,3,3,3,3,3,3,3,3,3,3,3,3,3,3,3,3,3,3,3,3,3,3,3,3,3,
3,3,3,3,3,3,3,3,3,3,3,3,3,3,4),(-2.64334436896556,-2.60354403016607,-2.56319357704322,
-2.52826625024512,-2.51459318907079,-2.50781535649548,-2.46564981317316,
-2.42348426985084,-2.39566963603287,-2.38341570939638,-2.37761610684016,
-2.336849738158,-2.29583153162079,-2.25519438983726,-2.22808079457215,-2.2136427889914,
-2.20824896814423,-2.20096719930704,-2.16123852890373,-2.12054358173304,
-2.07915011465577,-2.03779648847865,-2.03243166702702,-1.99089005776529,
-1.94895701700167,-1.90713874879756,-1.86743433790788,-1.85926764668736,
-1.85203534200324,-1.80992713326301,-1.76842432689819,-1.74832110523882,
-1.70676763322338,-1.68046855645703,-1.67322668686903,-1.63229330306282,
-1.58900444080018,-1.54654889761395,-1.51397808603242,-1.5045713939363,
-1.49689579776549,-1.49148547399684,-1.44889513044297,-1.40637477884859,
-1.36441427917375,-1.32519834206773,-1.31745702219618,-1.31155026142285,
-1.28598240496172,-1.24479777214057,-1.20266268120784,-1.15989915790716,
-1.13825803467134,-1.13225377395059,-1.12622665290763,-1.08347961800304,
-1.04027268262164,-0.997123369249094,-0.954546729607404,-0.947141190072399,
-0.941377976925763,-0.897944447185484,-0.855190214624572,-0.813641186133967,
-0.785925562678236,-0.769826109785476,-0.761910560472749,-0.75632393840638,
-0.714342458530382,-0.67097419230323,-0.627232222714931,-0.595102096230848,
-0.581045165894062,-0.572765453161588,-0.566918945151293,-0.523130330920948,
-0.47917700856887,-0.435659870904986,-0.402925540873628,-0.383690774196495,
-0.377633521738216,-0.37019121084227),.UNSPECIFIED.);
#1105=B_SPLINE_CURVE_WITH_KNOTS('',3,(#45670,#45671,#45672,#45673,#45674,
#45675,#45676,#45677,#45678,#45679,#45680,#45681,#45682,#45683,#45684,#45685,
#45686,#45687,#45688,#45689,#45690,#45691,#45692,#45693,#45694,#45695,#45696,
#45697,#45698,#45699,#45700,#45701,#45702,#45703,#45704,#45705,#45706,#45707,
#45708,#45709,#45710,#45711,#45712,#45713,#45714,#45715,#45716,#45717,#45718,
#45719,#45720,#45721,#45722,#45723,#45724,#45725,#45726,#45727,#45728,#45729,
#45730,#45731,#45732,#45733,#45734,#45735,#45736,#45737,#45738,#45739,#45740,
#45741,#45742),.UNSPECIFIED.,.F.,.F.,(4,3,3,3,3,3,3,3,3,3,3,3,3,3,3,3,3,
3,3,3,3,3,3,3,4),(-0.710745924398683,-0.666804013499017,-0.623090002091155,
-0.580490043399667,-0.549769720878275,-0.540030794848239,-0.533787755766615,
-0.491609440904295,-0.4576087533141,-0.414988201685294,-0.372400295436586,
-0.356121723662545,-0.350309819512417,-0.308708315030754,-0.266458526938774,
-0.224208738846794,-0.196182646490945,-0.183254318429312,-0.17525918271343,
-0.169900496948286,-0.127425372711214,-0.0868708094010787,-0.0467252344004481,
-0.00739903503843566,0.),.UNSPECIFIED.);
#1106=B_SPLINE_CURVE_WITH_KNOTS('',3,(#45745,#45746,#45747,#45748,#45749,
#45750,#45751,#45752,#45753,#45754,#45755,#45756,#45757,#45758,#45759,#45760,
#45761,#45762,#45763,#45764,#45765,#45766,#45767,#45768,#45769,#45770,#45771,
#45772,#45773,#45774,#45775,#45776,#45777,#45778,#45779,#45780,#45781),
 .UNSPECIFIED.,.F.,.F.,(4,3,3,3,3,3,3,3,3,3,3,3,4),(-0.37019121084227,-0.331697325929431,
-0.288622232780515,-0.244797719637212,-0.21419800468256,-0.2008106293899,
-0.194172952745162,-0.188472403894731,-0.144967619206762,-0.100508059630889,
-0.0559598465844598,-0.0119678329618413,0.),.UNSPECIFIED.);
#1107=B_SPLINE_CURVE_WITH_KNOTS('',3,(#46302,#46303,#46304,#46305,#46306,
#46307,#46308,#46309,#46310),.UNSPECIFIED.,.F.,.F.,(4,1,1,1,1,1,4),(11.6150328478182,
12.1123165623719,12.6096002769257,13.6041677060331,14.5987351351405,15.5933025642479,
15.7079632679489),.UNSPECIFIED.);
#1108=B_SPLINE_CURVE_WITH_KNOTS('',3,(#46311,#46312,#46313,#46314,#46315,
#46316,#46317,#46318,#46319,#46320,#46321,#46322,#46323,#46324,#46325,#46326,
#46327,#46328,#46329,#46330,#46331,#46332,#46333,#46334,#46335,#46336,#46337,
#46338,#46339,#46340,#46341,#46342,#46343,#46344,#46345,#46346,#46347,#46348,
#46349,#46350,#46351,#46352,#46353,#46354,#46355,#46356,#46357,#46358,#46359,
#46360,#46361,#46362,#46363,#46364,#46365,#46366,#46367,#46368,#46369,#46370,
#46371,#46372,#46373,#46374,#46375,#46376,#46377,#46378,#46379,#46380,#46381,
#46382,#46383,#46384,#46385,#46386,#46387,#46388,#46389,#46390,#46391,#46392,
#46393,#46394,#46395,#46396,#46397,#46398,#46399,#46400,#46401,#46402,#46403,
#46404,#46405,#46406,#46407,#46408,#46409,#46410,#46411,#46412,#46413),
 .UNSPECIFIED.,.F.,.F.,(4,3,3,3,3,3,3,3,3,3,3,3,3,3,3,3,3,3,3,3,3,3,3,3,
3,3,3,3,3,3,3,3,3,3,4),(-0.965990216419481,-0.9272199902169,-0.883653696268922,
-0.856578499606751,-0.840281614965736,-0.83272424860471,-0.78942649842623,
-0.747054504832225,-0.728516757634848,-0.714850133126621,-0.708733859333935,
-0.665685633827477,-0.622719517527392,-0.579652275564091,-0.547351844091615,
-0.533932274491217,-0.525881927440116,-0.484249432147785,-0.450450549674188,
-0.408562082241703,-0.366597621077022,-0.351118396676314,-0.345479700399037,
-0.304353213451827,-0.263090931261655,-0.221828649071483,-0.194100067937547,
-0.181335497105944,-0.172973757166477,-0.167228677968348,-0.125421508476261,
-0.0849791978641806,-0.0449278087924871,-0.005690172937603,0.),
 .UNSPECIFIED.);
#1109=B_SPLINE_CURVE_WITH_KNOTS('',3,(#46414,#46415,#46416,#46417,#46418,
#46419,#46420,#46421,#46422,#46423,#46424,#46425,#46426,#46427,#46428,#46429,
#46430,#46431,#46432),.UNSPECIFIED.,.F.,.F.,(4,3,3,3,3,3,4),(-121.812676859456,
-121.337226351106,-120.342658921999,-119.348091492891,-118.353524063784,
-117.358956634676,-117.190265949363),.UNSPECIFIED.);
#1110=B_SPLINE_CURVE_WITH_KNOTS('',3,(#46435,#46436,#46437,#46438,#46439,
#46440,#46441,#46442,#46443),.UNSPECIFIED.,.F.,.F.,(4,1,1,1,1,1,4),(10.3761157273101,
11.2939580826676,12.2891492928624,13.2843405030573,14.2795317132521,15.2747229234469,
15.7079632679489),.UNSPECIFIED.);
#1111=B_SPLINE_CURVE_WITH_KNOTS('',3,(#46969,#46970,#46971,#46972,#46973,
#46974,#46975,#46976,#46977,#46978,#46979,#46980,#46981,#46982,#46983,#46984,
#46985,#46986,#46987,#46988,#46989,#46990),.UNSPECIFIED.,.F.,.F.,(4,3,3,
3,3,3,3,4),(114.213729037919,114.446989172405,115.4421803826,116.437371592795,
117.432562802989,118.427754013184,119.422945223379,119.744945584229),
 .UNSPECIFIED.);
#1112=B_SPLINE_CURVE_WITH_KNOTS('',3,(#46991,#46992,#46993,#46994,#46995,
#46996,#46997,#46998,#46999,#47000,#47001,#47002,#47003,#47004,#47005,#47006,
#47007,#47008,#47009,#47010,#47011,#47012,#47013,#47014,#47015,#47016,#47017,
#47018,#47019,#47020,#47021,#47022,#47023,#47024,#47025,#47026,#47027,#47028,
#47029,#47030,#47031,#47032,#47033,#47034,#47035,#47036,#47037,#47038,#47039,
#47040,#47041,#47042,#47043,#47044,#47045,#47046,#47047,#47048,#47049,#47050,
#47051,#47052,#47053,#47054,#47055,#47056,#47057,#47058,#47059,#47060,#47061,
#47062,#47063,#47064,#47065,#47066,#47067,#47068,#47069,#47070,#47071,#47072,
#47073,#47074,#47075,#47076,#47077,#47078,#47079,#47080,#47081,#47082,#47083,
#47084,#47085,#47086,#47087,#47088,#47089,#47090,#47091,#47092,#47093,#47094,
#47095,#47096),.UNSPECIFIED.,.F.,.F.,(4,3,3,3,3,3,3,3,3,3,3,3,3,3,3,3,3,
3,3,3,3,3,3,3,3,3,3,3,3,3,3,3,3,3,3,4),(-0.968477696161952,-0.934401878411372,
-0.894940908856935,-0.869057110968003,-0.857761995024893,-0.84957581141373,
-0.809420536841839,-0.768342987565862,-0.750371559757621,-0.741288256886726,
-0.734041921366352,-0.692568544969978,-0.650621991967233,-0.60816652963393,
-0.576324932883953,-0.562465720811907,-0.556565387998925,-0.513962262185476,
-0.480800142634022,-0.43927778705218,-0.397173024145668,-0.382659788254531,
-0.376822993230344,-0.334735665268914,-0.292008067784669,-0.248907378913767,
-0.243684959408641,-0.213224339482561,-0.199897818264901,-0.191569349313896,
-0.186008989480452,-0.142614739306227,-0.0987671132040068,-0.0550446346348842,
-0.0119839009752852,0.),.UNSPECIFIED.);
#1113=B_SPLINE_CURVE_WITH_KNOTS('',3,(#47159,#47160,#47161,#47162),
 .UNSPECIFIED.,.F.,.F.,(4,4),(51.5750455984138,52.2824273504651),
 .UNSPECIFIED.);
#1114=B_SPLINE_CURVE_WITH_KNOTS('',3,(#47170,#47171,#47172,#47173,#47174,
#47175,#47176,#47177,#47178,#47179),.UNSPECIFIED.,.F.,.F.,(4,3,3,4),(-50.2654824574367,
-49.3230446702501,-48.3365837768451,-47.8312715558982),.UNSPECIFIED.);
#1115=B_SPLINE_CURVE_WITH_KNOTS('',3,(#47184,#47185,#47186,#47187,#47188,
#47189,#47190,#47191,#47192,#47193,#47194,#47195,#47196,#47197,#47198,#47199,
#47200,#47201,#47202,#47203,#47204,#47205,#47206,#47207,#47208),
 .UNSPECIFIED.,.F.,.F.,(4,3,3,3,3,3,3,3,4),(45.2918602912342,45.3772010966301,
46.3636619900351,47.3501228834401,48.3365837768451,49.3230446702501,50.3095055636551,
51.2959664570601,51.5750455984138),.UNSPECIFIED.);
#1116=B_SPLINE_CURVE_WITH_KNOTS('',3,(#47209,#47210,#47211,#47212,#47213,
#47214,#47215,#47216,#47217,#47218,#47219,#47220,#47221,#47222,#47223,#47224,
#47225,#47226,#47227,#47228,#47229,#47230),.UNSPECIFIED.,.F.,.F.,(4,3,3,
3,3,3,3,4),(-47.8312715558982,-47.3501228834401,-46.3636619900351,-45.3772010966301,
-44.3907402032251,-43.4042793098201,-42.4178184164151,-41.5480862487186),
 .UNSPECIFIED.);
#1117=B_SPLINE_CURVE_WITH_KNOTS('',3,(#47235,#47236,#47237,#47238,#47239,
#47240,#47241,#47242,#47243,#47244,#47245,#47246,#47247,#47248,#47249,#47250,
#47251,#47252,#47253,#47254,#47255,#47256),.UNSPECIFIED.,.F.,.F.,(4,3,3,
3,3,3,3,4),(39.0086749840546,39.4584357362001,40.4448966296051,41.4313575230101,
42.4178184164151,43.4042793098201,44.3907402032251,45.2918602912342),
 .UNSPECIFIED.);
#1118=B_SPLINE_CURVE_WITH_KNOTS('',3,(#47257,#47258,#47259,#47260,#47261,
#47262,#47263,#47264,#47265,#47266,#47267,#47268,#47269,#47270,#47271,#47272,
#47273,#47274,#47275,#47276,#47277,#47278,#47279,#47280,#47281),
 .UNSPECIFIED.,.F.,.F.,(4,3,3,3,3,3,3,3,4),(-41.5480862487186,-41.4313575230101,
-40.4448966296051,-39.4584357362001,-38.4719748427951,-37.4855139493901,
-36.4990530559851,-35.5125921625801,-35.264900941539),.UNSPECIFIED.);
#1119=B_SPLINE_CURVE_WITH_KNOTS('',3,(#47286,#47287,#47288,#47289,#47290,
#47291,#47292,#47293,#47294,#47295,#47296,#47297,#47298,#47299,#47300,#47301,
#47302,#47303,#47304,#47305,#47306,#47307),.UNSPECIFIED.,.F.,.F.,(4,3,3,
3,3,3,3,4),(32.725489676875,33.5396703757701,34.5261312691751,35.5125921625801,
36.4990530559851,37.4855139493901,38.4719748427951,39.0086749840546),
 .UNSPECIFIED.);
#1120=B_SPLINE_CURVE_WITH_KNOTS('',3,(#47308,#47309,#47310,#47311,#47312,
#47313,#47314,#47315,#47316,#47317,#47318,#47319,#47320,#47321,#47322,#47323,
#47324,#47325,#47326,#47327,#47328,#47329),.UNSPECIFIED.,.F.,.F.,(4,3,3,
3,3,3,3,4),(-35.264900941539,-34.5261312691751,-33.5396703757701,-32.5532094823651,
-31.5667485889601,-30.5802876955551,-29.5938268021501,-28.9817156343595),
 .UNSPECIFIED.);
#1121=B_SPLINE_CURVE_WITH_KNOTS('',3,(#47334,#47335,#47336,#47337,#47338,
#47339,#47340,#47341,#47342,#47343,#47344,#47345,#47346,#47347,#47348,#47349,
#47350,#47351,#47352,#47353,#47354,#47355,#47356,#47357,#47358),
 .UNSPECIFIED.,.F.,.F.,(4,3,3,3,3,3,3,3,4),(26.4423043696954,26.6344441219351,
27.6209050153401,28.6073659087451,29.5938268021501,30.5802876955551,31.5667485889601,
32.5532094823651,32.725489676875),.UNSPECIFIED.);
#1122=B_SPLINE_CURVE_WITH_KNOTS('',3,(#47359,#47360,#47361,#47362,#47363,
#47364,#47365,#47366,#47367,#47368,#47369,#47370,#47371,#47372,#47373,#47374,
#47375,#47376,#47377,#47378,#47379,#47380),.UNSPECIFIED.,.F.,.F.,(4,3,3,
3,3,3,3,4),(-28.9817156343595,-28.6073659087451,-27.6209050153401,-26.6344441219351,
-25.6479832285301,-24.6615223351251,-23.6750614417201,-22.6985303271799),
 .UNSPECIFIED.);
#1123=B_SPLINE_CURVE_WITH_KNOTS('',3,(#47385,#47386,#47387,#47388,#47389,
#47390,#47391,#47392,#47393,#47394,#47395,#47396,#47397,#47398,#47399,#47400,
#47401,#47402,#47403,#47404,#47405,#47406),.UNSPECIFIED.,.F.,.F.,(4,3,3,
3,3,3,3,4),(20.1591190625158,20.7156787615051,21.7021396549101,22.6886005483151,
23.6750614417201,24.6615223351251,25.6479832285301,26.4423043696954),
 .UNSPECIFIED.);
#1124=B_SPLINE_CURVE_WITH_KNOTS('',3,(#47407,#47408,#47409,#47410,#47411,
#47412,#47413,#47414,#47415,#47416,#47417,#47418,#47419,#47420,#47421,#47422,
#47423,#47424,#47425,#47426,#47427,#47428,#47429,#47430,#47431),
 .UNSPECIFIED.,.F.,.F.,(4,3,3,3,3,3,3,3,4),(-22.6985303271799,-22.6886005483151,
-21.7021396549101,-20.7156787615051,-19.7292178681001,-18.7427569746951,
-17.75629608129,-16.769835187885,-16.4153450200003),.UNSPECIFIED.);
#1125=B_SPLINE_CURVE_WITH_KNOTS('',3,(#47436,#47437,#47438,#47439,#47440,
#47441,#47442,#47443,#47444,#47445,#47446,#47447,#47448,#47449,#47450,#47451,
#47452,#47453,#47454,#47455,#47456,#47457),.UNSPECIFIED.,.F.,.F.,(4,3,3,
3,3,3,3,4),(13.8759337553362,14.796913401075,15.78337429448,16.769835187885,
17.75629608129,18.7427569746951,19.7292178681001,20.1591190625158),
 .UNSPECIFIED.);
#1126=B_SPLINE_CURVE_WITH_KNOTS('',3,(#47458,#47459,#47460,#47461,#47462,
#47463,#47464,#47465,#47466,#47467,#47468,#47469,#47470,#47471,#47472,#47473,
#47474,#47475,#47476,#47477,#47478,#47479),.UNSPECIFIED.,.F.,.F.,(4,3,3,
3,3,3,3,4),(-16.4153450200003,-15.78337429448,-14.796913401075,-13.81045250767,
-12.823991614265,-11.83753072086,-10.851069827455,-10.1321597128207),
 .UNSPECIFIED.);
#1127=B_SPLINE_CURVE_WITH_KNOTS('',3,(#47485,#47486,#47487,#47488,#47489,
#47490,#47491,#47492,#47493,#47494,#47495,#47496,#47497),.UNSPECIFIED.,
 .F.,.F.,(4,3,3,3,4),(-3.84897440564112,-2.95938268021501,-1.97292178681001,
-0.986460893405003,0.),.UNSPECIFIED.);
#1128=B_SPLINE_CURVE_WITH_KNOTS('',3,(#47500,#47501,#47502,#47503,#47504,
#47505,#47506,#47507,#47508,#47509,#47510,#47511,#47512,#47513,#47514,#47515,
#47516,#47517,#47518),.UNSPECIFIED.,.F.,.F.,(4,3,3,3,3,3,4),(2.01694489302844,
2.95938268021501,3.94584357362001,4.93230446702501,5.91876536043001,6.90522625383502,
7.59274844815664),.UNSPECIFIED.);
#1129=B_SPLINE_CURVE_WITH_KNOTS('',3,(#47524,#47525,#47526,#47527,#47528,
#47529,#47530,#47531),.UNSPECIFIED.,.F.,.F.,(4,1,1,1,1,4),(59.6902604182061,
60.195572639153,61.182033532558,62.168494425963,63.154955319368,64.141416212773),
 .UNSPECIFIED.);
#1130=B_SPLINE_CURVE_WITH_KNOTS('',3,(#47534,#47535,#47536,#47537,#47538,
#47539,#47540,#47541,#47542),.UNSPECIFIED.,.F.,.F.,(4,1,1,1,1,1,4),(59.6902604182061,
59.775601223602,60.762062117007,61.748523010412,62.734983903817,63.721444797222,
64.6638825844085),.UNSPECIFIED.);
#1131=B_SPLINE_CURVE_WITH_KNOTS('',3,(#47547,#47548,#47549,#47550,#47551,
#47552,#47553,#47554,#47555,#47556),.UNSPECIFIED.,.F.,.F.,(4,1,1,1,1,1,
1,4),(53.4070751110265,54.2768072787229,55.2632681721279,56.2497290655329,
57.2361899589379,58.222650852343,59.209111745748,59.6902604182061),
 .UNSPECIFIED.);
#1132=B_SPLINE_CURVE_WITH_KNOTS('',3,(#47557,#47558,#47559,#47560,#47561,
#47562,#47563,#47564,#47565,#47566),.UNSPECIFIED.,.F.,.F.,(4,1,1,1,1,1,
1,4),(53.4070751110265,53.856835863172,54.843296756577,55.829757649982,
56.816218543387,57.802679436792,58.789140330197,59.6902604182061),
 .UNSPECIFIED.);
#1133=B_SPLINE_CURVE_WITH_KNOTS('',3,(#47571,#47572,#47573,#47574,#47575,
#47576,#47577,#47578,#47579,#47580,#47581),.UNSPECIFIED.,.F.,.F.,(4,1,1,
1,1,1,1,1,4),(47.1238898038469,47.3715810248879,48.3580419182929,49.3445028116979,
50.3309637051029,51.3174245985079,52.3038854919129,53.2903463853179,53.4070751110265),
 .UNSPECIFIED.);
#1134=B_SPLINE_CURVE_WITH_KNOTS('',3,(#47582,#47583,#47584,#47585,#47586,
#47587,#47588,#47589,#47590,#47591),.UNSPECIFIED.,.F.,.F.,(4,1,1,1,1,1,
1,4),(47.1238898038469,47.938070502742,48.924531396147,49.910992289552,
50.897453182957,51.883914076362,52.870374969767,53.4070751110265),
 .UNSPECIFIED.);
#1135=B_SPLINE_CURVE_WITH_KNOTS('',3,(#47596,#47597,#47598,#47599,#47600,
#47601,#47602,#47603,#47604,#47605),.UNSPECIFIED.,.F.,.F.,(4,1,1,1,1,1,
1,4),(40.8407044966673,41.4528156644579,42.4392765578629,43.4257374512679,
44.4121983446729,45.3986592380779,46.3851201314829,47.1238898038469),
 .UNSPECIFIED.);
#1136=B_SPLINE_CURVE_WITH_KNOTS('',3,(#47606,#47607,#47608,#47609,#47610,
#47611,#47612,#47613,#47614,#47615,#47616),.UNSPECIFIED.,.F.,.F.,(4,1,1,
1,1,1,1,1,4),(40.8407044966673,41.0328442489069,42.0193051423119,43.0057660357169,
43.9922269291219,44.978687822527,45.965148715932,46.951609609337,47.1238898038469),
 .UNSPECIFIED.);
#1137=B_SPLINE_CURVE_WITH_KNOTS('',3,(#47621,#47622,#47623,#47624,#47625,
#47626,#47627,#47628,#47629,#47630),.UNSPECIFIED.,.F.,.F.,(4,1,1,1,1,1,
1,4),(34.5575191894877,35.5340503040279,36.5205111974329,37.5069720908379,
38.4934329842429,39.4798938776479,40.4663547710529,40.8407044966673),
 .UNSPECIFIED.);
#1138=B_SPLINE_CURVE_WITH_KNOTS('',3,(#47631,#47632,#47633,#47634,#47635,
#47636,#47637,#47638,#47639,#47640),.UNSPECIFIED.,.F.,.F.,(4,1,1,1,1,1,
1,4),(34.5575191894877,35.1140788884769,36.1005397818819,37.0870006752869,
38.0734615686919,39.0599224620969,40.0463833555019,40.8407044966673),
 .UNSPECIFIED.);
#1139=B_SPLINE_CURVE_WITH_KNOTS('',3,(#47645,#47646,#47647,#47648,#47649,
#47650,#47651,#47652,#47653,#47654,#47655),.UNSPECIFIED.,.F.,.F.,(4,1,1,
1,1,1,1,1,4),(28.2743338823081,28.6288240501929,29.6152849435979,30.6017458370029,
31.5882067304079,32.5746676238129,33.5611285172179,34.5475894106229,34.5575191894877),
 .UNSPECIFIED.);
#1140=B_SPLINE_CURVE_WITH_KNOTS('',3,(#47656,#47657,#47658,#47659,#47660,
#47661,#47662,#47663,#47664,#47665),.UNSPECIFIED.,.F.,.F.,(4,1,1,1,1,1,
1,4),(28.2743338823081,29.1953135280469,30.1817744214519,31.1682353148569,
32.1546962082619,33.1411571016669,34.1276179950719,34.5575191894877),
 .UNSPECIFIED.);
#1141=B_SPLINE_CURVE_WITH_KNOTS('',3,(#47670,#47671,#47672,#47673,#47674,
#47675,#47676,#47677,#47678,#47679),.UNSPECIFIED.,.F.,.F.,(4,1,1,1,1,1,
1,4),(21.9911485751285,22.7100586897629,23.6965195831679,24.6829804765729,
25.6694413699779,26.6559022633829,27.6423631567879,28.2743338823081),
 .UNSPECIFIED.);
#1142=B_SPLINE_CURVE_WITH_KNOTS('',3,(#47680,#47681,#47682,#47683,#47684,
#47685,#47686,#47687,#47688,#47689,#47690),.UNSPECIFIED.,.F.,.F.,(4,1,1,
1,1,1,1,1,4),(21.9911485751285,22.2900872742119,23.2765481676169,24.2630090610219,
25.2494699544269,26.2359308478319,27.2223917412369,28.2088526346419,28.2743338823081),
 .UNSPECIFIED.);
#1143=B_SPLINE_CURVE_WITH_KNOTS('',3,(#47696,#47697,#47698,#47699,#47700),
 .UNSPECIFIED.,.F.,.F.,(4,1,4),(14.3984001269719,15.3848610203769,15.7079632679489),
 .UNSPECIFIED.);
#1144=B_SPLINE_CURVE_WITH_KNOTS('',3,(#47703,#47704,#47705,#47706,#47707),
 .UNSPECIFIED.,.F.,.F.,(4,1,4),(13.8759337553363,14.8183715425228,15.7079632679489),
 .UNSPECIFIED.);
#1145=B_SPLINE_CURVE_WITH_KNOTS('',3,(#47713,#47714,#47715,#47716),
 .UNSPECIFIED.,.F.,.F.,(4,4),(51.5750455984138,52.2824273504651),
 .UNSPECIFIED.);
#1146=B_SPLINE_CURVE_WITH_KNOTS('',3,(#47724,#47725,#47726,#47727,#47728,
#47729,#47730,#47731,#47732,#47733),.UNSPECIFIED.,.F.,.F.,(4,3,3,4),(-50.2654824574367,
-49.3230446702501,-48.3365837768451,-47.8312715558982),.UNSPECIFIED.);
#1147=B_SPLINE_CURVE_WITH_KNOTS('',3,(#47738,#47739,#47740,#47741,#47742,
#47743,#47744,#47745,#47746,#47747,#47748,#47749,#47750,#47751,#47752,#47753,
#47754,#47755,#47756,#47757,#47758,#47759,#47760,#47761,#47762),
 .UNSPECIFIED.,.F.,.F.,(4,3,3,3,3,3,3,3,4),(45.2918602912342,45.3772010966301,
46.3636619900351,47.3501228834401,48.3365837768451,49.3230446702501,50.3095055636551,
51.2959664570601,51.5750455984138),.UNSPECIFIED.);
#1148=B_SPLINE_CURVE_WITH_KNOTS('',3,(#47763,#47764,#47765,#47766,#47767,
#47768,#47769,#47770,#47771,#47772,#47773,#47774,#47775,#47776,#47777,#47778,
#47779,#47780,#47781,#47782,#47783,#47784),.UNSPECIFIED.,.F.,.F.,(4,3,3,
3,3,3,3,4),(-47.8312715558982,-47.3501228834401,-46.3636619900351,-45.3772010966301,
-44.3907402032251,-43.4042793098201,-42.4178184164151,-41.5480862487186),
 .UNSPECIFIED.);
#1149=B_SPLINE_CURVE_WITH_KNOTS('',3,(#47789,#47790,#47791,#47792,#47793,
#47794,#47795,#47796,#47797,#47798,#47799,#47800,#47801,#47802,#47803,#47804,
#47805,#47806,#47807,#47808,#47809,#47810),.UNSPECIFIED.,.F.,.F.,(4,3,3,
3,3,3,3,4),(39.0086749840546,39.4584357362001,40.4448966296051,41.4313575230101,
42.4178184164151,43.4042793098201,44.3907402032251,45.2918602912342),
 .UNSPECIFIED.);
#1150=B_SPLINE_CURVE_WITH_KNOTS('',3,(#47811,#47812,#47813,#47814,#47815,
#47816,#47817,#47818,#47819,#47820,#47821,#47822,#47823,#47824,#47825,#47826,
#47827,#47828,#47829,#47830,#47831,#47832,#47833,#47834,#47835),
 .UNSPECIFIED.,.F.,.F.,(4,3,3,3,3,3,3,3,4),(-41.5480862487186,-41.4313575230101,
-40.4448966296051,-39.4584357362001,-38.4719748427951,-37.4855139493901,
-36.4990530559851,-35.5125921625801,-35.2649009415391),.UNSPECIFIED.);
#1151=B_SPLINE_CURVE_WITH_KNOTS('',3,(#47840,#47841,#47842,#47843,#47844,
#47845,#47846,#47847,#47848,#47849,#47850,#47851,#47852,#47853,#47854,#47855,
#47856,#47857,#47858,#47859,#47860,#47861),.UNSPECIFIED.,.F.,.F.,(4,3,3,
3,3,3,3,4),(32.725489676875,33.5396703757701,34.5261312691751,35.5125921625801,
36.4990530559851,37.4855139493901,38.4719748427951,39.0086749840546),
 .UNSPECIFIED.);
#1152=B_SPLINE_CURVE_WITH_KNOTS('',3,(#47862,#47863,#47864,#47865,#47866,
#47867,#47868,#47869,#47870,#47871,#47872,#47873,#47874,#47875,#47876,#47877,
#47878,#47879,#47880,#47881,#47882,#47883),.UNSPECIFIED.,.F.,.F.,(4,3,3,
3,3,3,3,4),(-35.2649009415391,-34.5261312691751,-33.5396703757701,-32.5532094823651,
-31.5667485889601,-30.5802876955551,-29.5938268021501,-28.9817156343595),
 .UNSPECIFIED.);
#1153=B_SPLINE_CURVE_WITH_KNOTS('',3,(#47888,#47889,#47890,#47891,#47892,
#47893,#47894,#47895,#47896,#47897,#47898,#47899,#47900,#47901,#47902,#47903,
#47904,#47905,#47906,#47907,#47908,#47909,#47910,#47911,#47912),
 .UNSPECIFIED.,.F.,.F.,(4,3,3,3,3,3,3,3,4),(26.4423043696954,26.6344441219351,
27.6209050153401,28.6073659087451,29.5938268021501,30.5802876955551,31.5667485889601,
32.5532094823651,32.725489676875),.UNSPECIFIED.);
#1154=B_SPLINE_CURVE_WITH_KNOTS('',3,(#47913,#47914,#47915,#47916,#47917,
#47918,#47919,#47920,#47921,#47922,#47923,#47924,#47925,#47926,#47927,#47928,
#47929,#47930,#47931,#47932,#47933,#47934),.UNSPECIFIED.,.F.,.F.,(4,3,3,
3,3,3,3,4),(-28.9817156343595,-28.6073659087451,-27.6209050153401,-26.6344441219351,
-25.6479832285301,-24.6615223351251,-23.6750614417201,-22.6985303271799),
 .UNSPECIFIED.);
#1155=B_SPLINE_CURVE_WITH_KNOTS('',3,(#47939,#47940,#47941,#47942,#47943,
#47944,#47945,#47946,#47947,#47948,#47949,#47950,#47951,#47952,#47953,#47954,
#47955,#47956,#47957,#47958,#47959,#47960),.UNSPECIFIED.,.F.,.F.,(4,3,3,
3,3,3,3,4),(20.1591190625158,20.7156787615051,21.7021396549101,22.6886005483151,
23.6750614417201,24.6615223351251,25.6479832285301,26.4423043696954),
 .UNSPECIFIED.);
#1156=B_SPLINE_CURVE_WITH_KNOTS('',3,(#47961,#47962,#47963,#47964,#47965,
#47966,#47967,#47968,#47969,#47970,#47971,#47972,#47973,#47974,#47975,#47976,
#47977,#47978,#47979,#47980,#47981,#47982,#47983,#47984,#47985),
 .UNSPECIFIED.,.F.,.F.,(4,3,3,3,3,3,3,3,4),(-22.6985303271799,-22.6886005483151,
-21.70213965491,-20.715678761505,-19.7292178681,-18.742756974695,-17.75629608129,
-16.769835187885,-16.4153450200003),.UNSPECIFIED.);
#1157=B_SPLINE_CURVE_WITH_KNOTS('',3,(#47990,#47991,#47992,#47993,#47994,
#47995,#47996,#47997,#47998,#47999,#48000,#48001,#48002,#48003,#48004,#48005,
#48006,#48007,#48008,#48009,#48010,#48011),.UNSPECIFIED.,.F.,.F.,(4,3,3,
3,3,3,3,4),(13.8759337553362,14.796913401075,15.78337429448,16.769835187885,
17.7562960812901,18.7427569746951,19.7292178681001,20.1591190625158),
 .UNSPECIFIED.);
#1158=B_SPLINE_CURVE_WITH_KNOTS('',3,(#48012,#48013,#48014,#48015,#48016,
#48017,#48018,#48019,#48020,#48021,#48022,#48023,#48024,#48025,#48026,#48027,
#48028,#48029,#48030,#48031,#48032,#48033),.UNSPECIFIED.,.F.,.F.,(4,3,3,
3,3,3,3,4),(-16.4153450200003,-15.78337429448,-14.796913401075,-13.81045250767,
-12.823991614265,-11.83753072086,-10.851069827455,-10.1321597128207),
 .UNSPECIFIED.);
#1159=B_SPLINE_CURVE_WITH_KNOTS('',3,(#48039,#48040,#48041,#48042,#48043,
#48044,#48045,#48046,#48047,#48048,#48049,#48050,#48051),.UNSPECIFIED.,
 .F.,.F.,(4,3,3,3,4),(-3.84897440564113,-2.95938268021501,-1.97292178681,
-0.986460893405001,0.),.UNSPECIFIED.);
#1160=B_SPLINE_CURVE_WITH_KNOTS('',3,(#48054,#48055,#48056,#48057,#48058,
#48059,#48060,#48061,#48062,#48063,#48064,#48065,#48066,#48067,#48068,#48069,
#48070,#48071,#48072),.UNSPECIFIED.,.F.,.F.,(4,3,3,3,3,3,4),(2.01694489302845,
2.95938268021501,3.94584357362001,4.93230446702501,5.91876536043002,6.90522625383501,
7.59274844815666),.UNSPECIFIED.);
#1161=B_SPLINE_CURVE_WITH_KNOTS('',3,(#48078,#48079,#48080,#48081,#48082,
#48083,#48084,#48085),.UNSPECIFIED.,.F.,.F.,(4,1,1,1,1,4),(59.6902604182061,
60.1955726391529,61.1820335325579,62.1684944259629,63.154955319368,64.141416212773),
 .UNSPECIFIED.);
#1162=B_SPLINE_CURVE_WITH_KNOTS('',3,(#48088,#48089,#48090,#48091,#48092,
#48093,#48094,#48095,#48096),.UNSPECIFIED.,.F.,.F.,(4,1,1,1,1,1,4),(59.6902604182061,
59.775601223602,60.762062117007,61.748523010412,62.734983903817,63.721444797222,
64.6638825844085),.UNSPECIFIED.);
#1163=B_SPLINE_CURVE_WITH_KNOTS('',3,(#48101,#48102,#48103,#48104,#48105,
#48106,#48107,#48108,#48109,#48110),.UNSPECIFIED.,.F.,.F.,(4,1,1,1,1,1,
1,4),(53.4070751110265,54.2768072787229,55.2632681721279,56.2497290655329,
57.2361899589379,58.2226508523429,59.2091117457479,59.6902604182061),
 .UNSPECIFIED.);
#1164=B_SPLINE_CURVE_WITH_KNOTS('',3,(#48111,#48112,#48113,#48114,#48115,
#48116,#48117,#48118,#48119,#48120),.UNSPECIFIED.,.F.,.F.,(4,1,1,1,1,1,
1,4),(53.4070751110265,53.856835863172,54.843296756577,55.829757649982,
56.816218543387,57.802679436792,58.789140330197,59.6902604182061),
 .UNSPECIFIED.);
#1165=B_SPLINE_CURVE_WITH_KNOTS('',3,(#48125,#48126,#48127,#48128,#48129,
#48130,#48131,#48132,#48133,#48134,#48135),.UNSPECIFIED.,.F.,.F.,(4,1,1,
1,1,1,1,1,4),(47.1238898038469,47.3715810248879,48.3580419182929,49.3445028116979,
50.3309637051029,51.3174245985079,52.3038854919129,53.2903463853179,53.4070751110265),
 .UNSPECIFIED.);
#1166=B_SPLINE_CURVE_WITH_KNOTS('',3,(#48136,#48137,#48138,#48139,#48140,
#48141,#48142,#48143,#48144,#48145),.UNSPECIFIED.,.F.,.F.,(4,1,1,1,1,1,
1,4),(47.1238898038469,47.9380705027419,48.9245313961469,49.9109922895519,
50.897453182957,51.883914076362,52.870374969767,53.4070751110265),
 .UNSPECIFIED.);
#1167=B_SPLINE_CURVE_WITH_KNOTS('',3,(#48150,#48151,#48152,#48153,#48154,
#48155,#48156,#48157,#48158,#48159),.UNSPECIFIED.,.F.,.F.,(4,1,1,1,1,1,
1,4),(40.8407044966673,41.4528156644579,42.4392765578629,43.4257374512679,
44.4121983446729,45.3986592380779,46.3851201314829,47.1238898038469),
 .UNSPECIFIED.);
#1168=B_SPLINE_CURVE_WITH_KNOTS('',3,(#48160,#48161,#48162,#48163,#48164,
#48165,#48166,#48167,#48168,#48169,#48170),.UNSPECIFIED.,.F.,.F.,(4,1,1,
1,1,1,1,1,4),(40.8407044966673,41.0328442489069,42.0193051423119,43.0057660357169,
43.9922269291219,44.9786878225269,45.9651487159319,46.9516096093369,47.1238898038469),
 .UNSPECIFIED.);
#1169=B_SPLINE_CURVE_WITH_KNOTS('',3,(#48175,#48176,#48177,#48178,#48179,
#48180,#48181,#48182,#48183,#48184),.UNSPECIFIED.,.F.,.F.,(4,1,1,1,1,1,
1,4),(34.5575191894877,35.5340503040279,36.5205111974329,37.5069720908379,
38.4934329842429,39.4798938776479,40.4663547710529,40.8407044966673),
 .UNSPECIFIED.);
#1170=B_SPLINE_CURVE_WITH_KNOTS('',3,(#48185,#48186,#48187,#48188,#48189,
#48190,#48191,#48192,#48193,#48194),.UNSPECIFIED.,.F.,.F.,(4,1,1,1,1,1,
1,4),(34.5575191894877,35.1140788884769,36.1005397818819,37.0870006752869,
38.0734615686919,39.0599224620969,40.0463833555019,40.8407044966673),
 .UNSPECIFIED.);
#1171=B_SPLINE_CURVE_WITH_KNOTS('',3,(#48199,#48200,#48201,#48202,#48203,
#48204,#48205,#48206,#48207,#48208,#48209),.UNSPECIFIED.,.F.,.F.,(4,1,1,
1,1,1,1,1,4),(28.2743338823081,28.6288240501929,29.6152849435979,30.6017458370029,
31.5882067304079,32.5746676238129,33.5611285172179,34.5475894106229,34.5575191894877),
 .UNSPECIFIED.);
#1172=B_SPLINE_CURVE_WITH_KNOTS('',3,(#48210,#48211,#48212,#48213,#48214,
#48215,#48216,#48217,#48218,#48219),.UNSPECIFIED.,.F.,.F.,(4,1,1,1,1,1,
1,4),(28.2743338823081,29.1953135280469,30.1817744214519,31.1682353148569,
32.1546962082619,33.1411571016669,34.1276179950719,34.5575191894877),
 .UNSPECIFIED.);
#1173=B_SPLINE_CURVE_WITH_KNOTS('',3,(#48224,#48225,#48226,#48227,#48228,
#48229,#48230,#48231,#48232,#48233),.UNSPECIFIED.,.F.,.F.,(4,1,1,1,1,1,
1,4),(21.9911485751285,22.7100586897628,23.6965195831678,24.6829804765729,
25.6694413699779,26.6559022633829,27.6423631567879,28.2743338823081),
 .UNSPECIFIED.);
#1174=B_SPLINE_CURVE_WITH_KNOTS('',3,(#48234,#48235,#48236,#48237,#48238,
#48239,#48240,#48241,#48242,#48243,#48244),.UNSPECIFIED.,.F.,.F.,(4,1,1,
1,1,1,1,1,4),(21.9911485751285,22.2900872742119,23.2765481676169,24.2630090610219,
25.2494699544269,26.2359308478319,27.2223917412369,28.2088526346419,28.2743338823081),
 .UNSPECIFIED.);
#1175=B_SPLINE_CURVE_WITH_KNOTS('',3,(#48250,#48251,#48252,#48253,#48254),
 .UNSPECIFIED.,.F.,.F.,(4,1,4),(14.3984001269719,15.3848610203769,15.7079632679489),
 .UNSPECIFIED.);
#1176=B_SPLINE_CURVE_WITH_KNOTS('',3,(#48257,#48258,#48259,#48260,#48261),
 .UNSPECIFIED.,.F.,.F.,(4,1,4),(13.8759337553363,14.8183715425228,15.7079632679489),
 .UNSPECIFIED.);
#1177=B_SPLINE_CURVE_WITH_KNOTS('',3,(#48267,#48268,#48269,#48270),
 .UNSPECIFIED.,.F.,.F.,(4,4),(51.5750455984138,52.2824273504651),
 .UNSPECIFIED.);
#1178=B_SPLINE_CURVE_WITH_KNOTS('',3,(#48278,#48279,#48280,#48281,#48282,
#48283,#48284,#48285,#48286,#48287),.UNSPECIFIED.,.F.,.F.,(4,3,3,4),(-50.2654824574367,
-49.3230446702501,-48.3365837768451,-47.8312715558982),.UNSPECIFIED.);
#1179=B_SPLINE_CURVE_WITH_KNOTS('',3,(#48292,#48293,#48294,#48295,#48296,
#48297,#48298,#48299,#48300,#48301,#48302,#48303,#48304,#48305,#48306,#48307,
#48308,#48309,#48310,#48311,#48312,#48313,#48314,#48315,#48316),
 .UNSPECIFIED.,.F.,.F.,(4,3,3,3,3,3,3,3,4),(45.2918602912342,45.3772010966301,
46.3636619900351,47.3501228834401,48.3365837768451,49.3230446702501,50.3095055636551,
51.2959664570601,51.5750455984138),.UNSPECIFIED.);
#1180=B_SPLINE_CURVE_WITH_KNOTS('',3,(#48317,#48318,#48319,#48320,#48321,
#48322,#48323,#48324,#48325,#48326,#48327,#48328,#48329,#48330,#48331,#48332,
#48333,#48334,#48335,#48336,#48337,#48338),.UNSPECIFIED.,.F.,.F.,(4,3,3,
3,3,3,3,4),(-47.8312715558982,-47.3501228834401,-46.3636619900351,-45.3772010966301,
-44.3907402032251,-43.4042793098201,-42.4178184164151,-41.5480862487186),
 .UNSPECIFIED.);
#1181=B_SPLINE_CURVE_WITH_KNOTS('',3,(#48343,#48344,#48345,#48346,#48347,
#48348,#48349,#48350,#48351,#48352,#48353,#48354,#48355,#48356,#48357,#48358,
#48359,#48360,#48361,#48362,#48363,#48364),.UNSPECIFIED.,.F.,.F.,(4,3,3,
3,3,3,3,4),(39.0086749840546,39.4584357362001,40.4448966296051,41.4313575230101,
42.4178184164151,43.4042793098201,44.3907402032251,45.2918602912342),
 .UNSPECIFIED.);
#1182=B_SPLINE_CURVE_WITH_KNOTS('',3,(#48365,#48366,#48367,#48368,#48369,
#48370,#48371,#48372,#48373,#48374,#48375,#48376,#48377,#48378,#48379,#48380,
#48381,#48382,#48383,#48384,#48385,#48386,#48387,#48388,#48389),
 .UNSPECIFIED.,.F.,.F.,(4,3,3,3,3,3,3,3,4),(-41.5480862487186,-41.4313575230101,
-40.4448966296051,-39.4584357362001,-38.4719748427951,-37.4855139493901,
-36.4990530559851,-35.5125921625801,-35.2649009415391),.UNSPECIFIED.);
#1183=B_SPLINE_CURVE_WITH_KNOTS('',3,(#48394,#48395,#48396,#48397,#48398,
#48399,#48400,#48401,#48402,#48403,#48404,#48405,#48406,#48407,#48408,#48409,
#48410,#48411,#48412,#48413,#48414,#48415),.UNSPECIFIED.,.F.,.F.,(4,3,3,
3,3,3,3,4),(32.725489676875,33.5396703757701,34.5261312691751,35.5125921625801,
36.4990530559851,37.4855139493901,38.4719748427951,39.0086749840546),
 .UNSPECIFIED.);
#1184=B_SPLINE_CURVE_WITH_KNOTS('',3,(#48416,#48417,#48418,#48419,#48420,
#48421,#48422,#48423,#48424,#48425,#48426,#48427,#48428,#48429,#48430,#48431,
#48432,#48433,#48434,#48435,#48436,#48437),.UNSPECIFIED.,.F.,.F.,(4,3,3,
3,3,3,3,4),(-35.2649009415391,-34.5261312691751,-33.5396703757701,-32.5532094823651,
-31.5667485889601,-30.5802876955551,-29.5938268021501,-28.9817156343595),
 .UNSPECIFIED.);
#1185=B_SPLINE_CURVE_WITH_KNOTS('',3,(#48442,#48443,#48444,#48445,#48446,
#48447,#48448,#48449,#48450,#48451,#48452,#48453,#48454,#48455,#48456,#48457,
#48458,#48459,#48460,#48461,#48462,#48463,#48464,#48465,#48466),
 .UNSPECIFIED.,.F.,.F.,(4,3,3,3,3,3,3,3,4),(26.4423043696954,26.6344441219351,
27.6209050153401,28.6073659087451,29.5938268021501,30.5802876955551,31.5667485889601,
32.5532094823651,32.725489676875),.UNSPECIFIED.);
#1186=B_SPLINE_CURVE_WITH_KNOTS('',3,(#48467,#48468,#48469,#48470,#48471,
#48472,#48473,#48474,#48475,#48476,#48477,#48478,#48479,#48480,#48481,#48482,
#48483,#48484,#48485,#48486,#48487,#48488),.UNSPECIFIED.,.F.,.F.,(4,3,3,
3,3,3,3,4),(-28.9817156343595,-28.6073659087451,-27.6209050153401,-26.6344441219351,
-25.6479832285301,-24.6615223351251,-23.6750614417201,-22.6985303271799),
 .UNSPECIFIED.);
#1187=B_SPLINE_CURVE_WITH_KNOTS('',3,(#48493,#48494,#48495,#48496,#48497,
#48498,#48499,#48500,#48501,#48502,#48503,#48504,#48505,#48506,#48507,#48508,
#48509,#48510,#48511,#48512,#48513,#48514),.UNSPECIFIED.,.F.,.F.,(4,3,3,
3,3,3,3,4),(20.1591190625158,20.7156787615051,21.7021396549101,22.6886005483151,
23.6750614417201,24.6615223351251,25.6479832285301,26.4423043696954),
 .UNSPECIFIED.);
#1188=B_SPLINE_CURVE_WITH_KNOTS('',3,(#48515,#48516,#48517,#48518,#48519,
#48520,#48521,#48522,#48523,#48524,#48525,#48526,#48527,#48528,#48529,#48530,
#48531,#48532,#48533,#48534,#48535,#48536,#48537,#48538,#48539),
 .UNSPECIFIED.,.F.,.F.,(4,3,3,3,3,3,3,3,4),(-22.6985303271799,-22.6886005483151,
-21.7021396549101,-20.7156787615051,-19.7292178681001,-18.742756974695,
-17.75629608129,-16.769835187885,-16.4153450200003),.UNSPECIFIED.);
#1189=B_SPLINE_CURVE_WITH_KNOTS('',3,(#48544,#48545,#48546,#48547,#48548,
#48549,#48550,#48551,#48552,#48553,#48554,#48555,#48556,#48557,#48558,#48559,
#48560,#48561,#48562,#48563,#48564,#48565),.UNSPECIFIED.,.F.,.F.,(4,3,3,
3,3,3,3,4),(13.8759337553362,14.796913401075,15.78337429448,16.769835187885,
17.75629608129,18.7427569746951,19.7292178681001,20.1591190625158),
 .UNSPECIFIED.);
#1190=B_SPLINE_CURVE_WITH_KNOTS('',3,(#48566,#48567,#48568,#48569,#48570,
#48571,#48572,#48573,#48574,#48575,#48576,#48577,#48578,#48579,#48580,#48581,
#48582,#48583,#48584,#48585,#48586,#48587),.UNSPECIFIED.,.F.,.F.,(4,3,3,
3,3,3,3,4),(-16.4153450200003,-15.78337429448,-14.796913401075,-13.81045250767,
-12.823991614265,-11.83753072086,-10.851069827455,-10.1321597128207),
 .UNSPECIFIED.);
#1191=B_SPLINE_CURVE_WITH_KNOTS('',3,(#48593,#48594,#48595,#48596,#48597,
#48598,#48599,#48600,#48601,#48602,#48603,#48604,#48605),.UNSPECIFIED.,
 .F.,.F.,(4,3,3,3,4),(-3.84897440564113,-2.95938268021501,-1.97292178681001,
-0.986460893405003,0.),.UNSPECIFIED.);
#1192=B_SPLINE_CURVE_WITH_KNOTS('',3,(#48608,#48609,#48610,#48611,#48612,
#48613,#48614,#48615,#48616,#48617,#48618,#48619,#48620,#48621,#48622,#48623,
#48624,#48625,#48626),.UNSPECIFIED.,.F.,.F.,(4,3,3,3,3,3,4),(2.01694489302845,
2.95938268021501,3.94584357362001,4.93230446702502,5.91876536043002,6.90522625383502,
7.59274844815666),.UNSPECIFIED.);
#1193=B_SPLINE_CURVE_WITH_KNOTS('',3,(#48632,#48633,#48634,#48635,#48636,
#48637,#48638,#48639),.UNSPECIFIED.,.F.,.F.,(4,1,1,1,1,4),(59.6902604182061,
60.1955726391529,61.1820335325579,62.1684944259629,63.154955319368,64.141416212773),
 .UNSPECIFIED.);
#1194=B_SPLINE_CURVE_WITH_KNOTS('',3,(#48642,#48643,#48644,#48645,#48646,
#48647,#48648,#48649,#48650),.UNSPECIFIED.,.F.,.F.,(4,1,1,1,1,1,4),(59.6902604182061,
59.775601223602,60.762062117007,61.748523010412,62.734983903817,63.721444797222,
64.6638825844085),.UNSPECIFIED.);
#1195=B_SPLINE_CURVE_WITH_KNOTS('',3,(#48655,#48656,#48657,#48658,#48659,
#48660,#48661,#48662,#48663,#48664),.UNSPECIFIED.,.F.,.F.,(4,1,1,1,1,1,
1,4),(53.4070751110265,54.2768072787229,55.2632681721279,56.2497290655329,
57.2361899589379,58.2226508523429,59.2091117457479,59.6902604182061),
 .UNSPECIFIED.);
#1196=B_SPLINE_CURVE_WITH_KNOTS('',3,(#48665,#48666,#48667,#48668,#48669,
#48670,#48671,#48672,#48673,#48674),.UNSPECIFIED.,.F.,.F.,(4,1,1,1,1,1,
1,4),(53.4070751110265,53.856835863172,54.843296756577,55.829757649982,
56.816218543387,57.802679436792,58.789140330197,59.6902604182061),
 .UNSPECIFIED.);
#1197=B_SPLINE_CURVE_WITH_KNOTS('',3,(#48679,#48680,#48681,#48682,#48683,
#48684,#48685,#48686,#48687,#48688,#48689),.UNSPECIFIED.,.F.,.F.,(4,1,1,
1,1,1,1,1,4),(47.1238898038469,47.3715810248879,48.3580419182929,49.3445028116979,
50.3309637051029,51.3174245985079,52.3038854919129,53.2903463853179,53.4070751110265),
 .UNSPECIFIED.);
#1198=B_SPLINE_CURVE_WITH_KNOTS('',3,(#48690,#48691,#48692,#48693,#48694,
#48695,#48696,#48697,#48698,#48699),.UNSPECIFIED.,.F.,.F.,(4,1,1,1,1,1,
1,4),(47.1238898038469,47.9380705027419,48.9245313961469,49.9109922895519,
50.897453182957,51.883914076362,52.870374969767,53.4070751110265),
 .UNSPECIFIED.);
#1199=B_SPLINE_CURVE_WITH_KNOTS('',3,(#48704,#48705,#48706,#48707,#48708,
#48709,#48710,#48711,#48712,#48713),.UNSPECIFIED.,.F.,.F.,(4,1,1,1,1,1,
1,4),(40.8407044966673,41.4528156644579,42.4392765578629,43.4257374512679,
44.4121983446729,45.3986592380779,46.3851201314829,47.1238898038469),
 .UNSPECIFIED.);
#1200=B_SPLINE_CURVE_WITH_KNOTS('',3,(#48714,#48715,#48716,#48717,#48718,
#48719,#48720,#48721,#48722,#48723,#48724),.UNSPECIFIED.,.F.,.F.,(4,1,1,
1,1,1,1,1,4),(40.8407044966673,41.0328442489069,42.0193051423119,43.0057660357169,
43.9922269291219,44.9786878225269,45.9651487159319,46.9516096093369,47.1238898038469),
 .UNSPECIFIED.);
#1201=B_SPLINE_CURVE_WITH_KNOTS('',3,(#48729,#48730,#48731,#48732,#48733,
#48734,#48735,#48736,#48737,#48738),.UNSPECIFIED.,.F.,.F.,(4,1,1,1,1,1,
1,4),(34.5575191894877,35.5340503040279,36.5205111974329,37.5069720908379,
38.4934329842429,39.4798938776479,40.4663547710529,40.8407044966673),
 .UNSPECIFIED.);
#1202=B_SPLINE_CURVE_WITH_KNOTS('',3,(#48739,#48740,#48741,#48742,#48743,
#48744,#48745,#48746,#48747,#48748),.UNSPECIFIED.,.F.,.F.,(4,1,1,1,1,1,
1,4),(34.5575191894877,35.1140788884769,36.1005397818819,37.0870006752869,
38.0734615686919,39.0599224620969,40.0463833555019,40.8407044966673),
 .UNSPECIFIED.);
#1203=B_SPLINE_CURVE_WITH_KNOTS('',3,(#48753,#48754,#48755,#48756,#48757,
#48758,#48759,#48760,#48761,#48762,#48763),.UNSPECIFIED.,.F.,.F.,(4,1,1,
1,1,1,1,1,4),(28.2743338823081,28.6288240501929,29.6152849435979,30.6017458370029,
31.5882067304079,32.5746676238129,33.5611285172179,34.5475894106229,34.5575191894877),
 .UNSPECIFIED.);
#1204=B_SPLINE_CURVE_WITH_KNOTS('',3,(#48764,#48765,#48766,#48767,#48768,
#48769,#48770,#48771,#48772,#48773),.UNSPECIFIED.,.F.,.F.,(4,1,1,1,1,1,
1,4),(28.2743338823081,29.1953135280469,30.1817744214519,31.1682353148569,
32.1546962082619,33.1411571016669,34.1276179950719,34.5575191894877),
 .UNSPECIFIED.);
#1205=B_SPLINE_CURVE_WITH_KNOTS('',3,(#48778,#48779,#48780,#48781,#48782,
#48783,#48784,#48785,#48786,#48787),.UNSPECIFIED.,.F.,.F.,(4,1,1,1,1,1,
1,4),(21.9911485751285,22.7100586897628,23.6965195831678,24.6829804765729,
25.6694413699779,26.6559022633829,27.6423631567879,28.2743338823081),
 .UNSPECIFIED.);
#1206=B_SPLINE_CURVE_WITH_KNOTS('',3,(#48788,#48789,#48790,#48791,#48792,
#48793,#48794,#48795,#48796,#48797,#48798),.UNSPECIFIED.,.F.,.F.,(4,1,1,
1,1,1,1,1,4),(21.9911485751285,22.2900872742119,23.2765481676169,24.2630090610219,
25.2494699544269,26.2359308478319,27.2223917412369,28.2088526346419,28.2743338823081),
 .UNSPECIFIED.);
#1207=B_SPLINE_CURVE_WITH_KNOTS('',3,(#48804,#48805,#48806,#48807,#48808),
 .UNSPECIFIED.,.F.,.F.,(4,1,4),(14.3984001269719,15.3848610203769,15.7079632679489),
 .UNSPECIFIED.);
#1208=B_SPLINE_CURVE_WITH_KNOTS('',3,(#48811,#48812,#48813,#48814,#48815),
 .UNSPECIFIED.,.F.,.F.,(4,1,4),(13.8759337553363,14.8183715425228,15.7079632679489),
 .UNSPECIFIED.);
#1209=B_SPLINE_CURVE_WITH_KNOTS('',3,(#48817,#48818,#48819,#48820,#48821,
#48822,#48823,#48824,#48825,#48826,#48827,#48828,#48829,#48830,#48831,#48832,
#48833,#48834,#48835,#48836,#48837,#48838,#48839,#48840,#48841,#48842,#48843,
#48844,#48845,#48846,#48847,#48848,#48849,#48850,#48851,#48852,#48853,#48854,
#48855,#48856,#48857,#48858,#48859,#48860,#48861,#48862,#48863,#48864,#48865,
#48866,#48867,#48868,#48869,#48870,#48871,#48872,#48873,#48874,#48875,#48876,
#48877,#48878,#48879,#48880,#48881,#48882,#48883,#48884,#48885,#48886,#48887,
#48888,#48889,#48890,#48891,#48892,#48893,#48894,#48895,#48896,#48897,#48898,
#48899,#48900,#48901,#48902,#48903,#48904,#48905,#48906,#48907,#48908,#48909,
#48910),.UNSPECIFIED.,.F.,.F.,(4,3,3,3,3,3,3,3,3,3,3,3,3,3,3,3,3,3,3,3,
3,3,3,3,3,3,3,3,3,3,3,4),(-0.569248610399453,-0.543562558043411,-0.517250584660783,
-0.510351573265488,-0.504796629765234,-0.477730613871864,-0.456104856148543,
-0.448985761186696,-0.442526474182097,-0.414793258161359,-0.386635508597981,
-0.358697135593994,-0.34520398971682,-0.340863862860947,-0.336326730527656,
-0.307401056922635,-0.304724552085299,-0.276937944371136,-0.248514561286397,
-0.23265772508323,-0.228221590562879,-0.199230787763733,-0.169668272024871,
-0.139872989252767,-0.12408548320274,-0.117715318700335,-0.113354339820942,
-0.0828129568830819,-0.0522455401301121,-0.022270235741096,-0.0135729408525504,
0.),.UNSPECIFIED.);
#1210=B_SPLINE_CURVE_WITH_KNOTS('',3,(#48911,#48912,#48913,#48914,#48915,
#48916,#48917,#48918,#48919,#48920,#48921,#48922,#48923,#48924,#48925,#48926,
#48927,#48928,#48929,#48930,#48931,#48932,#48933,#48934,#48935,#48936,#48937,
#48938,#48939,#48940,#48941,#48942,#48943,#48944,#48945,#48946,#48947,#48948,
#48949,#48950,#48951,#48952,#48953,#48954,#48955,#48956,#48957,#48958,#48959,
#48960,#48961,#48962,#48963,#48964,#48965,#48966,#48967,#48968,#48969,#48970,
#48971,#48972,#48973,#48974,#48975,#48976,#48977,#48978,#48979,#48980,#48981,
#48982,#48983,#48984,#48985,#48986,#48987,#48988,#48989,#48990,#48991,#48992,
#48993,#48994,#48995,#48996,#48997,#48998,#48999,#49000,#49001,#49002,#49003,
#49004,#49005,#49006,#49007),.UNSPECIFIED.,.F.,.F.,(4,3,3,3,3,3,3,3,3,3,
3,3,3,3,3,3,3,3,3,3,3,3,3,3,3,3,3,3,3,3,3,3,4),(-0.566847306048093,-0.536658716403432,
-0.50605373953314,-0.497358803993733,-0.490469668716376,-0.460327091817824,
-0.43729948162817,-0.425273577512184,-0.420376587364543,-0.390957251202536,
-0.362079079161669,-0.333750895422636,-0.319339724142124,-0.312267998605923,
-0.308232630749578,-0.280241862158672,-0.276106210300586,-0.247648696044962,
-0.218090837421661,-0.209492455589693,-0.204737921056362,-0.200614185310069,
-0.172780910553805,-0.145025994944757,-0.117750394973387,-0.104429823984033,
-0.100024823328952,-0.0958388020470428,-0.0691739371857627,-0.0429558817167698,
-0.017514133983365,-0.0111858270585532,0.),.UNSPECIFIED.);
#1211=B_SPLINE_CURVE_WITH_KNOTS('',3,(#49009,#49010,#49011,#49012,#49013,
#49014,#49015,#49016,#49017,#49018,#49019),.UNSPECIFIED.,.F.,.F.,(4,1,1,
1,1,1,1,1,4),(15.7079632679489,15.8048324359278,16.7912933293328,17.7777542227378,
18.7642151161428,19.7506760095478,20.7371369029528,21.7235977963578,21.9911485751285),
 .UNSPECIFIED.);
#1212=B_SPLINE_CURVE_WITH_KNOTS('',3,(#49020,#49021,#49022,#49023,#49024,
#49025,#49026,#49027,#49028,#49029),.UNSPECIFIED.,.F.,.F.,(4,1,1,1,1,1,
1,4),(15.7079632679489,16.3713219137819,17.3577828071869,18.3442437005919,
19.3307045939969,20.3171654874019,21.3036263808069,21.9911485751285),
 .UNSPECIFIED.);
#1213=B_SPLINE_CURVE_WITH_KNOTS('',3,(#49254,#49255,#49256,#49257,#49258,
#49259,#49260,#49261,#49262,#49263,#49264,#49265,#49266,#49267,#49268,#49269,
#49270,#49271,#49272,#49273,#49274,#49275,#49276,#49277,#49278,#49279,#49280,
#49281,#49282,#49283,#49284,#49285,#49286,#49287,#49288,#49289,#49290,#49291,
#49292,#49293,#49294,#49295,#49296,#49297,#49298,#49299,#49300,#49301,#49302,
#49303,#49304,#49305,#49306,#49307,#49308,#49309,#49310,#49311,#49312,#49313,
#49314,#49315,#49316,#49317,#49318,#49319,#49320,#49321,#49322,#49323,#49324,
#49325,#49326,#49327,#49328,#49329,#49330,#49331,#49332,#49333,#49334,#49335,
#49336,#49337,#49338,#49339,#49340,#49341,#49342,#49343,#49344),
 .UNSPECIFIED.,.F.,.F.,(4,3,3,3,3,3,3,3,3,3,3,3,3,3,3,3,3,3,3,3,3,3,3,3,
3,3,3,3,3,3,4),(0.,0.0253755398454445,0.0514213153132464,0.077957584539944,
0.0899764747654525,0.096803871475702,0.102648438541228,0.129953427359202,
0.157705320199216,0.184206857431119,0.195897861719558,0.201348082731475,
0.206600886453667,0.235230947526492,0.263711469126827,0.291580359310597,
0.307939787194046,0.312151069047901,0.340175334720984,0.369258031218753,
0.398694002185391,0.41802365259294,0.423204309536776,0.428148753834381,
0.459444366737233,0.482916076414372,0.491343338637999,0.498388095452059,
0.528903290158942,0.553331205445788,0.566847306048063),.UNSPECIFIED.);
#1214=B_SPLINE_CURVE_WITH_KNOTS('',3,(#49345,#49346,#49347,#49348,#49349,
#49350,#49351,#49352,#49353,#49354,#49355,#49356,#49357,#49358,#49359,#49360,
#49361,#49362,#49363,#49364,#49365,#49366,#49367,#49368,#49369),
 .UNSPECIFIED.,.F.,.F.,(4,3,3,3,3,3,3,3,4),(-10.1321597128207,-9.86460893405002,
-8.87814804064502,-7.89168714724002,-6.90522625383502,-5.91876536043002,
-4.93230446702501,-3.94584357362001,-3.84897440564113),.UNSPECIFIED.);
#1215=B_SPLINE_CURVE_WITH_KNOTS('',3,(#49594,#49595,#49596,#49597,#49598,
#49599,#49600,#49601,#49602,#49603,#49604,#49605,#49606,#49607,#49608,#49609,
#49610,#49611,#49612,#49613,#49614,#49615,#49616,#49617,#49618),
 .UNSPECIFIED.,.F.,.F.,(4,3,3,3,3,3,3,3,4),(7.59274844815666,7.89168714724002,
8.87814804064503,9.86460893405003,10.851069827455,11.83753072086,12.823991614265,
13.81045250767,13.8759337553362),.UNSPECIFIED.);
#1216=B_SPLINE_CURVE_WITH_KNOTS('',3,(#49619,#49620,#49621,#49622,#49623,
#49624,#49625,#49626,#49627,#49628,#49629,#49630,#49631,#49632,#49633,#49634,
#49635,#49636,#49637,#49638,#49639,#49640,#49641,#49642,#49643,#49644,#49645,
#49646,#49647,#49648,#49649,#49650,#49651,#49652,#49653,#49654,#49655,#49656,
#49657,#49658,#49659,#49660,#49661,#49662,#49663,#49664,#49665,#49666,#49667,
#49668,#49669,#49670,#49671,#49672,#49673,#49674,#49675,#49676,#49677,#49678,
#49679,#49680,#49681,#49682,#49683,#49684,#49685,#49686,#49687,#49688,#49689,
#49690,#49691,#49692,#49693,#49694,#49695,#49696,#49697,#49698,#49699,#49700,
#49701,#49702,#49703,#49704,#49705,#49706),.UNSPECIFIED.,.F.,.F.,(4,3,3,
3,3,3,3,3,3,3,3,3,3,3,3,3,3,3,3,3,3,3,3,3,3,3,3,3,3,4),(0.,0.0297349244535721,
0.060121569348429,0.0891410162773849,0.114533032340221,0.120626667476319,
0.15038169425931,0.17997017941563,0.208046920756741,0.230390549968388,0.234466744960236,
0.263371944870156,0.292277144780076,0.321216417936983,0.336017031727334,
0.340284462229876,0.344592011030409,0.372696707961539,0.400818636707195,
0.428516289762568,0.439576354164994,0.44540318305,0.450327524863458,0.477288294894219,
0.497472780816313,0.505235740104314,0.511959381000542,0.537907915849272,
0.558026238582596,0.569248610399449),.UNSPECIFIED.);
#1217=B_SPLINE_CURVE_WITH_KNOTS('',3,(#49709,#49710,#49711,#49712,#49713,
#49714,#49715,#49716,#49717,#49718,#49719,#49720,#49721,#49722,#49723,#49724,
#49725,#49726,#49727,#49728,#49729,#49730,#49731,#49732,#49733,#49734,#49735,
#49736,#49737,#49738,#49739,#49740,#49741,#49742,#49743,#49744,#49745,#49746,
#49747,#49748,#49749,#49750,#49751,#49752,#49753,#49754,#49755,#49756,#49757,
#49758,#49759,#49760,#49761,#49762,#49763,#49764,#49765,#49766,#49767,#49768,
#49769,#49770,#49771,#49772,#49773,#49774,#49775,#49776,#49777,#49778,#49779,
#49780,#49781,#49782,#49783,#49784,#49785,#49786,#49787,#49788,#49789,#49790,
#49791,#49792,#49793,#49794,#49795,#49796,#49797,#49798,#49799,#49800,#49801,
#49802),.UNSPECIFIED.,.F.,.F.,(4,3,3,3,3,3,3,3,3,3,3,3,3,3,3,3,3,3,3,3,
3,3,3,3,3,3,3,3,3,3,3,4),(-0.569248610399449,-0.543563182261633,-0.517251726319563,
-0.510354426439678,-0.50479695498386,-0.477731372271303,-0.456105519748053,
-0.448988869091777,-0.442526350881559,-0.414793531524841,-0.386635753667763,
-0.358697146614525,-0.34520399798222,-0.340863870845798,-0.33632674866549,
-0.307401034118885,-0.304724552085303,-0.276937498904782,-0.248513836066906,
-0.232656079580101,-0.228221193819419,-0.199230039362694,-0.1696673522492,
-0.139872047864531,-0.124084659488033,-0.117720027272243,-0.113355233265148,
-0.0828137979174933,-0.0522463837565239,-0.0222709947806455,-0.0135729408525504,
0.),.UNSPECIFIED.);
#1218=B_SPLINE_CURVE_WITH_KNOTS('',3,(#49803,#49804,#49805,#49806,#49807,
#49808,#49809,#49810,#49811,#49812,#49813,#49814,#49815,#49816,#49817,#49818,
#49819,#49820,#49821,#49822,#49823,#49824,#49825,#49826,#49827,#49828,#49829,
#49830,#49831,#49832,#49833,#49834,#49835,#49836,#49837,#49838,#49839,#49840,
#49841,#49842,#49843,#49844,#49845,#49846,#49847,#49848,#49849,#49850,#49851,
#49852,#49853,#49854,#49855,#49856,#49857,#49858,#49859,#49860,#49861,#49862,
#49863,#49864,#49865,#49866,#49867,#49868,#49869,#49870,#49871,#49872,#49873,
#49874,#49875,#49876,#49877,#49878,#49879,#49880,#49881,#49882,#49883,#49884,
#49885,#49886,#49887,#49888,#49889,#49890,#49891,#49892,#49893,#49894,#49895,
#49896,#49897,#49898,#49899),.UNSPECIFIED.,.F.,.F.,(4,3,3,3,3,3,3,3,3,3,
3,3,3,3,3,3,3,3,3,3,3,3,3,3,3,3,3,3,3,3,3,3,4),(-0.566847306048093,-0.536659041927388,
-0.506054142756331,-0.497359284644658,-0.490469768799004,-0.460327170439997,
-0.43729955042257,-0.425273732599625,-0.420376646332479,-0.390957260247852,
-0.362078935948881,-0.333750632250775,-0.319339526763226,-0.312267682102884,
-0.308232073167884,-0.280241164390834,-0.276106210300581,-0.247648676940529,
-0.218090820705282,-0.209492305755956,-0.204738428044034,-0.200614618605046,
-0.172781361973988,-0.145026407762726,-0.11775064123255,-0.1044300394608,
-0.100025210256123,-0.0958388268874492,-0.0691738559200647,-0.0429555864020897,
-0.0175134923892686,-0.011185827058555,0.),.UNSPECIFIED.);
#1219=B_SPLINE_CURVE_WITH_KNOTS('',3,(#49901,#49902,#49903,#49904,#49905,
#49906,#49907,#49908,#49909,#49910,#49911),.UNSPECIFIED.,.F.,.F.,(4,1,1,
1,1,1,1,1,4),(15.7079632679489,15.8048324359278,16.7912933293328,17.7777542227378,
18.7642151161428,19.7506760095478,20.7371369029528,21.7235977963578,21.9911485751285),
 .UNSPECIFIED.);
#1220=B_SPLINE_CURVE_WITH_KNOTS('',3,(#49912,#49913,#49914,#49915,#49916,
#49917,#49918,#49919,#49920,#49921),.UNSPECIFIED.,.F.,.F.,(4,1,1,1,1,1,
1,4),(15.7079632679489,16.3713219137819,17.3577828071869,18.3442437005919,
19.3307045939969,20.3171654874019,21.3036263808069,21.9911485751285),
 .UNSPECIFIED.);
#1221=B_SPLINE_CURVE_WITH_KNOTS('',3,(#50146,#50147,#50148,#50149,#50150,
#50151,#50152,#50153,#50154,#50155,#50156,#50157,#50158,#50159,#50160,#50161,
#50162,#50163,#50164,#50165,#50166,#50167,#50168,#50169,#50170,#50171,#50172,
#50173,#50174,#50175,#50176,#50177,#50178,#50179,#50180,#50181,#50182,#50183,
#50184,#50185,#50186,#50187,#50188,#50189,#50190,#50191,#50192,#50193,#50194,
#50195,#50196,#50197,#50198,#50199,#50200,#50201,#50202,#50203,#50204,#50205,
#50206,#50207,#50208,#50209,#50210,#50211,#50212,#50213,#50214,#50215,#50216,
#50217,#50218,#50219,#50220,#50221,#50222,#50223,#50224,#50225,#50226,#50227,
#50228,#50229,#50230,#50231,#50232,#50233,#50234,#50235,#50236),
 .UNSPECIFIED.,.F.,.F.,(4,3,3,3,3,3,3,3,3,3,3,3,3,3,3,3,3,3,3,3,3,3,3,3,
3,3,3,3,3,3,4),(0.,0.0253750087516075,0.0514203072172438,0.0779567024559424,
0.0899762332180016,0.0968038780381036,0.10264843024679,0.129953053284425,
0.157704773943122,0.18420644773905,0.195897666391424,0.201348497446843,
0.206600974226724,0.235231090538335,0.263711469126833,0.291580637154729,
0.307940047672921,0.312151253621455,0.340175922185425,0.369258810210864,
0.398694834915773,0.418024381232026,0.42320553295956,0.428148997028943,
0.459444549133158,0.482916213211318,0.491343671374895,0.498388182075807,
0.528903373982295,0.5533312054458,0.566847306048075),.UNSPECIFIED.);
#1222=B_SPLINE_CURVE_WITH_KNOTS('',3,(#50237,#50238,#50239,#50240,#50241,
#50242,#50243,#50244,#50245,#50246,#50247,#50248,#50249,#50250,#50251,#50252,
#50253,#50254,#50255,#50256,#50257,#50258,#50259,#50260,#50261),
 .UNSPECIFIED.,.F.,.F.,(4,3,3,3,3,3,3,3,4),(-10.1321597128207,-9.86460893405002,
-8.87814804064502,-7.89168714724002,-6.90522625383502,-5.91876536043002,
-4.93230446702501,-3.94584357362001,-3.84897440564113),.UNSPECIFIED.);
#1223=B_SPLINE_CURVE_WITH_KNOTS('',3,(#50486,#50487,#50488,#50489,#50490,
#50491,#50492,#50493,#50494,#50495,#50496,#50497,#50498,#50499,#50500,#50501,
#50502,#50503,#50504,#50505,#50506,#50507,#50508,#50509,#50510),
 .UNSPECIFIED.,.F.,.F.,(4,3,3,3,3,3,3,3,4),(7.59274844815666,7.89168714724002,
8.87814804064502,9.86460893405003,10.851069827455,11.83753072086,12.823991614265,
13.81045250767,13.8759337553362),.UNSPECIFIED.);
#1224=B_SPLINE_CURVE_WITH_KNOTS('',3,(#50511,#50512,#50513,#50514,#50515,
#50516,#50517,#50518,#50519,#50520,#50521,#50522,#50523,#50524,#50525,#50526,
#50527,#50528,#50529,#50530,#50531,#50532,#50533,#50534,#50535,#50536,#50537,
#50538,#50539,#50540,#50541,#50542,#50543,#50544,#50545,#50546,#50547,#50548,
#50549,#50550,#50551,#50552,#50553,#50554,#50555,#50556,#50557,#50558,#50559,
#50560,#50561,#50562,#50563,#50564,#50565,#50566,#50567,#50568,#50569,#50570,
#50571,#50572,#50573,#50574,#50575,#50576,#50577,#50578,#50579,#50580,#50581,
#50582,#50583,#50584,#50585,#50586,#50587,#50588,#50589,#50590,#50591,#50592,
#50593,#50594,#50595,#50596,#50597,#50598),.UNSPECIFIED.,.F.,.F.,(4,3,3,
3,3,3,3,3,3,3,3,3,3,3,3,3,3,3,3,3,3,3,3,3,3,3,3,3,3,4),(0.,0.0297343797035864,
0.060120761877283,0.0891403097401323,0.114532414120125,0.120626668186271,
0.150381698992516,0.17997034368319,0.208047043957412,0.230390900373193,
0.234467387186734,0.263372265983406,0.292277144780078,0.32121640004702,
0.336017014955494,0.340284508571086,0.34459204647613,0.372696730262498,
0.400818675119593,0.428516484798209,0.439577058767134,0.445404835481582,
0.450327801888399,0.477288765031749,0.497473133419461,0.505236404100872,
0.511959471749983,0.53790833305976,0.558026238582597,0.56924861039945),
 .UNSPECIFIED.);
#1225=B_SPLINE_CURVE_WITH_KNOTS('',3,(#50601,#50602,#50603,#50604,#50605,
#50606,#50607,#50608,#50609,#50610,#50611,#50612,#50613,#50614,#50615,#50616,
#50617,#50618,#50619,#50620,#50621,#50622,#50623,#50624,#50625,#50626,#50627,
#50628,#50629,#50630,#50631,#50632,#50633,#50634,#50635,#50636,#50637,#50638,
#50639,#50640,#50641,#50642,#50643,#50644,#50645,#50646,#50647,#50648,#50649,
#50650,#50651,#50652,#50653,#50654,#50655,#50656,#50657,#50658,#50659,#50660,
#50661,#50662,#50663,#50664,#50665,#50666,#50667,#50668,#50669,#50670,#50671,
#50672,#50673,#50674,#50675,#50676,#50677,#50678,#50679,#50680,#50681,#50682,
#50683,#50684,#50685,#50686,#50687,#50688,#50689,#50690,#50691,#50692,#50693,
#50694),.UNSPECIFIED.,.F.,.F.,(4,3,3,3,3,3,3,3,3,3,3,3,3,3,3,3,3,3,3,3,
3,3,3,3,3,3,3,3,3,3,3,4),(-0.569248610399439,-0.54356321026788,-0.51725177755219,
-0.510354554433286,-0.504796969238609,-0.477731405971173,-0.456105549235436,
-0.448989007169752,-0.44252634525638,-0.41479354371395,-0.386635764628684,
-0.358697147124577,-0.345203998364752,-0.340863871144016,-0.336326749475397,
-0.307401033120815,-0.304724552085278,-0.27693747898326,-0.248513803621531,
-0.232656005969356,-0.228221175977861,-0.199230005786307,-0.169667310992576,
-0.139872005633123,-0.124084622535551,-0.117720237608985,-0.113355273030534,
-0.0828138353231538,-0.052246421283799,-0.0222710285652406,-0.0135729408525455,
0.),.UNSPECIFIED.);
#1226=B_SPLINE_CURVE_WITH_KNOTS('',3,(#50695,#50696,#50697,#50698,#50699,
#50700,#50701,#50702,#50703,#50704,#50705,#50706,#50707,#50708,#50709,#50710,
#50711,#50712,#50713,#50714,#50715,#50716,#50717,#50718,#50719,#50720,#50721,
#50722,#50723,#50724,#50725,#50726,#50727,#50728,#50729,#50730,#50731,#50732,
#50733,#50734,#50735,#50736,#50737,#50738,#50739,#50740,#50741,#50742,#50743,
#50744,#50745,#50746,#50747,#50748,#50749,#50750,#50751,#50752,#50753,#50754,
#50755,#50756,#50757,#50758,#50759,#50760,#50761,#50762,#50763,#50764,#50765,
#50766,#50767,#50768,#50769,#50770,#50771,#50772,#50773,#50774,#50775,#50776,
#50777,#50778,#50779,#50780,#50781,#50782,#50783,#50784,#50785,#50786,#50787,
#50788,#50789,#50790,#50791),.UNSPECIFIED.,.F.,.F.,(4,3,3,3,3,3,3,3,3,3,
3,3,3,3,3,3,3,3,3,3,3,3,3,3,3,3,3,3,3,3,3,3,4),(-0.566847306048084,-0.536659061903649,
-0.506054167513983,-0.49735931415594,-0.490469774907708,-0.46032717525434,
-0.437299554635119,-0.425273742105126,-0.42037664994689,-0.390957260822939,
-0.362078927205336,-0.333750616169337,-0.319339514702147,-0.312267662800037,
-0.308232039095118,-0.280241121737425,-0.276106210300576,-0.247648675773662,
-0.218090819684273,-0.209492296602851,-0.204738459070877,-0.200614645085577,
-0.172781389578512,-0.145026433045361,-0.117750656382618,-0.10443005271711,
-0.100025234036307,-0.0958388284225397,-0.0691738510173895,-0.0429555684736812,
-0.0175134533592336,-0.0111858270585534,0.),.UNSPECIFIED.);
#1227=B_SPLINE_CURVE_WITH_KNOTS('',3,(#50793,#50794,#50795,#50796,#50797,
#50798,#50799,#50800,#50801,#50802,#50803),.UNSPECIFIED.,.F.,.F.,(4,1,1,
1,1,1,1,1,4),(15.7079632679489,15.8048324359278,16.7912933293328,17.7777542227378,
18.7642151161429,19.7506760095479,20.7371369029529,21.7235977963579,21.9911485751285),
 .UNSPECIFIED.);
#1228=B_SPLINE_CURVE_WITH_KNOTS('',3,(#50804,#50805,#50806,#50807,#50808,
#50809,#50810,#50811,#50812,#50813),.UNSPECIFIED.,.F.,.F.,(4,1,1,1,1,1,
1,4),(15.7079632679489,16.3713219137819,17.3577828071869,18.3442437005919,
19.3307045939969,20.3171654874019,21.3036263808069,21.9911485751285),
 .UNSPECIFIED.);
#1229=B_SPLINE_CURVE_WITH_KNOTS('',3,(#51038,#51039,#51040,#51041,#51042,
#51043,#51044,#51045,#51046,#51047,#51048,#51049,#51050,#51051,#51052,#51053,
#51054,#51055,#51056,#51057,#51058,#51059,#51060,#51061,#51062,#51063,#51064,
#51065,#51066,#51067,#51068,#51069,#51070,#51071,#51072,#51073,#51074,#51075,
#51076,#51077,#51078,#51079,#51080,#51081,#51082,#51083,#51084,#51085,#51086,
#51087,#51088,#51089,#51090,#51091,#51092,#51093,#51094,#51095,#51096,#51097,
#51098,#51099,#51100,#51101,#51102,#51103,#51104,#51105,#51106,#51107,#51108,
#51109,#51110,#51111,#51112,#51113,#51114,#51115,#51116,#51117,#51118,#51119,
#51120,#51121,#51122,#51123,#51124,#51125,#51126,#51127,#51128),
 .UNSPECIFIED.,.F.,.F.,(4,3,3,3,3,3,3,3,3,3,3,3,3,3,3,3,3,3,3,3,3,3,3,3,
3,3,3,3,3,3,4),(0.,0.0253749761808373,0.0514202453857712,0.0779566483534038,
0.0899762183904566,0.0968038784409555,0.102648429733812,0.129953030321501,
0.157704740391969,0.184206422575685,0.195897654370316,0.20134852299372,
0.206600979641336,0.235231099301492,0.263711469126832,0.291580654157613,
0.307940063613124,0.312151264914525,0.340175958120619,0.369258857874792,
0.398694885878799,0.418024425824675,0.423205607838508,0.428149011920458,
0.459444560301794,0.482916221587795,0.491343691753009,0.498388187388185,
0.528903379110968,0.553331205445801,0.566847306048077),.UNSPECIFIED.);
#1230=B_SPLINE_CURVE_WITH_KNOTS('',3,(#51129,#51130,#51131,#51132,#51133,
#51134,#51135,#51136,#51137,#51138,#51139,#51140,#51141,#51142,#51143,#51144,
#51145,#51146,#51147,#51148,#51149,#51150,#51151,#51152,#51153),
 .UNSPECIFIED.,.F.,.F.,(4,3,3,3,3,3,3,3,4),(-10.1321597128207,-9.86460893405003,
-8.87814804064503,-7.89168714724002,-6.90522625383502,-5.91876536043002,
-4.93230446702501,-3.94584357362001,-3.84897440564112),.UNSPECIFIED.);
#1231=B_SPLINE_CURVE_WITH_KNOTS('',3,(#51378,#51379,#51380,#51381,#51382,
#51383,#51384,#51385,#51386,#51387,#51388,#51389,#51390,#51391,#51392,#51393,
#51394,#51395,#51396,#51397,#51398,#51399,#51400,#51401,#51402),
 .UNSPECIFIED.,.F.,.F.,(4,3,3,3,3,3,3,3,4),(7.59274844815664,7.89168714724002,
8.87814804064502,9.86460893405003,10.851069827455,11.83753072086,12.823991614265,
13.81045250767,13.8759337553362),.UNSPECIFIED.);
#1232=B_SPLINE_CURVE_WITH_KNOTS('',3,(#51403,#51404,#51405,#51406,#51407,
#51408,#51409,#51410,#51411,#51412,#51413,#51414,#51415,#51416,#51417,#51418,
#51419,#51420,#51421,#51422,#51423,#51424,#51425,#51426,#51427,#51428,#51429,
#51430,#51431,#51432,#51433,#51434,#51435,#51436,#51437,#51438,#51439,#51440,
#51441,#51442,#51443,#51444,#51445,#51446,#51447,#51448,#51449,#51450,#51451,
#51452,#51453,#51454,#51455,#51456,#51457,#51458,#51459,#51460,#51461,#51462,
#51463,#51464,#51465,#51466,#51467,#51468,#51469,#51470,#51471,#51472,#51473,
#51474,#51475,#51476,#51477,#51478,#51479,#51480,#51481,#51482,#51483,#51484,
#51485,#51486,#51487,#51488,#51489,#51490),.UNSPECIFIED.,.F.,.F.,(4,3,3,
3,3,3,3,3,3,3,3,3,3,3,3,3,3,3,3,3,3,3,3,3,3,3,3,3,3,4),(0.,0.0297343552567438,
0.0601207256243431,0.0891402780188099,0.114532386363968,0.120626668225237,
0.150381699187288,0.179970351010139,0.208047049452624,0.230390915983779,
0.234467415790057,0.263372280285067,0.292277144780078,0.321216399233671,
0.336017014192979,0.340284510578769,0.344592048040137,0.372696731227283,
0.400818676768978,0.428516493390579,0.439577089903316,0.445404908685826,
0.450327814198675,0.477288785913009,0.497473149080406,0.505236433644848,
0.511959475796908,0.537908351627998,0.558026238582596,0.569248610399449),
 .UNSPECIFIED.);
#1233=B_SPLINE_CURVE_WITH_KNOTS('',3,(#51551,#51552,#51553,#51554,#51555,
#51556,#51557,#51558,#51559,#51560),.UNSPECIFIED.,.F.,.F.,(4,3,3,4),(-4.09293042013064,
-3.99009315480002,-2.99256986610002,-2.06773127522702),.UNSPECIFIED.);
#1234=B_SPLINE_CURVE_WITH_KNOTS('',3,(#51563,#51564,#51565,#51566,#51567,
#51568,#51569,#51570,#51571,#51572),.UNSPECIFIED.,.F.,.F.,(4,3,3,4),(0.,
0.49876164434999,0.997523288699981,1.11639350868703),.UNSPECIFIED.);
#1235=B_SPLINE_CURVE_WITH_KNOTS('',3,(#51577,#51578,#51579,#51580,#51581,
#51582,#51583,#51584,#51585,#51586,#51587,#51588,#51589,#51590,#51591,#51592,
#51593,#51594,#51595,#51596,#51597,#51598),.UNSPECIFIED.,.F.,.F.,(4,3,3,
3,3,3,3,4),(-10.3761157273102,-9.97523288700005,-8.97770959830005,-7.98018630960004,
-6.98266302090004,-5.98513973220003,-4.98761644350003,-4.09293042013064),
 .UNSPECIFIED.);
#1236=B_SPLINE_CURVE_WITH_KNOTS('',3,(#51599,#51600,#51601,#51602,#51603,
#51604,#51605,#51606,#51607,#51608,#51609,#51610,#51611,#51612,#51613,#51614,
#51615,#51616,#51617,#51618,#51619,#51620),.UNSPECIFIED.,.F.,.F.,(4,3,3,
3,3,3,3,4),(1.11639350868703,1.99504657739999,2.9925698661,3.9900931548,
4.98761644350001,5.98513973220002,6.98266302090003,7.39957881586659),
 .UNSPECIFIED.);
#1237=B_SPLINE_CURVE_WITH_KNOTS('',3,(#51625,#51626,#51627,#51628,#51629,
#51630,#51631,#51632,#51633,#51634,#51635,#51636,#51637,#51638,#51639,#51640,
#51641,#51642,#51643,#51644,#51645,#51646),.UNSPECIFIED.,.F.,.F.,(4,3,3,
3,3,3,3,4),(-16.6593010344898,-15.9603726192001,-14.9628493305001,-13.9653260418001,
-12.9678027531001,-11.9702794644001,-10.9727561757001,-10.3761157273102),
 .UNSPECIFIED.);
#1238=B_SPLINE_CURVE_WITH_KNOTS('',3,(#51647,#51648,#51649,#51650,#51651,
#51652,#51653,#51654,#51655,#51656,#51657,#51658,#51659,#51660,#51661,#51662,
#51663,#51664,#51665,#51666,#51667,#51668),.UNSPECIFIED.,.F.,.F.,(4,3,3,
3,3,3,3,4),(7.39957881586659,7.98018630960004,8.97770959830006,9.97523288700007,
10.9727561757001,11.9702794644001,12.9678027531001,13.6827641230462),
 .UNSPECIFIED.);
#1239=B_SPLINE_CURVE_WITH_KNOTS('',3,(#51673,#51674,#51675,#51676,#51677,
#51678,#51679,#51680,#51681,#51682,#51683,#51684,#51685,#51686,#51687,#51688,
#51689,#51690,#51691,#51692,#51693,#51694),.UNSPECIFIED.,.F.,.F.,(4,3,3,
3,3,3,3,4),(-22.9424863416694,-21.9455123514001,-20.9479890627001,-19.9504657740001,
-18.9529424853001,-17.9554191966001,-16.9578959079001,-16.6593010344898),
 .UNSPECIFIED.);
#1240=B_SPLINE_CURVE_WITH_KNOTS('',3,(#51695,#51696,#51697,#51698,#51699,
#51700,#51701,#51702,#51703,#51704,#51705,#51706,#51707,#51708,#51709,#51710,
#51711,#51712,#51713,#51714,#51715,#51716,#51717,#51718,#51719),
 .UNSPECIFIED.,.F.,.F.,(4,3,3,3,3,3,3,3,4),(13.6827641230462,13.9653260418001,
14.9628493305001,15.9603726192001,16.9578959079001,17.9554191966001,18.9529424853001,
19.9504657740001,19.9659494302258),.UNSPECIFIED.);
#1241=B_SPLINE_CURVE_WITH_KNOTS('',3,(#51724,#51725,#51726,#51727,#51728,
#51729,#51730,#51731,#51732,#51733,#51734,#51735,#51736,#51737,#51738,#51739,
#51740,#51741,#51742,#51743,#51744,#51745),.UNSPECIFIED.,.F.,.F.,(4,3,3,
3,3,3,3,4),(-29.225671648849,-28.9281753723002,-27.9306520836002,-26.9331287949001,
-25.9356055062001,-24.9380822175001,-23.9405589288001,-22.9424863416694),
 .UNSPECIFIED.);
#1242=B_SPLINE_CURVE_WITH_KNOTS('',3,(#51746,#51747,#51748,#51749,#51750,
#51751,#51752,#51753,#51754,#51755,#51756,#51757,#51758,#51759,#51760,#51761,
#51762,#51763,#51764,#51765,#51766,#51767),.UNSPECIFIED.,.F.,.F.,(4,3,3,
3,3,3,3,4),(19.9659494302258,20.9479890627001,21.9455123514001,22.9430356401001,
23.9405589288002,24.9380822175002,25.9356055062002,26.2491347374054),
 .UNSPECIFIED.);
#1243=B_SPLINE_CURVE_WITH_KNOTS('',3,(#51772,#51773,#51774,#51775,#51776,
#51777,#51778,#51779,#51780,#51781,#51782,#51783,#51784,#51785,#51786,#51787,
#51788,#51789,#51790,#51791,#51792,#51793),.UNSPECIFIED.,.F.,.F.,(4,3,3,
3,3,3,3,4),(-35.5088569560286,-34.9133151045002,-33.9157918158002,-32.9182685271002,
-31.9207452384002,-30.9232219497002,-29.9256986610002,-29.225671648849),
 .UNSPECIFIED.);
#1244=B_SPLINE_CURVE_WITH_KNOTS('',3,(#51794,#51795,#51796,#51797,#51798,
#51799,#51800,#51801,#51802,#51803,#51804,#51805,#51806,#51807,#51808,#51809,
#51810,#51811,#51812,#51813,#51814,#51815),.UNSPECIFIED.,.F.,.F.,(4,3,3,
3,3,3,3,4),(26.2491347374054,26.9331287949002,27.9306520836002,28.9281753723002,
29.9256986610002,30.9232219497002,31.9207452384002,32.532320044585),
 .UNSPECIFIED.);
#1245=B_SPLINE_CURVE_WITH_KNOTS('',3,(#51820,#51821,#51822,#51823,#51824,
#51825,#51826,#51827,#51828,#51829,#51830,#51831,#51832,#51833,#51834,#51835,
#51836,#51837,#51838,#51839,#51840,#51841),.UNSPECIFIED.,.F.,.F.,(4,3,3,
3,3,3,3,4),(-41.7920422632082,-40.8984548367002,-39.9009315480002,-38.9034082593002,
-37.9058849706002,-36.9083616819002,-35.9108383932002,-35.5088569560286),
 .UNSPECIFIED.);
#1246=B_SPLINE_CURVE_WITH_KNOTS('',3,(#51842,#51843,#51844,#51845,#51846,
#51847,#51848,#51849,#51850,#51851,#51852,#51853,#51854,#51855,#51856,#51857,
#51858,#51859,#51860,#51861,#51862,#51863),.UNSPECIFIED.,.F.,.F.,(4,3,3,
3,3,3,3,4),(32.532320044585,32.9182685271002,33.9157918158002,34.9133151045002,
35.9108383932002,36.9083616819002,37.9058849706002,38.8155053517645),
 .UNSPECIFIED.);
#1247=B_SPLINE_CURVE_WITH_KNOTS('',3,(#51868,#51869,#51870,#51871,#51872,
#51873,#51874,#51875,#51876,#51877,#51878,#51879,#51880,#51881,#51882,#51883,
#51884,#51885,#51886,#51887,#51888,#51889,#51890,#51891,#51892),
 .UNSPECIFIED.,.F.,.F.,(4,3,3,3,3,3,3,3,4),(-48.0752275703878,-47.8811178576003,
-46.8835945689003,-45.8860712802002,-44.8885479915002,-43.8910247028002,
-42.8935014141002,-41.8959781254002,-41.7920422632082),.UNSPECIFIED.);
#1248=B_SPLINE_CURVE_WITH_KNOTS('',3,(#51893,#51894,#51895,#51896,#51897,
#51898,#51899,#51900,#51901,#51902,#51903,#51904,#51905,#51906,#51907,#51908,
#51909,#51910,#51911,#51912,#51913,#51914,#51915,#51916,#51917),
 .UNSPECIFIED.,.F.,.F.,(4,3,3,3,3,3,3,3,4),(38.8155053517645,38.9034082593002,
39.9009315480002,40.8984548367002,41.8959781254002,42.8935014141002,43.8910247028003,
44.8885479915003,45.0986906589441),.UNSPECIFIED.);
#1249=B_SPLINE_CURVE_WITH_KNOTS('',3,(#51922,#51923,#51924,#51925,#51926,
#51927,#51928,#51929,#51930,#51931,#51932,#51933,#51934,#51935,#51936,#51937,
#51938,#51939,#51940,#51941,#51942,#51943),.UNSPECIFIED.,.F.,.F.,(4,3,3,
3,3,3,3,4),(-54.3584128775673,-53.8662575898003,-52.8687343011003,-51.8712110124003,
-50.8736877237003,-49.8761644350003,-48.8786411463003,-48.0752275703878),
 .UNSPECIFIED.);
#1250=B_SPLINE_CURVE_WITH_KNOTS('',3,(#51944,#51945,#51946,#51947,#51948,
#51949,#51950,#51951,#51952,#51953,#51954,#51955,#51956,#51957,#51958,#51959,
#51960,#51961,#51962,#51963,#51964,#51965),.UNSPECIFIED.,.F.,.F.,(4,3,3,
3,3,3,3,4),(45.0986906589441,45.8860712802003,46.8835945689003,47.8811178576003,
48.8786411463002,49.8761644350002,50.8736877237002,51.3818759661237),
 .UNSPECIFIED.);
#1251=B_SPLINE_CURVE_WITH_KNOTS('',3,(#51970,#51971,#51972,#51973,#51974,
#51975,#51976,#51977,#51978,#51979,#51980,#51981,#51982,#51983,#51984,#51985,
#51986,#51987,#51988,#51989,#51990,#51991),.UNSPECIFIED.,.F.,.F.,(4,3,3,
3,3,3,3,4),(-60.6415981847469,-59.8513973220003,-58.8538740333003,-57.8563507446003,
-56.8588274559003,-55.8613041672003,-54.8637808785003,-54.3584128775673),
 .UNSPECIFIED.);
#1252=B_SPLINE_CURVE_WITH_KNOTS('',3,(#51992,#51993,#51994,#51995,#51996,
#51997,#51998,#51999,#52000,#52001,#52002,#52003,#52004,#52005,#52006,#52007,
#52008,#52009,#52010,#52011,#52012,#52013),.UNSPECIFIED.,.F.,.F.,(4,3,3,
3,3,3,3,4),(51.3818759661237,51.8712110124002,52.8687343011003,53.8662575898003,
54.8637808785003,55.8613041672003,56.8588274559003,57.6650612733033),
 .UNSPECIFIED.);
#1253=B_SPLINE_CURVE_WITH_KNOTS('',3,(#52018,#52019,#52020,#52021,#52022,
#52023,#52024,#52025,#52026,#52027,#52028,#52029,#52030,#52031,#52032,#52033,
#52034,#52035,#52036,#52037,#52038,#52039,#52040,#52041,#52042),
 .UNSPECIFIED.,.F.,.F.,(4,3,3,3,3,3,3,3,4),(-66.9247834919265,-66.8340603429004,
-65.8365370542004,-64.8390137655004,-63.8414904768003,-62.8439671881003,
-61.8464438994003,-60.8489206107003,-60.6415981847469),.UNSPECIFIED.);
#1254=B_SPLINE_CURVE_WITH_KNOTS('',3,(#52043,#52044,#52045,#52046,#52047,
#52048,#52049,#52050,#52051,#52052,#52053,#52054,#52055,#52056,#52057,#52058,
#52059,#52060,#52061,#52062,#52063,#52064,#52065,#52066,#52067),
 .UNSPECIFIED.,.F.,.F.,(4,3,3,3,3,3,3,3,4),(57.6650612733033,57.8563507446003,
58.8538740333003,59.8513973220003,60.8489206107003,61.8464438994003,62.8439671881003,
63.8414904768003,63.9482465804829),.UNSPECIFIED.);
#1255=B_SPLINE_CURVE_WITH_KNOTS('',3,(#52072,#52073,#52074,#52075,#52076,
#52077,#52078,#52079,#52080,#52081,#52082,#52083,#52084,#52085,#52086,#52087,
#52088,#52089,#52090,#52091,#52092,#52093),.UNSPECIFIED.,.F.,.F.,(4,3,3,
3,3,3,3,4),(-73.2079687991061,-72.8192000751004,-71.8216767864004,-70.8241534977004,
-69.8266302090004,-68.8291069203004,-67.8315836316004,-66.9247834919265),
 .UNSPECIFIED.);
#1256=B_SPLINE_CURVE_WITH_KNOTS('',3,(#52094,#52095,#52096,#52097,#52098,
#52099,#52100,#52101,#52102,#52103,#52104,#52105,#52106,#52107,#52108,#52109,
#52110,#52111,#52112,#52113,#52114,#52115),.UNSPECIFIED.,.F.,.F.,(4,3,3,
3,3,3,3,4),(63.9482465804829,64.8390137655003,65.8365370542003,66.8340603429004,
67.8315836316004,68.8291069203004,69.8266302090004,70.2314318876625),
 .UNSPECIFIED.);
#1257=B_SPLINE_CURVE_WITH_KNOTS('',3,(#52120,#52121,#52122,#52123,#52124,
#52125,#52126,#52127,#52128,#52129,#52130,#52131,#52132,#52133,#52134,#52135,
#52136,#52137,#52138,#52139,#52140,#52141),.UNSPECIFIED.,.F.,.F.,(4,3,3,
3,3,3,3,4),(-79.4911541062857,-78.8043398073004,-77.8068165186004,-76.8092932299004,
-75.8117699412004,-74.8142466525004,-73.8167233638004,-73.2079687991061),
 .UNSPECIFIED.);
#1258=B_SPLINE_CURVE_WITH_KNOTS('',3,(#52142,#52143,#52144,#52145,#52146,
#52147,#52148,#52149,#52150,#52151,#52152,#52153,#52154,#52155,#52156,#52157,
#52158,#52159,#52160,#52161,#52162,#52163),.UNSPECIFIED.,.F.,.F.,(4,3,3,
3,3,3,3,4),(70.2314318876625,70.8241534977004,71.8216767864004,72.8192000751004,
73.8167233638004,74.8142466525004,75.8117699412004,76.5146171948421),
 .UNSPECIFIED.);
#1259=B_SPLINE_CURVE_WITH_KNOTS('',3,(#52168,#52169,#52170,#52171,#52172,
#52173,#52174,#52175,#52176,#52177,#52178,#52179,#52180,#52181,#52182,#52183,
#52184,#52185,#52186,#52187,#52188,#52189),.UNSPECIFIED.,.F.,.F.,(4,3,3,
3,3,3,3,4),(-85.7743394134653,-84.7894795395005,-83.7919562508005,-82.7944329621005,
-81.7969096734005,-80.7993863847005,-79.8018630960004,-79.4911541062857),
 .UNSPECIFIED.);
#1260=B_SPLINE_CURVE_WITH_KNOTS('',3,(#52190,#52191,#52192,#52193,#52194,
#52195,#52196,#52197,#52198,#52199,#52200,#52201,#52202,#52203,#52204,#52205,
#52206,#52207,#52208,#52209,#52210,#52211,#52212,#52213,#52214),
 .UNSPECIFIED.,.F.,.F.,(4,3,3,3,3,3,3,3,4),(76.5146171948421,76.8092932299004,
77.8068165186004,78.8043398073004,79.8018630960004,80.7993863847004,81.7969096734004,
82.7944329621005,82.7978025020217),.UNSPECIFIED.);
#1261=B_SPLINE_CURVE_WITH_KNOTS('',3,(#52219,#52220,#52221,#52222,#52223,
#52224,#52225,#52226,#52227,#52228,#52229,#52230,#52231,#52232,#52233,#52234,
#52235,#52236,#52237,#52238,#52239,#52240,#52241,#52242,#52243),
 .UNSPECIFIED.,.F.,.F.,(4,3,3,3,3,3,3,3,4),(-92.0575247206449,-91.7721425604005,
-90.7746192717005,-89.7770959830005,-88.7795726943005,-87.7820494056005,
-86.7845261169005,-85.7870028282005,-85.7743394134653),.UNSPECIFIED.);
#1262=B_SPLINE_CURVE_WITH_KNOTS('',3,(#52244,#52245,#52246,#52247,#52248,
#52249,#52250,#52251,#52252,#52253,#52254,#52255,#52256,#52257,#52258,#52259,
#52260,#52261,#52262,#52263,#52264,#52265),.UNSPECIFIED.,.F.,.F.,(4,3,3,
3,3,3,3,4),(82.7978025020217,83.7919562508005,84.7894795395004,85.7870028282005,
86.7845261169005,87.7820494056005,88.7795726943005,89.0809878092013),
 .UNSPECIFIED.);
#1263=B_SPLINE_CURVE_WITH_KNOTS('',3,(#52270,#52271,#52272,#52273,#52274,
#52275,#52276,#52277,#52278,#52279,#52280,#52281,#52282,#52283,#52284,#52285,
#52286,#52287,#52288,#52289,#52290,#52291),.UNSPECIFIED.,.F.,.F.,(4,3,3,
3,3,3,3,4),(-98.3407100278245,-97.7572822926005,-96.7597590039005,-95.7622357152005,
-94.7647124265005,-93.7671891378005,-92.7696658491005,-92.0575247206449),
 .UNSPECIFIED.);
#1264=B_SPLINE_CURVE_WITH_KNOTS('',3,(#52292,#52293,#52294,#52295,#52296,
#52297,#52298,#52299,#52300,#52301,#52302,#52303,#52304,#52305,#52306,#52307,
#52308,#52309,#52310,#52311,#52312,#52313),.UNSPECIFIED.,.F.,.F.,(4,3,3,
3,3,3,3,4),(89.0809878092013,89.7770959830005,90.7746192717005,91.7721425604005,
92.7696658491005,93.7671891378005,94.7647124265005,95.3641731163809),
 .UNSPECIFIED.);
#1265=B_SPLINE_CURVE_WITH_KNOTS('',3,(#52318,#52319,#52320,#52321,#52322,
#52323,#52324,#52325,#52326,#52327,#52328,#52329,#52330,#52331,#52332,#52333,
#52334,#52335,#52336,#52337,#52338,#52339),.UNSPECIFIED.,.F.,.F.,(4,3,3,
3,3,3,3,4),(-104.623895335004,-103.742422024801,-102.744898736101,-101.747375447401,
-100.749852158701,-99.7523288700005,-98.7548055813005,-98.3407100278245),
 .UNSPECIFIED.);
#1266=B_SPLINE_CURVE_WITH_KNOTS('',3,(#52340,#52341,#52342,#52343,#52344,
#52345,#52346,#52347,#52348,#52349,#52350,#52351,#52352,#52353,#52354,#52355,
#52356,#52357,#52358,#52359,#52360,#52361),.UNSPECIFIED.,.F.,.F.,(4,3,3,
3,3,3,3,4),(95.3641731163809,95.7622357152005,96.7597590039006,97.7572822926005,
98.7548055813005,99.7523288700006,100.749852158701,101.647358423561),
 .UNSPECIFIED.);
#1267=B_SPLINE_CURVE_WITH_KNOTS('',3,(#52366,#52367,#52368,#52369,#52370,
#52371,#52372,#52373,#52374,#52375,#52376,#52377,#52378,#52379,#52380,#52381,
#52382,#52383,#52384,#52385,#52386,#52387,#52388,#52389,#52390),
 .UNSPECIFIED.,.F.,.F.,(4,3,3,3,3,3,3,3,4),(-110.907080642184,-110.725085045701,
-109.727561757001,-108.730038468301,-107.732515179601,-106.734991890901,
-105.737468602201,-104.739945313501,-104.623895335004),.UNSPECIFIED.);
#1268=B_SPLINE_CURVE_WITH_KNOTS('',3,(#52391,#52392,#52393,#52394,#52395,
#52396,#52397,#52398,#52399,#52400,#52401,#52402,#52403,#52404,#52405,#52406,
#52407,#52408,#52409,#52410,#52411,#52412,#52413,#52414,#52415),
 .UNSPECIFIED.,.F.,.F.,(4,3,3,3,3,3,3,3,4),(101.647358423561,101.747375447401,
102.744898736101,103.742422024801,104.739945313501,105.737468602201,106.734991890901,
107.732515179601,107.93054373074),.UNSPECIFIED.);
#1269=B_SPLINE_CURVE_WITH_KNOTS('',3,(#52420,#52421,#52422,#52423,#52424,
#52425,#52426,#52427,#52428,#52429,#52430,#52431,#52432,#52433,#52434,#52435,
#52436,#52437,#52438,#52439,#52440,#52441),.UNSPECIFIED.,.F.,.F.,(4,3,3,
3,3,3,3,4),(-117.190265949363,-116.710224777901,-115.712701489201,-114.715178200501,
-113.717654911801,-112.720131623101,-111.722608334401,-110.907080642184),
 .UNSPECIFIED.);
#1270=B_SPLINE_CURVE_WITH_KNOTS('',3,(#52442,#52443,#52444,#52445,#52446,
#52447,#52448,#52449,#52450,#52451,#52452,#52453,#52454,#52455,#52456,#52457,
#52458,#52459,#52460,#52461,#52462,#52463),.UNSPECIFIED.,.F.,.F.,(4,3,3,
3,3,3,3,4),(107.93054373074,108.730038468301,109.727561757001,110.725085045701,
111.722608334401,112.720131623101,113.717654911801,114.21372903792),
 .UNSPECIFIED.);
#1271=B_SPLINE_CURVE_WITH_KNOTS('',3,(#52468,#52469,#52470,#52471,#52472,
#52473,#52474,#52475,#52476,#52477,#52478,#52479,#52480,#52481,#52482,#52483,
#52484,#52485,#52486,#52487,#52488,#52489),.UNSPECIFIED.,.F.,.F.,(4,3,3,
3,3,3,3,4),(-123.473451256543,-122.695364510101,-121.697841221401,-120.700317932701,
-119.702794644001,-118.705271355301,-117.707748066601,-117.190265949363),
 .UNSPECIFIED.);
#1272=B_SPLINE_CURVE_WITH_KNOTS('',3,(#52490,#52491,#52492,#52493,#52494,
#52495,#52496,#52497,#52498,#52499,#52500,#52501,#52502,#52503,#52504,#52505,
#52506,#52507,#52508,#52509,#52510,#52511),.UNSPECIFIED.,.F.,.F.,(4,3,3,
3,3,3,3,4),(114.21372903792,114.715178200501,115.712701489201,116.710224777901,
117.707748066601,118.705271355301,119.702794644001,120.496914345099),
 .UNSPECIFIED.);
#1273=B_SPLINE_CURVE_WITH_KNOTS('',3,(#52516,#52517,#52518,#52519,#52520,
#52521,#52522,#52523,#52524,#52525,#52526,#52527,#52528,#52529,#52530,#52531,
#52532,#52533,#52534,#52535,#52536,#52537,#52538,#52539,#52540),
 .UNSPECIFIED.,.F.,.F.,(4,3,3,3,3,3,3,3,4),(-129.756636563722,-129.678027531001,
-128.680504242301,-127.682980953601,-126.685457664901,-125.687934376201,
-124.690411087501,-123.692887798801,-123.473451256543),.UNSPECIFIED.);
#1274=B_SPLINE_CURVE_WITH_KNOTS('',3,(#52541,#52542,#52543,#52544,#52545,
#52546,#52547,#52548,#52549,#52550,#52551,#52552,#52553,#52554,#52555,#52556,
#52557,#52558,#52559,#52560,#52561,#52562,#52563,#52564,#52565),
 .UNSPECIFIED.,.F.,.F.,(4,3,3,3,3,3,3,3,4),(120.496914345099,120.700317932701,
121.697841221401,122.695364510101,123.692887798801,124.690411087501,125.687934376201,
126.685457664901,126.780099652279),.UNSPECIFIED.);
#1275=B_SPLINE_CURVE_WITH_KNOTS('',3,(#52570,#52571,#52572,#52573,#52574,
#52575,#52576,#52577,#52578,#52579,#52580,#52581,#52582,#52583,#52584,#52585,
#52586,#52587,#52588,#52589,#52590,#52591),.UNSPECIFIED.,.F.,.F.,(4,3,3,
3,3,3,3,4),(-136.039821870902,-135.663167263201,-134.665643974501,-133.668120685801,
-132.670597397101,-131.673074108401,-130.675550819701,-129.756636563722),
 .UNSPECIFIED.);
#1276=B_SPLINE_CURVE_WITH_KNOTS('',3,(#52592,#52593,#52594,#52595,#52596,
#52597,#52598,#52599,#52600,#52601,#52602,#52603,#52604,#52605,#52606,#52607,
#52608,#52609,#52610,#52611,#52612,#52613),.UNSPECIFIED.,.F.,.F.,(4,3,3,
3,3,3,3,4),(126.780099652279,127.682980953601,128.680504242301,129.678027531001,
130.675550819701,131.673074108401,132.670597397101,133.063284959458),
 .UNSPECIFIED.);
#1277=B_SPLINE_CURVE_WITH_KNOTS('',3,(#52618,#52619,#52620,#52621,#52622,
#52623,#52624,#52625,#52626,#52627,#52628,#52629,#52630,#52631,#52632,#52633,
#52634,#52635,#52636,#52637,#52638,#52639),.UNSPECIFIED.,.F.,.F.,(4,3,3,
3,3,3,3,4),(-142.323007178082,-141.648306995401,-140.650783706701,-139.653260418001,
-138.655737129301,-137.658213840601,-136.660690551901,-136.039821870902),
 .UNSPECIFIED.);
#1278=B_SPLINE_CURVE_WITH_KNOTS('',3,(#52640,#52641,#52642,#52643,#52644,
#52645,#52646,#52647,#52648,#52649,#52650,#52651,#52652,#52653,#52654,#52655,
#52656,#52657,#52658,#52659,#52660,#52661),.UNSPECIFIED.,.F.,.F.,(4,3,3,
3,3,3,3,4),(133.063284959458,133.668120685801,134.665643974501,135.663167263201,
136.660690551901,137.658213840601,138.655737129301,139.346470266638),
 .UNSPECIFIED.);
#1279=B_SPLINE_CURVE_WITH_KNOTS('',3,(#52666,#52667,#52668,#52669,#52670,
#52671,#52672,#52673,#52674,#52675,#52676,#52677,#52678,#52679,#52680,#52681,
#52682,#52683,#52684,#52685,#52686,#52687),.UNSPECIFIED.,.F.,.F.,(4,3,3,
3,3,3,3,4),(-148.606192485261,-147.633446727601,-146.635923438901,-145.638400150201,
-144.640876861501,-143.643353572801,-142.645830284101,-142.323007178082),
 .UNSPECIFIED.);
#1280=B_SPLINE_CURVE_WITH_KNOTS('',3,(#52688,#52689,#52690,#52691,#52692,
#52693,#52694,#52695,#52696,#52697,#52698,#52699,#52700,#52701,#52702,#52703,
#52704,#52705,#52706,#52707,#52708,#52709),.UNSPECIFIED.,.F.,.F.,(4,3,3,
3,3,3,3,4),(139.346470266638,139.653260418001,140.650783706701,141.648306995401,
142.645830284101,143.643353572801,144.640876861501,145.629655573818),
 .UNSPECIFIED.);
#1281=B_SPLINE_CURVE_WITH_KNOTS('',3,(#52714,#52715,#52716,#52717,#52718,
#52719,#52720,#52721,#52722,#52723,#52724,#52725,#52726,#52727,#52728,#52729,
#52730,#52731,#52732,#52733,#52734,#52735,#52736,#52737,#52738),
 .UNSPECIFIED.,.F.,.F.,(4,3,3,3,3,3,3,3,4),(-154.889377792441,-154.616109748501,
-153.618586459801,-152.621063171101,-151.623539882401,-150.626016593701,
-149.628493305001,-148.630970016301,-148.606192485261),.UNSPECIFIED.);
#1282=B_SPLINE_CURVE_WITH_KNOTS('',3,(#52739,#52740,#52741,#52742,#52743,
#52744,#52745,#52746,#52747,#52748,#52749,#52750,#52751,#52752,#52753,#52754,
#52755,#52756,#52757,#52758,#52759,#52760,#52761,#52762,#52763),
 .UNSPECIFIED.,.F.,.F.,(4,3,3,3,3,3,3,3,4),(145.629655573818,145.638400150201,
146.635923438901,147.633446727601,148.630970016301,149.628493305001,150.626016593701,
151.623539882401,151.912840880997),.UNSPECIFIED.);
#1283=B_SPLINE_CURVE_WITH_KNOTS('',3,(#52768,#52769,#52770,#52771,#52772,
#52773,#52774,#52775,#52776,#52777,#52778,#52779,#52780,#52781,#52782,#52783,
#52784,#52785,#52786,#52787,#52788,#52789),.UNSPECIFIED.,.F.,.F.,(4,3,3,
3,3,3,3,4),(-161.17256309962,-160.601249480701,-159.603726192001,-158.606202903301,
-157.608679614601,-156.611156325901,-155.613633037201,-154.889377792441),
 .UNSPECIFIED.);
#1284=B_SPLINE_CURVE_WITH_KNOTS('',3,(#52790,#52791,#52792,#52793,#52794,
#52795,#52796,#52797,#52798,#52799,#52800,#52801,#52802,#52803,#52804,#52805,
#52806,#52807,#52808,#52809,#52810,#52811),.UNSPECIFIED.,.F.,.F.,(4,3,3,
3,3,3,3,4),(151.912840880997,152.621063171101,153.618586459801,154.616109748501,
155.613633037201,156.611156325901,157.608679614601,158.196026188177),
 .UNSPECIFIED.);
#1285=B_SPLINE_CURVE_WITH_KNOTS('',3,(#52816,#52817,#52818,#52819,#52820,
#52821,#52822,#52823,#52824,#52825,#52826,#52827,#52828,#52829,#52830,#52831,
#52832,#52833,#52834,#52835,#52836,#52837),.UNSPECIFIED.,.F.,.F.,(4,3,3,
3,3,3,3,4),(-167.4557484068,-166.586389212901,-165.588865924201,-164.591342635501,
-163.593819346801,-162.596296058101,-161.598772769401,-161.17256309962),
 .UNSPECIFIED.);
#1286=B_SPLINE_CURVE_WITH_KNOTS('',3,(#52838,#52839,#52840,#52841,#52842,
#52843,#52844,#52845,#52846,#52847,#52848,#52849,#52850,#52851,#52852,#52853,
#52854,#52855,#52856,#52857,#52858,#52859),.UNSPECIFIED.,.F.,.F.,(4,3,3,
3,3,3,3,4),(158.196026188177,158.606202903301,159.603726192001,160.601249480701,
161.598772769401,162.596296058101,163.593819346801,164.479211495356),
 .UNSPECIFIED.);
#1287=B_SPLINE_CURVE_WITH_KNOTS('',3,(#52864,#52865,#52866,#52867,#52868,
#52869,#52870,#52871,#52872,#52873,#52874,#52875,#52876,#52877,#52878,#52879,
#52880,#52881,#52882,#52883,#52884,#52885,#52886,#52887,#52888),
 .UNSPECIFIED.,.F.,.F.,(4,3,3,3,3,3,3,3,4),(-173.738933713979,-173.569052233801,
-172.571528945101,-171.574005656401,-170.576482367701,-169.578959079001,
-168.581435790301,-167.583912501601,-167.4557484068),.UNSPECIFIED.);
#1288=B_SPLINE_CURVE_WITH_KNOTS('',3,(#52889,#52890,#52891,#52892,#52893,
#52894,#52895,#52896,#52897,#52898,#52899,#52900,#52901,#52902,#52903,#52904,
#52905,#52906,#52907,#52908,#52909,#52910,#52911,#52912,#52913),
 .UNSPECIFIED.,.F.,.F.,(4,3,3,3,3,3,3,3,4),(164.479211495356,164.591342635501,
165.588865924201,166.586389212901,167.583912501601,168.581435790301,169.578959079001,
170.576482367701,170.762396802536),.UNSPECIFIED.);
#1289=B_SPLINE_CURVE_WITH_KNOTS('',3,(#52918,#52919,#52920,#52921,#52922,
#52923,#52924,#52925,#52926,#52927,#52928,#52929,#52930,#52931,#52932,#52933,
#52934,#52935,#52936,#52937,#52938,#52939),.UNSPECIFIED.,.F.,.F.,(4,3,3,
3,3,3,3,4),(-180.022119021159,-179.554191966001,-178.556668677301,-177.559145388601,
-176.561622099901,-175.564098811201,-174.566575522501,-173.738933713979),
 .UNSPECIFIED.);
#1290=B_SPLINE_CURVE_WITH_KNOTS('',3,(#52940,#52941,#52942,#52943,#52944,
#52945,#52946,#52947,#52948,#52949,#52950,#52951,#52952,#52953,#52954,#52955,
#52956,#52957,#52958,#52959,#52960,#52961),.UNSPECIFIED.,.F.,.F.,(4,3,3,
3,3,3,3,4),(170.762396802536,171.574005656401,172.571528945101,173.569052233801,
174.566575522501,175.564098811201,176.561622099901,177.045582109715),
 .UNSPECIFIED.);
#1291=B_SPLINE_CURVE_WITH_KNOTS('',3,(#52966,#52967,#52968,#52969,#52970,
#52971,#52972,#52973,#52974,#52975,#52976,#52977,#52978,#52979,#52980,#52981,
#52982,#52983,#52984,#52985,#52986,#52987),.UNSPECIFIED.,.F.,.F.,(4,3,3,
3,3,3,3,4),(-186.305304328338,-185.539331698201,-184.541808409501,-183.544285120801,
-182.546761832101,-181.549238543401,-180.551715254701,-180.022119021159),
 .UNSPECIFIED.);
#1292=B_SPLINE_CURVE_WITH_KNOTS('',3,(#52988,#52989,#52990,#52991,#52992,
#52993,#52994,#52995,#52996,#52997,#52998,#52999,#53000,#53001,#53002,#53003,
#53004,#53005,#53006,#53007,#53008,#53009),.UNSPECIFIED.,.F.,.F.,(4,3,3,
3,3,3,3,4),(177.045582109715,177.559145388601,178.556668677301,179.554191966001,
180.551715254701,181.549238543401,182.546761832101,183.328767416895),
 .UNSPECIFIED.);
#1293=B_SPLINE_CURVE_WITH_KNOTS('',3,(#53014,#53015,#53016,#53017,#53018,
#53019,#53020,#53021,#53022,#53023,#53024,#53025,#53026,#53027,#53028,#53029,
#53030,#53031,#53032,#53033,#53034,#53035,#53036,#53037,#53038),
 .UNSPECIFIED.,.F.,.F.,(4,3,3,3,3,3,3,3,4),(-192.588489635518,-192.521994719101,
-191.524471430401,-190.526948141701,-189.529424853001,-188.531901564301,
-187.534378275601,-186.536854986901,-186.305304328338),.UNSPECIFIED.);
#1294=B_SPLINE_CURVE_WITH_KNOTS('',3,(#53039,#53040,#53041,#53042,#53043,
#53044,#53045,#53046,#53047,#53048,#53049,#53050,#53051,#53052,#53053,#53054,
#53055,#53056,#53057,#53058,#53059,#53060,#53061,#53062,#53063),
 .UNSPECIFIED.,.F.,.F.,(4,3,3,3,3,3,3,3,4),(183.328767416895,183.544285120801,
184.541808409501,185.539331698201,186.536854986901,187.534378275601,188.531901564301,
189.529424853001,189.611952724075),.UNSPECIFIED.);
#1295=B_SPLINE_CURVE_WITH_KNOTS('',3,(#53068,#53069,#53070,#53071,#53072,
#53073,#53074,#53075,#53076,#53077,#53078,#53079,#53080,#53081,#53082,#53083,
#53084,#53085,#53086,#53087,#53088,#53089),.UNSPECIFIED.,.F.,.F.,(4,3,3,
3,3,3,3,4),(-198.871674942698,-198.507134451301,-197.509611162601,-196.512087873901,
-195.514564585201,-194.517041296501,-193.519518007801,-192.588489635518),
 .UNSPECIFIED.);
#1296=B_SPLINE_CURVE_WITH_KNOTS('',3,(#53090,#53091,#53092,#53093,#53094,
#53095,#53096,#53097,#53098,#53099,#53100,#53101,#53102,#53103,#53104,#53105,
#53106,#53107,#53108,#53109,#53110,#53111),.UNSPECIFIED.,.F.,.F.,(4,3,3,
3,3,3,3,4),(189.611952724075,190.526948141701,191.524471430401,192.521994719101,
193.519518007801,194.517041296501,195.514564585201,195.895138031254),
 .UNSPECIFIED.);
#1297=B_SPLINE_CURVE_WITH_KNOTS('',3,(#53116,#53117,#53118,#53119,#53120,
#53121,#53122,#53123,#53124,#53125,#53126,#53127,#53128,#53129,#53130,#53131,
#53132,#53133,#53134,#53135,#53136,#53137),.UNSPECIFIED.,.F.,.F.,(4,3,3,
3,3,3,3,4),(-205.154860249877,-204.492274183501,-203.494750894801,-202.497227606101,
-201.499704317401,-200.502181028701,-199.504657740001,-198.871674942698),
 .UNSPECIFIED.);
#1298=B_SPLINE_CURVE_WITH_KNOTS('',3,(#53138,#53139,#53140,#53141,#53142,
#53143,#53144,#53145,#53146,#53147,#53148,#53149,#53150,#53151,#53152,#53153,
#53154,#53155,#53156,#53157,#53158,#53159),.UNSPECIFIED.,.F.,.F.,(4,3,3,
3,3,3,3,4),(195.895138031254,196.512087873901,197.509611162601,198.507134451301,
199.504657740001,200.502181028701,201.499704317401,202.178323338434),
 .UNSPECIFIED.);
#1299=B_SPLINE_CURVE_WITH_KNOTS('',3,(#53164,#53165,#53166,#53167,#53168,
#53169,#53170,#53171,#53172,#53173,#53174,#53175,#53176,#53177,#53178,#53179,
#53180,#53181,#53182,#53183,#53184,#53185),.UNSPECIFIED.,.F.,.F.,(4,3,3,
3,3,3,3,4),(-211.438045557057,-210.477413915701,-209.479890627001,-208.482367338301,
-207.484844049601,-206.487320760901,-205.489797472201,-205.154860249877),
 .UNSPECIFIED.);
#1300=B_SPLINE_CURVE_WITH_KNOTS('',3,(#53186,#53187,#53188,#53189,#53190,
#53191,#53192,#53193,#53194,#53195,#53196,#53197,#53198,#53199,#53200,#53201,
#53202,#53203,#53204,#53205,#53206,#53207),.UNSPECIFIED.,.F.,.F.,(4,3,3,
3,3,3,3,4),(202.178323338434,202.497227606101,203.494750894801,204.492274183501,
205.489797472201,206.487320760901,207.484844049601,208.461508645613),
 .UNSPECIFIED.);
#1301=B_SPLINE_CURVE_WITH_KNOTS('',3,(#53212,#53213,#53214,#53215,#53216,
#53217,#53218,#53219,#53220,#53221,#53222,#53223,#53224,#53225,#53226,#53227,
#53228,#53229,#53230,#53231,#53232,#53233,#53234,#53235,#53236),
 .UNSPECIFIED.,.F.,.F.,(4,3,3,3,3,3,3,3,4),(-217.721230864236,-217.460076936601,
-216.462553647901,-215.465030359201,-214.467507070501,-213.469983781801,
-212.472460493101,-211.474937204401,-211.438045557057),.UNSPECIFIED.);
#1302=B_SPLINE_CURVE_WITH_KNOTS('',3,(#53237,#53238,#53239,#53240,#53241,
#53242,#53243,#53244,#53245,#53246,#53247,#53248,#53249,#53250,#53251,#53252,
#53253,#53254,#53255,#53256,#53257,#53258,#53259,#53260,#53261),
 .UNSPECIFIED.,.F.,.F.,(4,3,3,3,3,3,3,3,4),(208.461508645613,208.482367338301,
209.479890627001,210.477413915701,211.474937204401,212.472460493101,213.469983781801,
214.467507070501,214.744693952793),.UNSPECIFIED.);
#1303=B_SPLINE_CURVE_WITH_KNOTS('',3,(#53266,#53267,#53268,#53269,#53270,
#53271,#53272,#53273,#53274,#53275,#53276,#53277,#53278,#53279,#53280,#53281,
#53282,#53283,#53284,#53285,#53286,#53287),.UNSPECIFIED.,.F.,.F.,(4,3,3,
3,3,3,3,4),(-224.004416171416,-223.445216668801,-222.447693380101,-221.450170091401,
-220.452646802701,-219.455123514001,-218.457600225301,-217.721230864236),
 .UNSPECIFIED.);
#1304=B_SPLINE_CURVE_WITH_KNOTS('',3,(#53288,#53289,#53290,#53291,#53292,
#53293,#53294,#53295,#53296,#53297,#53298,#53299,#53300,#53301,#53302,#53303,
#53304,#53305,#53306,#53307,#53308,#53309),.UNSPECIFIED.,.F.,.F.,(4,3,3,
3,3,3,3,4),(214.744693952793,215.465030359201,216.462553647901,217.460076936601,
218.457600225301,219.455123514001,220.452646802701,221.027879259972),
 .UNSPECIFIED.);
#1305=B_SPLINE_CURVE_WITH_KNOTS('',3,(#53314,#53315,#53316,#53317,#53318,
#53319,#53320,#53321,#53322,#53323,#53324,#53325,#53326,#53327,#53328,#53329,
#53330,#53331,#53332,#53333,#53334,#53335),.UNSPECIFIED.,.F.,.F.,(4,3,3,
3,3,3,3,4),(-230.287601478595,-229.430356401001,-228.432833112301,-227.435309823601,
-226.437786534901,-225.440263246201,-224.442739957501,-224.004416171416),
 .UNSPECIFIED.);
#1306=B_SPLINE_CURVE_WITH_KNOTS('',3,(#53336,#53337,#53338,#53339,#53340,
#53341,#53342,#53343,#53344,#53345,#53346,#53347,#53348,#53349,#53350,#53351,
#53352,#53353,#53354,#53355,#53356,#53357),.UNSPECIFIED.,.F.,.F.,(4,3,3,
3,3,3,3,4),(221.027879259972,221.450170091401,222.447693380101,223.445216668801,
224.442739957501,225.440263246201,226.437786534901,227.311064567152),
 .UNSPECIFIED.);
#1307=B_SPLINE_CURVE_WITH_KNOTS('',3,(#53362,#53363,#53364,#53365,#53366,
#53367,#53368,#53369,#53370,#53371,#53372,#53373,#53374,#53375,#53376,#53377,
#53378,#53379,#53380,#53381,#53382,#53383,#53384,#53385,#53386),
 .UNSPECIFIED.,.F.,.F.,(4,3,3,3,3,3,3,3,4),(-236.570786785775,-236.413019421901,
-235.415496133201,-234.417972844501,-233.420449555801,-232.422926267101,
-231.425402978401,-230.427879689701,-230.287601478595),.UNSPECIFIED.);
#1308=B_SPLINE_CURVE_WITH_KNOTS('',3,(#53387,#53388,#53389,#53390,#53391,
#53392,#53393,#53394,#53395,#53396,#53397,#53398,#53399,#53400,#53401,#53402,
#53403,#53404,#53405,#53406,#53407,#53408,#53409,#53410,#53411),
 .UNSPECIFIED.,.F.,.F.,(4,3,3,3,3,3,3,3,4),(227.311064567152,227.435309823601,
228.432833112301,229.430356401001,230.427879689701,231.425402978401,232.422926267101,
233.420449555801,233.594249874331),.UNSPECIFIED.);
#1309=B_SPLINE_CURVE_WITH_KNOTS('',3,(#53416,#53417,#53418,#53419,#53420,
#53421,#53422,#53423,#53424,#53425,#53426,#53427,#53428,#53429,#53430,#53431,
#53432,#53433,#53434,#53435,#53436,#53437),.UNSPECIFIED.,.F.,.F.,(4,3,3,
3,3,3,3,4),(-242.853972092955,-242.398159154101,-241.400635865401,-240.403112576701,
-239.405589288001,-238.408065999301,-237.410542710601,-236.570786785775),
 .UNSPECIFIED.);
#1310=B_SPLINE_CURVE_WITH_KNOTS('',3,(#53438,#53439,#53440,#53441,#53442,
#53443,#53444,#53445,#53446,#53447,#53448,#53449,#53450,#53451,#53452,#53453,
#53454,#53455,#53456,#53457,#53458,#53459),.UNSPECIFIED.,.F.,.F.,(4,3,3,
3,3,3,3,4),(233.594249874331,234.417972844501,235.415496133201,236.413019421901,
237.410542710601,238.408065999301,239.405589288001,239.877435181511),
 .UNSPECIFIED.);
#1311=B_SPLINE_CURVE_WITH_KNOTS('',3,(#53464,#53465,#53466,#53467,#53468,
#53469,#53470,#53471,#53472,#53473,#53474,#53475,#53476,#53477,#53478,#53479,
#53480,#53481,#53482,#53483,#53484,#53485),.UNSPECIFIED.,.F.,.F.,(4,3,3,
3,3,3,3,4),(-249.137157400134,-248.383298886301,-247.385775597601,-246.388252308901,
-245.390729020201,-244.393205731501,-243.395682442801,-242.853972092955),
 .UNSPECIFIED.);
#1312=B_SPLINE_CURVE_WITH_KNOTS('',3,(#53486,#53487,#53488,#53489,#53490,
#53491,#53492,#53493,#53494,#53495,#53496,#53497,#53498,#53499,#53500,#53501,
#53502,#53503,#53504,#53505,#53506,#53507),.UNSPECIFIED.,.F.,.F.,(4,3,3,
3,3,3,3,4),(239.877435181511,240.403112576701,241.400635865401,242.398159154101,
243.395682442801,244.393205731501,245.390729020201,246.160620488691),
 .UNSPECIFIED.);
#1313=B_SPLINE_CURVE_WITH_KNOTS('',3,(#53512,#53513,#53514,#53515,#53516,
#53517,#53518,#53519,#53520,#53521,#53522,#53523,#53524,#53525,#53526,#53527,
#53528,#53529,#53530,#53531,#53532,#53533,#53534,#53535,#53536),
 .UNSPECIFIED.,.F.,.F.,(4,3,3,3,3,3,3,3,4),(-255.420342707314,-255.365961907201,
-254.368438618501,-253.370915329801,-252.373392041101,-251.375868752401,
-250.378345463701,-249.380822175001,-249.137157400134),.UNSPECIFIED.);
#1314=B_SPLINE_CURVE_WITH_KNOTS('',3,(#53537,#53538,#53539,#53540,#53541,
#53542,#53543,#53544,#53545,#53546,#53547,#53548,#53549,#53550,#53551,#53552,
#53553,#53554,#53555,#53556,#53557,#53558,#53559,#53560,#53561),
 .UNSPECIFIED.,.F.,.F.,(4,3,3,3,3,3,3,3,4),(246.160620488691,246.388252308901,
247.385775597601,248.383298886301,249.380822175001,250.378345463701,251.375868752401,
252.373392041101,252.44380579587),.UNSPECIFIED.);
#1315=B_SPLINE_CURVE_WITH_KNOTS('',3,(#53566,#53567,#53568,#53569,#53570,
#53571,#53572,#53573,#53574,#53575,#53576,#53577,#53578,#53579,#53580,#53581,
#53582,#53583,#53584,#53585,#53586,#53587),.UNSPECIFIED.,.F.,.F.,(4,3,3,
3,3,3,3,4),(-261.703528014493,-261.351101639401,-260.353578350701,-259.356055062001,
-258.358531773301,-257.361008484601,-256.363485195901,-255.420342707314),
 .UNSPECIFIED.);
#1316=B_SPLINE_CURVE_WITH_KNOTS('',3,(#53588,#53589,#53590,#53591,#53592,
#53593,#53594,#53595,#53596,#53597,#53598,#53599,#53600,#53601,#53602,#53603,
#53604,#53605,#53606,#53607,#53608,#53609),.UNSPECIFIED.,.F.,.F.,(4,3,3,
3,3,3,3,4),(252.44380579587,253.370915329801,254.368438618501,255.365961907201,
256.363485195901,257.361008484601,258.358531773301,258.72699110305),
 .UNSPECIFIED.);
#1317=B_SPLINE_CURVE_WITH_KNOTS('',3,(#53614,#53615,#53616,#53617,#53618,
#53619,#53620,#53621,#53622,#53623,#53624,#53625,#53626,#53627,#53628,#53629,
#53630,#53631,#53632,#53633,#53634,#53635),.UNSPECIFIED.,.F.,.F.,(4,3,3,
3,3,3,3,4),(-267.986713321673,-267.336241371601,-266.338718082901,-265.341194794201,
-264.343671505501,-263.346148216802,-262.348624928101,-261.703528014493),
 .UNSPECIFIED.);
#1318=B_SPLINE_CURVE_WITH_KNOTS('',3,(#53636,#53637,#53638,#53639,#53640,
#53641,#53642,#53643,#53644,#53645,#53646,#53647,#53648,#53649,#53650,#53651,
#53652,#53653,#53654,#53655,#53656,#53657),.UNSPECIFIED.,.F.,.F.,(4,3,3,
3,3,3,3,4),(258.72699110305,259.356055062001,260.353578350701,261.351101639402,
262.348624928102,263.346148216802,264.343671505502,265.010176410229),
 .UNSPECIFIED.);
#1319=B_SPLINE_CURVE_WITH_KNOTS('',3,(#53662,#53663,#53664,#53665,#53666,
#53667,#53668,#53669,#53670,#53671,#53672,#53673,#53674,#53675,#53676,#53677,
#53678,#53679,#53680,#53681,#53682,#53683),.UNSPECIFIED.,.F.,.F.,(4,3,3,
3,3,3,3,4),(-274.269898628852,-273.321381103802,-272.323857815102,-271.326334526402,
-270.328811237701,-269.331287949001,-268.333764660301,-267.986713321673),
 .UNSPECIFIED.);
#1320=B_SPLINE_CURVE_WITH_KNOTS('',3,(#53684,#53685,#53686,#53687,#53688,
#53689,#53690,#53691,#53692,#53693,#53694,#53695,#53696,#53697,#53698,#53699,
#53700,#53701,#53702,#53703,#53704,#53705),.UNSPECIFIED.,.F.,.F.,(4,3,3,
3,3,3,3,4),(265.010176410229,265.341194794201,266.338718082902,267.336241371602,
268.333764660302,269.331287949002,270.328811237702,271.293361717409),
 .UNSPECIFIED.);
#1321=B_SPLINE_CURVE_WITH_KNOTS('',3,(#53710,#53711,#53712,#53713,#53714,
#53715,#53716,#53717,#53718,#53719,#53720,#53721,#53722,#53723,#53724,#53725,
#53726,#53727,#53728,#53729,#53730,#53731,#53732,#53733,#53734),
 .UNSPECIFIED.,.F.,.F.,(4,3,3,3,3,3,3,3,4),(-280.553083936032,-280.304044124702,
-279.306520836001,-278.308997547301,-277.311474258601,-276.313950969901,
-275.316427681202,-274.318904392502,-274.269898628852),.UNSPECIFIED.);
#1322=B_SPLINE_CURVE_WITH_KNOTS('',3,(#53735,#53736,#53737,#53738,#53739,
#53740,#53741,#53742,#53743,#53744,#53745,#53746,#53747,#53748,#53749,#53750,
#53751,#53752,#53753,#53754,#53755,#53756,#53757,#53758,#53759),
 .UNSPECIFIED.,.F.,.F.,(4,3,3,3,3,3,3,3,4),(271.293361717409,271.326334526402,
272.323857815102,273.321381103802,274.318904392502,275.316427681202,276.313950969902,
277.311474258602,277.576547024588),.UNSPECIFIED.);
#1323=B_SPLINE_CURVE_WITH_KNOTS('',3,(#53764,#53765,#53766,#53767,#53768,
#53769,#53770,#53771,#53772,#53773,#53774,#53775,#53776,#53777,#53778,#53779,
#53780,#53781,#53782,#53783,#53784,#53785),.UNSPECIFIED.,.F.,.F.,(4,3,3,
3,3,3,3,4),(-286.836269243212,-286.289183856902,-285.291660568202,-284.294137279502,
-283.296613990802,-282.299090702102,-281.301567413402,-280.553083936032),
 .UNSPECIFIED.);
#1324=B_SPLINE_CURVE_WITH_KNOTS('',3,(#53786,#53787,#53788,#53789,#53790,
#53791,#53792,#53793,#53794,#53795,#53796,#53797,#53798,#53799,#53800,#53801,
#53802,#53803,#53804,#53805,#53806,#53807),.UNSPECIFIED.,.F.,.F.,(4,3,3,
3,3,3,3,4),(277.576547024588,278.308997547302,279.306520836002,280.304044124702,
281.301567413402,282.299090702102,283.296613990802,283.859732331768),
 .UNSPECIFIED.);
#1325=B_SPLINE_CURVE_WITH_KNOTS('',3,(#53812,#53813,#53814,#53815,#53816,
#53817,#53818,#53819,#53820,#53821,#53822,#53823,#53824,#53825,#53826,#53827,
#53828,#53829,#53830,#53831,#53832,#53833),.UNSPECIFIED.,.F.,.F.,(4,3,3,
3,3,3,3,4),(-293.119454550391,-292.274323589102,-291.276800300402,-290.279277011702,
-289.281753723002,-288.284230434302,-287.286707145602,-286.836269243212),
 .UNSPECIFIED.);
#1326=B_SPLINE_CURVE_WITH_KNOTS('',3,(#53834,#53835,#53836,#53837,#53838,
#53839,#53840,#53841,#53842,#53843,#53844,#53845,#53846,#53847,#53848,#53849,
#53850,#53851,#53852,#53853,#53854,#53855),.UNSPECIFIED.,.F.,.F.,(4,3,3,
3,3,3,3,4),(283.859732331768,284.294137279502,285.291660568202,286.289183856902,
287.286707145602,288.284230434302,289.281753723002,290.142917638947),
 .UNSPECIFIED.);
#1327=B_SPLINE_CURVE_WITH_KNOTS('',3,(#53860,#53861,#53862,#53863,#53864,
#53865,#53866,#53867,#53868,#53869,#53870,#53871,#53872,#53873,#53874,#53875,
#53876,#53877,#53878,#53879,#53880,#53881,#53882,#53883,#53884),
 .UNSPECIFIED.,.F.,.F.,(4,3,3,3,3,3,3,3,4),(-299.402639857571,-299.256986610002,
-298.259463321302,-297.261940032602,-296.264416743902,-295.266893455202,
-294.269370166502,-293.271846877802,-293.119454550391),.UNSPECIFIED.);
#1328=B_SPLINE_CURVE_WITH_KNOTS('',3,(#53885,#53886,#53887,#53888,#53889,
#53890,#53891,#53892,#53893,#53894,#53895,#53896,#53897,#53898,#53899,#53900,
#53901,#53902,#53903,#53904,#53905,#53906,#53907,#53908,#53909),
 .UNSPECIFIED.,.F.,.F.,(4,3,3,3,3,3,3,3,4),(290.142917638947,290.279277011702,
291.276800300402,292.274323589102,293.271846877802,294.269370166502,295.266893455202,
296.264416743902,296.426102946127),.UNSPECIFIED.);
#1329=B_SPLINE_CURVE_WITH_KNOTS('',3,(#53914,#53915,#53916,#53917,#53918,
#53919,#53920,#53921,#53922,#53923,#53924,#53925,#53926,#53927,#53928,#53929,
#53930,#53931,#53932,#53933,#53934,#53935),.UNSPECIFIED.,.F.,.F.,(4,3,3,
3,3,3,3,4),(-305.68582516475,-305.242126342202,-304.244603053502,-303.247079764802,
-302.249556476102,-301.252033187402,-300.254509898702,-299.402639857571),
 .UNSPECIFIED.);
#1330=B_SPLINE_CURVE_WITH_KNOTS('',3,(#53936,#53937,#53938,#53939,#53940,
#53941,#53942,#53943,#53944,#53945,#53946,#53947,#53948,#53949,#53950,#53951,
#53952,#53953,#53954,#53955,#53956,#53957),.UNSPECIFIED.,.F.,.F.,(4,3,3,
3,3,3,3,4),(296.426102946127,297.261940032602,298.259463321302,299.256986610002,
300.254509898702,301.252033187402,302.249556476102,302.709288253307),
 .UNSPECIFIED.);
#1331=B_SPLINE_CURVE_WITH_KNOTS('',3,(#53962,#53963,#53964,#53965,#53966,
#53967,#53968,#53969,#53970,#53971,#53972,#53973,#53974,#53975,#53976,#53977,
#53978,#53979,#53980,#53981,#53982,#53983),.UNSPECIFIED.,.F.,.F.,(4,3,3,
3,3,3,3,4),(-311.96901047193,-311.227266074402,-310.229742785702,-309.232219497002,
-308.234696208302,-307.237172919602,-306.239649630902,-305.68582516475),
 .UNSPECIFIED.);
#1332=B_SPLINE_CURVE_WITH_KNOTS('',3,(#53984,#53985,#53986,#53987,#53988,
#53989,#53990,#53991,#53992,#53993,#53994,#53995,#53996,#53997,#53998,#53999,
#54000,#54001,#54002,#54003,#54004,#54005),.UNSPECIFIED.,.F.,.F.,(4,3,3,
3,3,3,3,4),(302.709288253307,303.247079764802,304.244603053502,305.242126342202,
306.239649630902,307.237172919602,308.234696208302,308.992473560486),
 .UNSPECIFIED.);
#1333=B_SPLINE_CURVE_WITH_KNOTS('',3,(#54010,#54011,#54012,#54013,#54014,
#54015,#54016,#54017,#54018,#54019,#54020,#54021,#54022,#54023,#54024,#54025,
#54026,#54027,#54028,#54029,#54030,#54031,#54032,#54033,#54034),
 .UNSPECIFIED.,.F.,.F.,(4,3,3,3,3,3,3,3,4),(-318.252195779109,-318.209929095302,
-317.212405806602,-316.214882517902,-315.217359229202,-314.219835940502,
-313.222312651802,-312.224789363102,-311.96901047193),.UNSPECIFIED.);
#1334=B_SPLINE_CURVE_WITH_KNOTS('',3,(#54035,#54036,#54037,#54038,#54039,
#54040,#54041,#54042,#54043,#54044,#54045,#54046,#54047,#54048,#54049,#54050,
#54051,#54052,#54053,#54054,#54055,#54056,#54057,#54058,#54059),
 .UNSPECIFIED.,.F.,.F.,(4,3,3,3,3,3,3,3,4),(308.992473560486,309.232219497002,
310.229742785702,311.227266074402,312.224789363102,313.222312651802,314.219835940502,
315.217359229202,315.275658867666),.UNSPECIFIED.);
#1335=B_SPLINE_CURVE_WITH_KNOTS('',3,(#54064,#54065,#54066,#54067,#54068,
#54069,#54070,#54071,#54072,#54073,#54074,#54075,#54076,#54077,#54078,#54079,
#54080,#54081,#54082,#54083,#54084,#54085),.UNSPECIFIED.,.F.,.F.,(4,3,3,
3,3,3,3,4),(-324.535381086289,-324.195068827502,-323.197545538802,-322.200022250102,
-321.202498961402,-320.204975672702,-319.207452384002,-318.252195779109),
 .UNSPECIFIED.);
#1336=B_SPLINE_CURVE_WITH_KNOTS('',3,(#54086,#54087,#54088,#54089,#54090,
#54091,#54092,#54093,#54094,#54095,#54096,#54097,#54098,#54099,#54100,#54101,
#54102,#54103,#54104,#54105,#54106,#54107),.UNSPECIFIED.,.F.,.F.,(4,3,3,
3,3,3,3,4),(315.275658867666,316.214882517902,317.212405806602,318.209929095302,
319.207452384002,320.204975672702,321.202498961402,321.558844174845),
 .UNSPECIFIED.);
#1337=B_SPLINE_CURVE_WITH_KNOTS('',3,(#54112,#54113,#54114,#54115,#54116,
#54117,#54118,#54119,#54120,#54121,#54122,#54123,#54124,#54125,#54126,#54127,
#54128,#54129,#54130,#54131,#54132,#54133),.UNSPECIFIED.,.F.,.F.,(4,3,3,
3,3,3,3,4),(-330.818566393468,-330.180208559702,-329.182685271002,-328.185161982302,
-327.187638693602,-326.190115404902,-325.192592116202,-324.535381086289),
 .UNSPECIFIED.);
#1338=B_SPLINE_CURVE_WITH_KNOTS('',3,(#54134,#54135,#54136,#54137,#54138,
#54139,#54140,#54141,#54142,#54143,#54144,#54145,#54146,#54147,#54148,#54149,
#54150,#54151,#54152,#54153,#54154,#54155),.UNSPECIFIED.,.F.,.F.,(4,3,3,
3,3,3,3,4),(321.558844174845,322.200022250102,323.197545538802,324.195068827502,
325.192592116202,326.190115404902,327.187638693602,327.842029482025),
 .UNSPECIFIED.);
#1339=B_SPLINE_CURVE_WITH_KNOTS('',3,(#54160,#54161,#54162,#54163,#54164,
#54165,#54166,#54167,#54168,#54169,#54170,#54171,#54172,#54173,#54174,#54175,
#54176,#54177,#54178,#54179,#54180,#54181),.UNSPECIFIED.,.F.,.F.,(4,3,3,
3,3,3,3,4),(-337.101751700648,-336.165348291902,-335.167825003202,-334.170301714502,
-333.172778425802,-332.175255137102,-331.177731848402,-330.818566393468),
 .UNSPECIFIED.);
#1340=B_SPLINE_CURVE_WITH_KNOTS('',3,(#54182,#54183,#54184,#54185,#54186,
#54187,#54188,#54189,#54190,#54191,#54192,#54193,#54194,#54195,#54196,#54197,
#54198,#54199,#54200,#54201,#54202,#54203),.UNSPECIFIED.,.F.,.F.,(4,3,3,
3,3,3,3,4),(327.842029482025,328.185161982302,329.182685271002,330.180208559702,
331.177731848402,332.175255137102,333.172778425802,334.125214789205),
 .UNSPECIFIED.);
#1341=B_SPLINE_CURVE_WITH_KNOTS('',3,(#54208,#54209,#54210,#54211,#54212,
#54213,#54214,#54215,#54216,#54217,#54218,#54219,#54220,#54221,#54222,#54223,
#54224,#54225,#54226,#54227,#54228,#54229,#54230,#54231,#54232),
 .UNSPECIFIED.,.F.,.F.,(4,3,3,3,3,3,3,3,4),(-343.384937007828,-343.148011312802,
-342.150488024102,-341.152964735402,-340.155441446702,-339.157918158002,
-338.160394869302,-337.162871580602,-337.101751700648),.UNSPECIFIED.);
#1342=B_SPLINE_CURVE_WITH_KNOTS('',3,(#54233,#54234,#54235,#54236,#54237,
#54238,#54239,#54240,#54241,#54242,#54243,#54244,#54245,#54246,#54247,#54248,
#54249,#54250,#54251,#54252,#54253,#54254,#54255,#54256,#54257),
 .UNSPECIFIED.,.F.,.F.,(4,3,3,3,3,3,3,3,4),(334.125214789205,334.170301714502,
335.167825003202,336.165348291902,337.162871580602,338.160394869302,339.157918158002,
340.155441446702,340.408400096384),.UNSPECIFIED.);
#1343=B_SPLINE_CURVE_WITH_KNOTS('',3,(#54262,#54263,#54264,#54265,#54266,
#54267,#54268,#54269,#54270,#54271,#54272,#54273,#54274,#54275,#54276,#54277,
#54278,#54279,#54280,#54281,#54282,#54283),.UNSPECIFIED.,.F.,.F.,(4,3,3,
3,3,3,3,4),(-349.668122315007,-349.133151045002,-348.135627756302,-347.138104467602,
-346.140581178902,-345.143057890202,-344.145534601502,-343.384937007828),
 .UNSPECIFIED.);
#1344=B_SPLINE_CURVE_WITH_KNOTS('',3,(#54284,#54285,#54286,#54287,#54288,
#54289,#54290,#54291,#54292,#54293,#54294,#54295,#54296,#54297,#54298,#54299,
#54300,#54301,#54302,#54303,#54304,#54305),.UNSPECIFIED.,.F.,.F.,(4,3,3,
3,3,3,3,4),(340.408400096384,341.152964735402,342.150488024102,343.148011312802,
344.145534601502,345.143057890202,346.140581178902,346.691585403564),
 .UNSPECIFIED.);
#1345=B_SPLINE_CURVE_WITH_KNOTS('',3,(#54310,#54311,#54312,#54313,#54314,
#54315,#54316,#54317,#54318,#54319,#54320,#54321,#54322,#54323,#54324,#54325,
#54326,#54327,#54328,#54329,#54330,#54331),.UNSPECIFIED.,.F.,.F.,(4,3,3,
3,3,3,3,4),(-355.951307622187,-355.118290777202,-354.120767488502,-353.123244199802,
-352.125720911102,-351.128197622402,-350.130674333702,-349.668122315007),
 .UNSPECIFIED.);
#1346=B_SPLINE_CURVE_WITH_KNOTS('',3,(#54332,#54333,#54334,#54335,#54336,
#54337,#54338,#54339,#54340,#54341,#54342,#54343,#54344,#54345,#54346,#54347,
#54348,#54349,#54350,#54351,#54352,#54353),.UNSPECIFIED.,.F.,.F.,(4,3,3,
3,3,3,3,4),(346.691585403564,347.138104467602,348.135627756302,349.133151045002,
350.130674333702,351.128197622402,352.125720911102,352.974770710743),
 .UNSPECIFIED.);
#1347=B_SPLINE_CURVE_WITH_KNOTS('',3,(#54358,#54359,#54360,#54361,#54362,
#54363,#54364,#54365,#54366,#54367,#54368,#54369,#54370,#54371,#54372,#54373,
#54374,#54375,#54376,#54377,#54378,#54379,#54380,#54381,#54382),
 .UNSPECIFIED.,.F.,.F.,(4,3,3,3,3,3,3,3,4),(-362.234492929366,-362.100953798102,
-361.103430509402,-360.105907220702,-359.108383932002,-358.110860643302,
-357.113337354602,-356.115814065902,-355.951307622187),.UNSPECIFIED.);
#1348=B_SPLINE_CURVE_WITH_KNOTS('',3,(#54383,#54384,#54385,#54386,#54387,
#54388,#54389,#54390,#54391,#54392,#54393,#54394,#54395,#54396,#54397,#54398,
#54399,#54400,#54401,#54402,#54403,#54404,#54405,#54406,#54407),
 .UNSPECIFIED.,.F.,.F.,(4,3,3,3,3,3,3,3,4),(352.974770710743,353.123244199802,
354.120767488502,355.118290777202,356.115814065902,357.113337354602,358.110860643302,
359.108383932002,359.257956017923),.UNSPECIFIED.);
#1349=B_SPLINE_CURVE_WITH_KNOTS('',3,(#54412,#54413,#54414,#54415,#54416,
#54417,#54418,#54419,#54420,#54421,#54422,#54423,#54424,#54425,#54426,#54427,
#54428,#54429,#54430,#54431,#54432,#54433),.UNSPECIFIED.,.F.,.F.,(4,3,3,
3,3,3,3,4),(-368.517678236546,-368.086093530302,-367.088570241602,-366.091046952902,
-365.093523664202,-364.096000375502,-363.098477086802,-362.234492929366),
 .UNSPECIFIED.);
#1350=B_SPLINE_CURVE_WITH_KNOTS('',3,(#54434,#54435,#54436,#54437,#54438,
#54439,#54440,#54441,#54442,#54443,#54444,#54445,#54446,#54447,#54448,#54449,
#54450,#54451,#54452,#54453,#54454,#54455),.UNSPECIFIED.,.F.,.F.,(4,3,3,
3,3,3,3,4),(359.257956017923,360.105907220702,361.103430509402,362.100953798102,
363.098477086802,364.096000375502,365.093523664202,365.541141325102),
 .UNSPECIFIED.);
#1351=B_SPLINE_CURVE_WITH_KNOTS('',3,(#54460,#54461,#54462,#54463,#54464,
#54465,#54466,#54467,#54468,#54469,#54470,#54471,#54472,#54473,#54474,#54475,
#54476,#54477,#54478,#54479,#54480,#54481),.UNSPECIFIED.,.F.,.F.,(4,3,3,
3,3,3,3,4),(-374.800863543725,-374.071233262502,-373.073709973802,-372.076186685102,
-371.078663396402,-370.081140107702,-369.083616819002,-368.517678236546),
 .UNSPECIFIED.);
#1352=B_SPLINE_CURVE_WITH_KNOTS('',3,(#54482,#54483,#54484,#54485,#54486,
#54487,#54488,#54489,#54490,#54491,#54492,#54493,#54494,#54495,#54496,#54497,
#54498,#54499,#54500,#54501,#54502,#54503),.UNSPECIFIED.,.F.,.F.,(4,3,3,
3,3,3,3,4),(365.541141325102,366.091046952902,367.088570241602,368.086093530302,
369.083616819002,370.081140107702,371.078663396402,371.824326632282),
 .UNSPECIFIED.);
#1353=B_SPLINE_CURVE_WITH_KNOTS('',3,(#54509,#54510,#54511,#54512,#54513,
#54514),.UNSPECIFIED.,.F.,.F.,(4,1,1,4),(386.415896391544,386.683789399021,
387.681312687721,388.606151278594),.UNSPECIFIED.);
#1354=B_SPLINE_CURVE_WITH_KNOTS('',3,(#54517,#54518,#54519,#54520,#54521),
 .UNSPECIFIED.,.F.,.F.,(4,1,4),(386.415896391544,386.868472513736,387.367234158086),
 .UNSPECIFIED.);
#1355=B_SPLINE_CURVE_WITH_KNOTS('',3,(#54526,#54527,#54528,#54529,#54530,
#54531,#54532,#54533,#54534,#54535),.UNSPECIFIED.,.F.,.F.,(4,1,1,1,1,1,
1,4),(380.132711084365,380.698649666821,381.696172955521,382.693696244221,
383.691219532921,384.688742821621,385.686266110321,386.415896391544),
 .UNSPECIFIED.);
#1356=B_SPLINE_CURVE_WITH_KNOTS('',3,(#54536,#54537,#54538,#54539,#54540,
#54541,#54542,#54543,#54544,#54545,#54546),.UNSPECIFIED.,.F.,.F.,(4,1,1,
1,1,1,1,1,4),(380.132711084365,380.384571137186,381.382094425886,382.379617714586,
383.377141003286,384.374664291986,385.372187580686,386.369710869386,386.415896391544),
 .UNSPECIFIED.);
#1357=B_SPLINE_CURVE_WITH_KNOTS('',3,(#54551,#54552,#54553,#54554,#54555,
#54556,#54557,#54558,#54559,#54560),.UNSPECIFIED.,.F.,.F.,(4,1,1,1,1,1,
1,4),(373.849525777185,374.713509934621,375.711033223321,376.708556512021,
377.706079800721,378.703603089421,379.701126378121,380.132711084365),
 .UNSPECIFIED.);
#1358=B_SPLINE_CURVE_WITH_KNOTS('',3,(#54561,#54562,#54563,#54564,#54565,
#54566,#54567,#54568,#54569,#54570),.UNSPECIFIED.,.F.,.F.,(4,1,1,1,1,1,
1,4),(373.849525777185,374.399431404986,375.396954693686,376.394477982386,
377.392001271086,378.389524559786,379.387047848486,380.132711084365),
 .UNSPECIFIED.);
#1359=B_SPLINE_CURVE_WITH_KNOTS('',3,(#54575,#54576,#54577,#54578,#54579,
#54580,#54581,#54582,#54583,#54584,#54585),.UNSPECIFIED.,.F.,.F.,(4,1,1,
1,1,1,1,1,4),(367.566340470006,367.730846913721,368.728370202421,369.725893491121,
370.723416779821,371.720940068521,372.718463357221,373.715986645921,373.849525777185),
 .UNSPECIFIED.);
#1360=B_SPLINE_CURVE_WITH_KNOTS('',3,(#54586,#54587,#54588,#54589,#54590,
#54591,#54592,#54593,#54594,#54595),.UNSPECIFIED.,.F.,.F.,(4,1,1,1,1,1,
1,4),(367.566340470006,368.414291672786,369.411814961486,370.409338250186,
371.406861538886,372.404384827586,373.401908116286,373.849525777185),
 .UNSPECIFIED.);
#1361=B_SPLINE_CURVE_WITH_KNOTS('',3,(#54600,#54601,#54602,#54603,#54604,
#54605,#54606,#54607,#54608,#54609),.UNSPECIFIED.,.F.,.F.,(4,1,1,1,1,1,
1,4),(361.283155162826,361.745707181521,362.743230470221,363.740753758921,
364.738277047621,365.735800336321,366.733323625021,367.566340470006),
 .UNSPECIFIED.);
#1362=B_SPLINE_CURVE_WITH_KNOTS('',3,(#54610,#54611,#54612,#54613,#54614,
#54615,#54616,#54617,#54618,#54619,#54620),.UNSPECIFIED.,.F.,.F.,(4,1,1,
1,1,1,1,1,4),(361.283155162826,361.431628651886,362.429151940586,363.426675229286,
364.424198517986,365.421721806686,366.419245095386,367.416768384086,367.566340470006),
 .UNSPECIFIED.);
#1363=B_SPLINE_CURVE_WITH_KNOTS('',3,(#54625,#54626,#54627,#54628,#54629,
#54630,#54631,#54632,#54633,#54634),.UNSPECIFIED.,.F.,.F.,(4,1,1,1,1,1,
1,4),(354.999969855647,355.760567449321,356.758090738021,357.755614026721,
358.753137315421,359.750660604121,360.748183892821,361.283155162826),
 .UNSPECIFIED.);
#1364=B_SPLINE_CURVE_WITH_KNOTS('',3,(#54635,#54636,#54637,#54638,#54639,
#54640,#54641,#54642,#54643,#54644),.UNSPECIFIED.,.F.,.F.,(4,1,1,1,1,1,
1,4),(354.999969855647,355.446488919686,356.444012208386,357.441535497086,
358.439058785786,359.436582074486,360.434105363186,361.283155162826),
 .UNSPECIFIED.);
#1365=B_SPLINE_CURVE_WITH_KNOTS('',3,(#54649,#54650,#54651,#54652,#54653,
#54654,#54655,#54656,#54657,#54658,#54659),.UNSPECIFIED.,.F.,.F.,(4,1,1,
1,1,1,1,1,4),(348.716784548467,348.777904428421,349.775427717121,350.772951005821,
351.770474294521,352.767997583221,353.765520871921,354.763044160621,354.999969855647),
 .UNSPECIFIED.);
#1366=B_SPLINE_CURVE_WITH_KNOTS('',3,(#54660,#54661,#54662,#54663,#54664,
#54665,#54666,#54667,#54668,#54669),.UNSPECIFIED.,.F.,.F.,(4,1,1,1,1,1,
1,4),(348.716784548467,349.461349187486,350.458872476186,351.456395764886,
352.453919053586,353.451442342286,354.448965630986,354.999969855647),
 .UNSPECIFIED.);
#1367=B_SPLINE_CURVE_WITH_KNOTS('',3,(#54674,#54675,#54676,#54677,#54678,
#54679,#54680,#54681,#54682,#54683),.UNSPECIFIED.,.F.,.F.,(4,1,1,1,1,1,
1,4),(342.433599241287,342.792764696221,343.790287984921,344.787811273621,
345.785334562321,346.782857851021,347.780381139721,348.716784548467),
 .UNSPECIFIED.);
#1368=B_SPLINE_CURVE_WITH_KNOTS('',3,(#54684,#54685,#54686,#54687,#54688,
#54689,#54690,#54691,#54692,#54693,#54694),.UNSPECIFIED.,.F.,.F.,(4,1,1,
1,1,1,1,1,4),(342.433599241287,342.478686166586,343.476209455286,344.473732743986,
345.471256032686,346.468779321386,347.466302610086,348.463825898786,348.716784548467),
 .UNSPECIFIED.);
#1369=B_SPLINE_CURVE_WITH_KNOTS('',3,(#54699,#54700,#54701,#54702,#54703,
#54704,#54705,#54706,#54707,#54708),.UNSPECIFIED.,.F.,.F.,(4,1,1,1,1,1,
1,4),(336.150413934108,336.807624964021,337.805148252721,338.802671541421,
339.800194830121,340.797718118821,341.795241407521,342.433599241287),
 .UNSPECIFIED.);
#1370=B_SPLINE_CURVE_WITH_KNOTS('',3,(#54709,#54710,#54711,#54712,#54713,
#54714,#54715,#54716,#54717,#54718),.UNSPECIFIED.,.F.,.F.,(4,1,1,1,1,1,
1,4),(336.150413934108,336.493546434386,337.491069723086,338.488593011786,
339.486116300486,340.483639589186,341.481162877886,342.433599241287),
 .UNSPECIFIED.);
#1371=B_SPLINE_CURVE_WITH_KNOTS('',3,(#54723,#54724,#54725,#54726,#54727,
#54728,#54729,#54730,#54731,#54732),.UNSPECIFIED.,.F.,.F.,(4,1,1,1,1,1,
1,4),(329.867228626928,330.822485231821,331.820008520521,332.817531809221,
333.815055097921,334.812578386621,335.810101675321,336.150413934108),
 .UNSPECIFIED.);
#1372=B_SPLINE_CURVE_WITH_KNOTS('',3,(#54733,#54734,#54735,#54736,#54737,
#54738,#54739,#54740,#54741,#54742),.UNSPECIFIED.,.F.,.F.,(4,1,1,1,1,1,
1,4),(329.867228626928,330.508406702186,331.505929990886,332.503453279586,
333.500976568286,334.498499856986,335.496023145686,336.150413934108),
 .UNSPECIFIED.);
#1373=B_SPLINE_CURVE_WITH_KNOTS('',3,(#54747,#54748,#54749,#54750,#54751,
#54752,#54753,#54754,#54755,#54756,#54757),.UNSPECIFIED.,.F.,.F.,(4,1,1,
1,1,1,1,1,4),(323.584043319749,323.839822210921,324.837345499621,325.834868788321,
326.832392077021,327.829915365721,328.827438654421,329.824961943121,329.867228626928),
 .UNSPECIFIED.);
#1374=B_SPLINE_CURVE_WITH_KNOTS('',3,(#54758,#54759,#54760,#54761,#54762,
#54763,#54764,#54765,#54766,#54767),.UNSPECIFIED.,.F.,.F.,(4,1,1,1,1,1,
1,4),(323.584043319749,324.523266969986,325.520790258686,326.518313547386,
327.515836836086,328.513360124786,329.510883413486,329.867228626928),
 .UNSPECIFIED.);
#1375=B_SPLINE_CURVE_WITH_KNOTS('',3,(#54772,#54773,#54774,#54775,#54776,
#54777,#54778,#54779,#54780,#54781),.UNSPECIFIED.,.F.,.F.,(4,1,1,1,1,1,
1,4),(317.300858012569,317.854682478721,318.852205767421,319.849729056121,
320.847252344821,321.844775633521,322.842298922221,323.584043319749),
 .UNSPECIFIED.);
#1376=B_SPLINE_CURVE_WITH_KNOTS('',3,(#54782,#54783,#54784,#54785,#54786,
#54787,#54788,#54789,#54790,#54791,#54792),.UNSPECIFIED.,.F.,.F.,(4,1,1,
1,1,1,1,1,4),(317.300858012569,317.540603949086,318.538127237786,319.535650526486,
320.533173815186,321.530697103886,322.528220392586,323.525743681286,323.584043319749),
 .UNSPECIFIED.);
#1377=B_SPLINE_CURVE_WITH_KNOTS('',3,(#54797,#54798,#54799,#54800,#54801,
#54802,#54803,#54804,#54805,#54806),.UNSPECIFIED.,.F.,.F.,(4,1,1,1,1,1,
1,4),(311.01767270539,311.869542746521,312.867066035221,313.864589323921,
314.862112612621,315.859635901321,316.857159190021,317.300858012569),
 .UNSPECIFIED.);
#1378=B_SPLINE_CURVE_WITH_KNOTS('',3,(#54807,#54808,#54809,#54810,#54811,
#54812,#54813,#54814,#54815,#54816),.UNSPECIFIED.,.F.,.F.,(4,1,1,1,1,1,
1,4),(311.01767270539,311.555464216886,312.552987505586,313.550510794286,
314.548034082986,315.545557371686,316.543080660386,317.300858012569),
 .UNSPECIFIED.);
#1379=B_SPLINE_CURVE_WITH_KNOTS('',3,(#54821,#54822,#54823,#54824,#54825,
#54826,#54827,#54828,#54829,#54830,#54831),.UNSPECIFIED.,.F.,.F.,(4,1,1,
1,1,1,1,1,4),(304.73448739821,304.886879725621,305.884403014321,306.881926303021,
307.879449591721,308.876972880421,309.874496169121,310.872019457821,311.01767270539),
 .UNSPECIFIED.);
#1380=B_SPLINE_CURVE_WITH_KNOTS('',3,(#54832,#54833,#54834,#54835,#54836,
#54837,#54838,#54839,#54840,#54841),.UNSPECIFIED.,.F.,.F.,(4,1,1,1,1,1,
1,4),(304.73448739821,305.570324484686,306.567847773386,307.565371062086,
308.562894350786,309.560417639486,310.557940928186,311.01767270539),
 .UNSPECIFIED.);
#1381=B_SPLINE_CURVE_WITH_KNOTS('',3,(#54846,#54847,#54848,#54849,#54850,
#54851,#54852,#54853,#54854,#54855),.UNSPECIFIED.,.F.,.F.,(4,1,1,1,1,1,
1,4),(298.451302091031,298.901739993421,299.899263282121,300.896786570821,
301.894309859521,302.891833148221,303.889356436921,304.73448739821),
 .UNSPECIFIED.);
#1382=B_SPLINE_CURVE_WITH_KNOTS('',3,(#54856,#54857,#54858,#54859,#54860,
#54861,#54862,#54863,#54864,#54865,#54866),.UNSPECIFIED.,.F.,.F.,(4,1,1,
1,1,1,1,1,4),(298.451302091031,298.587661463786,299.585184752486,300.582708041186,
301.580231329886,302.577754618586,303.575277907286,304.572801195986,304.73448739821),
 .UNSPECIFIED.);
#1383=B_SPLINE_CURVE_WITH_KNOTS('',3,(#54871,#54872,#54873,#54874,#54875,
#54876,#54877,#54878,#54879,#54880),.UNSPECIFIED.,.F.,.F.,(4,1,1,1,1,1,
1,4),(292.168116783851,292.916600261221,293.914123549921,294.911646838621,
295.909170127321,296.906693416021,297.904216704721,298.451302091031),
 .UNSPECIFIED.);
#1384=B_SPLINE_CURVE_WITH_KNOTS('',3,(#54881,#54882,#54883,#54884,#54885,
#54886,#54887,#54888,#54889,#54890),.UNSPECIFIED.,.F.,.F.,(4,1,1,1,1,1,
1,4),(292.168116783851,292.602521731586,293.600045020286,294.597568308986,
295.595091597686,296.592614886386,297.590138175086,298.451302091031),
 .UNSPECIFIED.);
#1385=B_SPLINE_CURVE_WITH_KNOTS('',3,(#54895,#54896,#54897,#54898,#54899,
#54900,#54901,#54902,#54903,#54904,#54905),.UNSPECIFIED.,.F.,.F.,(4,1,1,
1,1,1,1,1,4),(285.884931476671,285.933937240321,286.931460529021,287.928983817721,
288.926507106421,289.924030395121,290.921553683821,291.919076972521,292.168116783851),
 .UNSPECIFIED.);
#1386=B_SPLINE_CURVE_WITH_KNOTS('',3,(#54906,#54907,#54908,#54909,#54910,
#54911,#54912,#54913,#54914,#54915),.UNSPECIFIED.,.F.,.F.,(4,1,1,1,1,1,
1,4),(285.884931476671,286.617381999385,287.614905288085,288.612428576785,
289.609951865485,290.607475154186,291.604998442886,292.168116783851),
 .UNSPECIFIED.);
#1387=B_SPLINE_CURVE_WITH_KNOTS('',3,(#54920,#54921,#54922,#54923,#54924,
#54925,#54926,#54927,#54928,#54929),.UNSPECIFIED.,.F.,.F.,(4,1,1,1,1,1,
1,4),(279.601746169492,279.948797508121,280.946320796821,281.943844085521,
282.941367374221,283.938890662921,284.936413951621,285.884931476671),
 .UNSPECIFIED.);
#1388=B_SPLINE_CURVE_WITH_KNOTS('',3,(#54930,#54931,#54932,#54933,#54934,
#54935,#54936,#54937,#54938,#54939,#54940),.UNSPECIFIED.,.F.,.F.,(4,1,1,
1,1,1,1,1,4),(279.601746169492,279.634718978485,280.632242267185,281.629765555885,
282.627288844585,283.624812133285,284.622335421985,285.619858710685,285.884931476671),
 .UNSPECIFIED.);
#1389=B_SPLINE_CURVE_WITH_KNOTS('',3,(#54945,#54946,#54947,#54948,#54949,
#54950,#54951,#54952,#54953,#54954),.UNSPECIFIED.,.F.,.F.,(4,1,1,1,1,1,
1,4),(273.318560862312,273.963657775921,274.961181064621,275.958704353321,
276.956227642021,277.953750930721,278.951274219421,279.601746169492),
 .UNSPECIFIED.);
#1390=B_SPLINE_CURVE_WITH_KNOTS('',3,(#54955,#54956,#54957,#54958,#54959,
#54960,#54961,#54962,#54963,#54964),.UNSPECIFIED.,.F.,.F.,(4,1,1,1,1,1,
1,4),(273.318560862312,273.649579246285,274.647102534985,275.644625823685,
276.642149112385,277.639672401085,278.637195689785,279.601746169492),
 .UNSPECIFIED.);
#1391=B_SPLINE_CURVE_WITH_KNOTS('',3,(#54969,#54970,#54971,#54972,#54973,
#54974,#54975,#54976,#54977,#54978),.UNSPECIFIED.,.F.,.F.,(4,1,1,1,1,1,
1,4),(267.035375555133,267.97851804372,268.97604133242,269.973564621121,
270.971087909821,271.968611198521,272.966134487221,273.318560862312),
 .UNSPECIFIED.);
#1392=B_SPLINE_CURVE_WITH_KNOTS('',3,(#54979,#54980,#54981,#54982,#54983,
#54984,#54985,#54986,#54987,#54988),.UNSPECIFIED.,.F.,.F.,(4,1,1,1,1,1,
1,4),(267.035375555133,267.664439514085,268.661962802785,269.659486091485,
270.657009380185,271.654532668885,272.652055957585,273.318560862312),
 .UNSPECIFIED.);
#1393=B_SPLINE_CURVE_WITH_KNOTS('',3,(#54993,#54994,#54995,#54996,#54997,
#54998,#54999,#55000,#55001,#55002,#55003),.UNSPECIFIED.,.F.,.F.,(4,1,1,
1,1,1,1,1,4),(260.752190247953,260.99585502282,261.99337831152,262.99090160022,
263.98842488892,264.98594817762,265.983471466321,266.980994755021,267.035375555133),
 .UNSPECIFIED.);
#1394=B_SPLINE_CURVE_WITH_KNOTS('',3,(#55004,#55005,#55006,#55007,#55008,
#55009,#55010,#55011,#55012,#55013),.UNSPECIFIED.,.F.,.F.,(4,1,1,1,1,1,
1,4),(260.752190247953,261.679299781885,262.676823070585,263.674346359285,
264.671869647985,265.669392936685,266.666916225385,267.035375555133),
 .UNSPECIFIED.);
#1395=B_SPLINE_CURVE_WITH_KNOTS('',3,(#55018,#55019,#55020,#55021,#55022,
#55023,#55024,#55025,#55026,#55027),.UNSPECIFIED.,.F.,.F.,(4,1,1,1,1,1,
1,4),(254.469004940774,255.01071529062,256.00823857932,257.00576186802,
258.00328515672,259.00080844542,259.99833173412,260.752190247953),
 .UNSPECIFIED.);
#1396=B_SPLINE_CURVE_WITH_KNOTS('',3,(#55028,#55029,#55030,#55031,#55032,
#55033,#55034,#55035,#55036,#55037,#55038),.UNSPECIFIED.,.F.,.F.,(4,1,1,
1,1,1,1,1,4),(254.469004940774,254.696636760985,255.694160049685,256.691683338385,
257.689206627085,258.686729915785,259.684253204485,260.681776493185,260.752190247953),
 .UNSPECIFIED.);
#1397=B_SPLINE_CURVE_WITH_KNOTS('',3,(#55043,#55044,#55045,#55046,#55047,
#55048,#55049,#55050,#55051,#55052),.UNSPECIFIED.,.F.,.F.,(4,1,1,1,1,1,
1,4),(248.185819633594,249.02557555842,250.02309884712,251.02062213582,
252.01814542452,253.01566871322,254.01319200192,254.469004940774),
 .UNSPECIFIED.);
#1398=B_SPLINE_CURVE_WITH_KNOTS('',3,(#55053,#55054,#55055,#55056,#55057,
#55058,#55059,#55060,#55061,#55062),.UNSPECIFIED.,.F.,.F.,(4,1,1,1,1,1,
1,4),(248.185819633594,248.711497028785,249.709020317485,250.706543606185,
251.704066894885,252.701590183585,253.699113472285,254.469004940774),
 .UNSPECIFIED.);
#1399=B_SPLINE_CURVE_WITH_KNOTS('',3,(#55067,#55068,#55069,#55070,#55071,
#55072,#55073,#55074,#55075,#55076,#55077),.UNSPECIFIED.,.F.,.F.,(4,1,1,
1,1,1,1,1,4),(241.902634326414,242.04291253752,243.04043582622,244.03795911492,
245.03548240362,246.03300569232,247.03052898102,248.02805226972,248.185819633594),
 .UNSPECIFIED.);
#1400=B_SPLINE_CURVE_WITH_KNOTS('',3,(#55078,#55079,#55080,#55081,#55082,
#55083,#55084,#55085,#55086,#55087),.UNSPECIFIED.,.F.,.F.,(4,1,1,1,1,1,
1,4),(241.902634326414,242.726357296585,243.723880585285,244.721403873985,
245.718927162685,246.716450451385,247.713973740085,248.185819633594),
 .UNSPECIFIED.);
#1401=B_SPLINE_CURVE_WITH_KNOTS('',3,(#55092,#55093,#55094,#55095,#55096,
#55097,#55098,#55099,#55100,#55101),.UNSPECIFIED.,.F.,.F.,(4,1,1,1,1,1,
1,4),(235.619449019235,236.05777280532,237.05529609402,238.05281938272,
239.05034267142,240.04786596012,241.04538924882,241.902634326414),
 .UNSPECIFIED.);
#1402=B_SPLINE_CURVE_WITH_KNOTS('',3,(#55102,#55103,#55104,#55105,#55106,
#55107,#55108,#55109,#55110,#55111,#55112),.UNSPECIFIED.,.F.,.F.,(4,1,1,
1,1,1,1,1,4),(235.619449019235,235.743694275685,236.741217564385,237.738740853085,
238.736264141785,239.733787430485,240.731310719185,241.728834007885,241.902634326414),
 .UNSPECIFIED.);
#1403=B_SPLINE_CURVE_WITH_KNOTS('',3,(#55117,#55118,#55119,#55120,#55121,
#55122,#55123,#55124,#55125,#55126),.UNSPECIFIED.,.F.,.F.,(4,1,1,1,1,1,
1,4),(229.336263712055,230.07263307312,231.07015636182,232.06767965052,
233.06520293922,234.06272622792,235.06024951662,235.619449019235),
 .UNSPECIFIED.);
#1404=B_SPLINE_CURVE_WITH_KNOTS('',3,(#55127,#55128,#55129,#55130,#55131,
#55132,#55133,#55134,#55135,#55136),.UNSPECIFIED.,.F.,.F.,(4,1,1,1,1,1,
1,4),(229.336263712055,229.758554543485,230.756077832185,231.753601120885,
232.751124409585,233.748647698285,234.746170986985,235.619449019235),
 .UNSPECIFIED.);
#1405=B_SPLINE_CURVE_WITH_KNOTS('',3,(#55141,#55142,#55143,#55144,#55145,
#55146,#55147,#55148,#55149,#55150,#55151),.UNSPECIFIED.,.F.,.F.,(4,1,1,
1,1,1,1,1,4),(223.053078404876,223.08997005222,224.08749334092,225.08501662962,
226.08253991832,227.08006320702,228.07758649572,229.07510978442,229.336263712055),
 .UNSPECIFIED.);
#1406=B_SPLINE_CURVE_WITH_KNOTS('',3,(#55152,#55153,#55154,#55155,#55156,
#55157,#55158,#55159,#55160,#55161),.UNSPECIFIED.,.F.,.F.,(4,1,1,1,1,1,
1,4),(223.053078404876,223.773414811285,224.770938099985,225.768461388685,
226.765984677385,227.763507966085,228.761031254785,229.336263712055),
 .UNSPECIFIED.);
#1407=B_SPLINE_CURVE_WITH_KNOTS('',3,(#55166,#55167,#55168,#55169,#55170,
#55171,#55172,#55173,#55174,#55175),.UNSPECIFIED.,.F.,.F.,(4,1,1,1,1,1,
1,4),(216.769893097696,217.10483032002,218.10235360872,219.09987689742,
220.09740018612,221.09492347482,222.09244676352,223.053078404876),
 .UNSPECIFIED.);
#1408=B_SPLINE_CURVE_WITH_KNOTS('',3,(#55176,#55177,#55178,#55179,#55180,
#55181,#55182,#55183,#55184,#55185,#55186),.UNSPECIFIED.,.F.,.F.,(4,1,1,
1,1,1,1,1,4),(216.769893097696,216.790751790385,217.788275079085,218.785798367785,
219.783321656485,220.780844945185,221.778368233885,222.775891522585,223.053078404876),
 .UNSPECIFIED.);
#1409=B_SPLINE_CURVE_WITH_KNOTS('',3,(#55191,#55192,#55193,#55194,#55195,
#55196,#55197,#55198,#55199,#55200),.UNSPECIFIED.,.F.,.F.,(4,1,1,1,1,1,
1,4),(210.486707790517,211.11969058782,212.11721387652,213.11473716522,
214.11226045392,215.10978374262,216.10730703132,216.769893097696),
 .UNSPECIFIED.);
#1410=B_SPLINE_CURVE_WITH_KNOTS('',3,(#55201,#55202,#55203,#55204,#55205,
#55206,#55207,#55208,#55209,#55210),.UNSPECIFIED.,.F.,.F.,(4,1,1,1,1,1,
1,4),(210.486707790517,210.805612058185,211.803135346885,212.800658635585,
213.798181924285,214.795705212985,215.793228501685,216.769893097696),
 .UNSPECIFIED.);
#1411=B_SPLINE_CURVE_WITH_KNOTS('',3,(#55215,#55216,#55217,#55218,#55219,
#55220,#55221,#55222,#55223,#55224),.UNSPECIFIED.,.F.,.F.,(4,1,1,1,1,1,
1,4),(204.203522483337,205.13455085562,206.13207414432,207.12959743302,
208.12712072172,209.12464401042,210.12216729912,210.486707790517),
 .UNSPECIFIED.);
#1412=B_SPLINE_CURVE_WITH_KNOTS('',3,(#55225,#55226,#55227,#55228,#55229,
#55230,#55231,#55232,#55233,#55234),.UNSPECIFIED.,.F.,.F.,(4,1,1,1,1,1,
1,4),(204.203522483337,204.820472325985,205.817995614685,206.815518903385,
207.813042192085,208.810565480785,209.808088769485,210.486707790517),
 .UNSPECIFIED.);
#1413=B_SPLINE_CURVE_WITH_KNOTS('',3,(#55239,#55240,#55241,#55242,#55243,
#55244,#55245,#55246,#55247,#55248,#55249),.UNSPECIFIED.,.F.,.F.,(4,1,1,
1,1,1,1,1,4),(197.920337176158,198.15188783472,199.14941112342,200.14693441212,
201.14445770082,202.14198098952,203.13950427822,204.13702756692,204.203522483337),
 .UNSPECIFIED.);
#1414=B_SPLINE_CURVE_WITH_KNOTS('',3,(#55250,#55251,#55252,#55253,#55254,
#55255,#55256,#55257,#55258,#55259),.UNSPECIFIED.,.F.,.F.,(4,1,1,1,1,1,
1,4),(197.920337176158,198.835332593785,199.832855882485,200.830379171185,
201.827902459885,202.825425748585,203.822949037285,204.203522483337),
 .UNSPECIFIED.);
#1415=B_SPLINE_CURVE_WITH_KNOTS('',3,(#55264,#55265,#55266,#55267,#55268,
#55269,#55270,#55271,#55272,#55273),.UNSPECIFIED.,.F.,.F.,(4,1,1,1,1,1,
1,4),(191.637151868978,192.16674810252,193.16427139122,194.16179467992,
195.15931796862,196.15684125732,197.15436454602,197.920337176158),
 .UNSPECIFIED.);
#1416=B_SPLINE_CURVE_WITH_KNOTS('',3,(#55274,#55275,#55276,#55277,#55278,
#55279,#55280,#55281,#55282,#55283,#55284),.UNSPECIFIED.,.F.,.F.,(4,1,1,
1,1,1,1,1,4),(191.637151868978,191.852669572885,192.850192861585,193.847716150285,
194.845239438985,195.842762727685,196.840286016385,197.837809305085,197.920337176158),
 .UNSPECIFIED.);
#1417=B_SPLINE_CURVE_WITH_KNOTS('',3,(#55289,#55290,#55291,#55292,#55293,
#55294,#55295,#55296,#55297,#55298),.UNSPECIFIED.,.F.,.F.,(4,1,1,1,1,1,
1,4),(185.353966561798,186.18160837032,187.17913165902,188.17665494772,
189.17417823642,190.17170152512,191.16922481382,191.637151868978),
 .UNSPECIFIED.);
#1418=B_SPLINE_CURVE_WITH_KNOTS('',3,(#55299,#55300,#55301,#55302,#55303,
#55304,#55305,#55306,#55307,#55308),.UNSPECIFIED.,.F.,.F.,(4,1,1,1,1,1,
1,4),(185.353966561798,185.867529840685,186.865053129385,187.862576418085,
188.860099706785,189.857622995485,190.855146284185,191.637151868978),
 .UNSPECIFIED.);
#1419=B_SPLINE_CURVE_WITH_KNOTS('',3,(#55313,#55314,#55315,#55316,#55317,
#55318,#55319,#55320,#55321,#55322,#55323),.UNSPECIFIED.,.F.,.F.,(4,1,1,
1,1,1,1,1,4),(179.070781254619,179.19894534942,180.19646863812,181.19399192682,
182.19151521552,183.18903850422,184.18656179292,185.18408508162,185.353966561798),
 .UNSPECIFIED.);
#1420=B_SPLINE_CURVE_WITH_KNOTS('',3,(#55324,#55325,#55326,#55327,#55328,
#55329,#55330,#55331,#55332,#55333),.UNSPECIFIED.,.F.,.F.,(4,1,1,1,1,1,
1,4),(179.070781254619,179.882390108485,180.879913397185,181.877436685885,
182.874959974585,183.872483263285,184.870006551985,185.353966561798),
 .UNSPECIFIED.);
#1421=B_SPLINE_CURVE_WITH_KNOTS('',3,(#55338,#55339,#55340,#55341,#55342,
#55343,#55344,#55345,#55346,#55347),.UNSPECIFIED.,.F.,.F.,(4,1,1,1,1,1,
1,4),(172.787595947439,173.21380561722,174.21132890592,175.20885219462,
176.20637548332,177.20389877202,178.20142206072,179.070781254619),
 .UNSPECIFIED.);
#1422=B_SPLINE_CURVE_WITH_KNOTS('',3,(#55348,#55349,#55350,#55351,#55352,
#55353,#55354,#55355,#55356,#55357,#55358),.UNSPECIFIED.,.F.,.F.,(4,1,1,
1,1,1,1,1,4),(172.787595947439,172.899727087585,173.897250376285,174.894773664985,
175.892296953685,176.889820242385,177.887343531085,178.884866819785,179.070781254619),
 .UNSPECIFIED.);
#1423=B_SPLINE_CURVE_WITH_KNOTS('',3,(#55363,#55364,#55365,#55366,#55367,
#55368,#55369,#55370,#55371,#55372),.UNSPECIFIED.,.F.,.F.,(4,1,1,1,1,1,
1,4),(166.50441064026,167.22866588502,168.22618917372,169.22371246242,170.22123575112,
171.21875903982,172.21628232852,172.787595947439),.UNSPECIFIED.);
#1424=B_SPLINE_CURVE_WITH_KNOTS('',3,(#55373,#55374,#55375,#55376,#55377,
#55378,#55379,#55380,#55381,#55382),.UNSPECIFIED.,.F.,.F.,(4,1,1,1,1,1,
1,4),(166.50441064026,166.914587355385,167.912110644085,168.909633932785,
169.907157221485,170.904680510185,171.902203798885,172.787595947439),
 .UNSPECIFIED.);
#1425=B_SPLINE_CURVE_WITH_KNOTS('',3,(#55387,#55388,#55389,#55390,#55391,
#55392,#55393,#55394,#55395,#55396,#55397),.UNSPECIFIED.,.F.,.F.,(4,1,1,
1,1,1,1,1,4),(160.22122533308,160.24600286412,161.24352615282,162.24104944152,
163.23857273022,164.23609601892,165.23361930762,166.23114259632,166.50441064026),
 .UNSPECIFIED.);
#1426=B_SPLINE_CURVE_WITH_KNOTS('',3,(#55398,#55399,#55400,#55401,#55402,
#55403,#55404,#55405,#55406,#55407),.UNSPECIFIED.,.F.,.F.,(4,1,1,1,1,1,
1,4),(160.22122533308,160.929447623185,161.926970911885,162.924494200585,
163.922017489285,164.919540777985,165.917064066685,166.50441064026),
 .UNSPECIFIED.);
#1427=B_SPLINE_CURVE_WITH_KNOTS('',3,(#55412,#55413,#55414,#55415,#55416,
#55417,#55418,#55419,#55420,#55421),.UNSPECIFIED.,.F.,.F.,(4,1,1,1,1,1,
1,4),(153.938040025901,154.26086313192,155.25838642062,156.25590970932,
157.25343299802,158.25095628672,159.24847957542,160.22122533308),
 .UNSPECIFIED.);
#1428=B_SPLINE_CURVE_WITH_KNOTS('',3,(#55422,#55423,#55424,#55425,#55426,
#55427,#55428,#55429,#55430,#55431,#55432),.UNSPECIFIED.,.F.,.F.,(4,1,1,
1,1,1,1,1,4),(153.938040025901,153.946784602285,154.944307890985,155.941831179685,
156.939354468385,157.936877757085,158.934401045785,159.931924334485,160.22122533308),
 .UNSPECIFIED.);
#1429=B_SPLINE_CURVE_WITH_KNOTS('',3,(#55437,#55438,#55439,#55440,#55441,
#55442,#55443,#55444,#55445,#55446),.UNSPECIFIED.,.F.,.F.,(4,1,1,1,1,1,
1,4),(147.654854718721,148.27572339972,149.27324668842,150.27076997712,
151.26829326582,152.26581655452,153.26333984322,153.938040025901),
 .UNSPECIFIED.);
#1430=B_SPLINE_CURVE_WITH_KNOTS('',3,(#55447,#55448,#55449,#55450,#55451,
#55452,#55453,#55454,#55455,#55456),.UNSPECIFIED.,.F.,.F.,(4,1,1,1,1,1,
1,4),(147.654854718721,147.961644870085,148.959168158785,149.956691447485,
150.954214736185,151.951738024885,152.949261313585,153.938040025901),
 .UNSPECIFIED.);
#1431=B_SPLINE_CURVE_WITH_KNOTS('',3,(#55461,#55462,#55463,#55464,#55465,
#55466,#55467,#55468,#55469,#55470),.UNSPECIFIED.,.F.,.F.,(4,1,1,1,1,1,
1,4),(141.371669411541,142.29058366752,143.28810695622,144.28563024492,
145.28315353362,146.28067682232,147.27820011102,147.654854718721),
 .UNSPECIFIED.);
#1432=B_SPLINE_CURVE_WITH_KNOTS('',3,(#55471,#55472,#55473,#55474,#55475,
#55476,#55477,#55478,#55479,#55480),.UNSPECIFIED.,.F.,.F.,(4,1,1,1,1,1,
1,4),(141.371669411541,141.976505137885,142.974028426585,143.971551715285,
144.969075003985,145.966598292685,146.964121581385,147.654854718721),
 .UNSPECIFIED.);
#1433=B_SPLINE_CURVE_WITH_KNOTS('',3,(#55485,#55486,#55487,#55488,#55489,
#55490,#55491,#55492,#55493,#55494,#55495),.UNSPECIFIED.,.F.,.F.,(4,1,1,
1,1,1,1,1,4),(135.088484104362,135.30792064662,136.30544393532,137.30296722402,
138.30049051272,139.29801380142,140.29553709012,141.29306037882,141.371669411541),
 .UNSPECIFIED.);
#1434=B_SPLINE_CURVE_WITH_KNOTS('',3,(#55496,#55497,#55498,#55499,#55500,
#55501,#55502,#55503,#55504,#55505),.UNSPECIFIED.,.F.,.F.,(4,1,1,1,1,1,
1,4),(135.088484104362,135.991365405685,136.988888694385,137.986411983085,
138.983935271785,139.981458560485,140.978981849185,141.371669411541),
 .UNSPECIFIED.);
#1435=B_SPLINE_CURVE_WITH_KNOTS('',3,(#55510,#55511,#55512,#55513,#55514,
#55515,#55516,#55517,#55518,#55519),.UNSPECIFIED.,.F.,.F.,(4,1,1,1,1,1,
1,4),(128.805298797182,129.32278091442,130.32030420312,131.31782749182,
132.31535078052,133.31287406922,134.31039735792,135.088484104362),
 .UNSPECIFIED.);
#1436=B_SPLINE_CURVE_WITH_KNOTS('',3,(#55520,#55521,#55522,#55523,#55524,
#55525,#55526,#55527,#55528,#55529,#55530),.UNSPECIFIED.,.F.,.F.,(4,1,1,
1,1,1,1,1,4),(128.805298797182,129.008702384785,130.006225673485,131.003748962185,
132.001272250885,132.998795539585,133.996318828285,134.993842116985,135.088484104362),
 .UNSPECIFIED.);
#1437=B_SPLINE_CURVE_WITH_KNOTS('',3,(#55535,#55536,#55537,#55538,#55539,
#55540,#55541,#55542,#55543,#55544),.UNSPECIFIED.,.F.,.F.,(4,1,1,1,1,1,
1,4),(122.522113490003,123.33764118222,124.33516447092,125.33268775962,
126.33021104832,127.32773433702,128.32525762572,128.805298797182),
 .UNSPECIFIED.);
#1438=B_SPLINE_CURVE_WITH_KNOTS('',3,(#55545,#55546,#55547,#55548,#55549,
#55550,#55551,#55552,#55553,#55554),.UNSPECIFIED.,.F.,.F.,(4,1,1,1,1,1,
1,4),(122.522113490003,123.023562652585,124.021085941285,125.018609229985,
126.016132518685,127.013655807385,128.011179096085,128.805298797182),
 .UNSPECIFIED.);
#1439=B_SPLINE_CURVE_WITH_KNOTS('',3,(#55559,#55560,#55561,#55562,#55563,
#55564,#55565,#55566,#55567,#55568,#55569),.UNSPECIFIED.,.F.,.F.,(4,1,1,
1,1,1,1,1,4),(116.238928182823,116.35497816132,117.35250145002,118.35002473872,
119.34754802742,120.34507131612,121.34259460482,122.34011789352,122.522113490003),
 .UNSPECIFIED.);
#1440=B_SPLINE_CURVE_WITH_KNOTS('',3,(#55570,#55571,#55572,#55573,#55574,
#55575,#55576,#55577,#55578,#55579),.UNSPECIFIED.,.F.,.F.,(4,1,1,1,1,1,
1,4),(116.238928182823,117.038422920385,118.035946209085,119.033469497785,
120.030992786485,121.028516075185,122.026039363885,122.522113490003),
 .UNSPECIFIED.);
#1441=B_SPLINE_CURVE_WITH_KNOTS('',3,(#55584,#55585,#55586,#55587,#55588,
#55589,#55590,#55591,#55592,#55593),.UNSPECIFIED.,.F.,.F.,(4,1,1,1,1,1,
1,4),(109.955742875644,110.36983842912,111.36736171782,112.36488500652,
113.36240829522,114.35993158392,115.35745487262,116.238928182823),
 .UNSPECIFIED.);
#1442=B_SPLINE_CURVE_WITH_KNOTS('',3,(#55594,#55595,#55596,#55597,#55598,
#55599,#55600,#55601,#55602,#55603,#55604),.UNSPECIFIED.,.F.,.F.,(4,1,1,
1,1,1,1,1,4),(109.955742875644,110.055759899484,111.053283188184,112.050806476884,
113.048329765584,114.045853054284,115.043376342985,116.040899631685,116.238928182823),
 .UNSPECIFIED.);
#1443=B_SPLINE_CURVE_WITH_KNOTS('',3,(#55609,#55610,#55611,#55612,#55613,
#55614,#55615,#55616,#55617,#55618),.UNSPECIFIED.,.F.,.F.,(4,1,1,1,1,1,
1,4),(103.672557568464,104.38469869692,105.38222198562,106.37974527432,
107.37726856302,108.37479185172,109.37231514042,109.955742875644),
 .UNSPECIFIED.);
#1444=B_SPLINE_CURVE_WITH_KNOTS('',3,(#55619,#55620,#55621,#55622,#55623,
#55624,#55625,#55626,#55627,#55628),.UNSPECIFIED.,.F.,.F.,(4,1,1,1,1,1,
1,4),(103.672557568464,104.070620167284,105.068143455984,106.065666744684,
107.063190033384,108.060713322084,109.058236610784,109.955742875644),
 .UNSPECIFIED.);
#1445=B_SPLINE_CURVE_WITH_KNOTS('',3,(#55633,#55634,#55635,#55636,#55637,
#55638,#55639,#55640,#55641,#55642,#55643),.UNSPECIFIED.,.F.,.F.,(4,1,1,
1,1,1,1,1,4),(97.3893722612843,97.4020356760196,98.3995589647196,99.3970822534196,
100.39460554212,101.39212883082,102.38965211952,103.38717540822,103.672557568464),
 .UNSPECIFIED.);
#1446=B_SPLINE_CURVE_WITH_KNOTS('',3,(#55644,#55645,#55646,#55647,#55648,
#55649,#55650,#55651,#55652,#55653),.UNSPECIFIED.,.F.,.F.,(4,1,1,1,1,1,
1,4),(97.3893722612844,98.0854804350844,99.0830037237844,100.080527012484,
101.078050301184,102.075573589884,103.073096878584,103.672557568464),
 .UNSPECIFIED.);
#1447=B_SPLINE_CURVE_WITH_KNOTS('',3,(#55658,#55659,#55660,#55661,#55662,
#55663,#55664,#55665,#55666,#55667),.UNSPECIFIED.,.F.,.F.,(4,1,1,1,1,1,
1,4),(91.1061869541047,91.4168959438195,92.4144192325195,93.4119425212196,
94.4094658099196,95.4069890986196,96.4045123873196,97.3893722612843),
 .UNSPECIFIED.);
#1448=B_SPLINE_CURVE_WITH_KNOTS('',3,(#55668,#55669,#55670,#55671,#55672,
#55673,#55674,#55675,#55676,#55677),.UNSPECIFIED.,.F.,.F.,(4,1,1,1,1,1,
1,4),(91.1061869541048,92.1003407028844,93.0978639915844,94.0953872802844,
95.0929105689844,96.0904338576844,97.0879571463844,97.3893722612844),
 .UNSPECIFIED.);
#1449=B_SPLINE_CURVE_WITH_KNOTS('',3,(#55682,#55683,#55684,#55685,#55686,
#55687,#55688,#55689,#55690,#55691),.UNSPECIFIED.,.F.,.F.,(4,1,1,1,1,1,
1,4),(84.8230016469251,85.4317562116195,86.4292795003195,87.4268027890195,
88.4243260777195,89.4218493664195,90.4193726551195,91.1061869541047),
 .UNSPECIFIED.);
#1450=B_SPLINE_CURVE_WITH_KNOTS('',3,(#55692,#55693,#55694,#55695,#55696,
#55697,#55698,#55699,#55700,#55701,#55702),.UNSPECIFIED.,.F.,.F.,(4,1,1,
1,1,1,1,1,4),(84.8230016469252,85.1176776819843,86.1152009706843,87.1127242593844,
88.1102475480844,89.1077708367844,90.1052941254844,91.1028174141844,91.1061869541048),
 .UNSPECIFIED.);
#1451=B_SPLINE_CURVE_WITH_KNOTS('',3,(#55707,#55708,#55709,#55710,#55711,
#55712,#55713,#55714,#55715,#55716),.UNSPECIFIED.,.F.,.F.,(4,1,1,1,1,1,
1,4),(78.5398163397455,79.4466164794195,80.4441397681195,81.4416630568195,
82.4391863455195,83.4367096342195,84.4342329229195,84.8230016469251),
 .UNSPECIFIED.);
#1452=B_SPLINE_CURVE_WITH_KNOTS('',3,(#55717,#55718,#55719,#55720,#55721,
#55722,#55723,#55724,#55725,#55726),.UNSPECIFIED.,.F.,.F.,(4,1,1,1,1,1,
1,4),(78.5398163397456,79.1325379497843,80.1300612384843,81.1275845271843,
82.1251078158843,83.1226311045843,84.1201543932843,84.8230016469252),
 .UNSPECIFIED.);
#1453=B_SPLINE_CURVE_WITH_KNOTS('',3,(#55731,#55732,#55733,#55734,#55735,
#55736,#55737,#55738,#55739,#55740,#55741),.UNSPECIFIED.,.F.,.F.,(4,1,1,
1,1,1,1,1,4),(72.2566310325659,72.4639534585194,73.4614767472195,74.4590000359194,
75.4565233246195,76.4540466133195,77.4515699020195,78.4490931907195,78.5398163397455),
 .UNSPECIFIED.);
#1454=B_SPLINE_CURVE_WITH_KNOTS('',3,(#55742,#55743,#55744,#55745,#55746,
#55747,#55748,#55749,#55750,#55751),.UNSPECIFIED.,.F.,.F.,(4,1,1,1,1,1,
1,4),(72.256631032566,73.1473982175843,74.1449215062843,75.1424447949843,
76.1399680836843,77.1374913723843,78.1350146610843,78.5398163397456),
 .UNSPECIFIED.);
#1455=B_SPLINE_CURVE_WITH_KNOTS('',3,(#55756,#55757,#55758,#55759,#55760,
#55761,#55762,#55763,#55764,#55765),.UNSPECIFIED.,.F.,.F.,(4,1,1,1,1,1,
1,4),(65.9734457253863,66.4788137263194,67.4763370150194,68.4738603037194,
69.4713835924194,70.4689068811194,71.4664301698194,72.2566310325659),
 .UNSPECIFIED.);
#1456=B_SPLINE_CURVE_WITH_KNOTS('',3,(#55766,#55767,#55768,#55769,#55770,
#55771,#55772,#55773,#55774,#55775,#55776),.UNSPECIFIED.,.F.,.F.,(4,1,1,
1,1,1,1,1,4),(65.9734457253864,66.1647351966842,67.1622584853842,68.1597817740843,
69.1573050627842,70.1548283514843,71.1523516401843,72.1498749288843,72.256631032566),
 .UNSPECIFIED.);
#1457=B_SPLINE_CURVE_WITH_KNOTS('',3,(#55781,#55782,#55783,#55784,#55785,
#55786,#55787,#55788,#55789,#55790),.UNSPECIFIED.,.F.,.F.,(4,1,1,1,1,1,
1,4),(59.6902604182067,60.4936739941194,61.4911972828194,62.4887205715194,
63.4862438602194,64.4837671489194,65.4812904376194,65.9734457253863),
 .UNSPECIFIED.);
#1458=B_SPLINE_CURVE_WITH_KNOTS('',3,(#55791,#55792,#55793,#55794,#55795,
#55796,#55797,#55798,#55799,#55800),.UNSPECIFIED.,.F.,.F.,(4,1,1,1,1,1,
1,4),(59.6902604182069,60.1795954644842,61.1771187531842,62.1746420418842,
63.1721653305842,64.1696886192842,65.1672119079842,65.9734457253864),
 .UNSPECIFIED.);
#1459=B_SPLINE_CURVE_WITH_KNOTS('',3,(#55805,#55806,#55807,#55808,#55809,
#55810,#55811,#55812,#55813,#55814,#55815),.UNSPECIFIED.,.F.,.F.,(4,1,1,
1,1,1,1,1,4),(53.4070751110272,53.5110109732193,54.5085342619193,55.5060575506193,
56.5035808393194,57.5011041280194,58.4986274167194,59.4961507054194,59.6902604182067),
 .UNSPECIFIED.);
#1460=B_SPLINE_CURVE_WITH_KNOTS('',3,(#55816,#55817,#55818,#55819,#55820,
#55821,#55822,#55823,#55824,#55825),.UNSPECIFIED.,.F.,.F.,(4,1,1,1,1,1,
1,4),(53.4070751110273,54.1944557322842,55.1919790209842,56.1895023096842,
57.1870255983842,58.1845488870842,59.1820721757842,59.6902604182069),
 .UNSPECIFIED.);
#1461=B_SPLINE_CURVE_WITH_KNOTS('',3,(#55830,#55831,#55832,#55833,#55834,
#55835,#55836,#55837,#55838,#55839),.UNSPECIFIED.,.F.,.F.,(4,1,1,1,1,1,
1,4),(47.1238898038476,47.5258712410193,48.5233945297193,49.5209178184193,
50.5184411071193,51.5159643958193,52.5134876845193,53.4070751110272),
 .UNSPECIFIED.);
#1462=B_SPLINE_CURVE_WITH_KNOTS('',3,(#55840,#55841,#55842,#55843,#55844,
#55845,#55846,#55847,#55848,#55849,#55850),.UNSPECIFIED.,.F.,.F.,(4,1,1,
1,1,1,1,1,4),(47.1238898038477,47.2117927113841,48.2093160000841,49.2068392887841,
50.2043625774841,51.2018858661842,52.1994091548842,53.1969324435842,53.4070751110273),
 .UNSPECIFIED.);
#1463=B_SPLINE_CURVE_WITH_KNOTS('',3,(#55855,#55856,#55857,#55858,#55859,
#55860,#55861,#55862,#55863,#55864),.UNSPECIFIED.,.F.,.F.,(4,1,1,1,1,1,
1,4),(40.840704496668,41.5407315088193,42.5382547975193,43.5357780862193,
44.5333013749193,45.5308246636193,46.5283479523193,47.1238898038476),
 .UNSPECIFIED.);
#1464=B_SPLINE_CURVE_WITH_KNOTS('',3,(#55865,#55866,#55867,#55868,#55869,
#55870,#55871,#55872,#55873,#55874),.UNSPECIFIED.,.F.,.F.,(4,1,1,1,1,1,
1,4),(40.8407044966681,41.2266529791841,42.2241762678841,43.2216995565841,
44.2192228452841,45.2167461339841,46.2142694226841,47.1238898038477),
 .UNSPECIFIED.);
#1465=B_SPLINE_CURVE_WITH_KNOTS('',3,(#55879,#55880,#55881,#55882,#55883,
#55884,#55885,#55886,#55887,#55888,#55889),.UNSPECIFIED.,.F.,.F.,(4,1,1,
1,1,1,1,1,4),(34.5575191894884,34.5580684879192,35.5555917766192,36.5531150653192,
37.5506383540192,38.5481616427193,39.5456849314193,40.5432082201193,40.840704496668),
 .UNSPECIFIED.);
#1466=B_SPLINE_CURVE_WITH_KNOTS('',3,(#55890,#55891,#55892,#55893,#55894,
#55895,#55896,#55897,#55898,#55899),.UNSPECIFIED.,.F.,.F.,(4,1,1,1,1,1,
1,4),(34.5575191894885,35.2415132469841,36.2390365356841,37.2365598243841,
38.2340831130841,39.2316064017841,40.2291296904841,40.8407044966681),
 .UNSPECIFIED.);
#1467=B_SPLINE_CURVE_WITH_KNOTS('',3,(#55904,#55905,#55906,#55907,#55908,
#55909,#55910,#55911,#55912,#55913),.UNSPECIFIED.,.F.,.F.,(4,1,1,1,1,1,
1,4),(28.2743338823088,28.5729287557192,29.5704520444192,30.5679753331192,
31.5654986218192,32.5630219105192,33.5605451992192,34.5575191894884),
 .UNSPECIFIED.);
#1468=B_SPLINE_CURVE_WITH_KNOTS('',3,(#55914,#55915,#55916,#55917,#55918,
#55919,#55920,#55921,#55922,#55923),.UNSPECIFIED.,.F.,.F.,(4,1,1,1,1,1,
1,4),(28.2743338823089,29.256373514784,30.253896803484,31.251420092184,
32.2489433808841,33.2464666695841,34.2439899582841,34.5575191894885),
 .UNSPECIFIED.);
#1469=B_SPLINE_CURVE_WITH_KNOTS('',3,(#55928,#55929,#55930,#55931,#55932,
#55933,#55934,#55935,#55936,#55937),.UNSPECIFIED.,.F.,.F.,(4,1,1,1,1,1,
1,4),(21.9911485751292,22.5877890235192,23.5853123122192,24.5828356009192,
25.5803588896192,26.5778821783192,27.5754054670192,28.2743338823088),
 .UNSPECIFIED.);
#1470=B_SPLINE_CURVE_WITH_KNOTS('',3,(#55938,#55939,#55940,#55941,#55942,
#55943,#55944,#55945,#55946,#55947,#55948),.UNSPECIFIED.,.F.,.F.,(4,1,1,
1,1,1,1,1,4),(21.9911485751293,22.273710493884,23.271233782584,24.268757071284,
25.266280359984,26.263803648684,27.261326937384,28.258850226084,28.2743338823089),
 .UNSPECIFIED.);
#1471=B_SPLINE_CURVE_WITH_KNOTS('',3,(#55953,#55954,#55955,#55956,#55957,
#55958,#55959,#55960,#55961,#55962),.UNSPECIFIED.,.F.,.F.,(4,1,1,1,1,1,
1,4),(15.7079632679496,16.6026492913191,17.6001725800191,18.5976958687191,
19.5952191574192,20.5927424461192,21.5902657348192,21.9911485751292),
 .UNSPECIFIED.);
#1472=B_SPLINE_CURVE_WITH_KNOTS('',3,(#55963,#55964,#55965,#55966,#55967,
#55968,#55969,#55970,#55971,#55972),.UNSPECIFIED.,.F.,.F.,(4,1,1,1,1,1,
1,4),(15.7079632679497,16.288570761684,17.286094050384,18.283617339084,
19.281140627784,20.278663916484,21.276187205184,21.9911485751293),
 .UNSPECIFIED.);
#1473=B_SPLINE_CURVE_WITH_KNOTS('',3,(#57514,#57515,#57516,#57517,#57518,
#57519,#57520,#57521,#57522,#57523,#57524,#57525,#57526,#57527,#57528,#57529,
#57530,#57531,#57532,#57533,#57534,#57535,#57536,#57537,#57538,#57539,#57540,
#57541,#57542,#57543,#57544,#57545,#57546,#57547,#57548,#57549,#57550,#57551,
#57552,#57553,#57554,#57555,#57556,#57557,#57558,#57559,#57560,#57561,#57562,
#57563,#57564,#57565,#57566,#57567,#57568,#57569,#57570,#57571,#57572,#57573,
#57574,#57575,#57576,#57577,#57578,#57579,#57580,#57581,#57582,#57583,#57584,
#57585,#57586,#57587,#57588,#57589,#57590,#57591,#57592,#57593,#57594,#57595,
#57596,#57597,#57598,#57599,#57600,#57601,#57602,#57603,#57604,#57605,#57606,
#57607,#57608,#57609,#57610,#57611,#57612,#57613,#57614,#57615,#57616,#57617,
#57618,#57619,#57620,#57621,#57622),.UNSPECIFIED.,.F.,.F.,(4,3,3,3,3,3,
3,3,3,3,3,3,3,3,3,3,3,3,3,3,3,3,3,3,3,3,3,3,3,3,3,3,3,3,3,3,4),(0.,0.0359628151845056,
0.0790640675124802,0.122944974172411,0.167078080679047,0.180430545026742,
0.19037773183983,0.196180338284082,0.239492682886256,0.282925566791464,
0.325969530232972,0.368238370501489,0.375078460706215,0.381042467863404,
0.42346125387141,0.465393907031249,0.506323913773678,0.51599109870151,0.544714566753401,
0.554178082246963,0.559723896450525,0.565364051500323,0.606359797650403,
0.648015429264718,0.689524423166306,0.717651633141474,0.732581126571207,
0.739096451862393,0.745778843116641,0.786822056096576,0.827804944486442,
0.845389038445888,0.853674880949773,0.860823772315063,0.901249933519242,
0.94103892518765,0.96847769616201),.UNSPECIFIED.);
#1474=B_SPLINE_CURVE_WITH_KNOTS('',3,(#57623,#57624,#57625,#57626,#57627,
#57628,#57629,#57630,#57631,#57632,#57633,#57634,#57635,#57636,#57637,#57638,
#57639,#57640,#57641),.UNSPECIFIED.,.F.,.F.,(4,3,3,3,3,3,4),(371.824326632282,
372.076186685102,373.073709973802,374.071233262502,375.068756551202,376.066279839902,
376.991118430775),.UNSPECIFIED.);
#1475=B_SPLINE_CURVE_WITH_KNOTS('',3,(#57643,#57644,#57645,#57646,#57647,
#57648,#57649,#57650,#57651,#57652,#57653,#57654,#57655,#57656,#57657,#57658,
#57659,#57660,#57661,#57662,#57663,#57664,#57665,#57666,#57667,#57668,#57669,
#57670,#57671,#57672,#57673,#57674,#57675,#57676,#57677,#57678,#57679,#57680,
#57681,#57682,#57683,#57684,#57685,#57686,#57687,#57688,#57689,#57690,#57691,
#57692,#57693,#57694,#57695,#57696,#57697,#57698,#57699,#57700,#57701,#57702,
#57703,#57704,#57705,#57706,#57707,#57708,#57709,#57710,#57711,#57712,#57713,
#57714,#57715,#57716,#57717,#57718,#57719,#57720,#57721,#57722,#57723,#57724,
#57725,#57726,#57727,#57728,#57729,#57730,#57731,#57732,#57733,#57734,#57735,
#57736,#57737,#57738,#57739,#57740,#57741,#57742,#57743,#57744,#57745,#57746,
#57747,#57748),.UNSPECIFIED.,.F.,.F.,(4,3,3,3,3,3,3,3,3,3,3,3,3,3,3,3,3,
3,3,3,3,3,3,3,3,3,3,3,3,3,3,3,3,3,3,4),(-0.968477696161913,-0.936462781732006,
-0.897034237282827,-0.871088158002514,-0.855755616551603,-0.849836345176422,
-0.809673382933614,-0.76870133116664,-0.750776058518589,-0.741856737530979,
-0.7341371378361,-0.692655598295136,-0.650704137993651,-0.608502345694694,
-0.576851001470477,-0.56347054188062,-0.556078670388381,-0.513475355214464,
-0.481896968797825,-0.440388916382611,-0.398291621794682,-0.386095361159993,
-0.379050278062876,-0.373539380612515,-0.331389873213074,-0.287819274607371,
-0.244248676001668,-0.213717591501459,-0.200360242032618,-0.19269654176718,
-0.1869673316623,-0.143586522253231,-0.0997397595963603,-0.0560111116848197,
-0.0129407155146067,0.),.UNSPECIFIED.);
#1476=B_SPLINE_CURVE_WITH_KNOTS('',3,(#57749,#57750,#57751,#57752,#57753,
#57754,#57755,#57756,#57757),.UNSPECIFIED.,.F.,.F.,(4,1,1,1,1,1,4),(10.3761157273111,
11.3009543181839,12.2984776068839,13.2960008955839,14.2935241842839,15.291047472984,
15.7079632679497),.UNSPECIFIED.);
#1477=B_SPLINE_CURVE_WITH_KNOTS('',3,(#57761,#57762,#57763,#57764,#57765,
#57766,#57767,#57768,#57769),.UNSPECIFIED.,.F.,.F.,(4,1,1,1,1,1,4),(11.6150328478191,
12.1137944921691,12.6125561365191,13.6100794252191,14.6076027139191,15.6051260026191,
15.7079632679496),.UNSPECIFIED.);
#1478=B_SPLINE_CURVE_WITH_KNOTS('',3,(#59311,#59312,#59313,#59314,#59315,
#59316,#59317,#59318,#59319,#59320,#59321,#59322,#59323,#59324,#59325,#59326,
#59327,#59328,#59329,#59330,#59331,#59332,#59333,#59334,#59335,#59336,#59337,
#59338,#59339,#59340,#59341,#59342,#59343,#59344,#59345,#59346,#59347,#59348,
#59349,#59350,#59351,#59352,#59353,#59354,#59355,#59356,#59357,#59358,#59359,
#59360,#59361,#59362,#59363,#59364,#59365,#59366,#59367,#59368,#59369,#59370,
#59371,#59372,#59373,#59374,#59375,#59376,#59377,#59378,#59379,#59380,#59381,
#59382,#59383,#59384,#59385,#59386,#59387,#59388,#59389,#59390,#59391,#59392,
#59393,#59394,#59395,#59396,#59397,#59398,#59399,#59400,#59401,#59402,#59403,
#59404,#59405,#59406,#59407,#59408,#59409,#59410,#59411,#59412,#59413,#59414,
#59415,#59416,#59417,#59418,#59419),.UNSPECIFIED.,.F.,.F.,(4,3,3,3,3,3,
3,3,3,3,3,3,3,3,3,3,3,3,3,3,3,3,3,3,3,3,3,3,3,3,3,3,3,3,3,3,4),(0.,0.0319610084124964,
0.0709970802367925,0.110918019903594,0.151489267836741,0.166268550959158,
0.172136820332691,0.17773227169752,0.218621519728627,0.260105203172031,
0.301749535598996,0.343042584632714,0.348577800050639,0.354310610465885,
0.396643769367683,0.438881645932778,0.480394489143215,0.485838103022159,
0.515447494563868,0.527322668925359,0.533096841618444,0.574119197999633,
0.616402831080215,0.659075854182062,0.69089454476895,0.706803890062393,
0.714443723340302,0.720575125052056,0.722713235355837,0.765747942600601,
0.80908641486819,0.828699390062085,0.838036583520388,0.844245630783005,
0.888067982944121,0.931632292905962,0.965990216419354),.UNSPECIFIED.);
#1479=B_SPLINE_CURVE_WITH_KNOTS('',3,(#59420,#59421,#59422,#59423,#59424,
#59425,#59426,#59427,#59428,#59429,#59430,#59431,#59432,#59433,#59434,#59435,
#59436,#59437,#59438,#59439,#59440,#59441,#59442,#59443,#59444,#59445,#59446,
#59447,#59448,#59449,#59450,#59451,#59452,#59453,#59454,#59455,#59456,#59457,
#59458,#59459,#59460,#59461,#59462,#59463,#59464,#59465,#59466,#59467,#59468,
#59469,#59470,#59471,#59472,#59473,#59474,#59475,#59476,#59477,#59478,#59479,
#59480,#59481,#59482,#59483,#59484,#59485,#59486,#59487,#59488,#59489,#59490,
#59491,#59492,#59493,#59494,#59495,#59496,#59497,#59498,#59499,#59500,#59501,
#59502,#59503,#59504,#59505,#59506,#59507,#59508,#59509,#59510,#59511,#59512,
#59513,#59514,#59515,#59516,#59517,#59518,#59519,#59520,#59521,#59522),
 .UNSPECIFIED.,.F.,.F.,(4,3,3,3,3,3,3,3,3,3,3,3,3,3,3,3,3,3,3,3,3,3,3,3,
3,3,3,3,3,3,3,3,3,3,4),(-0.965990216419533,-0.930132396483882,-0.886600314752691,
-0.859427241407658,-0.844575649172136,-0.83450269382505,-0.791217440053876,
-0.748794152701163,-0.730233964484351,-0.71490535117285,-0.708744621568391,
-0.665691199232105,-0.622727628938354,-0.580003507011809,-0.5479604155669,
-0.535021607402038,-0.529041072836267,-0.487381790675506,-0.451831141232172,
-0.409951411560376,-0.367982065107459,-0.353448430125576,-0.345247061313217,
-0.304116472475951,-0.262917042414806,-0.222498465588061,-0.194686157389553,
-0.181409937644946,-0.17316340151046,-0.167260443835079,-0.125445332876309,
-0.0850027204681986,-0.0449509623998064,-0.00571310113625183,0.),
 .UNSPECIFIED.);
#1480=B_SPLINE_CURVE_WITH_KNOTS('',3,(#59523,#59524,#59525,#59526,#59527,
#59528,#59529,#59530,#59531,#59532,#59533,#59534,#59535,#59536,#59537,#59538,
#59539,#59540,#59541),.UNSPECIFIED.,.F.,.F.,(4,3,3,3,3,3,4),(-379.058849706002,
-378.560088061652,-378.061326417302,-377.063803128602,-376.066279839902,
-375.068756551202,-374.800863543725),.UNSPECIFIED.);
#1481=B_SPLINE_CURVE_WITH_KNOTS('',3,(#59598,#59599,#59600,#59601,#59602,
#59603,#59604),.UNSPECIFIED.,.F.,.F.,(4,3,4),(51.5745014586045,51.7886578973478,
52.2818832106559),.UNSPECIFIED.);
#1482=B_SPLINE_CURVE_WITH_KNOTS('',3,(#59607,#59608,#59609,#59610,#59611,
#59612,#59613,#59614,#59615,#59616),.UNSPECIFIED.,.F.,.F.,(4,3,3,4),(-50.2654824574367,
-49.3225313308074,-48.3360807041913,-47.8312715558983),.UNSPECIFIED.);
#1483=B_SPLINE_CURVE_WITH_KNOTS('',3,(#59621,#59622,#59623,#59624,#59625,
#59626,#59627,#59628,#59629,#59630,#59631,#59632,#59633,#59634,#59635,#59636,
#59637,#59638,#59639,#59640,#59641,#59642,#59643,#59644,#59645),
 .UNSPECIFIED.,.F.,.F.,(4,3,3,3,3,3,3,3,4),(45.291316151425,45.3767288243428,
46.363179450959,47.3496300775751,48.3360807041913,49.3225313308074,50.3089819574236,
51.2954325840397,51.5745014586045),.UNSPECIFIED.);
#1484=B_SPLINE_CURVE_WITH_KNOTS('',3,(#59646,#59647,#59648,#59649,#59650,
#59651,#59652,#59653,#59654,#59655,#59656,#59657,#59658,#59659,#59660,#59661,
#59662,#59663,#59664,#59665,#59666,#59667),.UNSPECIFIED.,.F.,.F.,(4,3,3,
3,3,3,3,4),(-47.8312715558983,-47.3496300775751,-46.363179450959,-45.3767288243428,
-44.3902781977267,-43.4038275711106,-42.4173769444944,-41.5480862487187),
 .UNSPECIFIED.);
#1485=B_SPLINE_CURVE_WITH_KNOTS('',3,(#59672,#59673,#59674,#59675,#59676,
#59677,#59678,#59679,#59680,#59681,#59682,#59683,#59684,#59685,#59686,#59687,
#59688,#59689,#59690,#59691,#59692,#59693),.UNSPECIFIED.,.F.,.F.,(4,3,3,
3,3,3,3,4),(39.0081308442454,39.458025064646,40.4444756912621,41.4309263178782,
42.4173769444944,43.4038275711105,44.3902781977267,45.291316151425),
 .UNSPECIFIED.);
#1486=B_SPLINE_CURVE_WITH_KNOTS('',3,(#59694,#59695,#59696,#59697,#59698,
#59699,#59700,#59701,#59702,#59703,#59704,#59705,#59706,#59707,#59708,#59709,
#59710,#59711,#59712,#59713,#59714,#59715,#59716,#59717,#59718),
 .UNSPECIFIED.,.F.,.F.,(4,3,3,3,3,3,3,3,4),(-41.5480862487187,-41.4309263178783,
-40.4444756912621,-39.458025064646,-38.4715744380298,-37.4851238114137,
-36.4986731847975,-35.5122225581814,-35.2649009415391),.UNSPECIFIED.);
#1487=B_SPLINE_CURVE_WITH_KNOTS('',3,(#59723,#59724,#59725,#59726,#59727,
#59728,#59729,#59730,#59731,#59732,#59733,#59734,#59735,#59736,#59737,#59738,
#59739,#59740,#59741,#59742,#59743,#59744),.UNSPECIFIED.,.F.,.F.,(4,3,3,
3,3,3,3,4),(32.7249455370658,33.5393213049491,34.5257719315652,35.5122225581814,
36.4986731847975,37.4851238114137,38.4715744380298,39.0081308442454),
 .UNSPECIFIED.);
#1488=B_SPLINE_CURVE_WITH_KNOTS('',3,(#59745,#59746,#59747,#59748,#59749,
#59750,#59751,#59752,#59753,#59754,#59755,#59756,#59757,#59758,#59759,#59760,
#59761,#59762,#59763,#59764,#59765,#59766),.UNSPECIFIED.,.F.,.F.,(4,3,3,
3,3,3,3,4),(-35.2649009415391,-34.5257719315652,-33.5393213049491,-32.5528706783329,
-31.5664200517168,-30.5799694251006,-29.5935187984845,-28.9817156343595),
 .UNSPECIFIED.);
#1489=B_SPLINE_CURVE_WITH_KNOTS('',3,(#59771,#59772,#59773,#59774,#59775,
#59776,#59777,#59778,#59779,#59780,#59781,#59782,#59783,#59784,#59785,#59786,
#59787,#59788,#59789,#59790,#59791,#59792,#59793,#59794,#59795),
 .UNSPECIFIED.,.F.,.F.,(4,3,3,3,3,3,3,3,4),(26.4417602298862,26.634166918636,
27.6206175452522,28.6070681718683,29.5935187984845,30.5799694251006,31.5664200517168,
32.5528706783329,32.7249455370658),.UNSPECIFIED.);
#1490=B_SPLINE_CURVE_WITH_KNOTS('',3,(#59796,#59797,#59798,#59799,#59800,
#59801,#59802,#59803,#59804,#59805,#59806,#59807,#59808,#59809,#59810,#59811,
#59812,#59813,#59814,#59815,#59816,#59817),.UNSPECIFIED.,.F.,.F.,(4,3,3,
3,3,3,3,4),(-28.9817156343595,-28.6070681718683,-27.6206175452522,-26.634166918636,
-25.6477162920199,-24.6612656654037,-23.6748150387876,-22.6985303271799),
 .UNSPECIFIED.);
#1491=B_SPLINE_CURVE_WITH_KNOTS('',3,(#59822,#59823,#59824,#59825,#59826,
#59827,#59828,#59829,#59830,#59831,#59832,#59833,#59834,#59835,#59836,#59837,
#59838,#59839,#59840,#59841,#59842,#59843),.UNSPECIFIED.,.F.,.F.,(4,3,3,
3,3,3,3,4),(20.1585749227066,20.7154631589391,21.7019137855553,22.6883644121714,
23.6748150387876,24.6612656654037,25.6477162920199,26.4417602298862),
 .UNSPECIFIED.);
#1492=B_SPLINE_CURVE_WITH_KNOTS('',3,(#59844,#59845,#59846,#59847,#59848,
#59849,#59850,#59851,#59852,#59853,#59854,#59855,#59856,#59857,#59858,#59859,
#59860,#59861,#59862,#59863,#59864,#59865,#59866,#59867,#59868),
 .UNSPECIFIED.,.F.,.F.,(4,3,3,3,3,3,3,3,4),(-22.6985303271799,-22.6883644121714,
-21.7019137855553,-20.7154631589391,-19.729012532323,-18.7425619057068,
-17.7561112790907,-16.7696606524745,-16.4153450200003),.UNSPECIFIED.);
#1493=B_SPLINE_CURVE_WITH_KNOTS('',3,(#59873,#59874,#59875,#59876,#59877,
#59878,#59879,#59880,#59881,#59882,#59883,#59884,#59885,#59886,#59887,#59888,
#59889,#59890,#59891,#59892,#59893,#59894),.UNSPECIFIED.,.F.,.F.,(4,3,3,
3,3,3,3,4),(13.875389615527,14.7967593992422,15.7832100258584,16.7696606524745,
17.7561112790907,18.7425619057068,19.729012532323,20.1585749227066),
 .UNSPECIFIED.);
#1494=B_SPLINE_CURVE_WITH_KNOTS('',3,(#59895,#59896,#59897,#59898,#59899,
#59900,#59901,#59902,#59903,#59904,#59905,#59906,#59907,#59908,#59909,#59910,
#59911,#59912,#59913,#59914,#59915,#59916),.UNSPECIFIED.,.F.,.F.,(4,3,3,
3,3,3,3,4),(-16.4153450200003,-15.7832100258584,-14.7967593992422,-13.8103087726261,
-12.8238581460099,-11.8374075193938,-10.8509568927776,-10.1321597128207),
 .UNSPECIFIED.);
#1495=B_SPLINE_CURVE_WITH_KNOTS('',3,(#59922,#59923,#59924,#59925,#59926,
#59927,#59928,#59929,#59930,#59931,#59932,#59933,#59934,#59935,#59936,#59937),
 .UNSPECIFIED.,.F.,.F.,(4,3,3,3,3,4),(-3.84897440564117,-2.95935187984845,
-1.9729012532323,-0.986450626616147,-0.493225313308074,0.),
 .UNSPECIFIED.);
#1496=B_SPLINE_CURVE_WITH_KNOTS('',3,(#59940,#59941,#59942,#59943,#59944,
#59945,#59946,#59947,#59948,#59949,#59950,#59951,#59952,#59953,#59954,#59955,
#59956,#59957,#59958),.UNSPECIFIED.,.F.,.F.,(4,3,3,3,3,3,4),(2.01640075321919,
2.95935187984845,3.9458025064646,4.93225313308074,5.9187037596969,6.90515438631305,
7.59220430834742),.UNSPECIFIED.);
#1497=B_SPLINE_CURVE_WITH_KNOTS('',3,(#59964,#59965,#59966,#59967,#59968,
#59969,#59970,#59971,#59972),.UNSPECIFIED.,.F.,.F.,(4,1,1,1,1,1,4),(59.6902604182061,
60.1950695664991,61.1815201931152,62.1679708197314,63.1544214463475,63.6476467596556,
64.1408720729637),.UNSPECIFIED.);
#1498=B_SPLINE_CURVE_WITH_KNOTS('',3,(#59975,#59976,#59977,#59978,#59979,
#59980,#59981,#59982,#59983),.UNSPECIFIED.,.F.,.F.,(4,1,1,1,1,1,4),(59.6902604182061,
59.7756730911239,60.7621237177401,61.7485743443562,62.7350249709724,63.7214755975885,
64.6644267242178),.UNSPECIFIED.);
#1499=B_SPLINE_CURVE_WITH_KNOTS('',3,(#59988,#59989,#59990,#59991,#59992,
#59993,#59994,#59995,#59996,#59997),.UNSPECIFIED.,.F.,.F.,(4,1,1,1,1,1,
1,4),(53.4070751110265,54.2763658068022,55.2628164334183,56.2492670600345,
57.2357176866506,58.2221683132668,59.2086189398829,59.6902604182061),
 .UNSPECIFIED.);
#1500=B_SPLINE_CURVE_WITH_KNOTS('',3,(#59998,#59999,#60000,#60001,#60002,
#60003,#60004,#60005,#60006,#60007),.UNSPECIFIED.,.F.,.F.,(4,1,1,1,1,1,
1,4),(53.4070751110265,53.856969331427,54.8434199580432,55.8298705846593,
56.8163212112755,57.8027718378916,58.7892224645078,59.6902604182061),
 .UNSPECIFIED.);
#1501=B_SPLINE_CURVE_WITH_KNOTS('',3,(#60012,#60013,#60014,#60015,#60016,
#60017,#60018,#60019,#60020,#60021,#60022),.UNSPECIFIED.,.F.,.F.,(4,1,1,
1,1,1,1,1,4),(47.1238898038469,47.3712114204891,48.3576620471053,49.3441126737214,
50.3305633003376,51.3170139269537,52.3034645535699,53.289915180186,53.4070751110265),
 .UNSPECIFIED.);
#1502=B_SPLINE_CURVE_WITH_KNOTS('',3,(#60023,#60024,#60025,#60026,#60027,
#60028,#60029,#60030,#60031,#60032),.UNSPECIFIED.,.F.,.F.,(4,1,1,1,1,1,
1,4),(47.1238898038469,47.9382655717301,48.9247161983463,49.9111668249625,
50.8976174515786,51.8840680781948,52.8705187048109,53.4070751110265),
 .UNSPECIFIED.);
#1503=B_SPLINE_CURVE_WITH_KNOTS('',3,(#60037,#60038,#60039,#60040,#60041,
#60042,#60043,#60044,#60045,#60046),.UNSPECIFIED.,.F.,.F.,(4,1,1,1,1,1,
1,4),(40.8407044966673,41.4525076607923,42.4389582874084,43.4254089140245,
44.4118595406407,45.3983101672568,46.384760793873,47.1238898038469),
 .UNSPECIFIED.);
#1504=B_SPLINE_CURVE_WITH_KNOTS('',3,(#60047,#60048,#60049,#60050,#60051,
#60052,#60053,#60054,#60055,#60056,#60057),.UNSPECIFIED.,.F.,.F.,(4,1,1,
1,1,1,1,1,4),(40.8407044966673,41.0331111854171,42.0195618120333,43.0060124386494,
43.9924630652656,44.9789136918817,45.9653643184979,46.951814945114,47.1238898038469),
 .UNSPECIFIED.);
#1505=B_SPLINE_CURVE_WITH_KNOTS('',3,(#60062,#60063,#60064,#60065,#60066,
#60067,#60068,#60069,#60070,#60071),.UNSPECIFIED.,.F.,.F.,(4,1,1,1,1,1,
1,4),(34.5575191894877,35.5338039010954,36.5202545277115,37.5067051543277,
38.4931557809438,39.47960640756,40.4660570341761,40.8407044966673),
 .UNSPECIFIED.);
#1506=B_SPLINE_CURVE_WITH_KNOTS('',3,(#60072,#60073,#60074,#60075,#60076,
#60077,#60078,#60079,#60080,#60081),.UNSPECIFIED.,.F.,.F.,(4,1,1,1,1,1,
1,4),(34.5575191894877,35.1144074257202,36.1008580523364,37.0873086789525,
38.0737593055687,39.0602099321848,40.046660558801,40.8407044966673),
 .UNSPECIFIED.);
#1507=B_SPLINE_CURVE_WITH_KNOTS('',3,(#60086,#60087,#60088,#60089,#60090,
#60091,#60092,#60093,#60094,#60095,#60096),.UNSPECIFIED.,.F.,.F.,(4,1,1,
1,1,1,1,1,4),(28.2743338823081,28.6286495147823,29.6151001413985,30.6015507680146,
31.5880013946308,32.5744520212469,33.5609026478631,34.5473532744792,34.5575191894877),
 .UNSPECIFIED.);
#1508=B_SPLINE_CURVE_WITH_KNOTS('',3,(#60097,#60098,#60099,#60100,#60101,
#60102,#60103,#60104,#60105,#60106),.UNSPECIFIED.,.F.,.F.,(4,1,1,1,1,1,
1,4),(28.2743338823081,29.1957036660233,30.1821542926395,31.1686049192556,
32.1550555458718,33.1415061724879,34.1279567991041,34.5575191894877),
 .UNSPECIFIED.);
#1509=B_SPLINE_CURVE_WITH_KNOTS('',3,(#60111,#60112,#60113,#60114,#60115,
#60116,#60117,#60118,#60119,#60120),.UNSPECIFIED.,.F.,.F.,(4,1,1,1,1,1,
1,4),(21.9911485751285,22.7099457550854,23.6963963817016,24.6828470083177,
25.6692976349339,26.65574826155,27.6421988881662,28.2743338823081),
 .UNSPECIFIED.);
#1510=B_SPLINE_CURVE_WITH_KNOTS('',3,(#60121,#60122,#60123,#60124,#60125,
#60126,#60127,#60128,#60129,#60130,#60131),.UNSPECIFIED.,.F.,.F.,(4,1,1,
1,1,1,1,1,4),(21.9911485751285,22.2905492797103,23.2769999063264,24.2634505329426,
25.2499011595587,26.2363517861749,27.222802412791,28.2092530394072,28.2743338823081),
 .UNSPECIFIED.);
#1511=B_SPLINE_CURVE_WITH_KNOTS('',3,(#60137,#60138,#60139,#60140,#60141,
#60142),.UNSPECIFIED.,.F.,.F.,(4,1,1,4),(14.3989442667811,14.8921695800892,
15.3853948933972,15.7079632679489),.UNSPECIFIED.);
#1512=B_SPLINE_CURVE_WITH_KNOTS('',3,(#60145,#60146,#60147,#60148,#60149),
 .UNSPECIFIED.,.F.,.F.,(4,1,4),(13.875389615527,14.8183407421562,15.7079632679489),
 .UNSPECIFIED.);
#1513=B_SPLINE_CURVE_WITH_KNOTS('',3,(#60151,#60152,#60153,#60154,#60155,
#60156,#60157,#60158,#60159,#60160,#60161),.UNSPECIFIED.,.F.,.F.,(4,1,1,
1,1,1,1,1,4),(15.7079632679489,15.8047913687724,16.7912419953885,17.7776926220047,
18.7641432486208,19.750593875237,20.7370445018531,21.7234951284693,21.9911485751285),
 .UNSPECIFIED.);
#1514=B_SPLINE_CURVE_WITH_KNOTS('',3,(#60162,#60163,#60164,#60165,#60166,
#60167,#60168,#60169,#60170,#60171),.UNSPECIFIED.,.F.,.F.,(4,1,1,1,1,1,
1,4),(15.7079632679489,16.3718455200134,17.3582961466295,18.3447467732457,
19.3311973998618,20.317648026478,21.3040986530941,21.9911485751285),
 .UNSPECIFIED.);
#1515=B_SPLINE_CURVE_WITH_KNOTS('',3,(#60404,#60405,#60406,#60407,#60408,
#60409,#60410,#60411,#60412,#60413,#60414,#60415,#60416,#60417,#60418,#60419,
#60420,#60421,#60422,#60423,#60424,#60425,#60426,#60427,#60428,#60429,#60430,
#60431,#60432,#60433,#60434,#60435,#60436,#60437,#60438,#60439,#60440,#60441,
#60442,#60443,#60444,#60445,#60446,#60447,#60448,#60449,#60450,#60451,#60452,
#60453,#60454,#60455,#60456,#60457,#60458,#60459,#60460,#60461,#60462,#60463,
#60464,#60465,#60466,#60467,#60468,#60469,#60470,#60471,#60472,#60473,#60474,
#60475,#60476,#60477,#60478,#60479,#60480,#60481,#60482,#60483,#60484,#60485,
#60486,#60487,#60488,#60489,#60490,#60491,#60492,#60493,#60494,#60495,#60496,
#60497,#60498,#60499,#60500,#60501,#60502,#60503,#60504,#60505,#60506,#60507,
#60508,#60509),.UNSPECIFIED.,.F.,.F.,(4,3,3,3,3,3,3,3,3,3,3,3,3,3,3,3,3,
3,3,3,3,3,3,3,3,3,3,3,3,3,3,3,3,3,3,4),(0.,0.0439873495596682,0.088535234885729,
0.133203648537345,0.177539443303643,0.193269018030229,0.199971189808446,
0.243934275067846,0.248071778815114,0.292055723719706,0.335717872507241,
0.374210944067843,0.384315712222397,0.391619070879034,0.434698852730331,
0.47712046629841,0.48969015874965,0.533088907914198,0.559308924386188,0.574291000021554,
0.57984588764462,0.62205897872085,0.66496509314549,0.707636118884185,0.738257750456918,
0.752576412624451,0.758605909671541,0.765028679465915,0.807111218921827,
0.843485707057882,0.85917048475052,0.866049641644265,0.873236607794053,
0.913787166992983,0.952609171466047,0.972375876542335),.UNSPECIFIED.);
#1516=B_SPLINE_CURVE_WITH_KNOTS('',3,(#60510,#60511,#60512,#60513,#60514,
#60515,#60516,#60517,#60518,#60519,#60520,#60521,#60522,#60523,#60524,#60525,
#60526,#60527,#60528,#60529,#60530,#60531,#60532,#60533,#60534,#60535,#60536,
#60537,#60538,#60539,#60540,#60541,#60542,#60543,#60544,#60545,#60546,#60547,
#60548,#60549,#60550,#60551,#60552,#60553,#60554,#60555,#60556,#60557,#60558,
#60559,#60560,#60561,#60562,#60563,#60564,#60565,#60566,#60567,#60568,#60569,
#60570,#60571,#60572,#60573,#60574,#60575,#60576,#60577,#60578,#60579,#60580,
#60581,#60582,#60583,#60584,#60585,#60586,#60587,#60588,#60589,#60590,#60591,
#60592,#60593,#60594,#60595,#60596,#60597,#60598,#60599,#60600,#60601,#60602,
#60603,#60604,#60605,#60606,#60607,#60608,#60609,#60610,#60611,#60612),
 .UNSPECIFIED.,.F.,.F.,(4,3,3,3,3,3,3,3,3,3,3,3,3,3,3,3,3,3,3,3,3,3,3,3,
3,3,3,3,3,3,3,3,3,3,4),(0.,0.0403422905180338,0.0813682734786595,0.122949980351713,
0.16449095941097,0.178014361827899,0.183409369411602,0.227186329885339,
0.269229509469957,0.311535350955759,0.348916065443153,0.357705618004978,
0.364415764229672,0.407315005273426,0.450191512111689,0.461058208905336,
0.503507289353387,0.531285871131442,0.541027225498738,0.546474827271459,
0.552442453195144,0.594916660917874,0.639047653028424,0.683117962531696,
0.716223791940519,0.731747366121405,0.738184546707727,0.782779716156374,
0.824075936567849,0.84301368069624,0.852796512264844,0.860145827789084,
0.904729831180339,0.947964597802275,0.97000658757344),.UNSPECIFIED.);
#1517=B_SPLINE_CURVE_WITH_KNOTS('',3,(#60613,#60614,#60615,#60616,#60617,
#60618,#60619,#60620,#60621,#60622,#60623,#60624,#60625,#60626,#60627,#60628,
#60629,#60630,#60631,#60632,#60633,#60634,#60635,#60636,#60637),
 .UNSPECIFIED.,.F.,.F.,(4,3,3,3,3,3,3,3,4),(-10.1321597128207,-9.86450626616149,
-8.87805563954534,-7.89160501292919,-6.90515438631305,-5.91870375969689,
-4.93225313308075,-3.94580250646459,-3.84897440564117),.UNSPECIFIED.);
#1518=B_SPLINE_CURVE_WITH_KNOTS('',3,(#60870,#60871,#60872,#60873,#60874,
#60875,#60876,#60877,#60878,#60879,#60880,#60881,#60882,#60883,#60884,#60885,
#60886,#60887,#60888,#60889,#60890,#60891,#60892,#60893,#60894,#60895,#60896,
#60897,#60898,#60899,#60900,#60901,#60902,#60903,#60904,#60905,#60906,#60907,
#60908,#60909,#60910,#60911,#60912,#60913,#60914,#60915,#60916,#60917,#60918,
#60919,#60920,#60921,#60922,#60923,#60924,#60925,#60926,#60927,#60928,#60929,
#60930,#60931,#60932,#60933,#60934,#60935,#60936,#60937,#60938,#60939,#60940,
#60941,#60942,#60943,#60944,#60945,#60946,#60947,#60948,#60949,#60950,#60951,
#60952,#60953,#60954,#60955,#60956,#60957,#60958,#60959,#60960,#60961,#60962,
#60963,#60964,#60965,#60966,#60967,#60968,#60969,#60970,#60971,#60972),
 .UNSPECIFIED.,.F.,.F.,(4,3,3,3,3,3,3,3,3,3,3,3,3,3,3,3,3,3,3,3,3,3,3,3,
3,3,3,3,3,3,3,3,3,3,4),(0.,0.0403420728543006,0.0813678367855401,0.122949539928715,
0.164490759249614,0.178014431809021,0.183409385478703,0.227186329885338,
0.269229949539637,0.311536068831159,0.348916603849705,0.357706091108837,
0.364415856383174,0.407315466341614,0.450192046682075,0.461058208905346,
0.5035070595844,0.531285655723017,0.541026743529684,0.54647402973548,0.552442268108838,
0.59491621056702,0.639047258971427,0.683117463220518,0.716223355043237,
0.731746708435023,0.738183753475272,0.782778798969233,0.824075248677492,
0.843013807341498,0.852796973522259,0.860145921094186,0.904729940902664,
0.947964597802271,0.970006587573432),.UNSPECIFIED.);
#1519=B_SPLINE_CURVE_WITH_KNOTS('',3,(#60973,#60974,#60975,#60976,#60977,
#60978,#60979,#60980,#60981,#60982,#60983,#60984,#60985,#60986,#60987,#60988,
#60989,#60990,#60991,#60992,#60993,#60994,#60995,#60996,#60997),
 .UNSPECIFIED.,.F.,.F.,(4,3,3,3,3,3,3,3,4),(7.59220430834742,7.89160501292919,
8.87805563954534,9.86450626616149,10.8509568927776,11.8374075193938,12.8238581460099,
13.8103087726261,13.875389615527),.UNSPECIFIED.);
#1520=B_SPLINE_CURVE_WITH_KNOTS('',3,(#60998,#60999,#61000,#61001,#61002,
#61003,#61004,#61005,#61006,#61007,#61008,#61009,#61010,#61011,#61012,#61013,
#61014,#61015,#61016,#61017,#61018,#61019,#61020,#61021,#61022,#61023,#61024,
#61025,#61026,#61027,#61028,#61029,#61030,#61031,#61032,#61033,#61034,#61035,
#61036,#61037,#61038,#61039,#61040,#61041,#61042,#61043,#61044,#61045,#61046,
#61047,#61048,#61049,#61050,#61051,#61052,#61053,#61054,#61055,#61056,#61057,
#61058,#61059,#61060,#61061,#61062,#61063,#61064,#61065,#61066,#61067,#61068,
#61069,#61070,#61071,#61072,#61073,#61074,#61075,#61076,#61077,#61078,#61079,
#61080,#61081,#61082,#61083,#61084,#61085,#61086,#61087,#61088,#61089,#61090,
#61091,#61092,#61093,#61094,#61095,#61096,#61097,#61098,#61099,#61100,#61101,
#61102,#61103),.UNSPECIFIED.,.F.,.F.,(4,3,3,3,3,3,3,3,3,3,3,3,3,3,3,3,3,
3,3,3,3,3,3,3,3,3,3,3,3,3,3,3,3,3,3,4),(0.,0.0439870213484189,0.0885347768590274,
0.133203573182163,0.177540067473735,0.193271868519026,0.199972102087808,
0.24393536506854,0.248071778815114,0.29205601261511,0.335718137618304,0.374211142901135,
0.3843154671772,0.391619008898289,0.434698890696845,0.477120259746675,0.489690158749629,
0.533088750991939,0.55930877727157,0.574290713387234,0.579845401630218,
0.622058272372198,0.664964305291723,0.707635330968564,0.738257061030748,
0.752575428668685,0.758604644157454,0.765028377494937,0.80711091192384,
0.843485476809388,0.85917031769407,0.86604942682694,0.87323655891021,0.913787164180478,
0.95260917146603,0.972375876542318),.UNSPECIFIED.);
#1521=B_SPLINE_CURVE_WITH_KNOTS('',3,(#61164,#61165,#61166,#61167,#61168,
#61169,#61170,#61171,#61172,#61173),.UNSPECIFIED.,.F.,.F.,(4,3,3,4),(-4.09293042013066,
-3.96748245563351,-2.97561184172513,-2.06863817490915),.UNSPECIFIED.);
#1522=B_SPLINE_CURVE_WITH_KNOTS('',3,(#61176,#61177,#61178,#61179,#61180,
#61181,#61182),.UNSPECIFIED.,.F.,.F.,(4,3,4),(0.,0.992711177740983,1.1173004083682),
 .UNSPECIFIED.);
#1523=B_SPLINE_CURVE_WITH_KNOTS('',3,(#61187,#61188,#61189,#61190,#61191,
#61192,#61193,#61194,#61195,#61196,#61197,#61198,#61199,#61200,#61201,#61202,
#61203,#61204,#61205,#61206,#61207,#61208),.UNSPECIFIED.,.F.,.F.,(4,3,3,
3,3,3,3,4),(-10.3761157273102,-9.91870613908378,-8.9268355251754,-7.93496491126702,
-6.94309429735864,-5.95122368345026,-4.95935306954189,-4.09293042013066),
 .UNSPECIFIED.);
#1524=B_SPLINE_CURVE_WITH_KNOTS('',3,(#61209,#61210,#61211,#61212,#61213,
#61214,#61215,#61216,#61217,#61218,#61219,#61220,#61221,#61222,#61223,#61224,
#61225,#61226,#61227,#61228,#61229,#61230),.UNSPECIFIED.,.F.,.F.,(4,3,3,
3,3,3,3,4),(1.1173004083682,1.98542235548196,2.97813353322293,3.97084471096391,
4.96355588870488,5.95626706644586,6.94897824418683,7.40048571554779),
 .UNSPECIFIED.);
#1525=B_SPLINE_CURVE_WITH_KNOTS('',3,(#61235,#61236,#61237,#61238,#61239,
#61240,#61241,#61242,#61243,#61244,#61245,#61246,#61247,#61248,#61249,#61250,
#61251,#61252,#61253,#61254,#61255,#61256),.UNSPECIFIED.,.F.,.F.,(4,3,3,
3,3,3,3,4),(-16.6593010344898,-15.869929822534,-14.8780592086257,-13.8861885947173,
-12.8943179808089,-11.9024473669005,-10.9105767529922,-10.3761157273102),
 .UNSPECIFIED.);
#1526=B_SPLINE_CURVE_WITH_KNOTS('',3,(#61257,#61258,#61259,#61260,#61261,
#61262,#61263,#61264,#61265,#61266,#61267,#61268,#61269,#61270,#61271,#61272,
#61273,#61274,#61275,#61276,#61277,#61278),.UNSPECIFIED.,.F.,.F.,(4,3,3,
3,3,3,3,4),(7.40048571554779,7.94168942192781,8.93440059966879,9.92711177740977,
10.9198229551507,11.9125341328917,12.9052453106327,13.6836710227274),
 .UNSPECIFIED.);
#1527=B_SPLINE_CURVE_WITH_KNOTS('',3,(#61283,#61284,#61285,#61286,#61287,
#61288,#61289,#61290,#61291,#61292,#61293,#61294,#61295,#61296,#61297,#61298,
#61299,#61300,#61301,#61302,#61303,#61304,#61305,#61306,#61307),
 .UNSPECIFIED.,.F.,.F.,(4,3,3,3,3,3,3,3,4),(-22.9424863416694,-22.8130241198927,
-21.8211535059843,-20.8292828920759,-19.8374122781676,-18.8455416642592,
-17.8536710503508,-16.8618004364424,-16.6593010344898),.UNSPECIFIED.);
#1528=B_SPLINE_CURVE_WITH_KNOTS('',3,(#61308,#61309,#61310,#61311,#61312,
#61313,#61314,#61315,#61316,#61317,#61318,#61319,#61320,#61321,#61322,#61323,
#61324,#61325,#61326,#61327,#61328,#61329,#61330,#61331,#61332),
 .UNSPECIFIED.,.F.,.F.,(4,3,3,3,3,3,3,3,4),(13.6836710227274,13.8979564883737,
14.8906676661147,15.8833788438556,16.8760900215966,17.8688011993376,18.8615123770786,
19.8542235548195,19.966856329907),.UNSPECIFIED.);
#1529=B_SPLINE_CURVE_WITH_KNOTS('',3,(#61337,#61338,#61339,#61340,#61341,
#61342,#61343,#61344,#61345,#61346,#61347,#61348,#61349,#61350,#61351,#61352,
#61353,#61354,#61355,#61356,#61357,#61358),.UNSPECIFIED.,.F.,.F.,(4,3,3,
3,3,3,3,4),(-29.225671648849,-28.764247803343,-27.7723771894346,-26.7805065755262,
-25.7886359616178,-24.7967653477094,-23.8048947338011,-22.9424863416694),
 .UNSPECIFIED.);
#1530=B_SPLINE_CURVE_WITH_KNOTS('',3,(#61359,#61360,#61361,#61362,#61363,
#61364,#61365,#61366,#61367,#61368,#61369,#61370,#61371,#61372,#61373,#61374,
#61375,#61376,#61377,#61378,#61379,#61380),.UNSPECIFIED.,.F.,.F.,(4,3,3,
3,3,3,3,4),(19.966856329907,20.8469347325605,21.8396459103015,22.8323570880425,
23.8250682657834,24.8177794435244,25.8104906212654,26.2500416370865),
 .UNSPECIFIED.);
#1531=B_SPLINE_CURVE_WITH_KNOTS('',3,(#61385,#61386,#61387,#61388,#61389,
#61390,#61391,#61392,#61393,#61394,#61395,#61396,#61397,#61398,#61399,#61400,
#61401,#61402,#61403,#61404,#61405,#61406),.UNSPECIFIED.,.F.,.F.,(4,3,3,
3,3,3,3,4),(-35.5088569560286,-34.7154714867932,-33.7236008728848,-32.7317302589765,
-31.7398596450681,-30.7479890311597,-29.7561184172513,-29.225671648849),
 .UNSPECIFIED.);
#1532=B_SPLINE_CURVE_WITH_KNOTS('',3,(#61407,#61408,#61409,#61410,#61411,
#61412,#61413,#61414,#61415,#61416,#61417,#61418,#61419,#61420,#61421,#61422,
#61423,#61424,#61425,#61426,#61427,#61428),.UNSPECIFIED.,.F.,.F.,(4,3,3,
3,3,3,3,4),(26.2500416370865,26.8032017990064,27.7959129767474,28.7886241544883,
29.7813353322293,30.7740465099703,31.7667576877113,32.5332269442661),
 .UNSPECIFIED.);
#1533=B_SPLINE_CURVE_WITH_KNOTS('',3,(#61433,#61434,#61435,#61436,#61437,
#61438,#61439,#61440,#61441,#61442,#61443,#61444,#61445,#61446,#61447,#61448,
#61449,#61450,#61451,#61452,#61453,#61454,#61455,#61456,#61457),
 .UNSPECIFIED.,.F.,.F.,(4,3,3,3,3,3,3,3,4),(-41.7920422632082,-41.6585657841519,
-40.6666951702435,-39.6748245563351,-38.6829539424267,-37.6910833285184,
-36.69921271461,-35.7073421007016,-35.5088569560286),.UNSPECIFIED.);
#1534=B_SPLINE_CURVE_WITH_KNOTS('',3,(#61458,#61459,#61460,#61461,#61462,
#61463,#61464,#61465,#61466,#61467,#61468,#61469,#61470,#61471,#61472,#61473,
#61474,#61475,#61476,#61477,#61478,#61479,#61480,#61481,#61482),
 .UNSPECIFIED.,.F.,.F.,(4,3,3,3,3,3,3,3,4),(32.5332269442661,32.7594688654522,
33.7521800431932,34.7448912209342,35.7376023986752,36.7303135764161,37.7230247541571,
38.7157359318981,38.8164122514457),.UNSPECIFIED.);
#1535=B_SPLINE_CURVE_WITH_KNOTS('',3,(#61487,#61488,#61489,#61490,#61491,
#61492,#61493,#61494,#61495,#61496,#61497,#61498,#61499,#61500,#61501,#61502,
#61503,#61504,#61505,#61506,#61507,#61508),.UNSPECIFIED.,.F.,.F.,(4,3,3,
3,3,3,3,4),(-48.0752275703878,-47.6097894676021,-46.6179188536938,-45.6260482397854,
-44.634177625877,-43.6423070119686,-42.6504363980602,-41.7920422632082),
 .UNSPECIFIED.);
#1536=B_SPLINE_CURVE_WITH_KNOTS('',3,(#61509,#61510,#61511,#61512,#61513,
#61514,#61515,#61516,#61517,#61518,#61519,#61520,#61521,#61522,#61523,#61524,
#61525,#61526,#61527,#61528,#61529,#61530),.UNSPECIFIED.,.F.,.F.,(4,3,3,
3,3,3,3,4),(38.8164122514457,39.7084471096391,40.7011582873801,41.693869465121,
42.686580642862,43.679291820603,44.672002998344,45.0995975586253),
 .UNSPECIFIED.);
#1537=B_SPLINE_CURVE_WITH_KNOTS('',3,(#61535,#61536,#61537,#61538,#61539,
#61540,#61541,#61542,#61543,#61544,#61545,#61546,#61547,#61548,#61549,#61550,
#61551,#61552,#61553,#61554,#61555,#61556),.UNSPECIFIED.,.F.,.F.,(4,3,3,
3,3,3,3,4),(-54.3584128775674,-53.5610131510524,-52.569142537144,-51.5772719232356,
-50.5854013093273,-49.5935306954189,-48.6016600815105,-48.0752275703878),
 .UNSPECIFIED.);
#1538=B_SPLINE_CURVE_WITH_KNOTS('',3,(#61557,#61558,#61559,#61560,#61561,
#61562,#61563,#61564,#61565,#61566,#61567,#61568,#61569,#61570,#61571,#61572,
#61573,#61574,#61575,#61576,#61577,#61578),.UNSPECIFIED.,.F.,.F.,(4,3,3,
3,3,3,3,4),(45.0995975586253,45.6647141760849,46.6574253538259,47.6501365315669,
48.6428477093079,49.6355588870488,50.6282700647898,51.3827828658049),
 .UNSPECIFIED.);
#1539=B_SPLINE_CURVE_WITH_KNOTS('',3,(#61583,#61584,#61585,#61586,#61587,
#61588,#61589,#61590,#61591,#61592,#61593,#61594,#61595,#61596,#61597,#61598,
#61599,#61600,#61601,#61602,#61603,#61604,#61605,#61606,#61607),
 .UNSPECIFIED.,.F.,.F.,(4,3,3,3,3,3,3,3,4),(-60.641598184747,-60.5041074484111,
-59.5122368345027,-58.5203662205943,-57.5284956066859,-56.5366249927775,
-55.5447543788692,-54.5528837649608,-54.3584128775674),.UNSPECIFIED.);
#1540=B_SPLINE_CURVE_WITH_KNOTS('',3,(#61608,#61609,#61610,#61611,#61612,
#61613,#61614,#61615,#61616,#61617,#61618,#61619,#61620,#61621,#61622,#61623,
#61624,#61625,#61626,#61627,#61628,#61629,#61630,#61631,#61632),
 .UNSPECIFIED.,.F.,.F.,(4,3,3,3,3,3,3,3,4),(51.3827828658049,51.6209812425308,
52.6136924202718,53.6064035980127,54.5991147757537,55.5918259534947,56.5845371312357,
57.5772483089767,57.6659681729845),.UNSPECIFIED.);
#1541=B_SPLINE_CURVE_WITH_KNOTS('',3,(#61637,#61638,#61639,#61640,#61641,
#61642,#61643,#61644,#61645,#61646,#61647,#61648,#61649,#61650,#61651,#61652,
#61653,#61654,#61655,#61656,#61657,#61658),.UNSPECIFIED.,.F.,.F.,(4,3,3,
3,3,3,3,4),(-66.9247834919266,-66.4553311318613,-65.4634605179529,-64.4715899040445,
-63.4797192901362,-62.4878486762278,-61.4959780623194,-60.641598184747),
 .UNSPECIFIED.);
#1542=B_SPLINE_CURVE_WITH_KNOTS('',3,(#61659,#61660,#61661,#61662,#61663,
#61664,#61665,#61666,#61667,#61668,#61669,#61670,#61671,#61672,#61673,#61674,
#61675,#61676,#61677,#61678,#61679,#61680),.UNSPECIFIED.,.F.,.F.,(4,3,3,
3,3,3,3,4),(57.6659681729845,58.5699594867177,59.5626706644586,60.5553818421996,
61.5480930199406,62.5408041976816,63.5335153754225,63.9491534801641),
 .UNSPECIFIED.);
#1543=B_SPLINE_CURVE_WITH_KNOTS('',3,(#61685,#61686,#61687,#61688,#61689,
#61690,#61691,#61692,#61693,#61694,#61695,#61696,#61697,#61698,#61699,#61700,
#61701,#61702,#61703,#61704,#61705,#61706),.UNSPECIFIED.,.F.,.F.,(4,3,3,
3,3,3,3,4),(-73.2079687991062,-72.4065548153116,-71.4146842014032,-70.4228135874948,
-69.4309429735864,-68.4390723596781,-67.4472017457697,-66.9247834919266),
 .UNSPECIFIED.);
#1544=B_SPLINE_CURVE_WITH_KNOTS('',3,(#61707,#61708,#61709,#61710,#61711,
#61712,#61713,#61714,#61715,#61716,#61717,#61718,#61719,#61720,#61721,#61722,
#61723,#61724,#61725,#61726,#61727,#61728),.UNSPECIFIED.,.F.,.F.,(4,3,3,
3,3,3,3,4),(63.9491534801641,64.5262265531635,65.5189377309045,66.5116489086455,
67.5043600863864,68.4970712641274,69.4897824418684,70.2323387873437),
 .UNSPECIFIED.);
#1545=B_SPLINE_CURVE_WITH_KNOTS('',3,(#61733,#61734,#61735,#61736,#61737,
#61738,#61739,#61740,#61741,#61742,#61743,#61744,#61745,#61746,#61747,#61748,
#61749,#61750,#61751,#61752,#61753,#61754,#61755,#61756,#61757),
 .UNSPECIFIED.,.F.,.F.,(4,3,3,3,3,3,3,3,4),(-79.4911541062857,-79.3496491126702,
-78.3577784987618,-77.3659078848535,-76.3740372709451,-75.3821666570367,
-74.3902960431283,-73.3984254292199,-73.2079687991062),.UNSPECIFIED.);
#1546=B_SPLINE_CURVE_WITH_KNOTS('',3,(#61758,#61759,#61760,#61761,#61762,
#61763,#61764,#61765,#61766,#61767,#61768,#61769,#61770,#61771,#61772,#61773,
#61774,#61775,#61776,#61777,#61778,#61779,#61780,#61781,#61782),
 .UNSPECIFIED.,.F.,.F.,(4,3,3,3,3,3,3,3,4),(70.2323387873437,70.4824936196094,
71.4752047973503,72.4679159750913,73.4606271528323,74.4533383305733,75.4460495083142,
76.4387606860552,76.5155240945233),.UNSPECIFIED.);
#1547=B_SPLINE_CURVE_WITH_KNOTS('',3,(#61787,#61788,#61789,#61790,#61791,
#61792,#61793,#61794,#61795,#61796,#61797,#61798,#61799,#61800,#61801,#61802,
#61803,#61804,#61805,#61806,#61807,#61808),.UNSPECIFIED.,.F.,.F.,(4,3,3,
3,3,3,3,4),(-85.7743394134653,-85.3008727961205,-84.3090021822121,-83.3171315683037,
-82.3252609543953,-81.333390340487,-80.3415197265786,-79.4911541062857),
 .UNSPECIFIED.);
#1548=B_SPLINE_CURVE_WITH_KNOTS('',3,(#61809,#61810,#61811,#61812,#61813,
#61814,#61815,#61816,#61817,#61818,#61819,#61820,#61821,#61822,#61823,#61824,
#61825,#61826,#61827,#61828,#61829,#61830),.UNSPECIFIED.,.F.,.F.,(4,3,3,
3,3,3,3,4),(76.5155240945233,77.4314718637962,78.4241830415372,79.4168942192782,
80.4096053970191,81.4023165747601,82.3950277525011,82.7987094017029),
 .UNSPECIFIED.);
#1549=B_SPLINE_CURVE_WITH_KNOTS('',3,(#61835,#61836,#61837,#61838,#61839,
#61840,#61841,#61842,#61843,#61844,#61845,#61846,#61847,#61848,#61849,#61850,
#61851,#61852,#61853,#61854,#61855,#61856),.UNSPECIFIED.,.F.,.F.,(4,3,3,
3,3,3,3,4),(-92.0575247206449,-91.2520964795708,-90.2602258656624,-89.268355251754,
-88.2764846378456,-87.2846140239373,-86.2927434100289,-85.7743394134653),
 .UNSPECIFIED.);
#1550=B_SPLINE_CURVE_WITH_KNOTS('',3,(#61857,#61858,#61859,#61860,#61861,
#61862,#61863,#61864,#61865,#61866,#61867,#61868,#61869,#61870,#61871,#61872,
#61873,#61874,#61875,#61876,#61877,#61878),.UNSPECIFIED.,.F.,.F.,(4,3,3,
3,3,3,3,4),(82.7987094017029,83.3877389302421,84.380450107983,85.373161285724,
86.365872463465,87.358583641206,88.351294818947,89.0818947088825),
 .UNSPECIFIED.);
#1551=B_SPLINE_CURVE_WITH_KNOTS('',3,(#61884,#61885,#61886,#61887,#61888,
#61889,#61890,#61891,#61892,#61893),.UNSPECIFIED.,.F.,.F.,(4,1,1,1,1,1,
1,4),(103.672557568463,103.858999941297,104.850870555206,105.842741169114,
106.834611783022,107.826482396931,108.818353010839,109.810223624748),
 .UNSPECIFIED.);
#1552=B_SPLINE_CURVE_WITH_KNOTS('',3,(#61896,#61897,#61898,#61899,#61900,
#61901,#61902,#61903),.UNSPECIFIED.,.F.,.F.,(4,1,1,1,1,4),(103.672557568463,
104.600461793276,105.593172971017,106.585884148758,107.578595326499,108.57130650424),
 .UNSPECIFIED.);
#1553=B_SPLINE_CURVE_WITH_KNOTS('',3,(#61908,#61909,#61910,#61911,#61912,
#61913,#61914,#61915,#61916,#61917),.UNSPECIFIED.,.F.,.F.,(4,1,1,1,1,1,
1,4),(97.3893722612836,97.9077762578471,98.8996468717555,99.8915174856638,
100.883388099572,101.875258713481,102.867129327389,103.672557568463),
 .UNSPECIFIED.);
#1554=B_SPLINE_CURVE_WITH_KNOTS('',3,(#61918,#61919,#61920,#61921,#61922,
#61923,#61924,#61925,#61926,#61927,#61928),.UNSPECIFIED.,.F.,.F.,(4,1,1,
1,1,1,1,1,4),(97.3893722612836,97.6514835490889,98.6441947268299,99.6369059045709,
100.629617082312,101.622328260053,102.615039437794,103.607750615535,103.672557568463),
 .UNSPECIFIED.);
#1555=B_SPLINE_CURVE_WITH_KNOTS('',3,(#61933,#61934,#61935,#61936,#61937,
#61938,#61939,#61940,#61941,#61942),.UNSPECIFIED.,.F.,.F.,(4,1,1,1,1,1,
1,4),(91.106186954104,91.9565525743968,92.9484231883052,93.9402938022136,
94.9321644161219,95.9240350300303,96.9159056439387,97.3893722612836),
 .UNSPECIFIED.);
#1556=B_SPLINE_CURVE_WITH_KNOTS('',3,(#61943,#61944,#61945,#61946,#61947,
#61948,#61949,#61950,#61951,#61952),.UNSPECIFIED.,.F.,.F.,(4,1,1,1,1,1,
1,4),(91.106186954104,91.6952164826431,92.687927660384,93.680638838125,
94.673350015866,95.666061193607,96.658772371348,97.3893722612836),
 .UNSPECIFIED.);
#1557=B_SPLINE_CURVE_WITH_KNOTS('',3,(#61957,#61958,#61959,#61960,#61961,
#61962,#61963,#61964,#61965,#61966,#61967),.UNSPECIFIED.,.F.,.F.,(4,1,1,
1,1,1,1,1,4),(84.8230016469244,85.0134582770382,86.0053288909465,86.9971995048549,
87.9890701187633,88.9809407326717,89.9728113465801,90.9646819604884,91.106186954104),
 .UNSPECIFIED.);
#1558=B_SPLINE_CURVE_WITH_KNOTS('',3,(#61968,#61969,#61970,#61971,#61972,
#61973,#61974,#61975,#61976,#61977),.UNSPECIFIED.,.F.,.F.,(4,1,1,1,1,1,
1,4),(84.8230016469244,85.7389494161972,86.7316605939382,87.7243717716792,
88.7170829494201,89.7097941271611,90.7025053049021,91.106186954104),
 .UNSPECIFIED.);
#1559=B_SPLINE_CURVE_WITH_KNOTS('',3,(#61982,#61983,#61984,#61985,#61986,
#61987,#61988,#61989,#61990,#61991),.UNSPECIFIED.,.F.,.F.,(4,1,1,1,1,1,
1,4),(78.5398163397448,79.0622345935879,80.0541052074963,81.0459758214047,
82.037846435313,83.0297170492214,84.0215876631298,84.8230016469244),
 .UNSPECIFIED.);
#1560=B_SPLINE_CURVE_WITH_KNOTS('',3,(#61992,#61993,#61994,#61995,#61996,
#61997,#61998,#61999,#62000,#62001,#62002),.UNSPECIFIED.,.F.,.F.,(4,1,1,
1,1,1,1,1,4),(78.5398163397448,78.7899711720104,79.7826823497514,80.7753935274923,
81.7681047052333,82.7608158829743,83.7535270607153,84.7462382384562,84.8230016469244),
 .UNSPECIFIED.);
#1561=B_SPLINE_CURVE_WITH_KNOTS('',3,(#62007,#62008,#62009,#62010,#62011,
#62012,#62013,#62014,#62015,#62016),.UNSPECIFIED.,.F.,.F.,(4,1,1,1,1,1,
1,4),(72.2566310325652,73.1110109101376,74.102881524046,75.0947521379544,
76.0866227518628,77.0784933657711,78.0703639796795,78.5398163397448),
 .UNSPECIFIED.);
#1562=B_SPLINE_CURVE_WITH_KNOTS('',3,(#62017,#62018,#62019,#62020,#62021,
#62022,#62023,#62024,#62025,#62026),.UNSPECIFIED.,.F.,.F.,(4,1,1,1,1,1,
1,4),(72.2566310325652,72.8337041055645,73.8264152833055,74.8191264610465,
75.8118376387874,76.8045488165284,77.7972599942694,78.5398163397448),
 .UNSPECIFIED.);
#1563=B_SPLINE_CURVE_WITH_KNOTS('',3,(#62031,#62032,#62033,#62034,#62035,
#62036,#62037,#62038,#62039,#62040,#62041),.UNSPECIFIED.,.F.,.F.,(4,1,1,
1,1,1,1,1,4),(65.9734457253856,66.167916612779,67.1597872266874,68.1516578405957,
69.1435284545041,70.1353990684125,71.1272696823209,72.1191402962293,72.2566310325652),
 .UNSPECIFIED.);
#1564=B_SPLINE_CURVE_WITH_KNOTS('',3,(#62042,#62043,#62044,#62045,#62046,
#62047,#62048,#62049,#62050,#62051),.UNSPECIFIED.,.F.,.F.,(4,1,1,1,1,1,
1,4),(65.9734457253856,66.8774370391187,67.8701482168596,68.8628593946006,
69.8555705723416,70.8482817500825,71.8409929278235,72.2566310325652),
 .UNSPECIFIED.);
#1565=B_SPLINE_CURVE_WITH_KNOTS('',3,(#62056,#62057,#62058,#62059,#62060,
#62061,#62062,#62063,#62064,#62065),.UNSPECIFIED.,.F.,.F.,(4,1,1,1,1,1,
1,4),(59.6902604182061,60.2166929293287,61.2085635432371,62.2004341571455,
63.1923047710539,64.1841753849622,65.1760459988706,65.9734457253856),
 .UNSPECIFIED.);
#1566=B_SPLINE_CURVE_WITH_KNOTS('',3,(#62066,#62067,#62068,#62069,#62070,
#62071,#62072,#62073,#62074,#62075,#62076),.UNSPECIFIED.,.F.,.F.,(4,1,1,
1,1,1,1,1,4),(59.690260418206,59.9284587949318,60.9211699726728,61.9138811504138,
62.9065923281547,63.8993035058957,64.8920146836367,65.8847258613777,65.9734457253856),
 .UNSPECIFIED.);
#1567=B_SPLINE_CURVE_WITH_KNOTS('',3,(#62081,#62082,#62083,#62084,#62085,
#62086,#62087,#62088,#62089,#62090),.UNSPECIFIED.,.F.,.F.,(4,1,1,1,1,1,
1,4),(53.4070751110265,54.2654692458785,55.2573398597868,56.2492104736952,
57.2410810876036,58.232951701512,59.2248223154203,59.6902604182061),
 .UNSPECIFIED.);
#1568=B_SPLINE_CURVE_WITH_KNOTS('',3,(#62091,#62092,#62093,#62094,#62095,
#62096,#62097,#62098,#62099,#62100),.UNSPECIFIED.,.F.,.F.,(4,1,1,1,1,1,
1,4),(53.4070751110264,53.972191728486,54.9649029062269,55.9576140839679,
56.9503252617089,57.9430364394499,58.9357476171908,59.690260418206),
 .UNSPECIFIED.);
#1569=B_SPLINE_CURVE_WITH_KNOTS('',3,(#62105,#62106,#62107,#62108,#62109,
#62110,#62111,#62112,#62113,#62114,#62115),.UNSPECIFIED.,.F.,.F.,(4,1,1,
1,1,1,1,1,4),(47.1238898038469,47.3223749485198,48.3142455624282,49.3061161763366,
50.2979867902449,51.2898574041533,52.2817280180617,53.2735986319701,53.4070751110265),
 .UNSPECIFIED.);
#1570=B_SPLINE_CURVE_WITH_KNOTS('',3,(#62116,#62117,#62118,#62119,#62120,
#62121,#62122,#62123,#62124,#62125),.UNSPECIFIED.,.F.,.F.,(4,1,1,1,1,1,
1,4),(47.1238898038468,48.0159246620401,49.0086358397811,50.001347017522,
50.994058195263,51.986769373004,52.979480550745,53.4070751110264),
 .UNSPECIFIED.);
#1571=B_SPLINE_CURVE_WITH_KNOTS('',3,(#62130,#62131,#62132,#62133,#62134,
#62135,#62136,#62137,#62138,#62139),.UNSPECIFIED.,.F.,.F.,(4,1,1,1,1,1,
1,4),(40.8407044966673,41.3711512650695,42.3630218789779,43.3548924928863,
44.3467631067947,45.3386337207031,46.3305043346114,47.1238898038469),
 .UNSPECIFIED.);
#1572=B_SPLINE_CURVE_WITH_KNOTS('',3,(#62140,#62141,#62142,#62143,#62144,
#62145,#62146,#62147,#62148,#62149,#62150),.UNSPECIFIED.,.F.,.F.,(4,1,1,
1,1,1,1,1,4),(40.8407044966672,41.0669464178533,42.0596575955942,43.0523687733352,
44.0450799510762,45.0377911288172,46.0305023065581,47.0232134842991,47.1238898038468),
 .UNSPECIFIED.);
#1573=B_SPLINE_CURVE_WITH_KNOTS('',3,(#62155,#62156,#62157,#62158,#62159,
#62160,#62161,#62162,#62163,#62164),.UNSPECIFIED.,.F.,.F.,(4,1,1,1,1,1,
1,4),(34.5575191894877,35.4199275816193,36.4117981955277,37.403668809436,
38.3955394233444,39.3874100372528,40.3792806511612,40.8407044966673),
 .UNSPECIFIED.);
#1574=B_SPLINE_CURVE_WITH_KNOTS('',3,(#62165,#62166,#62167,#62168,#62169,
#62170,#62171,#62172,#62173,#62174),.UNSPECIFIED.,.F.,.F.,(4,1,1,1,1,1,
1,4),(34.5575191894876,35.1106793514074,36.1033905291484,37.0961017068893,
38.0888128846303,39.0815240623713,40.0742352401123,40.8407044966672),
 .UNSPECIFIED.);
#1575=B_SPLINE_CURVE_WITH_KNOTS('',3,(#62179,#62180,#62181,#62182,#62183,
#62184,#62185,#62186,#62187,#62188,#62189),.UNSPECIFIED.,.F.,.F.,(4,1,1,
1,1,1,1,1,4),(28.2743338823081,28.4768332842606,29.468703898169,30.4605745120774,
31.4524451259858,32.4443157398941,33.4361863538025,34.4280569677109,34.5575191894877),
 .UNSPECIFIED.);
#1576=B_SPLINE_CURVE_WITH_KNOTS('',3,(#62190,#62191,#62192,#62193,#62194,
#62195,#62196,#62197,#62198,#62199),.UNSPECIFIED.,.F.,.F.,(4,1,1,1,1,1,
1,4),(28.2743338823081,29.1544122849615,30.1471234627025,31.1398346404435,
32.1325458181845,33.1252569959254,34.1179681736664,34.5575191894876),
 .UNSPECIFIED.);
#1577=B_SPLINE_CURVE_WITH_KNOTS('',3,(#62204,#62205,#62206,#62207,#62208,
#62209,#62210,#62211,#62212,#62213),.UNSPECIFIED.,.F.,.F.,(4,1,1,1,1,1,
1,4),(21.9911485751285,22.5256096008104,23.5174802147187,24.5093508286271,
25.5012214425355,26.4930920564439,27.4849626703523,28.2743338823081),
 .UNSPECIFIED.);
#1578=B_SPLINE_CURVE_WITH_KNOTS('',3,(#62214,#62215,#62216,#62217,#62218,
#62219,#62220,#62221,#62222,#62223,#62224),.UNSPECIFIED.,.F.,.F.,(4,1,1,
1,1,1,1,1,4),(21.9911485751285,22.2054340407747,23.1981452185157,24.1908563962566,
25.1835675739976,26.1762787517386,27.1689899294796,28.1617011072206,28.2743338823081),
 .UNSPECIFIED.);
#1579=B_SPLINE_CURVE_WITH_KNOTS('',3,(#62229,#62230,#62231,#62232,#62233,
#62234,#62235,#62236,#62237,#62238),.UNSPECIFIED.,.F.,.F.,(4,1,1,1,1,1,
1,4),(15.7079632679489,16.5743859173601,17.5662565312685,18.5581271451769,
19.5499977590852,20.5418683729936,21.533738986902,21.9911485751285),
 .UNSPECIFIED.);
#1580=B_SPLINE_CURVE_WITH_KNOTS('',3,(#62239,#62240,#62241,#62242,#62243,
#62244,#62245,#62246,#62247,#62248),.UNSPECIFIED.,.F.,.F.,(4,1,1,1,1,1,
1,4),(15.7079632679489,16.2491669743288,17.2418781520698,18.2345893298108,
19.2273005075518,20.2200116852927,21.2127228630337,21.9911485751285),
 .UNSPECIFIED.);
#1581=B_SPLINE_CURVE_WITH_KNOTS('',3,(#62251,#62252,#62253,#62254,#62255,
#62256,#62257,#62258,#62259,#62260,#62261,#62262,#62263,#62264,#62265,#62266,
#62267,#62268,#62269,#62270,#62271,#62272,#62273,#62274,#62275,#62276,#62277,
#62278,#62279,#62280,#62281,#62282,#62283,#62284,#62285,#62286,#62287,#62288,
#62289,#62290,#62291,#62292,#62293,#62294,#62295,#62296,#62297,#62298,#62299,
#62300,#62301,#62302,#62303,#62304,#62305,#62306,#62307,#62308,#62309,#62310,
#62311,#62312,#62313,#62314,#62315,#62316,#62317,#62318,#62319,#62320,#62321,
#62322,#62323,#62324,#62325,#62326,#62327,#62328,#62329,#62330,#62331,#62332,
#62333,#62334,#62335,#62336,#62337,#62338,#62339,#62340,#62341,#62342,#62343,
#62344,#62345,#62346,#62347,#62348,#62349,#62350,#62351,#62352,#62353,#62354,
#62355,#62356,#62357,#62358,#62359,#62360,#62361,#62362,#62363,#62364,#62365,
#62366,#62367,#62368,#62369,#62370,#62371,#62372,#62373,#62374,#62375,#62376,
#62377,#62378,#62379,#62380,#62381,#62382,#62383,#62384,#62385,#62386,#62387,
#62388,#62389,#62390,#62391,#62392,#62393,#62394,#62395,#62396,#62397,#62398,
#62399,#62400,#62401,#62402,#62403,#62404,#62405,#62406,#62407,#62408,#62409,
#62410,#62411,#62412,#62413,#62414,#62415,#62416,#62417,#62418,#62419,#62420,
#62421,#62422,#62423,#62424,#62425,#62426,#62427,#62428,#62429,#62430,#62431,
#62432,#62433,#62434,#62435,#62436,#62437,#62438,#62439,#62440,#62441,#62442,
#62443,#62444,#62445,#62446,#62447,#62448,#62449,#62450,#62451,#62452,#62453,
#62454,#62455,#62456,#62457,#62458,#62459,#62460,#62461,#62462,#62463,#62464,
#62465,#62466,#62467,#62468,#62469,#62470),.UNSPECIFIED.,.F.,.F.,(4,3,3,
3,3,3,3,3,3,3,3,3,3,3,3,3,3,3,3,3,3,3,3,3,3,3,3,3,3,3,3,3,3,3,3,3,3,3,3,
3,3,3,3,3,3,3,3,3,3,3,3,3,3,3,3,3,3,3,3,3,3,3,3,3,3,3,3,3,3,3,3,3,3,4),
(-1.5115530493723,-1.48679433039677,-1.46137997144481,-1.44936627203976,
-1.44203978844916,-1.43723948275662,-1.41130482704604,-1.3851425648951,
-1.36907979899106,-1.36528335260342,-1.33883417182409,-1.31251413265359,
-1.29083745680875,-1.27999911888633,-1.27252822943752,-1.26916078096391,
-1.2438409010096,-1.21777622976252,-1.19264806966918,-1.18165449962834,
-1.17500808302858,-1.17140113753098,-1.14461626345551,-1.11752388424601,
-1.09233065043846,-1.08197947093734,-1.07663416157974,-1.07221334700158,
-1.04448214800868,-1.01675094901579,-0.989899829038698,-0.980534050538336,
-0.975142748268706,-0.971473262423844,-0.944367339171939,-0.916829945945447,
-0.889160172398661,-0.878253059899969,-0.87283587922991,-0.869128423226553,
-0.840502786522066,-0.812629809126308,-0.785184824902654,-0.776260550181423,
-0.769615191493828,-0.76539079696697,-0.754625876408607,-0.727617533495154,
-0.699889836956671,-0.672733437279935,-0.663027286995113,-0.658922109894078,
-0.630659562625353,-0.602060824740566,-0.57220527844112,-0.560770556686858,
-0.556383058918736,-0.552005977862112,-0.523133364911618,-0.494697204184849,
-0.482638639542781,-0.454174910522506,-0.448377858002803,-0.443883394073885,
-0.415482165359649,-0.386508614853008,-0.357316612716015,-0.340170191390177,
-0.335377465438287,-0.305918315871394,-0.27645436453335,-0.247645675491356,
-0.226999958751525,-0.219677966288016),.UNSPECIFIED.);
#1582=B_SPLINE_CURVE_WITH_KNOTS('',3,(#62472,#62473,#62474,#62475,#62476,
#62477,#62478,#62479,#62480,#62481,#62482,#62483,#62484,#62485,#62486,#62487,
#62488,#62489,#62490,#62491,#62492,#62493,#62494,#62495,#62496,#62497,#62498,
#62499,#62500,#62501,#62502,#62503,#62504,#62505,#62506,#62507,#62508,#62509,
#62510,#62511,#62512,#62513,#62514,#62515,#62516,#62517,#62518,#62519,#62520,
#62521,#62522,#62523,#62524,#62525,#62526,#62527,#62528,#62529,#62530,#62531,
#62532,#62533,#62534,#62535),.UNSPECIFIED.,.F.,.F.,(4,3,3,3,3,3,3,3,3,3,
3,3,3,3,3,3,3,3,3,3,3,4),(-0.410648750433038,-0.381296088292737,-0.350882391849445,
-0.328072119516976,-0.310964415267624,-0.305842993500878,-0.301661871504881,
-0.274116258800685,-0.259641302519569,-0.231392457082299,-0.202468399947011,
-0.198019208917011,-0.170841895434807,-0.143725312403613,-0.117042212888725,
-0.102411936277635,-0.097195049751494,-0.0935363835720784,-0.0677899334604712,
-0.0424347820407558,-0.0178142542830924,0.),.UNSPECIFIED.);
#1583=B_SPLINE_CURVE_WITH_KNOTS('',3,(#62538,#62539,#62540,#62541,#62542,
#62543,#62544,#62545,#62546,#62547,#62548,#62549,#62550,#62551,#62552,#62553,
#62554,#62555,#62556,#62557,#62558,#62559,#62560,#62561,#62562,#62563,#62564,
#62565,#62566,#62567,#62568),.UNSPECIFIED.,.F.,.F.,(4,3,3,3,3,3,3,3,3,3,
4),(-0.219677966288016,-0.201006229477425,-0.172158028090248,-0.142713390739092,
-0.124874216896705,-0.114789665948937,-0.110082687886506,-0.0803547102951982,
-0.0502957032480209,-0.0203907630638487,0.),.UNSPECIFIED.);
#1584=B_SPLINE_CURVE_WITH_KNOTS('',3,(#62981,#62982,#62983,#62984,#62985,
#62986,#62987,#62988),.UNSPECIFIED.,.F.,.F.,(4,1,1,1,1,4),(11.6150328478182,
12.6069034617266,13.598774075635,14.5906446895433,15.5825153034517,15.7079632679489),
 .UNSPECIFIED.);
#1585=B_SPLINE_CURVE_WITH_KNOTS('',3,(#62989,#62990,#62991,#62992,#62993,
#62994,#62995,#62996,#62997,#62998,#62999,#63000,#63001,#63002,#63003,#63004,
#63005,#63006,#63007,#63008,#63009,#63010,#63011,#63012,#63013,#63014,#63015,
#63016,#63017,#63018,#63019,#63020,#63021,#63022,#63023,#63024,#63025,#63026,
#63027,#63028,#63029,#63030,#63031,#63032,#63033,#63034,#63035,#63036,#63037,
#63038,#63039,#63040,#63041,#63042,#63043,#63044,#63045,#63046,#63047,#63048,
#63049,#63050,#63051,#63052,#63053,#63054,#63055,#63056,#63057,#63058,#63059,
#63060,#63061,#63062,#63063,#63064,#63065,#63066,#63067,#63068,#63069,#63070,
#63071,#63072,#63073,#63074,#63075,#63076),.UNSPECIFIED.,.F.,.F.,(4,3,3,
3,3,3,3,3,3,3,3,3,3,3,3,3,3,3,3,3,3,3,3,3,3,3,3,3,3,4),(-0.552745378375041,
-0.527830263536694,-0.498419933292456,-0.482944277728704,-0.477004703287069,
-0.471889411648522,-0.442842142020847,-0.418838054802294,-0.408336266644177,
-0.40199148464016,-0.397446251891128,-0.369139848009071,-0.341087780585202,
-0.313931322984348,-0.298150853306366,-0.293754274173184,-0.266922432864957,
-0.250809444272419,-0.223433348051691,-0.19550417954523,-0.19139998392206,
-0.164790719651446,-0.138164593558308,-0.11192170155777,-0.0979314888630491,
-0.0936568444848153,-0.0680692021908508,-0.0428602319276656,-0.0184469101431373,
0.),.UNSPECIFIED.);
#1586=B_SPLINE_CURVE_WITH_KNOTS('',3,(#63077,#63078,#63079,#63080,#63081,
#63082,#63083,#63084,#63085,#63086,#63087,#63088,#63089,#63090,#63091,#63092,
#63093,#63094,#63095),.UNSPECIFIED.,.F.,.F.,(4,3,3,3,3,3,4),(-96.6808425304193,
-96.2114495491126,-95.2195789352043,-94.2277083212959,-93.2358377073875,
-92.2439670934791,-92.0575247206449),.UNSPECIFIED.);
#1587=B_SPLINE_CURVE_WITH_KNOTS('',3,(#63098,#63099,#63100,#63101,#63102,
#63103,#63104,#63105,#63106),.UNSPECIFIED.,.F.,.F.,(4,1,1,1,1,1,4),(10.3761157273101,
11.2856110856239,12.2783222633649,13.2710334411059,14.2637446188469,15.2564557965878,
15.7079632679489),.UNSPECIFIED.);
#1588=B_SPLINE_CURVE_WITH_KNOTS('',3,(#63524,#63525,#63526,#63527,#63528,
#63529,#63530,#63531,#63532,#63533,#63534,#63535,#63536,#63537,#63538,#63539,
#63540,#63541,#63542,#63543,#63544,#63545),.UNSPECIFIED.,.F.,.F.,(4,3,3,
3,3,3,3,4),(89.0818947088825,89.3440059966879,90.3367171744289,91.3294283521699,
92.3221395299109,93.3148507076518,94.3075618853928,94.6122043555102),
 .UNSPECIFIED.);
#1589=B_SPLINE_CURVE_WITH_KNOTS('',3,(#63546,#63547,#63548,#63549,#63550,
#63551,#63552,#63553,#63554,#63555,#63556,#63557,#63558,#63559,#63560,#63561,
#63562,#63563,#63564,#63565,#63566,#63567,#63568,#63569,#63570,#63571,#63572,
#63573,#63574,#63575,#63576,#63577,#63578,#63579,#63580,#63581,#63582,#63583,
#63584,#63585,#63586,#63587,#63588,#63589,#63590,#63591,#63592,#63593,#63594,
#63595,#63596,#63597,#63598,#63599,#63600,#63601,#63602,#63603,#63604,#63605,
#63606,#63607,#63608,#63609,#63610,#63611,#63612,#63613,#63614,#63615,#63616,
#63617,#63618,#63619,#63620,#63621,#63622,#63623,#63624,#63625,#63626,#63627,
#63628,#63629,#63630,#63631,#63632,#63633),.UNSPECIFIED.,.F.,.F.,(4,3,3,
3,3,3,3,3,3,3,3,3,3,3,3,3,3,3,3,3,3,3,3,3,3,3,3,3,3,4),(-0.555272788399392,
-0.535208229286056,-0.51046000550438,-0.495927663091087,-0.490771565699598,
-0.464551573131573,-0.44160907963455,-0.431518091480653,-0.425427657470475,
-0.420791193383041,-0.394188077983384,-0.365893964776387,-0.344673379871139,
-0.328757941192203,-0.324434111993057,-0.296521822210165,-0.281011625155395,
-0.254049889550291,-0.226554106924644,-0.220947145848259,-0.216688100237889,
-0.188737539857684,-0.160250957640402,-0.131525362881473,-0.114279480489655,
-0.109581292141837,-0.0801117384511396,-0.0505679692714886,-0.0215915474943119,
0.),.UNSPECIFIED.);
#1590=CYLINDRICAL_SURFACE('',#14527,3.5175);
#1591=CYLINDRICAL_SURFACE('',#14529,3.5175);
#1592=CYLINDRICAL_SURFACE('',#14530,3.5175);
#1593=CYLINDRICAL_SURFACE('',#14531,3.5175);
#1594=CYLINDRICAL_SURFACE('',#14532,3.5175);
#1595=CYLINDRICAL_SURFACE('',#14533,3.5175);
#1596=CYLINDRICAL_SURFACE('',#14534,3.5175);
#1597=CYLINDRICAL_SURFACE('',#14535,3.5175);
#1598=CYLINDRICAL_SURFACE('',#14537,3.5175);
#1599=CYLINDRICAL_SURFACE('',#14539,3.5175);
#1600=CYLINDRICAL_SURFACE('',#14540,3.5175);
#1601=CYLINDRICAL_SURFACE('',#14541,3.5175);
#1602=CYLINDRICAL_SURFACE('',#14542,3.5175);
#1603=CYLINDRICAL_SURFACE('',#14543,3.5175);
#1604=CYLINDRICAL_SURFACE('',#14544,3.5175);
#1605=CYLINDRICAL_SURFACE('',#14545,3.5175);
#1606=CYLINDRICAL_SURFACE('',#14547,3.5175);
#1607=CYLINDRICAL_SURFACE('',#14549,3.5175);
#1608=CYLINDRICAL_SURFACE('',#14550,3.5175);
#1609=CYLINDRICAL_SURFACE('',#14551,3.5175);
#1610=CYLINDRICAL_SURFACE('',#14552,3.5175);
#1611=CYLINDRICAL_SURFACE('',#14553,3.5175);
#1612=CYLINDRICAL_SURFACE('',#14554,3.5175);
#1613=CYLINDRICAL_SURFACE('',#14555,3.5175);
#1614=CYLINDRICAL_SURFACE('',#14557,3.5175);
#1615=CYLINDRICAL_SURFACE('',#14559,3.5175);
#1616=CYLINDRICAL_SURFACE('',#14560,3.5175);
#1617=CYLINDRICAL_SURFACE('',#14561,3.5175);
#1618=CYLINDRICAL_SURFACE('',#14562,3.5175);
#1619=CYLINDRICAL_SURFACE('',#14563,3.5175);
#1620=CYLINDRICAL_SURFACE('',#14564,3.5175);
#1621=CYLINDRICAL_SURFACE('',#14565,3.5175);
#1622=CYLINDRICAL_SURFACE('',#14567,4.07350000000001);
#1623=CYLINDRICAL_SURFACE('',#14569,4.07350000000001);
#1624=CYLINDRICAL_SURFACE('',#14570,4.07350000000001);
#1625=CYLINDRICAL_SURFACE('',#14571,4.07350000000001);
#1626=CYLINDRICAL_SURFACE('',#14572,4.07350000000001);
#1627=CYLINDRICAL_SURFACE('',#14573,4.07350000000001);
#1628=CYLINDRICAL_SURFACE('',#14574,4.07350000000001);
#1629=CYLINDRICAL_SURFACE('',#14575,4.07350000000001);
#1630=CYLINDRICAL_SURFACE('',#14577,4.07350000000001);
#1631=CYLINDRICAL_SURFACE('',#14579,4.07350000000001);
#1632=CYLINDRICAL_SURFACE('',#14580,4.07350000000001);
#1633=CYLINDRICAL_SURFACE('',#14581,4.07350000000001);
#1634=CYLINDRICAL_SURFACE('',#14582,4.07350000000001);
#1635=CYLINDRICAL_SURFACE('',#14583,4.07350000000001);
#1636=CYLINDRICAL_SURFACE('',#14584,4.07350000000001);
#1637=CYLINDRICAL_SURFACE('',#14585,4.07350000000001);
#1638=CYLINDRICAL_SURFACE('',#14587,4.0735);
#1639=CYLINDRICAL_SURFACE('',#14589,4.0735);
#1640=CYLINDRICAL_SURFACE('',#14590,4.0735);
#1641=CYLINDRICAL_SURFACE('',#14591,4.0735);
#1642=CYLINDRICAL_SURFACE('',#14592,4.0735);
#1643=CYLINDRICAL_SURFACE('',#14593,4.0735);
#1644=CYLINDRICAL_SURFACE('',#14594,4.0735);
#1645=CYLINDRICAL_SURFACE('',#14595,4.0735);
#1646=CYLINDRICAL_SURFACE('',#14597,4.0735);
#1647=CYLINDRICAL_SURFACE('',#14599,4.0735);
#1648=CYLINDRICAL_SURFACE('',#14600,4.0735);
#1649=CYLINDRICAL_SURFACE('',#14601,4.0735);
#1650=CYLINDRICAL_SURFACE('',#14602,4.0735);
#1651=CYLINDRICAL_SURFACE('',#14603,4.0735);
#1652=CYLINDRICAL_SURFACE('',#14604,4.0735);
#1653=CYLINDRICAL_SURFACE('',#14605,4.0735);
#1654=CYLINDRICAL_SURFACE('',#14607,4.0735);
#1655=CYLINDRICAL_SURFACE('',#14609,4.0735);
#1656=CYLINDRICAL_SURFACE('',#14610,4.07350000000001);
#1657=CYLINDRICAL_SURFACE('',#14611,4.07350000000001);
#1658=CYLINDRICAL_SURFACE('',#14612,3.5175);
#1659=CYLINDRICAL_SURFACE('',#14613,3.5175);
#1660=CYLINDRICAL_SURFACE('',#14614,3.5175);
#1661=CYLINDRICAL_SURFACE('',#14615,3.5175);
#1662=CYLINDRICAL_SURFACE('',#14622,3.942);
#1663=CYLINDRICAL_SURFACE('',#14624,3.942);
#1664=CYLINDRICAL_SURFACE('',#14625,3.942);
#1665=CYLINDRICAL_SURFACE('',#14626,3.942);
#1666=CYLINDRICAL_SURFACE('',#14627,3.942);
#1667=CYLINDRICAL_SURFACE('',#14628,3.942);
#1668=CYLINDRICAL_SURFACE('',#14629,3.942);
#1669=CYLINDRICAL_SURFACE('',#14630,3.942);
#1670=CYLINDRICAL_SURFACE('',#14631,3.942);
#1671=CYLINDRICAL_SURFACE('',#14632,3.942);
#1672=CYLINDRICAL_SURFACE('',#14633,3.942);
#1673=CYLINDRICAL_SURFACE('',#14634,3.942);
#1674=CYLINDRICAL_SURFACE('',#14635,3.942);
#1675=CYLINDRICAL_SURFACE('',#14636,3.942);
#1676=CYLINDRICAL_SURFACE('',#14637,3.942);
#1677=CYLINDRICAL_SURFACE('',#14638,3.942);
#1678=CYLINDRICAL_SURFACE('',#14639,3.942);
#1679=CYLINDRICAL_SURFACE('',#14640,3.942);
#1680=CYLINDRICAL_SURFACE('',#14641,3.942);
#1681=CYLINDRICAL_SURFACE('',#14642,3.942);
#1682=CYLINDRICAL_SURFACE('',#14643,3.942);
#1683=CYLINDRICAL_SURFACE('',#14644,3.942);
#1684=CYLINDRICAL_SURFACE('',#14645,3.942);
#1685=CYLINDRICAL_SURFACE('',#14646,3.942);
#1686=CYLINDRICAL_SURFACE('',#14647,3.37175);
#1687=CYLINDRICAL_SURFACE('',#14649,3.37175);
#1688=CYLINDRICAL_SURFACE('',#14650,3.37175);
#1689=CYLINDRICAL_SURFACE('',#14651,3.37175);
#1690=CYLINDRICAL_SURFACE('',#14652,3.37175);
#1691=CYLINDRICAL_SURFACE('',#14653,3.37175);
#1692=CYLINDRICAL_SURFACE('',#14654,3.37175);
#1693=CYLINDRICAL_SURFACE('',#14655,3.37175);
#1694=CYLINDRICAL_SURFACE('',#14656,3.37175);
#1695=CYLINDRICAL_SURFACE('',#14657,3.37175);
#1696=CYLINDRICAL_SURFACE('',#14658,3.37175);
#1697=CYLINDRICAL_SURFACE('',#14659,3.37175);
#1698=CYLINDRICAL_SURFACE('',#14660,3.37175);
#1699=CYLINDRICAL_SURFACE('',#14661,3.37175);
#1700=CYLINDRICAL_SURFACE('',#14662,3.37175);
#1701=CYLINDRICAL_SURFACE('',#14663,3.37175);
#1702=CYLINDRICAL_SURFACE('',#14664,3.37175);
#1703=CYLINDRICAL_SURFACE('',#14665,3.37175);
#1704=CYLINDRICAL_SURFACE('',#14666,3.37175);
#1705=CYLINDRICAL_SURFACE('',#14667,3.37175);
#1706=CYLINDRICAL_SURFACE('',#14668,3.37175);
#1707=CYLINDRICAL_SURFACE('',#14669,3.37175);
#1708=CYLINDRICAL_SURFACE('',#14670,3.37175);
#1709=CYLINDRICAL_SURFACE('',#14671,3.37175);
#1710=CYLINDRICAL_SURFACE('',#14675,3.37175);
#1711=CYLINDRICAL_SURFACE('',#14677,3.942);
#1712=CYLINDRICAL_SURFACE('',#14687,6.5);
#1713=CYLINDRICAL_SURFACE('',#14692,4.5);
#1714=CYLINDRICAL_SURFACE('',#14695,9.);
#1715=CYLINDRICAL_SURFACE('',#14742,4.51775);
#1716=CYLINDRICAL_SURFACE('',#14746,4.51775);
#1717=CYLINDRICAL_SURFACE('',#14747,4.51775);
#1718=CYLINDRICAL_SURFACE('',#14748,4.51775);
#1719=CYLINDRICAL_SURFACE('',#14749,4.51775);
#1720=CYLINDRICAL_SURFACE('',#14750,4.51775);
#1721=CYLINDRICAL_SURFACE('',#14751,4.51775);
#1722=CYLINDRICAL_SURFACE('',#14752,4.51775);
#1723=CYLINDRICAL_SURFACE('',#14753,4.51775);
#1724=CYLINDRICAL_SURFACE('',#14754,4.51775);
#1725=CYLINDRICAL_SURFACE('',#14755,4.51775);
#1726=CYLINDRICAL_SURFACE('',#14756,4.51775);
#1727=CYLINDRICAL_SURFACE('',#14757,4.51775);
#1728=CYLINDRICAL_SURFACE('',#14758,4.51775);
#1729=CYLINDRICAL_SURFACE('',#14759,4.51775);
#1730=CYLINDRICAL_SURFACE('',#14760,4.51775);
#1731=CYLINDRICAL_SURFACE('',#14761,4.51775);
#1732=CYLINDRICAL_SURFACE('',#14762,4.51775);
#1733=CYLINDRICAL_SURFACE('',#14763,4.51775);
#1734=CYLINDRICAL_SURFACE('',#14764,4.51775);
#1735=CYLINDRICAL_SURFACE('',#14765,4.51775);
#1736=CYLINDRICAL_SURFACE('',#14766,4.51775);
#1737=CYLINDRICAL_SURFACE('',#14767,4.51775);
#1738=CYLINDRICAL_SURFACE('',#14768,4.51775);
#1739=CYLINDRICAL_SURFACE('',#14769,4.51775);
#1740=CYLINDRICAL_SURFACE('',#14771,5.0736);
#1741=CYLINDRICAL_SURFACE('',#14773,5.0736);
#1742=CYLINDRICAL_SURFACE('',#14774,5.0736);
#1743=CYLINDRICAL_SURFACE('',#14775,5.0736);
#1744=CYLINDRICAL_SURFACE('',#14776,5.0736);
#1745=CYLINDRICAL_SURFACE('',#14777,5.0736);
#1746=CYLINDRICAL_SURFACE('',#14778,5.0736);
#1747=CYLINDRICAL_SURFACE('',#14779,5.0736);
#1748=CYLINDRICAL_SURFACE('',#14780,5.0736);
#1749=CYLINDRICAL_SURFACE('',#14781,5.0736);
#1750=CYLINDRICAL_SURFACE('',#14782,5.0736);
#1751=CYLINDRICAL_SURFACE('',#14783,5.0736);
#1752=CYLINDRICAL_SURFACE('',#14784,5.0736);
#1753=CYLINDRICAL_SURFACE('',#14785,5.0736);
#1754=CYLINDRICAL_SURFACE('',#14786,5.0736);
#1755=CYLINDRICAL_SURFACE('',#14787,5.0736);
#1756=CYLINDRICAL_SURFACE('',#14788,5.0736);
#1757=CYLINDRICAL_SURFACE('',#14789,5.0736);
#1758=CYLINDRICAL_SURFACE('',#14790,5.0736);
#1759=CYLINDRICAL_SURFACE('',#14791,5.0736);
#1760=CYLINDRICAL_SURFACE('',#14792,5.0736);
#1761=CYLINDRICAL_SURFACE('',#14793,5.0736);
#1762=CYLINDRICAL_SURFACE('',#14794,5.0736);
#1763=CYLINDRICAL_SURFACE('',#14795,5.0736);
#1764=CYLINDRICAL_SURFACE('',#14796,5.0736);
#1765=CYLINDRICAL_SURFACE('',#14798,4.51775);
#1766=CYLINDRICAL_SURFACE('',#14802,4.51775);
#1767=CYLINDRICAL_SURFACE('',#14803,4.51775);
#1768=CYLINDRICAL_SURFACE('',#14804,4.51775);
#1769=CYLINDRICAL_SURFACE('',#14805,4.51775);
#1770=CYLINDRICAL_SURFACE('',#14806,4.51775);
#1771=CYLINDRICAL_SURFACE('',#14807,4.51775);
#1772=CYLINDRICAL_SURFACE('',#14808,4.51775);
#1773=CYLINDRICAL_SURFACE('',#14809,4.51775);
#1774=CYLINDRICAL_SURFACE('',#14810,4.51775);
#1775=CYLINDRICAL_SURFACE('',#14811,4.51775);
#1776=CYLINDRICAL_SURFACE('',#14812,4.51775);
#1777=CYLINDRICAL_SURFACE('',#14813,4.51775);
#1778=CYLINDRICAL_SURFACE('',#14814,4.51775);
#1779=CYLINDRICAL_SURFACE('',#14815,4.51775);
#1780=CYLINDRICAL_SURFACE('',#14816,4.51775);
#1781=CYLINDRICAL_SURFACE('',#14817,4.51775);
#1782=CYLINDRICAL_SURFACE('',#14818,4.51775);
#1783=CYLINDRICAL_SURFACE('',#14819,4.51775);
#1784=CYLINDRICAL_SURFACE('',#14820,4.51775);
#1785=CYLINDRICAL_SURFACE('',#14821,4.51775);
#1786=CYLINDRICAL_SURFACE('',#14822,4.51775);
#1787=CYLINDRICAL_SURFACE('',#14823,4.51775);
#1788=CYLINDRICAL_SURFACE('',#14824,4.51775);
#1789=CYLINDRICAL_SURFACE('',#14825,4.51775);
#1790=CYLINDRICAL_SURFACE('',#14826,4.51775);
#1791=CYLINDRICAL_SURFACE('',#14827,4.51775);
#1792=CYLINDRICAL_SURFACE('',#14828,4.51775);
#1793=CYLINDRICAL_SURFACE('',#14829,4.51775);
#1794=CYLINDRICAL_SURFACE('',#14830,4.51775);
#1795=CYLINDRICAL_SURFACE('',#14831,4.51775);
#1796=CYLINDRICAL_SURFACE('',#14832,4.51775);
#1797=CYLINDRICAL_SURFACE('',#14833,4.51775);
#1798=CYLINDRICAL_SURFACE('',#14834,4.51775);
#1799=CYLINDRICAL_SURFACE('',#14835,4.51775);
#1800=CYLINDRICAL_SURFACE('',#14836,4.51775);
#1801=CYLINDRICAL_SURFACE('',#14837,4.51775);
#1802=CYLINDRICAL_SURFACE('',#14838,4.51775);
#1803=CYLINDRICAL_SURFACE('',#14839,4.51775);
#1804=CYLINDRICAL_SURFACE('',#14840,4.51775);
#1805=CYLINDRICAL_SURFACE('',#14842,5.0736);
#1806=CYLINDRICAL_SURFACE('',#14844,5.0736);
#1807=CYLINDRICAL_SURFACE('',#14845,5.0736);
#1808=CYLINDRICAL_SURFACE('',#14846,5.0736);
#1809=CYLINDRICAL_SURFACE('',#14847,5.0736);
#1810=CYLINDRICAL_SURFACE('',#14848,5.0736);
#1811=CYLINDRICAL_SURFACE('',#14849,5.0736);
#1812=CYLINDRICAL_SURFACE('',#14850,5.0736);
#1813=CYLINDRICAL_SURFACE('',#14851,5.0736);
#1814=CYLINDRICAL_SURFACE('',#14852,5.0736);
#1815=CYLINDRICAL_SURFACE('',#14853,5.0736);
#1816=CYLINDRICAL_SURFACE('',#14854,5.0736);
#1817=CYLINDRICAL_SURFACE('',#14855,5.0736);
#1818=CYLINDRICAL_SURFACE('',#14856,5.0736);
#1819=CYLINDRICAL_SURFACE('',#14857,5.0736);
#1820=CYLINDRICAL_SURFACE('',#14858,5.0736);
#1821=CYLINDRICAL_SURFACE('',#14859,5.0736);
#1822=CYLINDRICAL_SURFACE('',#14860,5.0736);
#1823=CYLINDRICAL_SURFACE('',#14861,5.0736);
#1824=CYLINDRICAL_SURFACE('',#14862,5.0736);
#1825=CYLINDRICAL_SURFACE('',#14863,5.0736);
#1826=CYLINDRICAL_SURFACE('',#14864,5.0736);
#1827=CYLINDRICAL_SURFACE('',#14865,5.0736);
#1828=CYLINDRICAL_SURFACE('',#14866,5.0736);
#1829=CYLINDRICAL_SURFACE('',#14867,5.0736);
#1830=CYLINDRICAL_SURFACE('',#14868,5.0736);
#1831=CYLINDRICAL_SURFACE('',#14869,5.0736);
#1832=CYLINDRICAL_SURFACE('',#14870,5.0736);
#1833=CYLINDRICAL_SURFACE('',#14871,5.0736);
#1834=CYLINDRICAL_SURFACE('',#14872,5.0736);
#1835=CYLINDRICAL_SURFACE('',#14873,5.0736);
#1836=CYLINDRICAL_SURFACE('',#14874,5.0736);
#1837=CYLINDRICAL_SURFACE('',#14875,5.0736);
#1838=CYLINDRICAL_SURFACE('',#14876,5.0736);
#1839=CYLINDRICAL_SURFACE('',#14877,5.0736);
#1840=CYLINDRICAL_SURFACE('',#14878,5.0736);
#1841=CYLINDRICAL_SURFACE('',#14879,5.0736);
#1842=CYLINDRICAL_SURFACE('',#14880,5.0736);
#1843=CYLINDRICAL_SURFACE('',#14881,5.0736);
#1844=CYLINDRICAL_SURFACE('',#14882,5.0736);
#1845=CYLINDRICAL_SURFACE('',#14885,5.0736);
#1846=CYLINDRICAL_SURFACE('',#14886,4.51775);
#1847=CYLINDRICAL_SURFACE('',#14890,5.0736);
#1848=CYLINDRICAL_SURFACE('',#14891,4.51775);
#1849=CYLINDRICAL_SURFACE('',#14894,1.);
#1850=CYLINDRICAL_SURFACE('',#14938,1.);
#1851=CYLINDRICAL_SURFACE('',#14941,1.);
#1852=CYLINDRICAL_SURFACE('',#14944,1.);
#1853=CYLINDRICAL_SURFACE('',#14947,1.);
#1854=CYLINDRICAL_SURFACE('',#14950,1.);
#1855=CYLINDRICAL_SURFACE('',#14952,1.);
#1856=CYLINDRICAL_SURFACE('',#14955,1.);
#1857=CYLINDRICAL_SURFACE('',#14957,1.);
#1858=CYLINDRICAL_SURFACE('',#14960,1.);
#1859=CYLINDRICAL_SURFACE('',#14962,1.);
#1860=CYLINDRICAL_SURFACE('',#14965,1.);
#1861=CYLINDRICAL_SURFACE('',#14968,1.);
#1862=CYLINDRICAL_SURFACE('',#14971,1.);
#1863=CYLINDRICAL_SURFACE('',#14974,1.);
#1864=CYLINDRICAL_SURFACE('',#14976,1.);
#1865=CYLINDRICAL_SURFACE('',#14979,1.);
#1866=CYLINDRICAL_SURFACE('',#14981,1.);
#1867=CYLINDRICAL_SURFACE('',#14984,1.);
#1868=CYLINDRICAL_SURFACE('',#14986,1.);
#1869=CYLINDRICAL_SURFACE('',#14989,1.);
#1870=CYLINDRICAL_SURFACE('',#14992,1.);
#1871=CYLINDRICAL_SURFACE('',#14995,1.);
#1872=CYLINDRICAL_SURFACE('',#14998,1.);
#1873=CYLINDRICAL_SURFACE('',#15000,1.);
#1874=CYLINDRICAL_SURFACE('',#15003,1.);
#1875=CYLINDRICAL_SURFACE('',#15005,1.);
#1876=CYLINDRICAL_SURFACE('',#15008,1.);
#1877=CYLINDRICAL_SURFACE('',#15010,1.);
#1878=CYLINDRICAL_SURFACE('',#15013,1.);
#1879=CYLINDRICAL_SURFACE('',#15016,1.);
#1880=CYLINDRICAL_SURFACE('',#15019,1.);
#1881=CYLINDRICAL_SURFACE('',#15022,1.);
#1882=CYLINDRICAL_SURFACE('',#15024,1.);
#1883=CYLINDRICAL_SURFACE('',#15027,1.);
#1884=CYLINDRICAL_SURFACE('',#15029,1.);
#1885=CYLINDRICAL_SURFACE('',#15031,3.);
#1886=CYLINDRICAL_SURFACE('',#15033,3.);
#1887=CYLINDRICAL_SURFACE('',#15035,4.);
#1888=CYLINDRICAL_SURFACE('',#15036,3.);
#1889=CYLINDRICAL_SURFACE('',#15038,3.);
#1890=CYLINDRICAL_SURFACE('',#15057,8.5);
#1891=CYLINDRICAL_SURFACE('',#15059,5.5);
#1892=CYLINDRICAL_SURFACE('',#15061,4.5);
#1893=CYLINDRICAL_SURFACE('',#15064,4.5);
#1894=CYLINDRICAL_SURFACE('',#15067,4.5);
#1895=CYLINDRICAL_SURFACE('',#15070,4.5);
#1896=CYLINDRICAL_SURFACE('',#15080,4.942);
#1897=CYLINDRICAL_SURFACE('',#15082,4.942);
#1898=CYLINDRICAL_SURFACE('',#15083,4.942);
#1899=CYLINDRICAL_SURFACE('',#15084,4.942);
#1900=CYLINDRICAL_SURFACE('',#15085,4.942);
#1901=CYLINDRICAL_SURFACE('',#15086,4.942);
#1902=CYLINDRICAL_SURFACE('',#15087,4.942);
#1903=CYLINDRICAL_SURFACE('',#15088,4.942);
#1904=CYLINDRICAL_SURFACE('',#15089,4.942);
#1905=CYLINDRICAL_SURFACE('',#15090,4.942);
#1906=CYLINDRICAL_SURFACE('',#15091,4.942);
#1907=CYLINDRICAL_SURFACE('',#15092,4.942);
#1908=CYLINDRICAL_SURFACE('',#15093,4.942);
#1909=CYLINDRICAL_SURFACE('',#15094,4.942);
#1910=CYLINDRICAL_SURFACE('',#15095,4.942);
#1911=CYLINDRICAL_SURFACE('',#15096,4.942);
#1912=CYLINDRICAL_SURFACE('',#15097,4.942);
#1913=CYLINDRICAL_SURFACE('',#15098,4.942);
#1914=CYLINDRICAL_SURFACE('',#15099,4.942);
#1915=CYLINDRICAL_SURFACE('',#15100,4.372);
#1916=CYLINDRICAL_SURFACE('',#15102,4.372);
#1917=CYLINDRICAL_SURFACE('',#15103,4.372);
#1918=CYLINDRICAL_SURFACE('',#15104,4.372);
#1919=CYLINDRICAL_SURFACE('',#15105,4.372);
#1920=CYLINDRICAL_SURFACE('',#15106,4.372);
#1921=CYLINDRICAL_SURFACE('',#15107,4.372);
#1922=CYLINDRICAL_SURFACE('',#15108,4.372);
#1923=CYLINDRICAL_SURFACE('',#15109,4.372);
#1924=CYLINDRICAL_SURFACE('',#15110,4.372);
#1925=CYLINDRICAL_SURFACE('',#15111,4.372);
#1926=CYLINDRICAL_SURFACE('',#15112,4.372);
#1927=CYLINDRICAL_SURFACE('',#15113,4.372);
#1928=CYLINDRICAL_SURFACE('',#15114,4.372);
#1929=CYLINDRICAL_SURFACE('',#15115,4.372);
#1930=CYLINDRICAL_SURFACE('',#15116,4.372);
#1931=CYLINDRICAL_SURFACE('',#15117,4.372);
#1932=CYLINDRICAL_SURFACE('',#15118,4.372);
#1933=CYLINDRICAL_SURFACE('',#15119,4.372);
#1934=CYLINDRICAL_SURFACE('',#15123,4.372);
#1935=CYLINDRICAL_SURFACE('',#15125,4.942);
#1936=CYLINDRICAL_SURFACE('',#15135,8.);
#1937=CYLINDRICAL_SURFACE('',#15140,30.);
#1938=CYLINDRICAL_SURFACE('',#15146,2.5175);
#1939=CYLINDRICAL_SURFACE('',#15150,2.5175);
#1940=CYLINDRICAL_SURFACE('',#15151,2.5175);
#1941=CYLINDRICAL_SURFACE('',#15152,2.5175);
#1942=CYLINDRICAL_SURFACE('',#15153,2.5175);
#1943=CYLINDRICAL_SURFACE('',#15154,2.5175);
#1944=CYLINDRICAL_SURFACE('',#15155,2.5175);
#1945=CYLINDRICAL_SURFACE('',#15156,2.5175);
#1946=CYLINDRICAL_SURFACE('',#15158,3.0735);
#1947=CYLINDRICAL_SURFACE('',#15160,3.0735);
#1948=CYLINDRICAL_SURFACE('',#15161,3.0735);
#1949=CYLINDRICAL_SURFACE('',#15162,3.0735);
#1950=CYLINDRICAL_SURFACE('',#15163,3.0735);
#1951=CYLINDRICAL_SURFACE('',#15164,3.0735);
#1952=CYLINDRICAL_SURFACE('',#15165,3.0735);
#1953=CYLINDRICAL_SURFACE('',#15166,3.0735);
#1954=CYLINDRICAL_SURFACE('',#15168,2.5175);
#1955=CYLINDRICAL_SURFACE('',#15172,2.5175);
#1956=CYLINDRICAL_SURFACE('',#15173,2.5175);
#1957=CYLINDRICAL_SURFACE('',#15174,2.5175);
#1958=CYLINDRICAL_SURFACE('',#15175,2.5175);
#1959=CYLINDRICAL_SURFACE('',#15176,2.5175);
#1960=CYLINDRICAL_SURFACE('',#15177,2.5175);
#1961=CYLINDRICAL_SURFACE('',#15178,2.5175);
#1962=CYLINDRICAL_SURFACE('',#15180,3.0735);
#1963=CYLINDRICAL_SURFACE('',#15182,3.0735);
#1964=CYLINDRICAL_SURFACE('',#15183,3.0735);
#1965=CYLINDRICAL_SURFACE('',#15184,3.0735);
#1966=CYLINDRICAL_SURFACE('',#15185,3.0735);
#1967=CYLINDRICAL_SURFACE('',#15186,3.0735);
#1968=CYLINDRICAL_SURFACE('',#15187,3.0735);
#1969=CYLINDRICAL_SURFACE('',#15188,3.0735);
#1970=CYLINDRICAL_SURFACE('',#15190,2.5175);
#1971=CYLINDRICAL_SURFACE('',#15194,2.5175);
#1972=CYLINDRICAL_SURFACE('',#15195,2.5175);
#1973=CYLINDRICAL_SURFACE('',#15196,2.5175);
#1974=CYLINDRICAL_SURFACE('',#15197,2.5175);
#1975=CYLINDRICAL_SURFACE('',#15198,2.5175);
#1976=CYLINDRICAL_SURFACE('',#15199,2.5175);
#1977=CYLINDRICAL_SURFACE('',#15200,2.5175);
#1978=CYLINDRICAL_SURFACE('',#15202,3.0735);
#1979=CYLINDRICAL_SURFACE('',#15204,3.0735);
#1980=CYLINDRICAL_SURFACE('',#15205,3.0735);
#1981=CYLINDRICAL_SURFACE('',#15206,3.0735);
#1982=CYLINDRICAL_SURFACE('',#15207,3.0735);
#1983=CYLINDRICAL_SURFACE('',#15208,3.0735);
#1984=CYLINDRICAL_SURFACE('',#15209,3.0735);
#1985=CYLINDRICAL_SURFACE('',#15210,3.0735);
#1986=CYLINDRICAL_SURFACE('',#15213,3.0735);
#1987=CYLINDRICAL_SURFACE('',#15214,2.5175);
#1988=CYLINDRICAL_SURFACE('',#15216,3.0735);
#1989=CYLINDRICAL_SURFACE('',#15217,2.5175);
#1990=CYLINDRICAL_SURFACE('',#15219,3.0735);
#1991=CYLINDRICAL_SURFACE('',#15220,2.5175);
#1992=CYLINDRICAL_SURFACE('',#15227,30.);
#1993=CYLINDRICAL_SURFACE('',#15233,3.5);
#1994=CYLINDRICAL_SURFACE('',#15236,3.5);
#1995=CYLINDRICAL_SURFACE('',#15239,3.5);
#1996=CYLINDRICAL_SURFACE('',#15246,5.5);
#1997=CYLINDRICAL_SURFACE('',#15248,22.);
#1998=CYLINDRICAL_SURFACE('',#15254,4.942);
#1999=CYLINDRICAL_SURFACE('',#15256,4.942);
#2000=CYLINDRICAL_SURFACE('',#15257,4.942);
#2001=CYLINDRICAL_SURFACE('',#15258,4.942);
#2002=CYLINDRICAL_SURFACE('',#15259,4.942);
#2003=CYLINDRICAL_SURFACE('',#15260,4.942);
#2004=CYLINDRICAL_SURFACE('',#15261,4.942);
#2005=CYLINDRICAL_SURFACE('',#15262,4.942);
#2006=CYLINDRICAL_SURFACE('',#15263,4.942);
#2007=CYLINDRICAL_SURFACE('',#15264,4.942);
#2008=CYLINDRICAL_SURFACE('',#15265,4.942);
#2009=CYLINDRICAL_SURFACE('',#15266,4.942);
#2010=CYLINDRICAL_SURFACE('',#15267,4.942);
#2011=CYLINDRICAL_SURFACE('',#15268,4.942);
#2012=CYLINDRICAL_SURFACE('',#15269,4.942);
#2013=CYLINDRICAL_SURFACE('',#15270,4.942);
#2014=CYLINDRICAL_SURFACE('',#15271,4.942);
#2015=CYLINDRICAL_SURFACE('',#15272,4.942);
#2016=CYLINDRICAL_SURFACE('',#15273,4.942);
#2017=CYLINDRICAL_SURFACE('',#15274,4.942);
#2018=CYLINDRICAL_SURFACE('',#15275,4.942);
#2019=CYLINDRICAL_SURFACE('',#15276,4.942);
#2020=CYLINDRICAL_SURFACE('',#15277,4.942);
#2021=CYLINDRICAL_SURFACE('',#15278,4.942);
#2022=CYLINDRICAL_SURFACE('',#15279,4.942);
#2023=CYLINDRICAL_SURFACE('',#15280,4.942);
#2024=CYLINDRICAL_SURFACE('',#15281,4.942);
#2025=CYLINDRICAL_SURFACE('',#15282,4.942);
#2026=CYLINDRICAL_SURFACE('',#15283,4.942);
#2027=CYLINDRICAL_SURFACE('',#15284,4.942);
#2028=CYLINDRICAL_SURFACE('',#15285,4.942);
#2029=CYLINDRICAL_SURFACE('',#15286,4.942);
#2030=CYLINDRICAL_SURFACE('',#15287,4.942);
#2031=CYLINDRICAL_SURFACE('',#15288,4.942);
#2032=CYLINDRICAL_SURFACE('',#15289,4.942);
#2033=CYLINDRICAL_SURFACE('',#15290,4.942);
#2034=CYLINDRICAL_SURFACE('',#15291,4.942);
#2035=CYLINDRICAL_SURFACE('',#15292,4.942);
#2036=CYLINDRICAL_SURFACE('',#15293,4.942);
#2037=CYLINDRICAL_SURFACE('',#15294,4.942);
#2038=CYLINDRICAL_SURFACE('',#15295,4.942);
#2039=CYLINDRICAL_SURFACE('',#15296,4.942);
#2040=CYLINDRICAL_SURFACE('',#15297,4.942);
#2041=CYLINDRICAL_SURFACE('',#15298,4.942);
#2042=CYLINDRICAL_SURFACE('',#15299,4.942);
#2043=CYLINDRICAL_SURFACE('',#15300,4.942);
#2044=CYLINDRICAL_SURFACE('',#15301,4.942);
#2045=CYLINDRICAL_SURFACE('',#15302,4.942);
#2046=CYLINDRICAL_SURFACE('',#15303,4.942);
#2047=CYLINDRICAL_SURFACE('',#15304,4.942);
#2048=CYLINDRICAL_SURFACE('',#15305,4.942);
#2049=CYLINDRICAL_SURFACE('',#15306,4.942);
#2050=CYLINDRICAL_SURFACE('',#15307,4.942);
#2051=CYLINDRICAL_SURFACE('',#15308,4.942);
#2052=CYLINDRICAL_SURFACE('',#15309,4.942);
#2053=CYLINDRICAL_SURFACE('',#15310,4.942);
#2054=CYLINDRICAL_SURFACE('',#15311,4.942);
#2055=CYLINDRICAL_SURFACE('',#15312,4.942);
#2056=CYLINDRICAL_SURFACE('',#15313,4.942);
#2057=CYLINDRICAL_SURFACE('',#15314,4.942);
#2058=CYLINDRICAL_SURFACE('',#15315,4.372);
#2059=CYLINDRICAL_SURFACE('',#15317,4.372);
#2060=CYLINDRICAL_SURFACE('',#15318,4.372);
#2061=CYLINDRICAL_SURFACE('',#15319,4.372);
#2062=CYLINDRICAL_SURFACE('',#15320,4.372);
#2063=CYLINDRICAL_SURFACE('',#15321,4.372);
#2064=CYLINDRICAL_SURFACE('',#15322,4.372);
#2065=CYLINDRICAL_SURFACE('',#15323,4.372);
#2066=CYLINDRICAL_SURFACE('',#15324,4.372);
#2067=CYLINDRICAL_SURFACE('',#15325,4.372);
#2068=CYLINDRICAL_SURFACE('',#15326,4.372);
#2069=CYLINDRICAL_SURFACE('',#15327,4.372);
#2070=CYLINDRICAL_SURFACE('',#15328,4.372);
#2071=CYLINDRICAL_SURFACE('',#15329,4.372);
#2072=CYLINDRICAL_SURFACE('',#15330,4.372);
#2073=CYLINDRICAL_SURFACE('',#15331,4.372);
#2074=CYLINDRICAL_SURFACE('',#15332,4.372);
#2075=CYLINDRICAL_SURFACE('',#15333,4.372);
#2076=CYLINDRICAL_SURFACE('',#15334,4.372);
#2077=CYLINDRICAL_SURFACE('',#15335,4.372);
#2078=CYLINDRICAL_SURFACE('',#15336,4.372);
#2079=CYLINDRICAL_SURFACE('',#15337,4.372);
#2080=CYLINDRICAL_SURFACE('',#15338,4.372);
#2081=CYLINDRICAL_SURFACE('',#15339,4.372);
#2082=CYLINDRICAL_SURFACE('',#15340,4.372);
#2083=CYLINDRICAL_SURFACE('',#15341,4.372);
#2084=CYLINDRICAL_SURFACE('',#15342,4.372);
#2085=CYLINDRICAL_SURFACE('',#15343,4.372);
#2086=CYLINDRICAL_SURFACE('',#15344,4.372);
#2087=CYLINDRICAL_SURFACE('',#15345,4.372);
#2088=CYLINDRICAL_SURFACE('',#15346,4.372);
#2089=CYLINDRICAL_SURFACE('',#15347,4.372);
#2090=CYLINDRICAL_SURFACE('',#15348,4.372);
#2091=CYLINDRICAL_SURFACE('',#15349,4.372);
#2092=CYLINDRICAL_SURFACE('',#15350,4.372);
#2093=CYLINDRICAL_SURFACE('',#15351,4.372);
#2094=CYLINDRICAL_SURFACE('',#15352,4.372);
#2095=CYLINDRICAL_SURFACE('',#15353,4.372);
#2096=CYLINDRICAL_SURFACE('',#15354,4.372);
#2097=CYLINDRICAL_SURFACE('',#15355,4.372);
#2098=CYLINDRICAL_SURFACE('',#15356,4.372);
#2099=CYLINDRICAL_SURFACE('',#15357,4.372);
#2100=CYLINDRICAL_SURFACE('',#15358,4.372);
#2101=CYLINDRICAL_SURFACE('',#15359,4.372);
#2102=CYLINDRICAL_SURFACE('',#15360,4.372);
#2103=CYLINDRICAL_SURFACE('',#15361,4.372);
#2104=CYLINDRICAL_SURFACE('',#15362,4.372);
#2105=CYLINDRICAL_SURFACE('',#15363,4.372);
#2106=CYLINDRICAL_SURFACE('',#15364,4.372);
#2107=CYLINDRICAL_SURFACE('',#15365,4.372);
#2108=CYLINDRICAL_SURFACE('',#15366,4.372);
#2109=CYLINDRICAL_SURFACE('',#15367,4.372);
#2110=CYLINDRICAL_SURFACE('',#15368,4.372);
#2111=CYLINDRICAL_SURFACE('',#15369,4.372);
#2112=CYLINDRICAL_SURFACE('',#15370,4.372);
#2113=CYLINDRICAL_SURFACE('',#15371,4.372);
#2114=CYLINDRICAL_SURFACE('',#15372,4.372);
#2115=CYLINDRICAL_SURFACE('',#15373,4.372);
#2116=CYLINDRICAL_SURFACE('',#15374,4.372);
#2117=CYLINDRICAL_SURFACE('',#15375,4.372);
#2118=CYLINDRICAL_SURFACE('',#15376,4.372);
#2119=CYLINDRICAL_SURFACE('',#15378,4.942);
#2120=CYLINDRICAL_SURFACE('',#15389,5.);
#2121=CYLINDRICAL_SURFACE('',#15395,4.51775);
#2122=CYLINDRICAL_SURFACE('',#15397,4.51775);
#2123=CYLINDRICAL_SURFACE('',#15398,4.51775);
#2124=CYLINDRICAL_SURFACE('',#15399,4.51775);
#2125=CYLINDRICAL_SURFACE('',#15400,4.51775);
#2126=CYLINDRICAL_SURFACE('',#15401,4.51775);
#2127=CYLINDRICAL_SURFACE('',#15402,4.51775);
#2128=CYLINDRICAL_SURFACE('',#15403,4.51775);
#2129=CYLINDRICAL_SURFACE('',#15405,5.0736);
#2130=CYLINDRICAL_SURFACE('',#15407,5.0736);
#2131=CYLINDRICAL_SURFACE('',#15408,5.0736);
#2132=CYLINDRICAL_SURFACE('',#15409,5.0736);
#2133=CYLINDRICAL_SURFACE('',#15410,5.0736);
#2134=CYLINDRICAL_SURFACE('',#15411,5.0736);
#2135=CYLINDRICAL_SURFACE('',#15412,5.0736);
#2136=CYLINDRICAL_SURFACE('',#15413,5.0736);
#2137=CYLINDRICAL_SURFACE('',#15415,5.0736);
#2138=CYLINDRICAL_SURFACE('',#15417,4.51775);
#2139=CYLINDRICAL_SURFACE('',#15426,5.5);
#2140=CYLINDRICAL_SURFACE('',#15429,11.);
#2141=CYLINDRICAL_SURFACE('',#15435,2.942);
#2142=CYLINDRICAL_SURFACE('',#15437,2.942);
#2143=CYLINDRICAL_SURFACE('',#15438,2.942);
#2144=CYLINDRICAL_SURFACE('',#15439,2.942);
#2145=CYLINDRICAL_SURFACE('',#15440,2.942);
#2146=CYLINDRICAL_SURFACE('',#15441,2.942);
#2147=CYLINDRICAL_SURFACE('',#15442,2.942);
#2148=CYLINDRICAL_SURFACE('',#15443,2.942);
#2149=CYLINDRICAL_SURFACE('',#15444,2.942);
#2150=CYLINDRICAL_SURFACE('',#15445,2.942);
#2151=CYLINDRICAL_SURFACE('',#15446,2.942);
#2152=CYLINDRICAL_SURFACE('',#15447,2.942);
#2153=CYLINDRICAL_SURFACE('',#15448,2.942);
#2154=CYLINDRICAL_SURFACE('',#15449,2.942);
#2155=CYLINDRICAL_SURFACE('',#15450,2.942);
#2156=CYLINDRICAL_SURFACE('',#15451,2.37175);
#2157=CYLINDRICAL_SURFACE('',#15453,2.37175);
#2158=CYLINDRICAL_SURFACE('',#15454,2.37175);
#2159=CYLINDRICAL_SURFACE('',#15455,2.37175);
#2160=CYLINDRICAL_SURFACE('',#15456,2.37175);
#2161=CYLINDRICAL_SURFACE('',#15457,2.37175);
#2162=CYLINDRICAL_SURFACE('',#15458,2.37175);
#2163=CYLINDRICAL_SURFACE('',#15459,2.37175);
#2164=CYLINDRICAL_SURFACE('',#15460,2.37175);
#2165=CYLINDRICAL_SURFACE('',#15461,2.37175);
#2166=CYLINDRICAL_SURFACE('',#15462,2.37175);
#2167=CYLINDRICAL_SURFACE('',#15463,2.37175);
#2168=CYLINDRICAL_SURFACE('',#15464,2.37175);
#2169=CYLINDRICAL_SURFACE('',#15465,2.37175);
#2170=CYLINDRICAL_SURFACE('',#15466,2.37175);
#2171=CYLINDRICAL_SURFACE('',#15470,2.37175);
#2172=CYLINDRICAL_SURFACE('',#15472,2.942);
#2173=CYLINDRICAL_SURFACE('',#15482,5.);
#2174=CYLINDRICAL_SURFACE('',#15487,3.5);
#2175=CYLINDRICAL_SURFACE('',#15490,7.);
#2176=SHAPE_REPRESENTATION_RELATIONSHIP('SRR','None',#63860,#2192);
#2177=SHAPE_REPRESENTATION_RELATIONSHIP('SRR','None',#63861,#2193);
#2178=SHAPE_REPRESENTATION_RELATIONSHIP('SRR','None',#63862,#2194);
#2179=SHAPE_REPRESENTATION_RELATIONSHIP('SRR','None',#63863,#2195);
#2180=SHAPE_REPRESENTATION_RELATIONSHIP('SRR','None',#63864,#2196);
#2181=SHAPE_REPRESENTATION_RELATIONSHIP('SRR','None',#63866,#2197);
#2182=SHAPE_REPRESENTATION_RELATIONSHIP('SRR','None',#63867,#2198);
#2183=SHAPE_REPRESENTATION_RELATIONSHIP('SRR','None',#63868,#2199);
#2184=SHAPE_REPRESENTATION_RELATIONSHIP('SRR','None',#63869,#2200);
#2185=SHAPE_REPRESENTATION_RELATIONSHIP('SRR','None',#63870,#2201);
#2186=SHAPE_REPRESENTATION_RELATIONSHIP('SRR','None',#63871,#2202);
#2187=SHAPE_REPRESENTATION_RELATIONSHIP('SRR','None',#63872,#2203);
#2188=SHAPE_REPRESENTATION_RELATIONSHIP('SRR','None',#63873,#2204);
#2189=SHAPE_REPRESENTATION_RELATIONSHIP('SRR','None',#63874,#2205);
#2190=SHAPE_REPRESENTATION_RELATIONSHIP('SRR','None',#63875,#2206);
#2191=SHAPE_REPRESENTATION_RELATIONSHIP('SRR','None',#63876,#2207);
#2192=ADVANCED_BREP_SHAPE_REPRESENTATION('',(#2224),#63738);
#2193=ADVANCED_BREP_SHAPE_REPRESENTATION('',(#2225),#63739);
#2194=ADVANCED_BREP_SHAPE_REPRESENTATION('',(#2226),#63740);
#2195=ADVANCED_BREP_SHAPE_REPRESENTATION('',(#2227),#63741);
#2196=ADVANCED_BREP_SHAPE_REPRESENTATION('',(#2228),#63742);
#2197=ADVANCED_BREP_SHAPE_REPRESENTATION('',(#2229),#63744);
#2198=ADVANCED_BREP_SHAPE_REPRESENTATION('',(#2230),#63745);
#2199=ADVANCED_BREP_SHAPE_REPRESENTATION('',(#2231),#63746);
#2200=ADVANCED_BREP_SHAPE_REPRESENTATION('',(#2232),#63747);
#2201=ADVANCED_BREP_SHAPE_REPRESENTATION('',(#2233),#63748);
#2202=ADVANCED_BREP_SHAPE_REPRESENTATION('',(#2234),#63749);
#2203=ADVANCED_BREP_SHAPE_REPRESENTATION('',(#2235),#63750);
#2204=ADVANCED_BREP_SHAPE_REPRESENTATION('',(#2236),#63751);
#2205=ADVANCED_BREP_SHAPE_REPRESENTATION('',(#2237),#63752);
#2206=ADVANCED_BREP_SHAPE_REPRESENTATION('',(#2238),#63753);
#2207=ADVANCED_BREP_SHAPE_REPRESENTATION('',(#2239),#63754);
#2208=STYLED_ITEM('',(#63958),#2224);
#2209=STYLED_ITEM('',(#63958),#2225);
#2210=STYLED_ITEM('',(#63959),#2226);
#2211=STYLED_ITEM('',(#63960),#2227);
#2212=STYLED_ITEM('',(#63961),#2228);
#2213=STYLED_ITEM('',(#63958),#2229);
#2214=STYLED_ITEM('',(#63962),#2230);
#2215=STYLED_ITEM('',(#63960),#2231);
#2216=STYLED_ITEM('',(#63960),#2232);
#2217=STYLED_ITEM('',(#63962),#2233);
#2218=STYLED_ITEM('',(#63959),#2234);
#2219=STYLED_ITEM('',(#63963),#2235);
#2220=STYLED_ITEM('',(#63962),#2236);
#2221=STYLED_ITEM('',(#63961),#2237);
#2222=STYLED_ITEM('',(#63960),#2238);
#2223=STYLED_ITEM('',(#63961),#2239);
#2224=MANIFOLD_SOLID_BREP('Body1',#14309);
#2225=MANIFOLD_SOLID_BREP('Body1',#14310);
#2226=MANIFOLD_SOLID_BREP('Body1',#14311);
#2227=MANIFOLD_SOLID_BREP('Body1',#14312);
#2228=MANIFOLD_SOLID_BREP('Body1',#14313);
#2229=MANIFOLD_SOLID_BREP('Aluminum slotted profile',#14314);
#2230=MANIFOLD_SOLID_BREP('Body1',#14315);
#2231=MANIFOLD_SOLID_BREP('Body1',#14316);
#2232=MANIFOLD_SOLID_BREP('Body1',#14317);
#2233=MANIFOLD_SOLID_BREP('Body1',#14318);
#2234=MANIFOLD_SOLID_BREP('Body1',#14319);
#2235=MANIFOLD_SOLID_BREP('Body1',#14320);
#2236=MANIFOLD_SOLID_BREP('Body1',#14321);
#2237=MANIFOLD_SOLID_BREP('Body1',#14322);
#2238=MANIFOLD_SOLID_BREP('Body1',#14323);
#2239=MANIFOLD_SOLID_BREP('Body1',#14324);
#2240=FACE_BOUND('',#3072,.T.);
#2241=FACE_BOUND('',#3074,.T.);
#2242=FACE_BOUND('',#3084,.T.);
#2243=FACE_BOUND('',#3086,.T.);
#2244=FACE_BOUND('',#3155,.T.);
#2245=FACE_BOUND('',#3156,.T.);
#2246=FACE_BOUND('',#3157,.T.);
#2247=FACE_BOUND('',#3158,.T.);
#2248=FACE_BOUND('',#3177,.T.);
#2249=FACE_BOUND('',#3178,.T.);
#2250=FACE_BOUND('',#3179,.T.);
#2251=FACE_BOUND('',#3180,.T.);
#2252=FACE_BOUND('',#3242,.T.);
#2253=FACE_BOUND('',#3245,.T.);
#2254=FACE_BOUND('',#3250,.T.);
#2255=FACE_BOUND('',#3252,.T.);
#2256=FACE_BOUND('',#3389,.T.);
#2257=FACE_BOUND('',#3396,.T.);
#2258=FACE_BOUND('',#3400,.T.);
#2259=FACE_BOUND('',#3401,.T.);
#2260=FACE_BOUND('',#3402,.T.);
#2261=FACE_BOUND('',#3403,.T.);
#2262=FACE_BOUND('',#3404,.T.);
#2263=FACE_BOUND('',#3481,.T.);
#2264=FACE_BOUND('',#3482,.T.);
#2265=FACE_BOUND('',#3483,.T.);
#2266=FACE_BOUND('',#3484,.T.);
#2267=FACE_BOUND('',#3485,.T.);
#2268=FACE_BOUND('',#3487,.T.);
#2269=FACE_BOUND('',#3499,.T.);
#2270=FACE_BOUND('',#3500,.T.);
#2271=FACE_BOUND('',#3501,.T.);
#2272=FACE_BOUND('',#3502,.T.);
#2273=FACE_BOUND('',#3503,.T.);
#2274=FACE_BOUND('',#3505,.T.);
#2275=FACE_BOUND('',#3506,.T.);
#2276=FACE_BOUND('',#3507,.T.);
#2277=FACE_BOUND('',#3508,.T.);
#2278=FACE_BOUND('',#3509,.T.);
#2279=FACE_BOUND('',#3561,.T.);
#2280=FACE_BOUND('',#3564,.T.);
#2281=FACE_BOUND('',#3638,.T.);
#2282=FACE_BOUND('',#3639,.T.);
#2283=FACE_BOUND('',#3640,.T.);
#2284=FACE_BOUND('',#3641,.T.);
#2285=FACE_BOUND('',#3650,.T.);
#2286=FACE_BOUND('',#3651,.T.);
#2287=FACE_BOUND('',#3652,.T.);
#2288=FACE_BOUND('',#3653,.T.);
#2289=FACE_BOUND('',#3655,.T.);
#2290=FACE_BOUND('',#3656,.T.);
#2291=FACE_BOUND('',#3657,.T.);
#2292=FACE_BOUND('',#3658,.T.);
#2293=FACE_BOUND('',#3784,.T.);
#2294=FACE_BOUND('',#3786,.T.);
#2295=FACE_BOUND('',#3816,.T.);
#2296=FACE_BOUND('',#3825,.T.);
#2297=FACE_BOUND('',#3829,.T.);
#2298=FACE_BOUND('',#3831,.T.);
#2299=FACE_BOUND('',#3875,.T.);
#2300=FACE_BOUND('',#3878,.T.);
#2301=FACE_BOUND('',#3883,.T.);
#2302=FACE_BOUND('',#3885,.T.);
#2303=FACE_OUTER_BOUND('',#3063,.T.);
#2304=FACE_OUTER_BOUND('',#3064,.T.);
#2305=FACE_OUTER_BOUND('',#3065,.T.);
#2306=FACE_OUTER_BOUND('',#3066,.T.);
#2307=FACE_OUTER_BOUND('',#3067,.T.);
#2308=FACE_OUTER_BOUND('',#3068,.T.);
#2309=FACE_OUTER_BOUND('',#3069,.T.);
#2310=FACE_OUTER_BOUND('',#3070,.T.);
#2311=FACE_OUTER_BOUND('',#3071,.T.);
#2312=FACE_OUTER_BOUND('',#3073,.T.);
#2313=FACE_OUTER_BOUND('',#3075,.T.);
#2314=FACE_OUTER_BOUND('',#3076,.T.);
#2315=FACE_OUTER_BOUND('',#3077,.T.);
#2316=FACE_OUTER_BOUND('',#3078,.T.);
#2317=FACE_OUTER_BOUND('',#3079,.T.);
#2318=FACE_OUTER_BOUND('',#3080,.T.);
#2319=FACE_OUTER_BOUND('',#3081,.T.);
#2320=FACE_OUTER_BOUND('',#3082,.T.);
#2321=FACE_OUTER_BOUND('',#3083,.T.);
#2322=FACE_OUTER_BOUND('',#3085,.T.);
#2323=FACE_OUTER_BOUND('',#3087,.T.);
#2324=FACE_OUTER_BOUND('',#3088,.T.);
#2325=FACE_OUTER_BOUND('',#3089,.T.);
#2326=FACE_OUTER_BOUND('',#3090,.T.);
#2327=FACE_OUTER_BOUND('',#3091,.T.);
#2328=FACE_OUTER_BOUND('',#3092,.T.);
#2329=FACE_OUTER_BOUND('',#3093,.T.);
#2330=FACE_OUTER_BOUND('',#3094,.T.);
#2331=FACE_OUTER_BOUND('',#3095,.T.);
#2332=FACE_OUTER_BOUND('',#3096,.T.);
#2333=FACE_OUTER_BOUND('',#3097,.T.);
#2334=FACE_OUTER_BOUND('',#3098,.T.);
#2335=FACE_OUTER_BOUND('',#3099,.T.);
#2336=FACE_OUTER_BOUND('',#3100,.T.);
#2337=FACE_OUTER_BOUND('',#3101,.T.);
#2338=FACE_OUTER_BOUND('',#3102,.T.);
#2339=FACE_OUTER_BOUND('',#3103,.T.);
#2340=FACE_OUTER_BOUND('',#3104,.T.);
#2341=FACE_OUTER_BOUND('',#3105,.T.);
#2342=FACE_OUTER_BOUND('',#3106,.T.);
#2343=FACE_OUTER_BOUND('',#3107,.T.);
#2344=FACE_OUTER_BOUND('',#3108,.T.);
#2345=FACE_OUTER_BOUND('',#3109,.T.);
#2346=FACE_OUTER_BOUND('',#3110,.T.);
#2347=FACE_OUTER_BOUND('',#3111,.T.);
#2348=FACE_OUTER_BOUND('',#3112,.T.);
#2349=FACE_OUTER_BOUND('',#3113,.T.);
#2350=FACE_OUTER_BOUND('',#3114,.T.);
#2351=FACE_OUTER_BOUND('',#3115,.T.);
#2352=FACE_OUTER_BOUND('',#3116,.T.);
#2353=FACE_OUTER_BOUND('',#3117,.T.);
#2354=FACE_OUTER_BOUND('',#3118,.T.);
#2355=FACE_OUTER_BOUND('',#3119,.T.);
#2356=FACE_OUTER_BOUND('',#3120,.T.);
#2357=FACE_OUTER_BOUND('',#3121,.T.);
#2358=FACE_OUTER_BOUND('',#3122,.T.);
#2359=FACE_OUTER_BOUND('',#3123,.T.);
#2360=FACE_OUTER_BOUND('',#3124,.T.);
#2361=FACE_OUTER_BOUND('',#3125,.T.);
#2362=FACE_OUTER_BOUND('',#3126,.T.);
#2363=FACE_OUTER_BOUND('',#3127,.T.);
#2364=FACE_OUTER_BOUND('',#3128,.T.);
#2365=FACE_OUTER_BOUND('',#3129,.T.);
#2366=FACE_OUTER_BOUND('',#3130,.T.);
#2367=FACE_OUTER_BOUND('',#3131,.T.);
#2368=FACE_OUTER_BOUND('',#3132,.T.);
#2369=FACE_OUTER_BOUND('',#3133,.T.);
#2370=FACE_OUTER_BOUND('',#3134,.T.);
#2371=FACE_OUTER_BOUND('',#3135,.T.);
#2372=FACE_OUTER_BOUND('',#3136,.T.);
#2373=FACE_OUTER_BOUND('',#3137,.T.);
#2374=FACE_OUTER_BOUND('',#3138,.T.);
#2375=FACE_OUTER_BOUND('',#3139,.T.);
#2376=FACE_OUTER_BOUND('',#3140,.T.);
#2377=FACE_OUTER_BOUND('',#3141,.T.);
#2378=FACE_OUTER_BOUND('',#3142,.T.);
#2379=FACE_OUTER_BOUND('',#3143,.T.);
#2380=FACE_OUTER_BOUND('',#3144,.T.);
#2381=FACE_OUTER_BOUND('',#3145,.T.);
#2382=FACE_OUTER_BOUND('',#3146,.T.);
#2383=FACE_OUTER_BOUND('',#3147,.T.);
#2384=FACE_OUTER_BOUND('',#3148,.T.);
#2385=FACE_OUTER_BOUND('',#3149,.T.);
#2386=FACE_OUTER_BOUND('',#3150,.T.);
#2387=FACE_OUTER_BOUND('',#3151,.T.);
#2388=FACE_OUTER_BOUND('',#3152,.T.);
#2389=FACE_OUTER_BOUND('',#3153,.T.);
#2390=FACE_OUTER_BOUND('',#3154,.T.);
#2391=FACE_OUTER_BOUND('',#3159,.T.);
#2392=FACE_OUTER_BOUND('',#3160,.T.);
#2393=FACE_OUTER_BOUND('',#3161,.T.);
#2394=FACE_OUTER_BOUND('',#3162,.T.);
#2395=FACE_OUTER_BOUND('',#3163,.T.);
#2396=FACE_OUTER_BOUND('',#3164,.T.);
#2397=FACE_OUTER_BOUND('',#3165,.T.);
#2398=FACE_OUTER_BOUND('',#3166,.T.);
#2399=FACE_OUTER_BOUND('',#3167,.T.);
#2400=FACE_OUTER_BOUND('',#3168,.T.);
#2401=FACE_OUTER_BOUND('',#3169,.T.);
#2402=FACE_OUTER_BOUND('',#3170,.T.);
#2403=FACE_OUTER_BOUND('',#3171,.T.);
#2404=FACE_OUTER_BOUND('',#3172,.T.);
#2405=FACE_OUTER_BOUND('',#3173,.T.);
#2406=FACE_OUTER_BOUND('',#3174,.T.);
#2407=FACE_OUTER_BOUND('',#3175,.T.);
#2408=FACE_OUTER_BOUND('',#3176,.T.);
#2409=FACE_OUTER_BOUND('',#3181,.T.);
#2410=FACE_OUTER_BOUND('',#3182,.T.);
#2411=FACE_OUTER_BOUND('',#3183,.T.);
#2412=FACE_OUTER_BOUND('',#3184,.T.);
#2413=FACE_OUTER_BOUND('',#3185,.T.);
#2414=FACE_OUTER_BOUND('',#3186,.T.);
#2415=FACE_OUTER_BOUND('',#3187,.T.);
#2416=FACE_OUTER_BOUND('',#3188,.T.);
#2417=FACE_OUTER_BOUND('',#3189,.T.);
#2418=FACE_OUTER_BOUND('',#3190,.T.);
#2419=FACE_OUTER_BOUND('',#3191,.T.);
#2420=FACE_OUTER_BOUND('',#3192,.T.);
#2421=FACE_OUTER_BOUND('',#3193,.T.);
#2422=FACE_OUTER_BOUND('',#3194,.T.);
#2423=FACE_OUTER_BOUND('',#3195,.T.);
#2424=FACE_OUTER_BOUND('',#3196,.T.);
#2425=FACE_OUTER_BOUND('',#3197,.T.);
#2426=FACE_OUTER_BOUND('',#3198,.T.);
#2427=FACE_OUTER_BOUND('',#3199,.T.);
#2428=FACE_OUTER_BOUND('',#3200,.T.);
#2429=FACE_OUTER_BOUND('',#3201,.T.);
#2430=FACE_OUTER_BOUND('',#3202,.T.);
#2431=FACE_OUTER_BOUND('',#3203,.T.);
#2432=FACE_OUTER_BOUND('',#3204,.T.);
#2433=FACE_OUTER_BOUND('',#3205,.T.);
#2434=FACE_OUTER_BOUND('',#3206,.T.);
#2435=FACE_OUTER_BOUND('',#3207,.T.);
#2436=FACE_OUTER_BOUND('',#3208,.T.);
#2437=FACE_OUTER_BOUND('',#3209,.T.);
#2438=FACE_OUTER_BOUND('',#3210,.T.);
#2439=FACE_OUTER_BOUND('',#3211,.T.);
#2440=FACE_OUTER_BOUND('',#3212,.T.);
#2441=FACE_OUTER_BOUND('',#3213,.T.);
#2442=FACE_OUTER_BOUND('',#3214,.T.);
#2443=FACE_OUTER_BOUND('',#3215,.T.);
#2444=FACE_OUTER_BOUND('',#3216,.T.);
#2445=FACE_OUTER_BOUND('',#3217,.T.);
#2446=FACE_OUTER_BOUND('',#3218,.T.);
#2447=FACE_OUTER_BOUND('',#3219,.T.);
#2448=FACE_OUTER_BOUND('',#3220,.T.);
#2449=FACE_OUTER_BOUND('',#3221,.T.);
#2450=FACE_OUTER_BOUND('',#3222,.T.);
#2451=FACE_OUTER_BOUND('',#3223,.T.);
#2452=FACE_OUTER_BOUND('',#3224,.T.);
#2453=FACE_OUTER_BOUND('',#3225,.T.);
#2454=FACE_OUTER_BOUND('',#3226,.T.);
#2455=FACE_OUTER_BOUND('',#3227,.T.);
#2456=FACE_OUTER_BOUND('',#3228,.T.);
#2457=FACE_OUTER_BOUND('',#3229,.T.);
#2458=FACE_OUTER_BOUND('',#3230,.T.);
#2459=FACE_OUTER_BOUND('',#3231,.T.);
#2460=FACE_OUTER_BOUND('',#3232,.T.);
#2461=FACE_OUTER_BOUND('',#3233,.T.);
#2462=FACE_OUTER_BOUND('',#3234,.T.);
#2463=FACE_OUTER_BOUND('',#3235,.T.);
#2464=FACE_OUTER_BOUND('',#3236,.T.);
#2465=FACE_OUTER_BOUND('',#3237,.T.);
#2466=FACE_OUTER_BOUND('',#3238,.T.);
#2467=FACE_OUTER_BOUND('',#3239,.T.);
#2468=FACE_OUTER_BOUND('',#3240,.T.);
#2469=FACE_OUTER_BOUND('',#3241,.T.);
#2470=FACE_OUTER_BOUND('',#3243,.T.);
#2471=FACE_OUTER_BOUND('',#3244,.T.);
#2472=FACE_OUTER_BOUND('',#3246,.T.);
#2473=FACE_OUTER_BOUND('',#3247,.T.);
#2474=FACE_OUTER_BOUND('',#3248,.T.);
#2475=FACE_OUTER_BOUND('',#3249,.T.);
#2476=FACE_OUTER_BOUND('',#3251,.T.);
#2477=FACE_OUTER_BOUND('',#3253,.T.);
#2478=FACE_OUTER_BOUND('',#3254,.T.);
#2479=FACE_OUTER_BOUND('',#3255,.T.);
#2480=FACE_OUTER_BOUND('',#3256,.T.);
#2481=FACE_OUTER_BOUND('',#3257,.T.);
#2482=FACE_OUTER_BOUND('',#3258,.T.);
#2483=FACE_OUTER_BOUND('',#3259,.T.);
#2484=FACE_OUTER_BOUND('',#3260,.T.);
#2485=FACE_OUTER_BOUND('',#3261,.T.);
#2486=FACE_OUTER_BOUND('',#3262,.T.);
#2487=FACE_OUTER_BOUND('',#3263,.T.);
#2488=FACE_OUTER_BOUND('',#3264,.T.);
#2489=FACE_OUTER_BOUND('',#3265,.T.);
#2490=FACE_OUTER_BOUND('',#3266,.T.);
#2491=FACE_OUTER_BOUND('',#3267,.T.);
#2492=FACE_OUTER_BOUND('',#3268,.T.);
#2493=FACE_OUTER_BOUND('',#3269,.T.);
#2494=FACE_OUTER_BOUND('',#3270,.T.);
#2495=FACE_OUTER_BOUND('',#3271,.T.);
#2496=FACE_OUTER_BOUND('',#3272,.T.);
#2497=FACE_OUTER_BOUND('',#3273,.T.);
#2498=FACE_OUTER_BOUND('',#3274,.T.);
#2499=FACE_OUTER_BOUND('',#3275,.T.);
#2500=FACE_OUTER_BOUND('',#3276,.T.);
#2501=FACE_OUTER_BOUND('',#3277,.T.);
#2502=FACE_OUTER_BOUND('',#3278,.T.);
#2503=FACE_OUTER_BOUND('',#3279,.T.);
#2504=FACE_OUTER_BOUND('',#3280,.T.);
#2505=FACE_OUTER_BOUND('',#3281,.T.);
#2506=FACE_OUTER_BOUND('',#3282,.T.);
#2507=FACE_OUTER_BOUND('',#3283,.T.);
#2508=FACE_OUTER_BOUND('',#3284,.T.);
#2509=FACE_OUTER_BOUND('',#3285,.T.);
#2510=FACE_OUTER_BOUND('',#3286,.T.);
#2511=FACE_OUTER_BOUND('',#3287,.T.);
#2512=FACE_OUTER_BOUND('',#3288,.T.);
#2513=FACE_OUTER_BOUND('',#3289,.T.);
#2514=FACE_OUTER_BOUND('',#3290,.T.);
#2515=FACE_OUTER_BOUND('',#3291,.T.);
#2516=FACE_OUTER_BOUND('',#3292,.T.);
#2517=FACE_OUTER_BOUND('',#3293,.T.);
#2518=FACE_OUTER_BOUND('',#3294,.T.);
#2519=FACE_OUTER_BOUND('',#3295,.T.);
#2520=FACE_OUTER_BOUND('',#3296,.T.);
#2521=FACE_OUTER_BOUND('',#3297,.T.);
#2522=FACE_OUTER_BOUND('',#3298,.T.);
#2523=FACE_OUTER_BOUND('',#3299,.T.);
#2524=FACE_OUTER_BOUND('',#3300,.T.);
#2525=FACE_OUTER_BOUND('',#3301,.T.);
#2526=FACE_OUTER_BOUND('',#3302,.T.);
#2527=FACE_OUTER_BOUND('',#3303,.T.);
#2528=FACE_OUTER_BOUND('',#3304,.T.);
#2529=FACE_OUTER_BOUND('',#3305,.T.);
#2530=FACE_OUTER_BOUND('',#3306,.T.);
#2531=FACE_OUTER_BOUND('',#3307,.T.);
#2532=FACE_OUTER_BOUND('',#3308,.T.);
#2533=FACE_OUTER_BOUND('',#3309,.T.);
#2534=FACE_OUTER_BOUND('',#3310,.T.);
#2535=FACE_OUTER_BOUND('',#3311,.T.);
#2536=FACE_OUTER_BOUND('',#3312,.T.);
#2537=FACE_OUTER_BOUND('',#3313,.T.);
#2538=FACE_OUTER_BOUND('',#3314,.T.);
#2539=FACE_OUTER_BOUND('',#3315,.T.);
#2540=FACE_OUTER_BOUND('',#3316,.T.);
#2541=FACE_OUTER_BOUND('',#3317,.T.);
#2542=FACE_OUTER_BOUND('',#3318,.T.);
#2543=FACE_OUTER_BOUND('',#3319,.T.);
#2544=FACE_OUTER_BOUND('',#3320,.T.);
#2545=FACE_OUTER_BOUND('',#3321,.T.);
#2546=FACE_OUTER_BOUND('',#3322,.T.);
#2547=FACE_OUTER_BOUND('',#3323,.T.);
#2548=FACE_OUTER_BOUND('',#3324,.T.);
#2549=FACE_OUTER_BOUND('',#3325,.T.);
#2550=FACE_OUTER_BOUND('',#3326,.T.);
#2551=FACE_OUTER_BOUND('',#3327,.T.);
#2552=FACE_OUTER_BOUND('',#3328,.T.);
#2553=FACE_OUTER_BOUND('',#3329,.T.);
#2554=FACE_OUTER_BOUND('',#3330,.T.);
#2555=FACE_OUTER_BOUND('',#3331,.T.);
#2556=FACE_OUTER_BOUND('',#3332,.T.);
#2557=FACE_OUTER_BOUND('',#3333,.T.);
#2558=FACE_OUTER_BOUND('',#3334,.T.);
#2559=FACE_OUTER_BOUND('',#3335,.T.);
#2560=FACE_OUTER_BOUND('',#3336,.T.);
#2561=FACE_OUTER_BOUND('',#3337,.T.);
#2562=FACE_OUTER_BOUND('',#3338,.T.);
#2563=FACE_OUTER_BOUND('',#3339,.T.);
#2564=FACE_OUTER_BOUND('',#3340,.T.);
#2565=FACE_OUTER_BOUND('',#3341,.T.);
#2566=FACE_OUTER_BOUND('',#3342,.T.);
#2567=FACE_OUTER_BOUND('',#3343,.T.);
#2568=FACE_OUTER_BOUND('',#3344,.T.);
#2569=FACE_OUTER_BOUND('',#3345,.T.);
#2570=FACE_OUTER_BOUND('',#3346,.T.);
#2571=FACE_OUTER_BOUND('',#3347,.T.);
#2572=FACE_OUTER_BOUND('',#3348,.T.);
#2573=FACE_OUTER_BOUND('',#3349,.T.);
#2574=FACE_OUTER_BOUND('',#3350,.T.);
#2575=FACE_OUTER_BOUND('',#3351,.T.);
#2576=FACE_OUTER_BOUND('',#3352,.T.);
#2577=FACE_OUTER_BOUND('',#3353,.T.);
#2578=FACE_OUTER_BOUND('',#3354,.T.);
#2579=FACE_OUTER_BOUND('',#3355,.T.);
#2580=FACE_OUTER_BOUND('',#3356,.T.);
#2581=FACE_OUTER_BOUND('',#3357,.T.);
#2582=FACE_OUTER_BOUND('',#3358,.T.);
#2583=FACE_OUTER_BOUND('',#3359,.T.);
#2584=FACE_OUTER_BOUND('',#3360,.T.);
#2585=FACE_OUTER_BOUND('',#3361,.T.);
#2586=FACE_OUTER_BOUND('',#3362,.T.);
#2587=FACE_OUTER_BOUND('',#3363,.T.);
#2588=FACE_OUTER_BOUND('',#3364,.T.);
#2589=FACE_OUTER_BOUND('',#3365,.T.);
#2590=FACE_OUTER_BOUND('',#3366,.T.);
#2591=FACE_OUTER_BOUND('',#3367,.T.);
#2592=FACE_OUTER_BOUND('',#3368,.T.);
#2593=FACE_OUTER_BOUND('',#3369,.T.);
#2594=FACE_OUTER_BOUND('',#3370,.T.);
#2595=FACE_OUTER_BOUND('',#3371,.T.);
#2596=FACE_OUTER_BOUND('',#3372,.T.);
#2597=FACE_OUTER_BOUND('',#3373,.T.);
#2598=FACE_OUTER_BOUND('',#3374,.T.);
#2599=FACE_OUTER_BOUND('',#3375,.T.);
#2600=FACE_OUTER_BOUND('',#3376,.T.);
#2601=FACE_OUTER_BOUND('',#3377,.T.);
#2602=FACE_OUTER_BOUND('',#3378,.T.);
#2603=FACE_OUTER_BOUND('',#3379,.T.);
#2604=FACE_OUTER_BOUND('',#3380,.T.);
#2605=FACE_OUTER_BOUND('',#3381,.T.);
#2606=FACE_OUTER_BOUND('',#3382,.T.);
#2607=FACE_OUTER_BOUND('',#3383,.T.);
#2608=FACE_OUTER_BOUND('',#3384,.T.);
#2609=FACE_OUTER_BOUND('',#3385,.T.);
#2610=FACE_OUTER_BOUND('',#3386,.T.);
#2611=FACE_OUTER_BOUND('',#3387,.T.);
#2612=FACE_OUTER_BOUND('',#3388,.T.);
#2613=FACE_OUTER_BOUND('',#3390,.T.);
#2614=FACE_OUTER_BOUND('',#3391,.T.);
#2615=FACE_OUTER_BOUND('',#3392,.T.);
#2616=FACE_OUTER_BOUND('',#3393,.T.);
#2617=FACE_OUTER_BOUND('',#3394,.T.);
#2618=FACE_OUTER_BOUND('',#3395,.T.);
#2619=FACE_OUTER_BOUND('',#3397,.T.);
#2620=FACE_OUTER_BOUND('',#3398,.T.);
#2621=FACE_OUTER_BOUND('',#3399,.T.);
#2622=FACE_OUTER_BOUND('',#3405,.T.);
#2623=FACE_OUTER_BOUND('',#3406,.T.);
#2624=FACE_OUTER_BOUND('',#3407,.T.);
#2625=FACE_OUTER_BOUND('',#3408,.T.);
#2626=FACE_OUTER_BOUND('',#3409,.T.);
#2627=FACE_OUTER_BOUND('',#3410,.T.);
#2628=FACE_OUTER_BOUND('',#3411,.T.);
#2629=FACE_OUTER_BOUND('',#3412,.T.);
#2630=FACE_OUTER_BOUND('',#3413,.T.);
#2631=FACE_OUTER_BOUND('',#3414,.T.);
#2632=FACE_OUTER_BOUND('',#3415,.T.);
#2633=FACE_OUTER_BOUND('',#3416,.T.);
#2634=FACE_OUTER_BOUND('',#3417,.T.);
#2635=FACE_OUTER_BOUND('',#3418,.T.);
#2636=FACE_OUTER_BOUND('',#3419,.T.);
#2637=FACE_OUTER_BOUND('',#3420,.T.);
#2638=FACE_OUTER_BOUND('',#3421,.T.);
#2639=FACE_OUTER_BOUND('',#3422,.T.);
#2640=FACE_OUTER_BOUND('',#3423,.T.);
#2641=FACE_OUTER_BOUND('',#3424,.T.);
#2642=FACE_OUTER_BOUND('',#3425,.T.);
#2643=FACE_OUTER_BOUND('',#3426,.T.);
#2644=FACE_OUTER_BOUND('',#3427,.T.);
#2645=FACE_OUTER_BOUND('',#3428,.T.);
#2646=FACE_OUTER_BOUND('',#3429,.T.);
#2647=FACE_OUTER_BOUND('',#3430,.T.);
#2648=FACE_OUTER_BOUND('',#3431,.T.);
#2649=FACE_OUTER_BOUND('',#3432,.T.);
#2650=FACE_OUTER_BOUND('',#3433,.T.);
#2651=FACE_OUTER_BOUND('',#3434,.T.);
#2652=FACE_OUTER_BOUND('',#3435,.T.);
#2653=FACE_OUTER_BOUND('',#3436,.T.);
#2654=FACE_OUTER_BOUND('',#3437,.T.);
#2655=FACE_OUTER_BOUND('',#3438,.T.);
#2656=FACE_OUTER_BOUND('',#3439,.T.);
#2657=FACE_OUTER_BOUND('',#3440,.T.);
#2658=FACE_OUTER_BOUND('',#3441,.T.);
#2659=FACE_OUTER_BOUND('',#3442,.T.);
#2660=FACE_OUTER_BOUND('',#3443,.T.);
#2661=FACE_OUTER_BOUND('',#3444,.T.);
#2662=FACE_OUTER_BOUND('',#3445,.T.);
#2663=FACE_OUTER_BOUND('',#3446,.T.);
#2664=FACE_OUTER_BOUND('',#3447,.T.);
#2665=FACE_OUTER_BOUND('',#3448,.T.);
#2666=FACE_OUTER_BOUND('',#3449,.T.);
#2667=FACE_OUTER_BOUND('',#3450,.T.);
#2668=FACE_OUTER_BOUND('',#3451,.T.);
#2669=FACE_OUTER_BOUND('',#3452,.T.);
#2670=FACE_OUTER_BOUND('',#3453,.T.);
#2671=FACE_OUTER_BOUND('',#3454,.T.);
#2672=FACE_OUTER_BOUND('',#3455,.T.);
#2673=FACE_OUTER_BOUND('',#3456,.T.);
#2674=FACE_OUTER_BOUND('',#3457,.T.);
#2675=FACE_OUTER_BOUND('',#3458,.T.);
#2676=FACE_OUTER_BOUND('',#3459,.T.);
#2677=FACE_OUTER_BOUND('',#3460,.T.);
#2678=FACE_OUTER_BOUND('',#3461,.T.);
#2679=FACE_OUTER_BOUND('',#3462,.T.);
#2680=FACE_OUTER_BOUND('',#3463,.T.);
#2681=FACE_OUTER_BOUND('',#3464,.T.);
#2682=FACE_OUTER_BOUND('',#3465,.T.);
#2683=FACE_OUTER_BOUND('',#3466,.T.);
#2684=FACE_OUTER_BOUND('',#3467,.T.);
#2685=FACE_OUTER_BOUND('',#3468,.T.);
#2686=FACE_OUTER_BOUND('',#3469,.T.);
#2687=FACE_OUTER_BOUND('',#3470,.T.);
#2688=FACE_OUTER_BOUND('',#3471,.T.);
#2689=FACE_OUTER_BOUND('',#3472,.T.);
#2690=FACE_OUTER_BOUND('',#3473,.T.);
#2691=FACE_OUTER_BOUND('',#3474,.T.);
#2692=FACE_OUTER_BOUND('',#3475,.T.);
#2693=FACE_OUTER_BOUND('',#3476,.T.);
#2694=FACE_OUTER_BOUND('',#3477,.T.);
#2695=FACE_OUTER_BOUND('',#3478,.T.);
#2696=FACE_OUTER_BOUND('',#3479,.T.);
#2697=FACE_OUTER_BOUND('',#3480,.T.);
#2698=FACE_OUTER_BOUND('',#3486,.T.);
#2699=FACE_OUTER_BOUND('',#3488,.T.);
#2700=FACE_OUTER_BOUND('',#3489,.T.);
#2701=FACE_OUTER_BOUND('',#3490,.T.);
#2702=FACE_OUTER_BOUND('',#3491,.T.);
#2703=FACE_OUTER_BOUND('',#3492,.T.);
#2704=FACE_OUTER_BOUND('',#3493,.T.);
#2705=FACE_OUTER_BOUND('',#3494,.T.);
#2706=FACE_OUTER_BOUND('',#3495,.T.);
#2707=FACE_OUTER_BOUND('',#3496,.T.);
#2708=FACE_OUTER_BOUND('',#3497,.T.);
#2709=FACE_OUTER_BOUND('',#3498,.T.);
#2710=FACE_OUTER_BOUND('',#3504,.T.);
#2711=FACE_OUTER_BOUND('',#3510,.T.);
#2712=FACE_OUTER_BOUND('',#3511,.T.);
#2713=FACE_OUTER_BOUND('',#3512,.T.);
#2714=FACE_OUTER_BOUND('',#3513,.T.);
#2715=FACE_OUTER_BOUND('',#3514,.T.);
#2716=FACE_OUTER_BOUND('',#3515,.T.);
#2717=FACE_OUTER_BOUND('',#3516,.T.);
#2718=FACE_OUTER_BOUND('',#3517,.T.);
#2719=FACE_OUTER_BOUND('',#3518,.T.);
#2720=FACE_OUTER_BOUND('',#3519,.T.);
#2721=FACE_OUTER_BOUND('',#3520,.T.);
#2722=FACE_OUTER_BOUND('',#3521,.T.);
#2723=FACE_OUTER_BOUND('',#3522,.T.);
#2724=FACE_OUTER_BOUND('',#3523,.T.);
#2725=FACE_OUTER_BOUND('',#3524,.T.);
#2726=FACE_OUTER_BOUND('',#3525,.T.);
#2727=FACE_OUTER_BOUND('',#3526,.T.);
#2728=FACE_OUTER_BOUND('',#3527,.T.);
#2729=FACE_OUTER_BOUND('',#3528,.T.);
#2730=FACE_OUTER_BOUND('',#3529,.T.);
#2731=FACE_OUTER_BOUND('',#3530,.T.);
#2732=FACE_OUTER_BOUND('',#3531,.T.);
#2733=FACE_OUTER_BOUND('',#3532,.T.);
#2734=FACE_OUTER_BOUND('',#3533,.T.);
#2735=FACE_OUTER_BOUND('',#3534,.T.);
#2736=FACE_OUTER_BOUND('',#3535,.T.);
#2737=FACE_OUTER_BOUND('',#3536,.T.);
#2738=FACE_OUTER_BOUND('',#3537,.T.);
#2739=FACE_OUTER_BOUND('',#3538,.T.);
#2740=FACE_OUTER_BOUND('',#3539,.T.);
#2741=FACE_OUTER_BOUND('',#3540,.T.);
#2742=FACE_OUTER_BOUND('',#3541,.T.);
#2743=FACE_OUTER_BOUND('',#3542,.T.);
#2744=FACE_OUTER_BOUND('',#3543,.T.);
#2745=FACE_OUTER_BOUND('',#3544,.T.);
#2746=FACE_OUTER_BOUND('',#3545,.T.);
#2747=FACE_OUTER_BOUND('',#3546,.T.);
#2748=FACE_OUTER_BOUND('',#3547,.T.);
#2749=FACE_OUTER_BOUND('',#3548,.T.);
#2750=FACE_OUTER_BOUND('',#3549,.T.);
#2751=FACE_OUTER_BOUND('',#3550,.T.);
#2752=FACE_OUTER_BOUND('',#3551,.T.);
#2753=FACE_OUTER_BOUND('',#3552,.T.);
#2754=FACE_OUTER_BOUND('',#3553,.T.);
#2755=FACE_OUTER_BOUND('',#3554,.T.);
#2756=FACE_OUTER_BOUND('',#3555,.T.);
#2757=FACE_OUTER_BOUND('',#3556,.T.);
#2758=FACE_OUTER_BOUND('',#3557,.T.);
#2759=FACE_OUTER_BOUND('',#3558,.T.);
#2760=FACE_OUTER_BOUND('',#3559,.T.);
#2761=FACE_OUTER_BOUND('',#3560,.T.);
#2762=FACE_OUTER_BOUND('',#3562,.T.);
#2763=FACE_OUTER_BOUND('',#3563,.T.);
#2764=FACE_OUTER_BOUND('',#3565,.T.);
#2765=FACE_OUTER_BOUND('',#3566,.T.);
#2766=FACE_OUTER_BOUND('',#3567,.T.);
#2767=FACE_OUTER_BOUND('',#3568,.T.);
#2768=FACE_OUTER_BOUND('',#3569,.T.);
#2769=FACE_OUTER_BOUND('',#3570,.T.);
#2770=FACE_OUTER_BOUND('',#3571,.T.);
#2771=FACE_OUTER_BOUND('',#3572,.T.);
#2772=FACE_OUTER_BOUND('',#3573,.T.);
#2773=FACE_OUTER_BOUND('',#3574,.T.);
#2774=FACE_OUTER_BOUND('',#3575,.T.);
#2775=FACE_OUTER_BOUND('',#3576,.T.);
#2776=FACE_OUTER_BOUND('',#3577,.T.);
#2777=FACE_OUTER_BOUND('',#3578,.T.);
#2778=FACE_OUTER_BOUND('',#3579,.T.);
#2779=FACE_OUTER_BOUND('',#3580,.T.);
#2780=FACE_OUTER_BOUND('',#3581,.T.);
#2781=FACE_OUTER_BOUND('',#3582,.T.);
#2782=FACE_OUTER_BOUND('',#3583,.T.);
#2783=FACE_OUTER_BOUND('',#3584,.T.);
#2784=FACE_OUTER_BOUND('',#3585,.T.);
#2785=FACE_OUTER_BOUND('',#3586,.T.);
#2786=FACE_OUTER_BOUND('',#3587,.T.);
#2787=FACE_OUTER_BOUND('',#3588,.T.);
#2788=FACE_OUTER_BOUND('',#3589,.T.);
#2789=FACE_OUTER_BOUND('',#3590,.T.);
#2790=FACE_OUTER_BOUND('',#3591,.T.);
#2791=FACE_OUTER_BOUND('',#3592,.T.);
#2792=FACE_OUTER_BOUND('',#3593,.T.);
#2793=FACE_OUTER_BOUND('',#3594,.T.);
#2794=FACE_OUTER_BOUND('',#3595,.T.);
#2795=FACE_OUTER_BOUND('',#3596,.T.);
#2796=FACE_OUTER_BOUND('',#3597,.T.);
#2797=FACE_OUTER_BOUND('',#3598,.T.);
#2798=FACE_OUTER_BOUND('',#3599,.T.);
#2799=FACE_OUTER_BOUND('',#3600,.T.);
#2800=FACE_OUTER_BOUND('',#3601,.T.);
#2801=FACE_OUTER_BOUND('',#3602,.T.);
#2802=FACE_OUTER_BOUND('',#3603,.T.);
#2803=FACE_OUTER_BOUND('',#3604,.T.);
#2804=FACE_OUTER_BOUND('',#3605,.T.);
#2805=FACE_OUTER_BOUND('',#3606,.T.);
#2806=FACE_OUTER_BOUND('',#3607,.T.);
#2807=FACE_OUTER_BOUND('',#3608,.T.);
#2808=FACE_OUTER_BOUND('',#3609,.T.);
#2809=FACE_OUTER_BOUND('',#3610,.T.);
#2810=FACE_OUTER_BOUND('',#3611,.T.);
#2811=FACE_OUTER_BOUND('',#3612,.T.);
#2812=FACE_OUTER_BOUND('',#3613,.T.);
#2813=FACE_OUTER_BOUND('',#3614,.T.);
#2814=FACE_OUTER_BOUND('',#3615,.T.);
#2815=FACE_OUTER_BOUND('',#3616,.T.);
#2816=FACE_OUTER_BOUND('',#3617,.T.);
#2817=FACE_OUTER_BOUND('',#3618,.T.);
#2818=FACE_OUTER_BOUND('',#3619,.T.);
#2819=FACE_OUTER_BOUND('',#3620,.T.);
#2820=FACE_OUTER_BOUND('',#3621,.T.);
#2821=FACE_OUTER_BOUND('',#3622,.T.);
#2822=FACE_OUTER_BOUND('',#3623,.T.);
#2823=FACE_OUTER_BOUND('',#3624,.T.);
#2824=FACE_OUTER_BOUND('',#3625,.T.);
#2825=FACE_OUTER_BOUND('',#3626,.T.);
#2826=FACE_OUTER_BOUND('',#3627,.T.);
#2827=FACE_OUTER_BOUND('',#3628,.T.);
#2828=FACE_OUTER_BOUND('',#3629,.T.);
#2829=FACE_OUTER_BOUND('',#3630,.T.);
#2830=FACE_OUTER_BOUND('',#3631,.T.);
#2831=FACE_OUTER_BOUND('',#3632,.T.);
#2832=FACE_OUTER_BOUND('',#3633,.T.);
#2833=FACE_OUTER_BOUND('',#3634,.T.);
#2834=FACE_OUTER_BOUND('',#3635,.T.);
#2835=FACE_OUTER_BOUND('',#3636,.T.);
#2836=FACE_OUTER_BOUND('',#3637,.T.);
#2837=FACE_OUTER_BOUND('',#3642,.T.);
#2838=FACE_OUTER_BOUND('',#3643,.T.);
#2839=FACE_OUTER_BOUND('',#3644,.T.);
#2840=FACE_OUTER_BOUND('',#3645,.T.);
#2841=FACE_OUTER_BOUND('',#3646,.T.);
#2842=FACE_OUTER_BOUND('',#3647,.T.);
#2843=FACE_OUTER_BOUND('',#3648,.T.);
#2844=FACE_OUTER_BOUND('',#3649,.T.);
#2845=FACE_OUTER_BOUND('',#3654,.T.);
#2846=FACE_OUTER_BOUND('',#3659,.T.);
#2847=FACE_OUTER_BOUND('',#3660,.T.);
#2848=FACE_OUTER_BOUND('',#3661,.T.);
#2849=FACE_OUTER_BOUND('',#3662,.T.);
#2850=FACE_OUTER_BOUND('',#3663,.T.);
#2851=FACE_OUTER_BOUND('',#3664,.T.);
#2852=FACE_OUTER_BOUND('',#3665,.T.);
#2853=FACE_OUTER_BOUND('',#3666,.T.);
#2854=FACE_OUTER_BOUND('',#3667,.T.);
#2855=FACE_OUTER_BOUND('',#3668,.T.);
#2856=FACE_OUTER_BOUND('',#3669,.T.);
#2857=FACE_OUTER_BOUND('',#3670,.T.);
#2858=FACE_OUTER_BOUND('',#3671,.T.);
#2859=FACE_OUTER_BOUND('',#3672,.T.);
#2860=FACE_OUTER_BOUND('',#3673,.T.);
#2861=FACE_OUTER_BOUND('',#3674,.T.);
#2862=FACE_OUTER_BOUND('',#3675,.T.);
#2863=FACE_OUTER_BOUND('',#3676,.T.);
#2864=FACE_OUTER_BOUND('',#3677,.T.);
#2865=FACE_OUTER_BOUND('',#3678,.T.);
#2866=FACE_OUTER_BOUND('',#3679,.T.);
#2867=FACE_OUTER_BOUND('',#3680,.T.);
#2868=FACE_OUTER_BOUND('',#3681,.T.);
#2869=FACE_OUTER_BOUND('',#3682,.T.);
#2870=FACE_OUTER_BOUND('',#3683,.T.);
#2871=FACE_OUTER_BOUND('',#3684,.T.);
#2872=FACE_OUTER_BOUND('',#3685,.T.);
#2873=FACE_OUTER_BOUND('',#3686,.T.);
#2874=FACE_OUTER_BOUND('',#3687,.T.);
#2875=FACE_OUTER_BOUND('',#3688,.T.);
#2876=FACE_OUTER_BOUND('',#3689,.T.);
#2877=FACE_OUTER_BOUND('',#3690,.T.);
#2878=FACE_OUTER_BOUND('',#3691,.T.);
#2879=FACE_OUTER_BOUND('',#3692,.T.);
#2880=FACE_OUTER_BOUND('',#3693,.T.);
#2881=FACE_OUTER_BOUND('',#3694,.T.);
#2882=FACE_OUTER_BOUND('',#3695,.T.);
#2883=FACE_OUTER_BOUND('',#3696,.T.);
#2884=FACE_OUTER_BOUND('',#3697,.T.);
#2885=FACE_OUTER_BOUND('',#3698,.T.);
#2886=FACE_OUTER_BOUND('',#3699,.T.);
#2887=FACE_OUTER_BOUND('',#3700,.T.);
#2888=FACE_OUTER_BOUND('',#3701,.T.);
#2889=FACE_OUTER_BOUND('',#3702,.T.);
#2890=FACE_OUTER_BOUND('',#3703,.T.);
#2891=FACE_OUTER_BOUND('',#3704,.T.);
#2892=FACE_OUTER_BOUND('',#3705,.T.);
#2893=FACE_OUTER_BOUND('',#3706,.T.);
#2894=FACE_OUTER_BOUND('',#3707,.T.);
#2895=FACE_OUTER_BOUND('',#3708,.T.);
#2896=FACE_OUTER_BOUND('',#3709,.T.);
#2897=FACE_OUTER_BOUND('',#3710,.T.);
#2898=FACE_OUTER_BOUND('',#3711,.T.);
#2899=FACE_OUTER_BOUND('',#3712,.T.);
#2900=FACE_OUTER_BOUND('',#3713,.T.);
#2901=FACE_OUTER_BOUND('',#3714,.T.);
#2902=FACE_OUTER_BOUND('',#3715,.T.);
#2903=FACE_OUTER_BOUND('',#3716,.T.);
#2904=FACE_OUTER_BOUND('',#3717,.T.);
#2905=FACE_OUTER_BOUND('',#3718,.T.);
#2906=FACE_OUTER_BOUND('',#3719,.T.);
#2907=FACE_OUTER_BOUND('',#3720,.T.);
#2908=FACE_OUTER_BOUND('',#3721,.T.);
#2909=FACE_OUTER_BOUND('',#3722,.T.);
#2910=FACE_OUTER_BOUND('',#3723,.T.);
#2911=FACE_OUTER_BOUND('',#3724,.T.);
#2912=FACE_OUTER_BOUND('',#3725,.T.);
#2913=FACE_OUTER_BOUND('',#3726,.T.);
#2914=FACE_OUTER_BOUND('',#3727,.T.);
#2915=FACE_OUTER_BOUND('',#3728,.T.);
#2916=FACE_OUTER_BOUND('',#3729,.T.);
#2917=FACE_OUTER_BOUND('',#3730,.T.);
#2918=FACE_OUTER_BOUND('',#3731,.T.);
#2919=FACE_OUTER_BOUND('',#3732,.T.);
#2920=FACE_OUTER_BOUND('',#3733,.T.);
#2921=FACE_OUTER_BOUND('',#3734,.T.);
#2922=FACE_OUTER_BOUND('',#3735,.T.);
#2923=FACE_OUTER_BOUND('',#3736,.T.);
#2924=FACE_OUTER_BOUND('',#3737,.T.);
#2925=FACE_OUTER_BOUND('',#3738,.T.);
#2926=FACE_OUTER_BOUND('',#3739,.T.);
#2927=FACE_OUTER_BOUND('',#3740,.T.);
#2928=FACE_OUTER_BOUND('',#3741,.T.);
#2929=FACE_OUTER_BOUND('',#3742,.T.);
#2930=FACE_OUTER_BOUND('',#3743,.T.);
#2931=FACE_OUTER_BOUND('',#3744,.T.);
#2932=FACE_OUTER_BOUND('',#3745,.T.);
#2933=FACE_OUTER_BOUND('',#3746,.T.);
#2934=FACE_OUTER_BOUND('',#3747,.T.);
#2935=FACE_OUTER_BOUND('',#3748,.T.);
#2936=FACE_OUTER_BOUND('',#3749,.T.);
#2937=FACE_OUTER_BOUND('',#3750,.T.);
#2938=FACE_OUTER_BOUND('',#3751,.T.);
#2939=FACE_OUTER_BOUND('',#3752,.T.);
#2940=FACE_OUTER_BOUND('',#3753,.T.);
#2941=FACE_OUTER_BOUND('',#3754,.T.);
#2942=FACE_OUTER_BOUND('',#3755,.T.);
#2943=FACE_OUTER_BOUND('',#3756,.T.);
#2944=FACE_OUTER_BOUND('',#3757,.T.);
#2945=FACE_OUTER_BOUND('',#3758,.T.);
#2946=FACE_OUTER_BOUND('',#3759,.T.);
#2947=FACE_OUTER_BOUND('',#3760,.T.);
#2948=FACE_OUTER_BOUND('',#3761,.T.);
#2949=FACE_OUTER_BOUND('',#3762,.T.);
#2950=FACE_OUTER_BOUND('',#3763,.T.);
#2951=FACE_OUTER_BOUND('',#3764,.T.);
#2952=FACE_OUTER_BOUND('',#3765,.T.);
#2953=FACE_OUTER_BOUND('',#3766,.T.);
#2954=FACE_OUTER_BOUND('',#3767,.T.);
#2955=FACE_OUTER_BOUND('',#3768,.T.);
#2956=FACE_OUTER_BOUND('',#3769,.T.);
#2957=FACE_OUTER_BOUND('',#3770,.T.);
#2958=FACE_OUTER_BOUND('',#3771,.T.);
#2959=FACE_OUTER_BOUND('',#3772,.T.);
#2960=FACE_OUTER_BOUND('',#3773,.T.);
#2961=FACE_OUTER_BOUND('',#3774,.T.);
#2962=FACE_OUTER_BOUND('',#3775,.T.);
#2963=FACE_OUTER_BOUND('',#3776,.T.);
#2964=FACE_OUTER_BOUND('',#3777,.T.);
#2965=FACE_OUTER_BOUND('',#3778,.T.);
#2966=FACE_OUTER_BOUND('',#3779,.T.);
#2967=FACE_OUTER_BOUND('',#3780,.T.);
#2968=FACE_OUTER_BOUND('',#3781,.T.);
#2969=FACE_OUTER_BOUND('',#3782,.T.);
#2970=FACE_OUTER_BOUND('',#3783,.T.);
#2971=FACE_OUTER_BOUND('',#3785,.T.);
#2972=FACE_OUTER_BOUND('',#3787,.T.);
#2973=FACE_OUTER_BOUND('',#3788,.T.);
#2974=FACE_OUTER_BOUND('',#3789,.T.);
#2975=FACE_OUTER_BOUND('',#3790,.T.);
#2976=FACE_OUTER_BOUND('',#3791,.T.);
#2977=FACE_OUTER_BOUND('',#3792,.T.);
#2978=FACE_OUTER_BOUND('',#3793,.T.);
#2979=FACE_OUTER_BOUND('',#3794,.T.);
#2980=FACE_OUTER_BOUND('',#3795,.T.);
#2981=FACE_OUTER_BOUND('',#3796,.T.);
#2982=FACE_OUTER_BOUND('',#3797,.T.);
#2983=FACE_OUTER_BOUND('',#3798,.T.);
#2984=FACE_OUTER_BOUND('',#3799,.T.);
#2985=FACE_OUTER_BOUND('',#3800,.T.);
#2986=FACE_OUTER_BOUND('',#3801,.T.);
#2987=FACE_OUTER_BOUND('',#3802,.T.);
#2988=FACE_OUTER_BOUND('',#3803,.T.);
#2989=FACE_OUTER_BOUND('',#3804,.T.);
#2990=FACE_OUTER_BOUND('',#3805,.T.);
#2991=FACE_OUTER_BOUND('',#3806,.T.);
#2992=FACE_OUTER_BOUND('',#3807,.T.);
#2993=FACE_OUTER_BOUND('',#3808,.T.);
#2994=FACE_OUTER_BOUND('',#3809,.T.);
#2995=FACE_OUTER_BOUND('',#3810,.T.);
#2996=FACE_OUTER_BOUND('',#3811,.T.);
#2997=FACE_OUTER_BOUND('',#3812,.T.);
#2998=FACE_OUTER_BOUND('',#3813,.T.);
#2999=FACE_OUTER_BOUND('',#3814,.T.);
#3000=FACE_OUTER_BOUND('',#3815,.T.);
#3001=FACE_OUTER_BOUND('',#3817,.T.);
#3002=FACE_OUTER_BOUND('',#3818,.T.);
#3003=FACE_OUTER_BOUND('',#3819,.T.);
#3004=FACE_OUTER_BOUND('',#3820,.T.);
#3005=FACE_OUTER_BOUND('',#3821,.T.);
#3006=FACE_OUTER_BOUND('',#3822,.T.);
#3007=FACE_OUTER_BOUND('',#3823,.T.);
#3008=FACE_OUTER_BOUND('',#3824,.T.);
#3009=FACE_OUTER_BOUND('',#3826,.T.);
#3010=FACE_OUTER_BOUND('',#3827,.T.);
#3011=FACE_OUTER_BOUND('',#3828,.T.);
#3012=FACE_OUTER_BOUND('',#3830,.T.);
#3013=FACE_OUTER_BOUND('',#3832,.T.);
#3014=FACE_OUTER_BOUND('',#3833,.T.);
#3015=FACE_OUTER_BOUND('',#3834,.T.);
#3016=FACE_OUTER_BOUND('',#3835,.T.);
#3017=FACE_OUTER_BOUND('',#3836,.T.);
#3018=FACE_OUTER_BOUND('',#3837,.T.);
#3019=FACE_OUTER_BOUND('',#3838,.T.);
#3020=FACE_OUTER_BOUND('',#3839,.T.);
#3021=FACE_OUTER_BOUND('',#3840,.T.);
#3022=FACE_OUTER_BOUND('',#3841,.T.);
#3023=FACE_OUTER_BOUND('',#3842,.T.);
#3024=FACE_OUTER_BOUND('',#3843,.T.);
#3025=FACE_OUTER_BOUND('',#3844,.T.);
#3026=FACE_OUTER_BOUND('',#3845,.T.);
#3027=FACE_OUTER_BOUND('',#3846,.T.);
#3028=FACE_OUTER_BOUND('',#3847,.T.);
#3029=FACE_OUTER_BOUND('',#3848,.T.);
#3030=FACE_OUTER_BOUND('',#3849,.T.);
#3031=FACE_OUTER_BOUND('',#3850,.T.);
#3032=FACE_OUTER_BOUND('',#3851,.T.);
#3033=FACE_OUTER_BOUND('',#3852,.T.);
#3034=FACE_OUTER_BOUND('',#3853,.T.);
#3035=FACE_OUTER_BOUND('',#3854,.T.);
#3036=FACE_OUTER_BOUND('',#3855,.T.);
#3037=FACE_OUTER_BOUND('',#3856,.T.);
#3038=FACE_OUTER_BOUND('',#3857,.T.);
#3039=FACE_OUTER_BOUND('',#3858,.T.);
#3040=FACE_OUTER_BOUND('',#3859,.T.);
#3041=FACE_OUTER_BOUND('',#3860,.T.);
#3042=FACE_OUTER_BOUND('',#3861,.T.);
#3043=FACE_OUTER_BOUND('',#3862,.T.);
#3044=FACE_OUTER_BOUND('',#3863,.T.);
#3045=FACE_OUTER_BOUND('',#3864,.T.);
#3046=FACE_OUTER_BOUND('',#3865,.T.);
#3047=FACE_OUTER_BOUND('',#3866,.T.);
#3048=FACE_OUTER_BOUND('',#3867,.T.);
#3049=FACE_OUTER_BOUND('',#3868,.T.);
#3050=FACE_OUTER_BOUND('',#3869,.T.);
#3051=FACE_OUTER_BOUND('',#3870,.T.);
#3052=FACE_OUTER_BOUND('',#3871,.T.);
#3053=FACE_OUTER_BOUND('',#3872,.T.);
#3054=FACE_OUTER_BOUND('',#3873,.T.);
#3055=FACE_OUTER_BOUND('',#3874,.T.);
#3056=FACE_OUTER_BOUND('',#3876,.T.);
#3057=FACE_OUTER_BOUND('',#3877,.T.);
#3058=FACE_OUTER_BOUND('',#3879,.T.);
#3059=FACE_OUTER_BOUND('',#3880,.T.);
#3060=FACE_OUTER_BOUND('',#3881,.T.);
#3061=FACE_OUTER_BOUND('',#3882,.T.);
#3062=FACE_OUTER_BOUND('',#3884,.T.);
#3063=EDGE_LOOP('',(#9127,#9128,#9129,#9130));
#3064=EDGE_LOOP('',(#9131,#9132,#9133,#9134));
#3065=EDGE_LOOP('',(#9135,#9136,#9137,#9138));
#3066=EDGE_LOOP('',(#9139,#9140,#9141,#9142));
#3067=EDGE_LOOP('',(#9143,#9144,#9145,#9146));
#3068=EDGE_LOOP('',(#9147,#9148,#9149,#9150));
#3069=EDGE_LOOP('',(#9151,#9152,#9153,#9154));
#3070=EDGE_LOOP('',(#9155,#9156,#9157,#9158));
#3071=EDGE_LOOP('',(#9159,#9160,#9161,#9162));
#3072=EDGE_LOOP('',(#9163,#9164,#9165,#9166));
#3073=EDGE_LOOP('',(#9167,#9168,#9169,#9170));
#3074=EDGE_LOOP('',(#9171,#9172,#9173,#9174));
#3075=EDGE_LOOP('',(#9175,#9176,#9177,#9178));
#3076=EDGE_LOOP('',(#9179,#9180,#9181,#9182));
#3077=EDGE_LOOP('',(#9183,#9184,#9185,#9186));
#3078=EDGE_LOOP('',(#9187,#9188,#9189,#9190));
#3079=EDGE_LOOP('',(#9191,#9192,#9193,#9194));
#3080=EDGE_LOOP('',(#9195,#9196,#9197,#9198));
#3081=EDGE_LOOP('',(#9199,#9200,#9201,#9202));
#3082=EDGE_LOOP('',(#9203,#9204,#9205,#9206));
#3083=EDGE_LOOP('',(#9207,#9208,#9209,#9210));
#3084=EDGE_LOOP('',(#9211,#9212,#9213,#9214));
#3085=EDGE_LOOP('',(#9215,#9216,#9217,#9218));
#3086=EDGE_LOOP('',(#9219,#9220,#9221,#9222));
#3087=EDGE_LOOP('',(#9223,#9224,#9225,#9226));
#3088=EDGE_LOOP('',(#9227,#9228,#9229,#9230));
#3089=EDGE_LOOP('',(#9231,#9232,#9233,#9234));
#3090=EDGE_LOOP('',(#9235,#9236,#9237,#9238));
#3091=EDGE_LOOP('',(#9239,#9240,#9241,#9242));
#3092=EDGE_LOOP('',(#9243,#9244,#9245,#9246));
#3093=EDGE_LOOP('',(#9247,#9248,#9249,#9250));
#3094=EDGE_LOOP('',(#9251,#9252,#9253,#9254));
#3095=EDGE_LOOP('',(#9255,#9256,#9257,#9258));
#3096=EDGE_LOOP('',(#9259,#9260,#9261,#9262));
#3097=EDGE_LOOP('',(#9263,#9264,#9265,#9266));
#3098=EDGE_LOOP('',(#9267,#9268,#9269,#9270));
#3099=EDGE_LOOP('',(#9271,#9272,#9273,#9274));
#3100=EDGE_LOOP('',(#9275,#9276,#9277,#9278));
#3101=EDGE_LOOP('',(#9279,#9280,#9281,#9282));
#3102=EDGE_LOOP('',(#9283,#9284,#9285,#9286));
#3103=EDGE_LOOP('',(#9287,#9288,#9289,#9290));
#3104=EDGE_LOOP('',(#9291,#9292,#9293,#9294));
#3105=EDGE_LOOP('',(#9295,#9296,#9297,#9298));
#3106=EDGE_LOOP('',(#9299,#9300,#9301,#9302));
#3107=EDGE_LOOP('',(#9303,#9304,#9305,#9306));
#3108=EDGE_LOOP('',(#9307,#9308,#9309,#9310));
#3109=EDGE_LOOP('',(#9311,#9312,#9313,#9314));
#3110=EDGE_LOOP('',(#9315,#9316,#9317,#9318));
#3111=EDGE_LOOP('',(#9319,#9320,#9321,#9322));
#3112=EDGE_LOOP('',(#9323,#9324,#9325,#9326));
#3113=EDGE_LOOP('',(#9327,#9328,#9329,#9330));
#3114=EDGE_LOOP('',(#9331,#9332,#9333,#9334));
#3115=EDGE_LOOP('',(#9335,#9336,#9337,#9338));
#3116=EDGE_LOOP('',(#9339,#9340,#9341,#9342));
#3117=EDGE_LOOP('',(#9343,#9344,#9345,#9346));
#3118=EDGE_LOOP('',(#9347,#9348,#9349,#9350));
#3119=EDGE_LOOP('',(#9351,#9352,#9353,#9354));
#3120=EDGE_LOOP('',(#9355,#9356,#9357,#9358));
#3121=EDGE_LOOP('',(#9359,#9360,#9361,#9362));
#3122=EDGE_LOOP('',(#9363,#9364,#9365,#9366));
#3123=EDGE_LOOP('',(#9367,#9368,#9369,#9370));
#3124=EDGE_LOOP('',(#9371,#9372,#9373,#9374));
#3125=EDGE_LOOP('',(#9375,#9376,#9377,#9378));
#3126=EDGE_LOOP('',(#9379,#9380,#9381,#9382));
#3127=EDGE_LOOP('',(#9383,#9384,#9385,#9386));
#3128=EDGE_LOOP('',(#9387,#9388,#9389,#9390));
#3129=EDGE_LOOP('',(#9391,#9392,#9393,#9394));
#3130=EDGE_LOOP('',(#9395,#9396,#9397,#9398));
#3131=EDGE_LOOP('',(#9399,#9400,#9401,#9402));
#3132=EDGE_LOOP('',(#9403,#9404,#9405,#9406));
#3133=EDGE_LOOP('',(#9407,#9408,#9409,#9410));
#3134=EDGE_LOOP('',(#9411,#9412,#9413,#9414));
#3135=EDGE_LOOP('',(#9415,#9416,#9417,#9418));
#3136=EDGE_LOOP('',(#9419,#9420,#9421,#9422));
#3137=EDGE_LOOP('',(#9423,#9424,#9425,#9426));
#3138=EDGE_LOOP('',(#9427,#9428,#9429,#9430));
#3139=EDGE_LOOP('',(#9431,#9432,#9433,#9434));
#3140=EDGE_LOOP('',(#9435,#9436,#9437,#9438));
#3141=EDGE_LOOP('',(#9439,#9440,#9441,#9442));
#3142=EDGE_LOOP('',(#9443,#9444,#9445,#9446));
#3143=EDGE_LOOP('',(#9447,#9448,#9449,#9450));
#3144=EDGE_LOOP('',(#9451,#9452,#9453,#9454));
#3145=EDGE_LOOP('',(#9455,#9456,#9457,#9458));
#3146=EDGE_LOOP('',(#9459,#9460,#9461,#9462));
#3147=EDGE_LOOP('',(#9463,#9464,#9465,#9466));
#3148=EDGE_LOOP('',(#9467,#9468,#9469,#9470));
#3149=EDGE_LOOP('',(#9471,#9472,#9473,#9474));
#3150=EDGE_LOOP('',(#9475,#9476,#9477,#9478));
#3151=EDGE_LOOP('',(#9479,#9480,#9481,#9482));
#3152=EDGE_LOOP('',(#9483,#9484,#9485,#9486,#9487,#9488,#9489,#9490,#9491,
#9492,#9493,#9494,#9495,#9496,#9497,#9498,#9499,#9500,#9501,#9502));
#3153=EDGE_LOOP('',(#9503,#9504,#9505,#9506,#9507,#9508,#9509,#9510,#9511,
#9512,#9513,#9514,#9515,#9516,#9517,#9518,#9519,#9520,#9521,#9522));
#3154=EDGE_LOOP('',(#9523,#9524,#9525,#9526));
#3155=EDGE_LOOP('',(#9527,#9528,#9529,#9530));
#3156=EDGE_LOOP('',(#9531,#9532,#9533,#9534));
#3157=EDGE_LOOP('',(#9535,#9536,#9537,#9538));
#3158=EDGE_LOOP('',(#9539,#9540,#9541,#9542));
#3159=EDGE_LOOP('',(#9543,#9544,#9545,#9546));
#3160=EDGE_LOOP('',(#9547,#9548,#9549,#9550,#9551,#9552,#9553,#9554,#9555,
#9556,#9557,#9558,#9559,#9560,#9561,#9562,#9563,#9564,#9565,#9566));
#3161=EDGE_LOOP('',(#9567,#9568,#9569,#9570,#9571,#9572,#9573,#9574,#9575,
#9576,#9577,#9578,#9579,#9580,#9581,#9582,#9583,#9584,#9585,#9586));
#3162=EDGE_LOOP('',(#9587,#9588,#9589,#9590));
#3163=EDGE_LOOP('',(#9591,#9592,#9593,#9594,#9595,#9596,#9597,#9598,#9599,
#9600,#9601,#9602,#9603,#9604,#9605,#9606,#9607,#9608,#9609,#9610));
#3164=EDGE_LOOP('',(#9611,#9612,#9613,#9614,#9615,#9616,#9617,#9618,#9619,
#9620,#9621,#9622,#9623,#9624,#9625,#9626,#9627,#9628,#9629,#9630));
#3165=EDGE_LOOP('',(#9631,#9632,#9633,#9634));
#3166=EDGE_LOOP('',(#9635,#9636,#9637,#9638,#9639,#9640,#9641,#9642,#9643,
#9644,#9645,#9646,#9647,#9648,#9649,#9650,#9651,#9652,#9653,#9654));
#3167=EDGE_LOOP('',(#9655,#9656,#9657,#9658,#9659,#9660,#9661,#9662,#9663,
#9664,#9665,#9666,#9667,#9668,#9669,#9670,#9671,#9672,#9673,#9674));
#3168=EDGE_LOOP('',(#9675,#9676,#9677,#9678));
#3169=EDGE_LOOP('',(#9679,#9680,#9681,#9682));
#3170=EDGE_LOOP('',(#9683,#9684,#9685,#9686));
#3171=EDGE_LOOP('',(#9687,#9688,#9689,#9690));
#3172=EDGE_LOOP('',(#9691,#9692,#9693,#9694));
#3173=EDGE_LOOP('',(#9695,#9696,#9697,#9698));
#3174=EDGE_LOOP('',(#9699,#9700,#9701,#9702));
#3175=EDGE_LOOP('',(#9703,#9704,#9705,#9706));
#3176=EDGE_LOOP('',(#9707,#9708,#9709,#9710));
#3177=EDGE_LOOP('',(#9711,#9712,#9713,#9714));
#3178=EDGE_LOOP('',(#9715,#9716,#9717,#9718));
#3179=EDGE_LOOP('',(#9719,#9720,#9721,#9722));
#3180=EDGE_LOOP('',(#9723,#9724,#9725,#9726));
#3181=EDGE_LOOP('',(#9727,#9728,#9729,#9730));
#3182=EDGE_LOOP('',(#9731,#9732,#9733,#9734));
#3183=EDGE_LOOP('',(#9735,#9736,#9737,#9738));
#3184=EDGE_LOOP('',(#9739,#9740,#9741,#9742));
#3185=EDGE_LOOP('',(#9743,#9744,#9745,#9746));
#3186=EDGE_LOOP('',(#9747,#9748,#9749,#9750));
#3187=EDGE_LOOP('',(#9751,#9752,#9753,#9754));
#3188=EDGE_LOOP('',(#9755,#9756,#9757,#9758));
#3189=EDGE_LOOP('',(#9759,#9760,#9761,#9762));
#3190=EDGE_LOOP('',(#9763,#9764,#9765,#9766));
#3191=EDGE_LOOP('',(#9767,#9768,#9769,#9770));
#3192=EDGE_LOOP('',(#9771,#9772,#9773,#9774));
#3193=EDGE_LOOP('',(#9775,#9776,#9777,#9778));
#3194=EDGE_LOOP('',(#9779,#9780,#9781,#9782));
#3195=EDGE_LOOP('',(#9783,#9784,#9785,#9786));
#3196=EDGE_LOOP('',(#9787,#9788,#9789,#9790));
#3197=EDGE_LOOP('',(#9791,#9792,#9793,#9794));
#3198=EDGE_LOOP('',(#9795,#9796,#9797,#9798));
#3199=EDGE_LOOP('',(#9799,#9800,#9801,#9802));
#3200=EDGE_LOOP('',(#9803,#9804,#9805,#9806));
#3201=EDGE_LOOP('',(#9807,#9808,#9809,#9810));
#3202=EDGE_LOOP('',(#9811,#9812,#9813,#9814));
#3203=EDGE_LOOP('',(#9815,#9816,#9817,#9818));
#3204=EDGE_LOOP('',(#9819,#9820,#9821,#9822));
#3205=EDGE_LOOP('',(#9823,#9824,#9825,#9826));
#3206=EDGE_LOOP('',(#9827,#9828,#9829,#9830));
#3207=EDGE_LOOP('',(#9831,#9832,#9833,#9834));
#3208=EDGE_LOOP('',(#9835,#9836,#9837,#9838));
#3209=EDGE_LOOP('',(#9839,#9840,#9841,#9842));
#3210=EDGE_LOOP('',(#9843,#9844,#9845,#9846));
#3211=EDGE_LOOP('',(#9847,#9848,#9849,#9850));
#3212=EDGE_LOOP('',(#9851,#9852,#9853,#9854));
#3213=EDGE_LOOP('',(#9855,#9856,#9857,#9858));
#3214=EDGE_LOOP('',(#9859,#9860,#9861,#9862));
#3215=EDGE_LOOP('',(#9863,#9864,#9865,#9866));
#3216=EDGE_LOOP('',(#9867,#9868,#9869,#9870));
#3217=EDGE_LOOP('',(#9871,#9872,#9873,#9874));
#3218=EDGE_LOOP('',(#9875,#9876,#9877,#9878));
#3219=EDGE_LOOP('',(#9879,#9880,#9881,#9882));
#3220=EDGE_LOOP('',(#9883,#9884,#9885,#9886));
#3221=EDGE_LOOP('',(#9887,#9888,#9889,#9890));
#3222=EDGE_LOOP('',(#9891,#9892,#9893,#9894));
#3223=EDGE_LOOP('',(#9895,#9896,#9897,#9898));
#3224=EDGE_LOOP('',(#9899,#9900,#9901,#9902));
#3225=EDGE_LOOP('',(#9903,#9904,#9905,#9906));
#3226=EDGE_LOOP('',(#9907,#9908,#9909,#9910));
#3227=EDGE_LOOP('',(#9911,#9912,#9913,#9914));
#3228=EDGE_LOOP('',(#9915,#9916,#9917,#9918));
#3229=EDGE_LOOP('',(#9919,#9920,#9921,#9922,#9923,#9924,#9925,#9926));
#3230=EDGE_LOOP('',(#9927,#9928,#9929,#9930,#9931,#9932,#9933,#9934,#9935,
#9936,#9937,#9938,#9939,#9940,#9941,#9942,#9943,#9944,#9945,#9946,#9947,
#9948,#9949,#9950,#9951,#9952,#9953,#9954,#9955,#9956,#9957,#9958,#9959,
#9960,#9961,#9962,#9963,#9964,#9965,#9966,#9967,#9968,#9969,#9970,#9971,
#9972,#9973,#9974,#9975,#9976,#9977,#9978));
#3231=EDGE_LOOP('',(#9979,#9980,#9981,#9982));
#3232=EDGE_LOOP('',(#9983,#9984,#9985,#9986,#9987,#9988,#9989,#9990,#9991,
#9992,#9993,#9994,#9995,#9996,#9997,#9998,#9999,#10000,#10001,#10002,#10003,
#10004,#10005,#10006,#10007,#10008,#10009,#10010,#10011,#10012,#10013,#10014,
#10015,#10016,#10017,#10018,#10019,#10020,#10021,#10022,#10023,#10024,#10025,
#10026,#10027,#10028,#10029,#10030,#10031,#10032,#10033,#10034,#10035));
#3233=EDGE_LOOP('',(#10036,#10037,#10038,#10039));
#3234=EDGE_LOOP('',(#10040,#10041,#10042,#10043));
#3235=EDGE_LOOP('',(#10044,#10045,#10046,#10047));
#3236=EDGE_LOOP('',(#10048,#10049,#10050,#10051));
#3237=EDGE_LOOP('',(#10052,#10053,#10054,#10055));
#3238=EDGE_LOOP('',(#10056,#10057,#10058,#10059));
#3239=EDGE_LOOP('',(#10060,#10061,#10062,#10063));
#3240=EDGE_LOOP('',(#10064,#10065,#10066,#10067,#10068,#10069));
#3241=EDGE_LOOP('',(#10070));
#3242=EDGE_LOOP('',(#10071,#10072,#10073,#10074));
#3243=EDGE_LOOP('',(#10075,#10076,#10077,#10078));
#3244=EDGE_LOOP('',(#10079));
#3245=EDGE_LOOP('',(#10080,#10081,#10082,#10083,#10084,#10085));
#3246=EDGE_LOOP('',(#10086));
#3247=EDGE_LOOP('',(#10087,#10088,#10089,#10090));
#3248=EDGE_LOOP('',(#10091,#10092,#10093,#10094));
#3249=EDGE_LOOP('',(#10095));
#3250=EDGE_LOOP('',(#10096));
#3251=EDGE_LOOP('',(#10097));
#3252=EDGE_LOOP('',(#10098));
#3253=EDGE_LOOP('',(#10099,#10100,#10101,#10102,#10103,#10104,#10105,#10106));
#3254=EDGE_LOOP('',(#10107,#10108,#10109,#10110));
#3255=EDGE_LOOP('',(#10111,#10112,#10113,#10114));
#3256=EDGE_LOOP('',(#10115,#10116,#10117,#10118));
#3257=EDGE_LOOP('',(#10119,#10120,#10121,#10122));
#3258=EDGE_LOOP('',(#10123,#10124,#10125,#10126));
#3259=EDGE_LOOP('',(#10127,#10128,#10129,#10130));
#3260=EDGE_LOOP('',(#10131,#10132,#10133,#10134));
#3261=EDGE_LOOP('',(#10135,#10136,#10137,#10138));
#3262=EDGE_LOOP('',(#10139,#10140,#10141,#10142));
#3263=EDGE_LOOP('',(#10143,#10144,#10145,#10146));
#3264=EDGE_LOOP('',(#10147,#10148,#10149,#10150));
#3265=EDGE_LOOP('',(#10151,#10152,#10153,#10154));
#3266=EDGE_LOOP('',(#10155,#10156,#10157,#10158));
#3267=EDGE_LOOP('',(#10159,#10160,#10161,#10162));
#3268=EDGE_LOOP('',(#10163,#10164,#10165,#10166));
#3269=EDGE_LOOP('',(#10167,#10168,#10169,#10170));
#3270=EDGE_LOOP('',(#10171,#10172,#10173,#10174));
#3271=EDGE_LOOP('',(#10175,#10176,#10177,#10178));
#3272=EDGE_LOOP('',(#10179,#10180,#10181,#10182));
#3273=EDGE_LOOP('',(#10183,#10184,#10185,#10186));
#3274=EDGE_LOOP('',(#10187,#10188,#10189,#10190));
#3275=EDGE_LOOP('',(#10191,#10192,#10193,#10194));
#3276=EDGE_LOOP('',(#10195,#10196,#10197,#10198));
#3277=EDGE_LOOP('',(#10199,#10200,#10201,#10202));
#3278=EDGE_LOOP('',(#10203,#10204,#10205,#10206));
#3279=EDGE_LOOP('',(#10207,#10208,#10209,#10210));
#3280=EDGE_LOOP('',(#10211,#10212,#10213,#10214));
#3281=EDGE_LOOP('',(#10215,#10216,#10217,#10218));
#3282=EDGE_LOOP('',(#10219,#10220,#10221,#10222));
#3283=EDGE_LOOP('',(#10223,#10224,#10225,#10226));
#3284=EDGE_LOOP('',(#10227,#10228,#10229,#10230));
#3285=EDGE_LOOP('',(#10231,#10232,#10233,#10234));
#3286=EDGE_LOOP('',(#10235,#10236,#10237,#10238));
#3287=EDGE_LOOP('',(#10239,#10240,#10241,#10242));
#3288=EDGE_LOOP('',(#10243,#10244,#10245,#10246));
#3289=EDGE_LOOP('',(#10247,#10248,#10249,#10250));
#3290=EDGE_LOOP('',(#10251,#10252,#10253,#10254));
#3291=EDGE_LOOP('',(#10255,#10256,#10257,#10258));
#3292=EDGE_LOOP('',(#10259,#10260,#10261,#10262));
#3293=EDGE_LOOP('',(#10263,#10264,#10265,#10266));
#3294=EDGE_LOOP('',(#10267,#10268,#10269,#10270));
#3295=EDGE_LOOP('',(#10271,#10272,#10273,#10274));
#3296=EDGE_LOOP('',(#10275,#10276,#10277,#10278));
#3297=EDGE_LOOP('',(#10279,#10280,#10281,#10282));
#3298=EDGE_LOOP('',(#10283,#10284,#10285,#10286));
#3299=EDGE_LOOP('',(#10287,#10288,#10289,#10290));
#3300=EDGE_LOOP('',(#10291,#10292,#10293,#10294));
#3301=EDGE_LOOP('',(#10295,#10296,#10297,#10298));
#3302=EDGE_LOOP('',(#10299,#10300,#10301,#10302));
#3303=EDGE_LOOP('',(#10303,#10304,#10305,#10306,#10307,#10308,#10309,#10310));
#3304=EDGE_LOOP('',(#10311,#10312,#10313,#10314));
#3305=EDGE_LOOP('',(#10315,#10316,#10317,#10318));
#3306=EDGE_LOOP('',(#10319,#10320,#10321,#10322));
#3307=EDGE_LOOP('',(#10323,#10324,#10325,#10326));
#3308=EDGE_LOOP('',(#10327,#10328,#10329,#10330));
#3309=EDGE_LOOP('',(#10331,#10332,#10333,#10334));
#3310=EDGE_LOOP('',(#10335,#10336,#10337,#10338));
#3311=EDGE_LOOP('',(#10339,#10340,#10341,#10342));
#3312=EDGE_LOOP('',(#10343,#10344,#10345,#10346));
#3313=EDGE_LOOP('',(#10347,#10348,#10349,#10350));
#3314=EDGE_LOOP('',(#10351,#10352,#10353,#10354));
#3315=EDGE_LOOP('',(#10355,#10356,#10357,#10358));
#3316=EDGE_LOOP('',(#10359,#10360,#10361,#10362));
#3317=EDGE_LOOP('',(#10363,#10364,#10365,#10366));
#3318=EDGE_LOOP('',(#10367,#10368,#10369,#10370));
#3319=EDGE_LOOP('',(#10371,#10372,#10373,#10374));
#3320=EDGE_LOOP('',(#10375,#10376,#10377,#10378));
#3321=EDGE_LOOP('',(#10379,#10380,#10381,#10382));
#3322=EDGE_LOOP('',(#10383,#10384,#10385,#10386));
#3323=EDGE_LOOP('',(#10387,#10388,#10389,#10390));
#3324=EDGE_LOOP('',(#10391,#10392,#10393,#10394));
#3325=EDGE_LOOP('',(#10395,#10396,#10397,#10398));
#3326=EDGE_LOOP('',(#10399,#10400,#10401,#10402));
#3327=EDGE_LOOP('',(#10403,#10404,#10405,#10406));
#3328=EDGE_LOOP('',(#10407,#10408,#10409,#10410));
#3329=EDGE_LOOP('',(#10411,#10412,#10413,#10414));
#3330=EDGE_LOOP('',(#10415,#10416,#10417,#10418));
#3331=EDGE_LOOP('',(#10419,#10420,#10421,#10422));
#3332=EDGE_LOOP('',(#10423,#10424,#10425,#10426));
#3333=EDGE_LOOP('',(#10427,#10428,#10429,#10430));
#3334=EDGE_LOOP('',(#10431,#10432,#10433,#10434));
#3335=EDGE_LOOP('',(#10435,#10436,#10437,#10438));
#3336=EDGE_LOOP('',(#10439,#10440,#10441,#10442));
#3337=EDGE_LOOP('',(#10443,#10444,#10445,#10446));
#3338=EDGE_LOOP('',(#10447,#10448,#10449,#10450));
#3339=EDGE_LOOP('',(#10451,#10452,#10453,#10454));
#3340=EDGE_LOOP('',(#10455,#10456,#10457,#10458));
#3341=EDGE_LOOP('',(#10459,#10460,#10461,#10462));
#3342=EDGE_LOOP('',(#10463,#10464,#10465,#10466));
#3343=EDGE_LOOP('',(#10467,#10468,#10469,#10470));
#3344=EDGE_LOOP('',(#10471,#10472,#10473,#10474));
#3345=EDGE_LOOP('',(#10475,#10476,#10477,#10478));
#3346=EDGE_LOOP('',(#10479,#10480,#10481,#10482));
#3347=EDGE_LOOP('',(#10483,#10484,#10485,#10486));
#3348=EDGE_LOOP('',(#10487,#10488,#10489,#10490));
#3349=EDGE_LOOP('',(#10491,#10492,#10493,#10494));
#3350=EDGE_LOOP('',(#10495,#10496,#10497,#10498));
#3351=EDGE_LOOP('',(#10499,#10500,#10501,#10502));
#3352=EDGE_LOOP('',(#10503,#10504,#10505,#10506));
#3353=EDGE_LOOP('',(#10507,#10508,#10509,#10510));
#3354=EDGE_LOOP('',(#10511,#10512,#10513,#10514));
#3355=EDGE_LOOP('',(#10515,#10516,#10517,#10518));
#3356=EDGE_LOOP('',(#10519,#10520,#10521,#10522));
#3357=EDGE_LOOP('',(#10523,#10524,#10525,#10526));
#3358=EDGE_LOOP('',(#10527,#10528,#10529,#10530));
#3359=EDGE_LOOP('',(#10531,#10532,#10533,#10534));
#3360=EDGE_LOOP('',(#10535,#10536,#10537,#10538));
#3361=EDGE_LOOP('',(#10539,#10540,#10541,#10542));
#3362=EDGE_LOOP('',(#10543,#10544,#10545,#10546));
#3363=EDGE_LOOP('',(#10547,#10548,#10549,#10550));
#3364=EDGE_LOOP('',(#10551,#10552,#10553,#10554));
#3365=EDGE_LOOP('',(#10555,#10556,#10557,#10558));
#3366=EDGE_LOOP('',(#10559,#10560,#10561,#10562));
#3367=EDGE_LOOP('',(#10563,#10564,#10565,#10566));
#3368=EDGE_LOOP('',(#10567,#10568,#10569,#10570));
#3369=EDGE_LOOP('',(#10571,#10572,#10573,#10574));
#3370=EDGE_LOOP('',(#10575,#10576,#10577,#10578));
#3371=EDGE_LOOP('',(#10579,#10580,#10581,#10582));
#3372=EDGE_LOOP('',(#10583,#10584,#10585,#10586));
#3373=EDGE_LOOP('',(#10587,#10588,#10589,#10590));
#3374=EDGE_LOOP('',(#10591,#10592,#10593,#10594));
#3375=EDGE_LOOP('',(#10595,#10596,#10597,#10598));
#3376=EDGE_LOOP('',(#10599,#10600,#10601,#10602));
#3377=EDGE_LOOP('',(#10603,#10604,#10605,#10606));
#3378=EDGE_LOOP('',(#10607,#10608,#10609,#10610));
#3379=EDGE_LOOP('',(#10611,#10612,#10613,#10614));
#3380=EDGE_LOOP('',(#10615,#10616,#10617,#10618));
#3381=EDGE_LOOP('',(#10619,#10620,#10621,#10622));
#3382=EDGE_LOOP('',(#10623,#10624,#10625,#10626));
#3383=EDGE_LOOP('',(#10627,#10628,#10629,#10630,#10631));
#3384=EDGE_LOOP('',(#10632,#10633,#10634,#10635));
#3385=EDGE_LOOP('',(#10636,#10637,#10638,#10639,#10640,#10641,#10642,#10643,
#10644,#10645,#10646,#10647,#10648,#10649,#10650,#10651,#10652,#10653,#10654,
#10655,#10656,#10657,#10658,#10659,#10660,#10661,#10662,#10663,#10664,#10665,
#10666,#10667,#10668,#10669,#10670,#10671,#10672,#10673,#10674,#10675,#10676,
#10677,#10678,#10679,#10680,#10681,#10682,#10683,#10684,#10685,#10686,#10687,
#10688,#10689,#10690,#10691,#10692,#10693,#10694,#10695,#10696,#10697,#10698,
#10699,#10700,#10701,#10702,#10703,#10704,#10705,#10706,#10707,#10708,#10709,
#10710,#10711,#10712,#10713,#10714,#10715,#10716,#10717,#10718,#10719));
#3386=EDGE_LOOP('',(#10720,#10721,#10722,#10723,#10724,#10725,#10726,#10727,
#10728,#10729,#10730,#10731,#10732,#10733,#10734,#10735,#10736,#10737,#10738,
#10739,#10740,#10741,#10742,#10743,#10744,#10745,#10746,#10747,#10748,#10749,
#10750,#10751,#10752,#10753,#10754,#10755,#10756,#10757,#10758,#10759,#10760,
#10761,#10762,#10763,#10764,#10765,#10766,#10767,#10768,#10769,#10770,#10771,
#10772,#10773,#10774,#10775,#10776,#10777,#10778,#10779,#10780,#10781,#10782,
#10783,#10784,#10785,#10786,#10787,#10788,#10789,#10790,#10791,#10792,#10793,
#10794,#10795,#10796,#10797,#10798,#10799,#10800,#10801,#10802,#10803));
#3387=EDGE_LOOP('',(#10804,#10805,#10806,#10807));
#3388=EDGE_LOOP('',(#10808));
#3389=EDGE_LOOP('',(#10809));
#3390=EDGE_LOOP('',(#10810,#10811,#10812,#10813,#10814));
#3391=EDGE_LOOP('',(#10815,#10816,#10817,#10818));
#3392=EDGE_LOOP('',(#10819,#10820,#10821,#10822,#10823,#10824,#10825,#10826,
#10827,#10828,#10829,#10830,#10831,#10832,#10833,#10834,#10835,#10836,#10837,
#10838,#10839,#10840,#10841,#10842,#10843,#10844,#10845,#10846,#10847,#10848,
#10849,#10850,#10851,#10852,#10853,#10854,#10855,#10856,#10857,#10858,#10859,
#10860,#10861,#10862,#10863,#10864,#10865,#10866,#10867,#10868,#10869,#10870,
#10871,#10872));
#3393=EDGE_LOOP('',(#10873,#10874,#10875,#10876,#10877,#10878,#10879,#10880,
#10881,#10882,#10883,#10884,#10885,#10886,#10887,#10888,#10889,#10890,#10891,
#10892,#10893,#10894,#10895,#10896,#10897,#10898,#10899,#10900,#10901,#10902,
#10903,#10904,#10905,#10906,#10907,#10908,#10909,#10910,#10911,#10912,#10913,
#10914,#10915,#10916,#10917,#10918,#10919,#10920,#10921,#10922,#10923,#10924,
#10925,#10926));
#3394=EDGE_LOOP('',(#10927,#10928,#10929,#10930));
#3395=EDGE_LOOP('',(#10931));
#3396=EDGE_LOOP('',(#10932));
#3397=EDGE_LOOP('',(#10933,#10934,#10935,#10936));
#3398=EDGE_LOOP('',(#10937,#10938,#10939,#10940));
#3399=EDGE_LOOP('',(#10941,#10942,#10943,#10944,#10945,#10946,#10947,#10948,
#10949,#10950,#10951,#10952,#10953,#10954,#10955,#10956,#10957,#10958,#10959,
#10960,#10961,#10962,#10963,#10964,#10965,#10966,#10967,#10968,#10969,#10970,
#10971,#10972,#10973,#10974,#10975,#10976,#10977,#10978,#10979,#10980,#10981,
#10982,#10983,#10984,#10985,#10986,#10987,#10988,#10989,#10990,#10991,#10992,
#10993,#10994,#10995,#10996,#10997,#10998,#10999,#11000,#11001,#11002,#11003,
#11004,#11005,#11006,#11007,#11008,#11009,#11010,#11011,#11012));
#3400=EDGE_LOOP('',(#11013,#11014,#11015,#11016));
#3401=EDGE_LOOP('',(#11017));
#3402=EDGE_LOOP('',(#11018));
#3403=EDGE_LOOP('',(#11019));
#3404=EDGE_LOOP('',(#11020));
#3405=EDGE_LOOP('',(#11021,#11022,#11023,#11024));
#3406=EDGE_LOOP('',(#11025,#11026,#11027,#11028));
#3407=EDGE_LOOP('',(#11029,#11030,#11031,#11032));
#3408=EDGE_LOOP('',(#11033,#11034,#11035,#11036));
#3409=EDGE_LOOP('',(#11037,#11038,#11039,#11040));
#3410=EDGE_LOOP('',(#11041,#11042,#11043,#11044));
#3411=EDGE_LOOP('',(#11045,#11046,#11047,#11048));
#3412=EDGE_LOOP('',(#11049,#11050,#11051,#11052));
#3413=EDGE_LOOP('',(#11053,#11054,#11055,#11056));
#3414=EDGE_LOOP('',(#11057,#11058,#11059,#11060));
#3415=EDGE_LOOP('',(#11061,#11062,#11063,#11064));
#3416=EDGE_LOOP('',(#11065,#11066,#11067,#11068));
#3417=EDGE_LOOP('',(#11069,#11070,#11071,#11072));
#3418=EDGE_LOOP('',(#11073,#11074,#11075,#11076));
#3419=EDGE_LOOP('',(#11077,#11078,#11079,#11080));
#3420=EDGE_LOOP('',(#11081,#11082,#11083,#11084));
#3421=EDGE_LOOP('',(#11085,#11086,#11087,#11088));
#3422=EDGE_LOOP('',(#11089,#11090,#11091,#11092));
#3423=EDGE_LOOP('',(#11093,#11094,#11095,#11096));
#3424=EDGE_LOOP('',(#11097,#11098,#11099,#11100));
#3425=EDGE_LOOP('',(#11101,#11102,#11103,#11104));
#3426=EDGE_LOOP('',(#11105,#11106,#11107,#11108));
#3427=EDGE_LOOP('',(#11109,#11110,#11111,#11112));
#3428=EDGE_LOOP('',(#11113,#11114,#11115,#11116));
#3429=EDGE_LOOP('',(#11117,#11118,#11119,#11120));
#3430=EDGE_LOOP('',(#11121,#11122,#11123,#11124));
#3431=EDGE_LOOP('',(#11125,#11126,#11127,#11128));
#3432=EDGE_LOOP('',(#11129,#11130,#11131,#11132));
#3433=EDGE_LOOP('',(#11133,#11134,#11135,#11136));
#3434=EDGE_LOOP('',(#11137,#11138,#11139,#11140));
#3435=EDGE_LOOP('',(#11141,#11142,#11143,#11144));
#3436=EDGE_LOOP('',(#11145,#11146,#11147,#11148));
#3437=EDGE_LOOP('',(#11149,#11150,#11151,#11152));
#3438=EDGE_LOOP('',(#11153,#11154,#11155,#11156));
#3439=EDGE_LOOP('',(#11157,#11158,#11159,#11160));
#3440=EDGE_LOOP('',(#11161,#11162,#11163,#11164));
#3441=EDGE_LOOP('',(#11165,#11166,#11167,#11168));
#3442=EDGE_LOOP('',(#11169,#11170,#11171,#11172));
#3443=EDGE_LOOP('',(#11173,#11174,#11175,#11176));
#3444=EDGE_LOOP('',(#11177,#11178,#11179,#11180));
#3445=EDGE_LOOP('',(#11181,#11182,#11183,#11184));
#3446=EDGE_LOOP('',(#11185,#11186,#11187,#11188));
#3447=EDGE_LOOP('',(#11189,#11190,#11191,#11192));
#3448=EDGE_LOOP('',(#11193,#11194,#11195,#11196));
#3449=EDGE_LOOP('',(#11197,#11198,#11199,#11200));
#3450=EDGE_LOOP('',(#11201,#11202,#11203,#11204));
#3451=EDGE_LOOP('',(#11205,#11206,#11207,#11208));
#3452=EDGE_LOOP('',(#11209,#11210,#11211,#11212));
#3453=EDGE_LOOP('',(#11213,#11214,#11215,#11216));
#3454=EDGE_LOOP('',(#11217,#11218,#11219,#11220));
#3455=EDGE_LOOP('',(#11221,#11222,#11223,#11224));
#3456=EDGE_LOOP('',(#11225,#11226,#11227,#11228));
#3457=EDGE_LOOP('',(#11229,#11230,#11231,#11232));
#3458=EDGE_LOOP('',(#11233,#11234,#11235,#11236));
#3459=EDGE_LOOP('',(#11237,#11238,#11239,#11240));
#3460=EDGE_LOOP('',(#11241,#11242,#11243,#11244));
#3461=EDGE_LOOP('',(#11245,#11246,#11247,#11248));
#3462=EDGE_LOOP('',(#11249,#11250,#11251,#11252));
#3463=EDGE_LOOP('',(#11253,#11254,#11255,#11256));
#3464=EDGE_LOOP('',(#11257,#11258,#11259,#11260));
#3465=EDGE_LOOP('',(#11261,#11262,#11263,#11264));
#3466=EDGE_LOOP('',(#11265,#11266,#11267,#11268));
#3467=EDGE_LOOP('',(#11269,#11270,#11271,#11272));
#3468=EDGE_LOOP('',(#11273,#11274,#11275,#11276));
#3469=EDGE_LOOP('',(#11277,#11278,#11279,#11280));
#3470=EDGE_LOOP('',(#11281,#11282,#11283,#11284));
#3471=EDGE_LOOP('',(#11285,#11286,#11287,#11288));
#3472=EDGE_LOOP('',(#11289,#11290,#11291,#11292));
#3473=EDGE_LOOP('',(#11293,#11294,#11295,#11296));
#3474=EDGE_LOOP('',(#11297,#11298,#11299,#11300));
#3475=EDGE_LOOP('',(#11301,#11302,#11303,#11304));
#3476=EDGE_LOOP('',(#11305,#11306,#11307,#11308));
#3477=EDGE_LOOP('',(#11309,#11310,#11311,#11312));
#3478=EDGE_LOOP('',(#11313,#11314,#11315,#11316));
#3479=EDGE_LOOP('',(#11317,#11318,#11319,#11320));
#3480=EDGE_LOOP('',(#11321,#11322,#11323,#11324,#11325,#11326,#11327,#11328,
#11329,#11330,#11331,#11332,#11333,#11334,#11335,#11336,#11337,#11338,#11339,
#11340,#11341,#11342,#11343,#11344,#11345,#11346,#11347,#11348,#11349,#11350,
#11351,#11352,#11353,#11354,#11355,#11356,#11357,#11358,#11359,#11360,#11361,
#11362,#11363,#11364,#11365,#11366,#11367,#11368,#11369,#11370,#11371,#11372,
#11373,#11374,#11375,#11376,#11377,#11378,#11379,#11380,#11381,#11382,#11383,
#11384,#11385,#11386,#11387,#11388,#11389,#11390,#11391,#11392));
#3481=EDGE_LOOP('',(#11393,#11394,#11395,#11396));
#3482=EDGE_LOOP('',(#11397));
#3483=EDGE_LOOP('',(#11398));
#3484=EDGE_LOOP('',(#11399));
#3485=EDGE_LOOP('',(#11400));
#3486=EDGE_LOOP('',(#11401));
#3487=EDGE_LOOP('',(#11402));
#3488=EDGE_LOOP('',(#11403,#11404,#11405,#11406));
#3489=EDGE_LOOP('',(#11407,#11408,#11409,#11410));
#3490=EDGE_LOOP('',(#11411,#11412,#11413,#11414));
#3491=EDGE_LOOP('',(#11415,#11416,#11417,#11418));
#3492=EDGE_LOOP('',(#11419,#11420,#11421,#11422));
#3493=EDGE_LOOP('',(#11423,#11424,#11425,#11426));
#3494=EDGE_LOOP('',(#11427,#11428,#11429,#11430));
#3495=EDGE_LOOP('',(#11431,#11432,#11433,#11434));
#3496=EDGE_LOOP('',(#11435,#11436,#11437,#11438));
#3497=EDGE_LOOP('',(#11439,#11440,#11441,#11442));
#3498=EDGE_LOOP('',(#11443,#11444,#11445,#11446));
#3499=EDGE_LOOP('',(#11447));
#3500=EDGE_LOOP('',(#11448));
#3501=EDGE_LOOP('',(#11449));
#3502=EDGE_LOOP('',(#11450));
#3503=EDGE_LOOP('',(#11451));
#3504=EDGE_LOOP('',(#11452,#11453,#11454,#11455));
#3505=EDGE_LOOP('',(#11456));
#3506=EDGE_LOOP('',(#11457));
#3507=EDGE_LOOP('',(#11458));
#3508=EDGE_LOOP('',(#11459));
#3509=EDGE_LOOP('',(#11460));
#3510=EDGE_LOOP('',(#11461,#11462,#11463,#11464));
#3511=EDGE_LOOP('',(#11465,#11466,#11467,#11468));
#3512=EDGE_LOOP('',(#11469,#11470,#11471,#11472));
#3513=EDGE_LOOP('',(#11473,#11474,#11475,#11476));
#3514=EDGE_LOOP('',(#11477,#11478,#11479,#11480));
#3515=EDGE_LOOP('',(#11481,#11482,#11483,#11484));
#3516=EDGE_LOOP('',(#11485,#11486,#11487,#11488));
#3517=EDGE_LOOP('',(#11489,#11490,#11491,#11492));
#3518=EDGE_LOOP('',(#11493,#11494,#11495,#11496));
#3519=EDGE_LOOP('',(#11497,#11498,#11499,#11500));
#3520=EDGE_LOOP('',(#11501,#11502,#11503,#11504));
#3521=EDGE_LOOP('',(#11505,#11506,#11507,#11508));
#3522=EDGE_LOOP('',(#11509,#11510,#11511,#11512));
#3523=EDGE_LOOP('',(#11513,#11514,#11515,#11516));
#3524=EDGE_LOOP('',(#11517,#11518,#11519,#11520));
#3525=EDGE_LOOP('',(#11521,#11522,#11523,#11524));
#3526=EDGE_LOOP('',(#11525,#11526,#11527,#11528));
#3527=EDGE_LOOP('',(#11529,#11530,#11531,#11532));
#3528=EDGE_LOOP('',(#11533,#11534,#11535,#11536));
#3529=EDGE_LOOP('',(#11537,#11538,#11539,#11540));
#3530=EDGE_LOOP('',(#11541,#11542,#11543,#11544));
#3531=EDGE_LOOP('',(#11545,#11546,#11547,#11548));
#3532=EDGE_LOOP('',(#11549,#11550,#11551,#11552));
#3533=EDGE_LOOP('',(#11553,#11554,#11555,#11556));
#3534=EDGE_LOOP('',(#11557,#11558,#11559,#11560));
#3535=EDGE_LOOP('',(#11561,#11562,#11563,#11564));
#3536=EDGE_LOOP('',(#11565,#11566,#11567,#11568));
#3537=EDGE_LOOP('',(#11569,#11570,#11571,#11572));
#3538=EDGE_LOOP('',(#11573,#11574,#11575,#11576));
#3539=EDGE_LOOP('',(#11577,#11578,#11579,#11580));
#3540=EDGE_LOOP('',(#11581,#11582,#11583,#11584));
#3541=EDGE_LOOP('',(#11585,#11586,#11587,#11588));
#3542=EDGE_LOOP('',(#11589,#11590,#11591,#11592));
#3543=EDGE_LOOP('',(#11593,#11594,#11595,#11596));
#3544=EDGE_LOOP('',(#11597,#11598,#11599,#11600));
#3545=EDGE_LOOP('',(#11601,#11602,#11603,#11604));
#3546=EDGE_LOOP('',(#11605,#11606,#11607,#11608));
#3547=EDGE_LOOP('',(#11609,#11610,#11611,#11612));
#3548=EDGE_LOOP('',(#11613,#11614,#11615,#11616,#11617,#11618,#11619,#11620));
#3549=EDGE_LOOP('',(#11621,#11622,#11623,#11624,#11625,#11626,#11627,#11628,
#11629,#11630,#11631,#11632,#11633,#11634,#11635,#11636,#11637,#11638,#11639,
#11640,#11641,#11642,#11643,#11644,#11645,#11646,#11647,#11648,#11649,#11650,
#11651,#11652,#11653,#11654,#11655,#11656,#11657,#11658,#11659,#11660,#11661,
#11662));
#3550=EDGE_LOOP('',(#11663,#11664,#11665,#11666));
#3551=EDGE_LOOP('',(#11667,#11668,#11669,#11670,#11671,#11672,#11673,#11674,
#11675,#11676,#11677,#11678,#11679,#11680,#11681,#11682,#11683,#11684,#11685,
#11686,#11687,#11688,#11689,#11690,#11691,#11692,#11693,#11694,#11695,#11696,
#11697,#11698,#11699,#11700,#11701,#11702,#11703,#11704,#11705,#11706,#11707,
#11708,#11709));
#3552=EDGE_LOOP('',(#11710,#11711,#11712,#11713));
#3553=EDGE_LOOP('',(#11714,#11715,#11716,#11717));
#3554=EDGE_LOOP('',(#11718,#11719,#11720,#11721));
#3555=EDGE_LOOP('',(#11722,#11723,#11724,#11725));
#3556=EDGE_LOOP('',(#11726,#11727,#11728,#11729));
#3557=EDGE_LOOP('',(#11730,#11731,#11732,#11733));
#3558=EDGE_LOOP('',(#11734,#11735,#11736,#11737));
#3559=EDGE_LOOP('',(#11738,#11739,#11740,#11741,#11742,#11743));
#3560=EDGE_LOOP('',(#11744));
#3561=EDGE_LOOP('',(#11745,#11746,#11747,#11748));
#3562=EDGE_LOOP('',(#11749,#11750,#11751,#11752));
#3563=EDGE_LOOP('',(#11753));
#3564=EDGE_LOOP('',(#11754,#11755,#11756,#11757,#11758,#11759));
#3565=EDGE_LOOP('',(#11760));
#3566=EDGE_LOOP('',(#11761,#11762,#11763,#11764));
#3567=EDGE_LOOP('',(#11765));
#3568=EDGE_LOOP('',(#11766));
#3569=EDGE_LOOP('',(#11767,#11768,#11769,#11770,#11771,#11772,#11773,#11774));
#3570=EDGE_LOOP('',(#11775,#11776,#11777,#11778));
#3571=EDGE_LOOP('',(#11779,#11780,#11781,#11782));
#3572=EDGE_LOOP('',(#11783,#11784,#11785,#11786));
#3573=EDGE_LOOP('',(#11787,#11788,#11789,#11790));
#3574=EDGE_LOOP('',(#11791,#11792,#11793,#11794));
#3575=EDGE_LOOP('',(#11795,#11796,#11797,#11798));
#3576=EDGE_LOOP('',(#11799,#11800,#11801,#11802));
#3577=EDGE_LOOP('',(#11803,#11804,#11805,#11806));
#3578=EDGE_LOOP('',(#11807,#11808,#11809,#11810));
#3579=EDGE_LOOP('',(#11811,#11812,#11813,#11814));
#3580=EDGE_LOOP('',(#11815,#11816,#11817,#11818));
#3581=EDGE_LOOP('',(#11819,#11820,#11821,#11822));
#3582=EDGE_LOOP('',(#11823,#11824,#11825,#11826));
#3583=EDGE_LOOP('',(#11827,#11828,#11829,#11830));
#3584=EDGE_LOOP('',(#11831,#11832,#11833,#11834));
#3585=EDGE_LOOP('',(#11835,#11836,#11837,#11838,#11839,#11840,#11841,#11842));
#3586=EDGE_LOOP('',(#11843,#11844,#11845,#11846));
#3587=EDGE_LOOP('',(#11847,#11848,#11849,#11850));
#3588=EDGE_LOOP('',(#11851,#11852,#11853,#11854));
#3589=EDGE_LOOP('',(#11855,#11856,#11857,#11858));
#3590=EDGE_LOOP('',(#11859,#11860,#11861,#11862));
#3591=EDGE_LOOP('',(#11863,#11864,#11865,#11866));
#3592=EDGE_LOOP('',(#11867,#11868,#11869,#11870));
#3593=EDGE_LOOP('',(#11871,#11872,#11873,#11874));
#3594=EDGE_LOOP('',(#11875,#11876,#11877,#11878));
#3595=EDGE_LOOP('',(#11879,#11880,#11881,#11882));
#3596=EDGE_LOOP('',(#11883,#11884,#11885,#11886));
#3597=EDGE_LOOP('',(#11887,#11888,#11889,#11890));
#3598=EDGE_LOOP('',(#11891,#11892,#11893,#11894));
#3599=EDGE_LOOP('',(#11895,#11896,#11897,#11898));
#3600=EDGE_LOOP('',(#11899,#11900,#11901,#11902));
#3601=EDGE_LOOP('',(#11903,#11904,#11905,#11906,#11907,#11908,#11909,#11910));
#3602=EDGE_LOOP('',(#11911,#11912,#11913,#11914));
#3603=EDGE_LOOP('',(#11915,#11916,#11917,#11918));
#3604=EDGE_LOOP('',(#11919,#11920,#11921,#11922));
#3605=EDGE_LOOP('',(#11923,#11924,#11925,#11926));
#3606=EDGE_LOOP('',(#11927,#11928,#11929,#11930));
#3607=EDGE_LOOP('',(#11931,#11932,#11933,#11934));
#3608=EDGE_LOOP('',(#11935,#11936,#11937,#11938));
#3609=EDGE_LOOP('',(#11939,#11940,#11941,#11942));
#3610=EDGE_LOOP('',(#11943,#11944,#11945,#11946));
#3611=EDGE_LOOP('',(#11947,#11948,#11949,#11950));
#3612=EDGE_LOOP('',(#11951,#11952,#11953,#11954));
#3613=EDGE_LOOP('',(#11955,#11956,#11957,#11958));
#3614=EDGE_LOOP('',(#11959,#11960,#11961,#11962));
#3615=EDGE_LOOP('',(#11963,#11964,#11965,#11966));
#3616=EDGE_LOOP('',(#11967,#11968,#11969,#11970));
#3617=EDGE_LOOP('',(#11971,#11972,#11973,#11974,#11975));
#3618=EDGE_LOOP('',(#11976,#11977,#11978,#11979));
#3619=EDGE_LOOP('',(#11980,#11981,#11982,#11983,#11984,#11985,#11986,#11987,
#11988,#11989,#11990,#11991,#11992,#11993,#11994,#11995,#11996,#11997,#11998,
#11999));
#3620=EDGE_LOOP('',(#12000,#12001,#12002,#12003,#12004,#12005,#12006,#12007,
#12008,#12009,#12010,#12011,#12012,#12013,#12014,#12015,#12016,#12017,#12018,
#12019));
#3621=EDGE_LOOP('',(#12020,#12021,#12022,#12023));
#3622=EDGE_LOOP('',(#12024,#12025,#12026,#12027,#12028));
#3623=EDGE_LOOP('',(#12029,#12030,#12031,#12032));
#3624=EDGE_LOOP('',(#12033,#12034,#12035,#12036,#12037,#12038,#12039,#12040,
#12041,#12042,#12043,#12044,#12045,#12046,#12047,#12048,#12049,#12050,#12051,
#12052));
#3625=EDGE_LOOP('',(#12053,#12054,#12055,#12056,#12057,#12058,#12059,#12060,
#12061,#12062,#12063,#12064,#12065,#12066,#12067,#12068,#12069,#12070,#12071,
#12072));
#3626=EDGE_LOOP('',(#12073,#12074,#12075,#12076));
#3627=EDGE_LOOP('',(#12077,#12078,#12079,#12080,#12081));
#3628=EDGE_LOOP('',(#12082,#12083,#12084,#12085));
#3629=EDGE_LOOP('',(#12086,#12087,#12088,#12089,#12090,#12091,#12092,#12093,
#12094,#12095,#12096,#12097,#12098,#12099,#12100,#12101,#12102,#12103,#12104,
#12105));
#3630=EDGE_LOOP('',(#12106,#12107,#12108,#12109,#12110,#12111,#12112,#12113,
#12114,#12115,#12116,#12117,#12118,#12119,#12120,#12121,#12122,#12123,#12124,
#12125));
#3631=EDGE_LOOP('',(#12126,#12127,#12128,#12129));
#3632=EDGE_LOOP('',(#12130));
#3633=EDGE_LOOP('',(#12131));
#3634=EDGE_LOOP('',(#12132));
#3635=EDGE_LOOP('',(#12133,#12134,#12135));
#3636=EDGE_LOOP('',(#12136,#12137,#12138,#12139));
#3637=EDGE_LOOP('',(#12140));
#3638=EDGE_LOOP('',(#12141,#12142,#12143,#12144));
#3639=EDGE_LOOP('',(#12145,#12146,#12147,#12148));
#3640=EDGE_LOOP('',(#12149,#12150,#12151,#12152));
#3641=EDGE_LOOP('',(#12153));
#3642=EDGE_LOOP('',(#12154));
#3643=EDGE_LOOP('',(#12155,#12156,#12157,#12158));
#3644=EDGE_LOOP('',(#12159,#12160,#12161,#12162));
#3645=EDGE_LOOP('',(#12163,#12164,#12165,#12166));
#3646=EDGE_LOOP('',(#12167,#12168,#12169,#12170));
#3647=EDGE_LOOP('',(#12171,#12172,#12173,#12174));
#3648=EDGE_LOOP('',(#12175,#12176,#12177,#12178));
#3649=EDGE_LOOP('',(#12179));
#3650=EDGE_LOOP('',(#12180));
#3651=EDGE_LOOP('',(#12181));
#3652=EDGE_LOOP('',(#12182));
#3653=EDGE_LOOP('',(#12183));
#3654=EDGE_LOOP('',(#12184));
#3655=EDGE_LOOP('',(#12185));
#3656=EDGE_LOOP('',(#12186));
#3657=EDGE_LOOP('',(#12187));
#3658=EDGE_LOOP('',(#12188));
#3659=EDGE_LOOP('',(#12189,#12190,#12191,#12192));
#3660=EDGE_LOOP('',(#12193,#12194,#12195,#12196));
#3661=EDGE_LOOP('',(#12197,#12198,#12199,#12200));
#3662=EDGE_LOOP('',(#12201,#12202,#12203,#12204));
#3663=EDGE_LOOP('',(#12205,#12206,#12207,#12208));
#3664=EDGE_LOOP('',(#12209,#12210,#12211,#12212));
#3665=EDGE_LOOP('',(#12213,#12214,#12215,#12216));
#3666=EDGE_LOOP('',(#12217,#12218,#12219,#12220));
#3667=EDGE_LOOP('',(#12221,#12222,#12223,#12224));
#3668=EDGE_LOOP('',(#12225,#12226,#12227,#12228));
#3669=EDGE_LOOP('',(#12229,#12230,#12231,#12232));
#3670=EDGE_LOOP('',(#12233,#12234,#12235,#12236));
#3671=EDGE_LOOP('',(#12237,#12238,#12239,#12240));
#3672=EDGE_LOOP('',(#12241,#12242,#12243,#12244));
#3673=EDGE_LOOP('',(#12245,#12246,#12247,#12248));
#3674=EDGE_LOOP('',(#12249,#12250,#12251,#12252));
#3675=EDGE_LOOP('',(#12253,#12254,#12255,#12256));
#3676=EDGE_LOOP('',(#12257,#12258,#12259,#12260));
#3677=EDGE_LOOP('',(#12261,#12262,#12263,#12264));
#3678=EDGE_LOOP('',(#12265,#12266,#12267,#12268));
#3679=EDGE_LOOP('',(#12269,#12270,#12271,#12272));
#3680=EDGE_LOOP('',(#12273,#12274,#12275,#12276));
#3681=EDGE_LOOP('',(#12277,#12278,#12279,#12280));
#3682=EDGE_LOOP('',(#12281,#12282,#12283,#12284));
#3683=EDGE_LOOP('',(#12285,#12286,#12287,#12288));
#3684=EDGE_LOOP('',(#12289,#12290,#12291,#12292));
#3685=EDGE_LOOP('',(#12293,#12294,#12295,#12296));
#3686=EDGE_LOOP('',(#12297,#12298,#12299,#12300));
#3687=EDGE_LOOP('',(#12301,#12302,#12303,#12304));
#3688=EDGE_LOOP('',(#12305,#12306,#12307,#12308));
#3689=EDGE_LOOP('',(#12309,#12310,#12311,#12312));
#3690=EDGE_LOOP('',(#12313,#12314,#12315,#12316));
#3691=EDGE_LOOP('',(#12317,#12318,#12319,#12320));
#3692=EDGE_LOOP('',(#12321,#12322,#12323,#12324));
#3693=EDGE_LOOP('',(#12325,#12326,#12327,#12328));
#3694=EDGE_LOOP('',(#12329,#12330,#12331,#12332));
#3695=EDGE_LOOP('',(#12333,#12334,#12335,#12336));
#3696=EDGE_LOOP('',(#12337,#12338,#12339,#12340));
#3697=EDGE_LOOP('',(#12341,#12342,#12343,#12344));
#3698=EDGE_LOOP('',(#12345,#12346,#12347,#12348));
#3699=EDGE_LOOP('',(#12349,#12350,#12351,#12352));
#3700=EDGE_LOOP('',(#12353,#12354,#12355,#12356));
#3701=EDGE_LOOP('',(#12357,#12358,#12359,#12360));
#3702=EDGE_LOOP('',(#12361,#12362,#12363,#12364));
#3703=EDGE_LOOP('',(#12365,#12366,#12367,#12368));
#3704=EDGE_LOOP('',(#12369,#12370,#12371,#12372));
#3705=EDGE_LOOP('',(#12373,#12374,#12375,#12376));
#3706=EDGE_LOOP('',(#12377,#12378,#12379,#12380));
#3707=EDGE_LOOP('',(#12381,#12382,#12383,#12384));
#3708=EDGE_LOOP('',(#12385,#12386,#12387,#12388));
#3709=EDGE_LOOP('',(#12389,#12390,#12391,#12392));
#3710=EDGE_LOOP('',(#12393,#12394,#12395,#12396));
#3711=EDGE_LOOP('',(#12397,#12398,#12399,#12400));
#3712=EDGE_LOOP('',(#12401,#12402,#12403,#12404));
#3713=EDGE_LOOP('',(#12405,#12406,#12407,#12408));
#3714=EDGE_LOOP('',(#12409,#12410,#12411,#12412));
#3715=EDGE_LOOP('',(#12413,#12414,#12415,#12416));
#3716=EDGE_LOOP('',(#12417,#12418,#12419,#12420));
#3717=EDGE_LOOP('',(#12421,#12422,#12423,#12424));
#3718=EDGE_LOOP('',(#12425,#12426,#12427,#12428));
#3719=EDGE_LOOP('',(#12429,#12430,#12431,#12432));
#3720=EDGE_LOOP('',(#12433,#12434,#12435,#12436));
#3721=EDGE_LOOP('',(#12437,#12438,#12439,#12440));
#3722=EDGE_LOOP('',(#12441,#12442,#12443,#12444));
#3723=EDGE_LOOP('',(#12445,#12446,#12447,#12448));
#3724=EDGE_LOOP('',(#12449,#12450,#12451,#12452));
#3725=EDGE_LOOP('',(#12453,#12454,#12455,#12456));
#3726=EDGE_LOOP('',(#12457,#12458,#12459,#12460));
#3727=EDGE_LOOP('',(#12461,#12462,#12463,#12464));
#3728=EDGE_LOOP('',(#12465,#12466,#12467,#12468));
#3729=EDGE_LOOP('',(#12469,#12470,#12471,#12472));
#3730=EDGE_LOOP('',(#12473,#12474,#12475,#12476));
#3731=EDGE_LOOP('',(#12477,#12478,#12479,#12480));
#3732=EDGE_LOOP('',(#12481,#12482,#12483,#12484));
#3733=EDGE_LOOP('',(#12485,#12486,#12487,#12488));
#3734=EDGE_LOOP('',(#12489,#12490,#12491,#12492));
#3735=EDGE_LOOP('',(#12493,#12494,#12495,#12496));
#3736=EDGE_LOOP('',(#12497,#12498,#12499,#12500));
#3737=EDGE_LOOP('',(#12501,#12502,#12503,#12504));
#3738=EDGE_LOOP('',(#12505,#12506,#12507,#12508));
#3739=EDGE_LOOP('',(#12509,#12510,#12511,#12512));
#3740=EDGE_LOOP('',(#12513,#12514,#12515,#12516));
#3741=EDGE_LOOP('',(#12517,#12518,#12519,#12520));
#3742=EDGE_LOOP('',(#12521,#12522,#12523,#12524));
#3743=EDGE_LOOP('',(#12525,#12526,#12527,#12528));
#3744=EDGE_LOOP('',(#12529,#12530,#12531,#12532));
#3745=EDGE_LOOP('',(#12533,#12534,#12535,#12536));
#3746=EDGE_LOOP('',(#12537,#12538,#12539,#12540));
#3747=EDGE_LOOP('',(#12541,#12542,#12543,#12544));
#3748=EDGE_LOOP('',(#12545,#12546,#12547,#12548));
#3749=EDGE_LOOP('',(#12549,#12550,#12551,#12552));
#3750=EDGE_LOOP('',(#12553,#12554,#12555,#12556));
#3751=EDGE_LOOP('',(#12557,#12558,#12559,#12560));
#3752=EDGE_LOOP('',(#12561,#12562,#12563,#12564));
#3753=EDGE_LOOP('',(#12565,#12566,#12567,#12568));
#3754=EDGE_LOOP('',(#12569,#12570,#12571,#12572));
#3755=EDGE_LOOP('',(#12573,#12574,#12575,#12576));
#3756=EDGE_LOOP('',(#12577,#12578,#12579,#12580));
#3757=EDGE_LOOP('',(#12581,#12582,#12583,#12584));
#3758=EDGE_LOOP('',(#12585,#12586,#12587,#12588));
#3759=EDGE_LOOP('',(#12589,#12590,#12591,#12592));
#3760=EDGE_LOOP('',(#12593,#12594,#12595,#12596));
#3761=EDGE_LOOP('',(#12597,#12598,#12599,#12600));
#3762=EDGE_LOOP('',(#12601,#12602,#12603,#12604));
#3763=EDGE_LOOP('',(#12605,#12606,#12607,#12608));
#3764=EDGE_LOOP('',(#12609,#12610,#12611,#12612));
#3765=EDGE_LOOP('',(#12613,#12614,#12615,#12616));
#3766=EDGE_LOOP('',(#12617,#12618,#12619,#12620));
#3767=EDGE_LOOP('',(#12621,#12622,#12623,#12624));
#3768=EDGE_LOOP('',(#12625,#12626,#12627,#12628));
#3769=EDGE_LOOP('',(#12629,#12630,#12631,#12632));
#3770=EDGE_LOOP('',(#12633,#12634,#12635,#12636));
#3771=EDGE_LOOP('',(#12637,#12638,#12639,#12640));
#3772=EDGE_LOOP('',(#12641,#12642,#12643,#12644));
#3773=EDGE_LOOP('',(#12645,#12646,#12647,#12648));
#3774=EDGE_LOOP('',(#12649,#12650,#12651,#12652));
#3775=EDGE_LOOP('',(#12653,#12654,#12655,#12656));
#3776=EDGE_LOOP('',(#12657,#12658,#12659,#12660));
#3777=EDGE_LOOP('',(#12661,#12662,#12663,#12664));
#3778=EDGE_LOOP('',(#12665,#12666,#12667,#12668));
#3779=EDGE_LOOP('',(#12669,#12670,#12671,#12672,#12673,#12674,#12675,#12676,
#12677,#12678,#12679,#12680,#12681,#12682,#12683,#12684,#12685,#12686,#12687,
#12688,#12689,#12690,#12691,#12692,#12693,#12694,#12695,#12696,#12697,#12698,
#12699,#12700,#12701,#12702,#12703,#12704,#12705,#12706,#12707,#12708,#12709,
#12710,#12711,#12712,#12713,#12714,#12715,#12716,#12717,#12718,#12719,#12720,
#12721,#12722,#12723,#12724,#12725,#12726,#12727,#12728,#12729,#12730,#12731,
#12732,#12733,#12734,#12735,#12736,#12737,#12738,#12739,#12740,#12741,#12742,
#12743,#12744,#12745,#12746,#12747,#12748,#12749,#12750,#12751,#12752,#12753,
#12754,#12755,#12756,#12757,#12758,#12759,#12760,#12761,#12762,#12763,#12764,
#12765,#12766,#12767,#12768,#12769,#12770,#12771,#12772,#12773,#12774,#12775,
#12776,#12777,#12778,#12779,#12780,#12781,#12782,#12783,#12784,#12785,#12786,
#12787,#12788,#12789,#12790,#12791,#12792));
#3780=EDGE_LOOP('',(#12793,#12794,#12795,#12796));
#3781=EDGE_LOOP('',(#12797,#12798,#12799,#12800,#12801,#12802,#12803,#12804,
#12805,#12806,#12807,#12808,#12809,#12810,#12811,#12812,#12813,#12814,#12815,
#12816,#12817,#12818,#12819,#12820,#12821,#12822,#12823,#12824,#12825,#12826,
#12827,#12828,#12829,#12830,#12831,#12832,#12833,#12834,#12835,#12836,#12837,
#12838,#12839,#12840,#12841,#12842,#12843,#12844,#12845,#12846,#12847,#12848,
#12849,#12850,#12851,#12852,#12853,#12854,#12855,#12856,#12857,#12858,#12859,
#12860,#12861,#12862,#12863,#12864,#12865,#12866,#12867,#12868,#12869,#12870,
#12871,#12872,#12873,#12874,#12875,#12876,#12877,#12878,#12879,#12880,#12881,
#12882,#12883,#12884,#12885,#12886,#12887,#12888,#12889,#12890,#12891,#12892,
#12893,#12894,#12895,#12896,#12897,#12898,#12899,#12900,#12901,#12902,#12903,
#12904,#12905,#12906,#12907,#12908,#12909,#12910,#12911,#12912,#12913,#12914,
#12915,#12916,#12917,#12918,#12919,#12920));
#3782=EDGE_LOOP('',(#12921,#12922,#12923,#12924));
#3783=EDGE_LOOP('',(#12925,#12926,#12927,#12928,#12929,#12930));
#3784=EDGE_LOOP('',(#12931,#12932,#12933,#12934));
#3785=EDGE_LOOP('',(#12935,#12936,#12937,#12938,#12939,#12940));
#3786=EDGE_LOOP('',(#12941));
#3787=EDGE_LOOP('',(#12942,#12943,#12944,#12945));
#3788=EDGE_LOOP('',(#12946,#12947,#12948,#12949));
#3789=EDGE_LOOP('',(#12950,#12951,#12952,#12953));
#3790=EDGE_LOOP('',(#12954,#12955,#12956,#12957));
#3791=EDGE_LOOP('',(#12958,#12959,#12960,#12961));
#3792=EDGE_LOOP('',(#12962,#12963,#12964,#12965));
#3793=EDGE_LOOP('',(#12966,#12967,#12968,#12969));
#3794=EDGE_LOOP('',(#12970,#12971,#12972,#12973));
#3795=EDGE_LOOP('',(#12974,#12975,#12976));
#3796=EDGE_LOOP('',(#12977,#12978,#12979,#12980));
#3797=EDGE_LOOP('',(#12981,#12982,#12983,#12984));
#3798=EDGE_LOOP('',(#12985,#12986,#12987,#12988));
#3799=EDGE_LOOP('',(#12989,#12990,#12991,#12992));
#3800=EDGE_LOOP('',(#12993,#12994,#12995,#12996));
#3801=EDGE_LOOP('',(#12997,#12998,#12999,#13000));
#3802=EDGE_LOOP('',(#13001,#13002,#13003,#13004));
#3803=EDGE_LOOP('',(#13005,#13006,#13007,#13008));
#3804=EDGE_LOOP('',(#13009,#13010,#13011,#13012));
#3805=EDGE_LOOP('',(#13013,#13014,#13015,#13016));
#3806=EDGE_LOOP('',(#13017,#13018,#13019,#13020));
#3807=EDGE_LOOP('',(#13021,#13022,#13023,#13024));
#3808=EDGE_LOOP('',(#13025,#13026,#13027,#13028));
#3809=EDGE_LOOP('',(#13029,#13030,#13031,#13032));
#3810=EDGE_LOOP('',(#13033,#13034,#13035,#13036));
#3811=EDGE_LOOP('',(#13037,#13038,#13039,#13040));
#3812=EDGE_LOOP('',(#13041,#13042,#13043,#13044));
#3813=EDGE_LOOP('',(#13045,#13046,#13047,#13048,#13049,#13050,#13051,#13052,
#13053,#13054,#13055,#13056,#13057,#13058,#13059,#13060,#13061,#13062,#13063,
#13064));
#3814=EDGE_LOOP('',(#13065,#13066,#13067,#13068,#13069,#13070,#13071,#13072,
#13073,#13074,#13075,#13076,#13077,#13078,#13079,#13080,#13081,#13082,#13083,
#13084));
#3815=EDGE_LOOP('',(#13085,#13086,#13087,#13088,#13089,#13090));
#3816=EDGE_LOOP('',(#13091,#13092,#13093,#13094));
#3817=EDGE_LOOP('',(#13095,#13096,#13097,#13098));
#3818=EDGE_LOOP('',(#13099,#13100,#13101,#13102));
#3819=EDGE_LOOP('',(#13103,#13104,#13105,#13106));
#3820=EDGE_LOOP('',(#13107,#13108,#13109,#13110));
#3821=EDGE_LOOP('',(#13111,#13112,#13113,#13114));
#3822=EDGE_LOOP('',(#13115,#13116,#13117,#13118));
#3823=EDGE_LOOP('',(#13119,#13120,#13121,#13122));
#3824=EDGE_LOOP('',(#13123,#13124,#13125,#13126,#13127,#13128));
#3825=EDGE_LOOP('',(#13129,#13130,#13131,#13132));
#3826=EDGE_LOOP('',(#13133,#13134,#13135,#13136));
#3827=EDGE_LOOP('',(#13137,#13138,#13139,#13140));
#3828=EDGE_LOOP('',(#13141));
#3829=EDGE_LOOP('',(#13142));
#3830=EDGE_LOOP('',(#13143));
#3831=EDGE_LOOP('',(#13144));
#3832=EDGE_LOOP('',(#13145,#13146,#13147,#13148));
#3833=EDGE_LOOP('',(#13149,#13150,#13151,#13152));
#3834=EDGE_LOOP('',(#13153,#13154,#13155,#13156));
#3835=EDGE_LOOP('',(#13157,#13158,#13159,#13160));
#3836=EDGE_LOOP('',(#13161,#13162,#13163,#13164));
#3837=EDGE_LOOP('',(#13165,#13166,#13167,#13168));
#3838=EDGE_LOOP('',(#13169,#13170,#13171,#13172));
#3839=EDGE_LOOP('',(#13173,#13174,#13175,#13176));
#3840=EDGE_LOOP('',(#13177,#13178,#13179,#13180));
#3841=EDGE_LOOP('',(#13181,#13182,#13183,#13184));
#3842=EDGE_LOOP('',(#13185,#13186,#13187,#13188));
#3843=EDGE_LOOP('',(#13189,#13190,#13191,#13192));
#3844=EDGE_LOOP('',(#13193,#13194,#13195,#13196));
#3845=EDGE_LOOP('',(#13197,#13198,#13199,#13200));
#3846=EDGE_LOOP('',(#13201,#13202,#13203,#13204));
#3847=EDGE_LOOP('',(#13205,#13206,#13207,#13208));
#3848=EDGE_LOOP('',(#13209,#13210,#13211,#13212));
#3849=EDGE_LOOP('',(#13213,#13214,#13215,#13216));
#3850=EDGE_LOOP('',(#13217,#13218,#13219,#13220));
#3851=EDGE_LOOP('',(#13221,#13222,#13223,#13224));
#3852=EDGE_LOOP('',(#13225,#13226,#13227,#13228));
#3853=EDGE_LOOP('',(#13229,#13230,#13231,#13232));
#3854=EDGE_LOOP('',(#13233,#13234,#13235,#13236));
#3855=EDGE_LOOP('',(#13237,#13238,#13239,#13240));
#3856=EDGE_LOOP('',(#13241,#13242,#13243,#13244));
#3857=EDGE_LOOP('',(#13245,#13246,#13247,#13248));
#3858=EDGE_LOOP('',(#13249,#13250,#13251,#13252));
#3859=EDGE_LOOP('',(#13253,#13254,#13255,#13256));
#3860=EDGE_LOOP('',(#13257,#13258,#13259,#13260));
#3861=EDGE_LOOP('',(#13261,#13262,#13263,#13264));
#3862=EDGE_LOOP('',(#13265,#13266,#13267,#13268,#13269,#13270,#13271,#13272));
#3863=EDGE_LOOP('',(#13273,#13274,#13275,#13276,#13277,#13278,#13279,#13280,
#13281,#13282,#13283,#13284,#13285,#13286,#13287,#13288,#13289,#13290,#13291,
#13292,#13293,#13294,#13295,#13296,#13297,#13298,#13299,#13300,#13301,#13302,
#13303,#13304,#13305,#13306));
#3864=EDGE_LOOP('',(#13307,#13308,#13309,#13310));
#3865=EDGE_LOOP('',(#13311,#13312,#13313,#13314,#13315,#13316,#13317,#13318,
#13319,#13320,#13321,#13322,#13323,#13324,#13325,#13326,#13327,#13328,#13329,
#13330,#13331,#13332,#13333,#13334,#13335,#13336,#13337,#13338,#13339,#13340,
#13341,#13342,#13343,#13344,#13345));
#3866=EDGE_LOOP('',(#13346,#13347,#13348,#13349));
#3867=EDGE_LOOP('',(#13350,#13351,#13352,#13353));
#3868=EDGE_LOOP('',(#13354,#13355,#13356,#13357));
#3869=EDGE_LOOP('',(#13358,#13359,#13360,#13361));
#3870=EDGE_LOOP('',(#13362,#13363,#13364,#13365));
#3871=EDGE_LOOP('',(#13366,#13367,#13368,#13369));
#3872=EDGE_LOOP('',(#13370,#13371,#13372,#13373));
#3873=EDGE_LOOP('',(#13374,#13375,#13376,#13377,#13378,#13379));
#3874=EDGE_LOOP('',(#13380));
#3875=EDGE_LOOP('',(#13381,#13382,#13383,#13384));
#3876=EDGE_LOOP('',(#13385,#13386,#13387,#13388));
#3877=EDGE_LOOP('',(#13389));
#3878=EDGE_LOOP('',(#13390,#13391,#13392,#13393,#13394,#13395));
#3879=EDGE_LOOP('',(#13396));
#3880=EDGE_LOOP('',(#13397,#13398,#13399,#13400));
#3881=EDGE_LOOP('',(#13401,#13402,#13403,#13404));
#3882=EDGE_LOOP('',(#13405));
#3883=EDGE_LOOP('',(#13406));
#3884=EDGE_LOOP('',(#13407));
#3885=EDGE_LOOP('',(#13408));
#3886=LINE('',#18383,#4722);
#3887=LINE('',#18385,#4723);
#3888=LINE('',#18387,#4724);
#3889=LINE('',#18388,#4725);
#3890=LINE('',#18391,#4726);
#3891=LINE('',#18393,#4727);
#3892=LINE('',#18394,#4728);
#3893=LINE('',#18397,#4729);
#3894=LINE('',#18399,#4730);
#3895=LINE('',#18400,#4731);
#3896=LINE('',#18402,#4732);
#3897=LINE('',#18403,#4733);
#3898=LINE('',#18407,#4734);
#3899=LINE('',#18409,#4735);
#3900=LINE('',#18411,#4736);
#3901=LINE('',#18412,#4737);
#3902=LINE('',#18415,#4738);
#3903=LINE('',#18417,#4739);
#3904=LINE('',#18418,#4740);
#3905=LINE('',#18421,#4741);
#3906=LINE('',#18423,#4742);
#3907=LINE('',#18424,#4743);
#3908=LINE('',#18426,#4744);
#3909=LINE('',#18427,#4745);
#3910=LINE('',#18434,#4746);
#3911=LINE('',#18436,#4747);
#3912=LINE('',#18438,#4748);
#3913=LINE('',#18439,#4749);
#3914=LINE('',#18442,#4750);
#3915=LINE('',#18444,#4751);
#3916=LINE('',#18445,#4752);
#3917=LINE('',#18448,#4753);
#3918=LINE('',#18450,#4754);
#3919=LINE('',#18451,#4755);
#3920=LINE('',#18453,#4756);
#3921=LINE('',#18454,#4757);
#3922=LINE('',#18458,#4758);
#3923=LINE('',#18460,#4759);
#3924=LINE('',#18462,#4760);
#3925=LINE('',#18463,#4761);
#3926=LINE('',#18466,#4762);
#3927=LINE('',#18468,#4763);
#3928=LINE('',#18469,#4764);
#3929=LINE('',#18472,#4765);
#3930=LINE('',#18474,#4766);
#3931=LINE('',#18475,#4767);
#3932=LINE('',#18477,#4768);
#3933=LINE('',#18478,#4769);
#3934=LINE('',#18485,#4770);
#3935=LINE('',#18506,#4771);
#3936=LINE('',#18557,#4772);
#3937=LINE('',#18608,#4773);
#3938=LINE('',#18656,#4774);
#3939=LINE('',#18707,#4775);
#3940=LINE('',#18758,#4776);
#3941=LINE('',#18806,#4777);
#3942=LINE('',#18845,#4778);
#3943=LINE('',#18866,#4779);
#3944=LINE('',#18917,#4780);
#3945=LINE('',#18968,#4781);
#3946=LINE('',#19016,#4782);
#3947=LINE('',#19067,#4783);
#3948=LINE('',#19118,#4784);
#3949=LINE('',#19166,#4785);
#3950=LINE('',#19205,#4786);
#3951=LINE('',#19226,#4787);
#3952=LINE('',#19277,#4788);
#3953=LINE('',#19328,#4789);
#3954=LINE('',#19376,#4790);
#3955=LINE('',#19427,#4791);
#3956=LINE('',#19478,#4792);
#3957=LINE('',#19526,#4793);
#3958=LINE('',#19565,#4794);
#3959=LINE('',#19586,#4795);
#3960=LINE('',#19637,#4796);
#3961=LINE('',#19688,#4797);
#3962=LINE('',#19736,#4798);
#3963=LINE('',#19787,#4799);
#3964=LINE('',#19838,#4800);
#3965=LINE('',#19886,#4801);
#3966=LINE('',#19925,#4802);
#3967=LINE('',#19949,#4803);
#3968=LINE('',#19973,#4804);
#3969=LINE('',#19998,#4805);
#3970=LINE('',#20023,#4806);
#3971=LINE('',#20047,#4807);
#3972=LINE('',#20072,#4808);
#3973=LINE('',#20097,#4809);
#3974=LINE('',#20114,#4810);
#3975=LINE('',#20138,#4811);
#3976=LINE('',#20162,#4812);
#3977=LINE('',#20187,#4813);
#3978=LINE('',#20212,#4814);
#3979=LINE('',#20236,#4815);
#3980=LINE('',#20261,#4816);
#3981=LINE('',#20286,#4817);
#3982=LINE('',#20303,#4818);
#3983=LINE('',#20327,#4819);
#3984=LINE('',#20351,#4820);
#3985=LINE('',#20376,#4821);
#3986=LINE('',#20401,#4822);
#3987=LINE('',#20425,#4823);
#3988=LINE('',#20450,#4824);
#3989=LINE('',#20475,#4825);
#3990=LINE('',#20492,#4826);
#3991=LINE('',#20516,#4827);
#3992=LINE('',#20540,#4828);
#3993=LINE('',#20565,#4829);
#3994=LINE('',#20590,#4830);
#3995=LINE('',#20614,#4831);
#3996=LINE('',#20639,#4832);
#3997=LINE('',#20664,#4833);
#3998=LINE('',#21583,#4834);
#3999=LINE('',#21585,#4835);
#4000=LINE('',#21587,#4836);
#4001=LINE('',#21588,#4837);
#4002=LINE('',#24302,#4838);
#4003=LINE('',#24303,#4839);
#4004=LINE('',#24304,#4840);
#4005=LINE('',#24307,#4841);
#4006=LINE('',#24308,#4842);
#4007=LINE('',#24311,#4843);
#4008=LINE('',#24312,#4844);
#4009=LINE('',#24314,#4845);
#4010=LINE('',#24320,#4846);
#4011=LINE('',#24344,#4847);
#4012=LINE('',#24392,#4848);
#4013=LINE('',#24440,#4849);
#4014=LINE('',#24488,#4850);
#4015=LINE('',#24542,#4851);
#4016=LINE('',#24590,#4852);
#4017=LINE('',#24638,#4853);
#4018=LINE('',#24692,#4854);
#4019=LINE('',#24740,#4855);
#4020=LINE('',#24788,#4856);
#4021=LINE('',#24842,#4857);
#4022=LINE('',#24890,#4858);
#4023=LINE('',#24938,#4859);
#4024=LINE('',#24986,#4860);
#4025=LINE('',#25040,#4861);
#4026=LINE('',#25088,#4862);
#4027=LINE('',#25136,#4863);
#4028=LINE('',#25190,#4864);
#4029=LINE('',#25238,#4865);
#4030=LINE('',#25286,#4866);
#4031=LINE('',#25334,#4867);
#4032=LINE('',#25388,#4868);
#4033=LINE('',#25436,#4869);
#4034=LINE('',#25484,#4870);
#4035=LINE('',#25509,#4871);
#4036=LINE('',#25534,#4872);
#4037=LINE('',#25558,#4873);
#4038=LINE('',#25583,#4874);
#4039=LINE('',#25608,#4875);
#4040=LINE('',#25632,#4876);
#4041=LINE('',#25656,#4877);
#4042=LINE('',#25681,#4878);
#4043=LINE('',#25706,#4879);
#4044=LINE('',#25730,#4880);
#4045=LINE('',#25755,#4881);
#4046=LINE('',#25780,#4882);
#4047=LINE('',#25804,#4883);
#4048=LINE('',#25828,#4884);
#4049=LINE('',#25853,#4885);
#4050=LINE('',#25878,#4886);
#4051=LINE('',#25902,#4887);
#4052=LINE('',#25927,#4888);
#4053=LINE('',#25952,#4889);
#4054=LINE('',#25976,#4890);
#4055=LINE('',#26001,#4891);
#4056=LINE('',#26026,#4892);
#4057=LINE('',#26050,#4893);
#4058=LINE('',#26407,#4894);
#4059=LINE('',#27941,#4895);
#4060=LINE('',#27943,#4896);
#4061=LINE('',#27945,#4897);
#4062=LINE('',#27946,#4898);
#4063=LINE('',#27949,#4899);
#4064=LINE('',#27951,#4900);
#4065=LINE('',#27952,#4901);
#4066=LINE('',#27955,#4902);
#4067=LINE('',#27957,#4903);
#4068=LINE('',#27958,#4904);
#4069=LINE('',#27961,#4905);
#4070=LINE('',#27963,#4906);
#4071=LINE('',#27964,#4907);
#4072=LINE('',#27967,#4908);
#4073=LINE('',#27969,#4909);
#4074=LINE('',#27970,#4910);
#4075=LINE('',#27972,#4911);
#4076=LINE('',#27973,#4912);
#4077=LINE('',#27980,#4913);
#4078=LINE('',#27989,#4914);
#4079=LINE('',#27995,#4915);
#4080=LINE('',#28044,#4916);
#4081=LINE('',#28056,#4917);
#4082=LINE('',#28079,#4918);
#4083=LINE('',#28169,#4919);
#4084=LINE('',#28256,#4920);
#4085=LINE('',#28343,#4921);
#4086=LINE('',#28430,#4922);
#4087=LINE('',#28520,#4923);
#4088=LINE('',#28607,#4924);
#4089=LINE('',#28694,#4925);
#4090=LINE('',#28784,#4926);
#4091=LINE('',#28871,#4927);
#4092=LINE('',#28958,#4928);
#4093=LINE('',#29045,#4929);
#4094=LINE('',#29135,#4930);
#4095=LINE('',#29222,#4931);
#4096=LINE('',#29309,#4932);
#4097=LINE('',#29396,#4933);
#4098=LINE('',#29486,#4934);
#4099=LINE('',#29573,#4935);
#4100=LINE('',#29660,#4936);
#4101=LINE('',#29750,#4937);
#4102=LINE('',#29837,#4938);
#4103=LINE('',#29924,#4939);
#4104=LINE('',#30011,#4940);
#4105=LINE('',#30101,#4941);
#4106=LINE('',#30170,#4942);
#4107=LINE('',#30203,#4943);
#4108=LINE('',#30240,#4944);
#4109=LINE('',#30278,#4945);
#4110=LINE('',#30314,#4946);
#4111=LINE('',#30352,#4947);
#4112=LINE('',#30390,#4948);
#4113=LINE('',#30426,#4949);
#4114=LINE('',#30464,#4950);
#4115=LINE('',#30502,#4951);
#4116=LINE('',#30538,#4952);
#4117=LINE('',#30576,#4953);
#4118=LINE('',#30613,#4954);
#4119=LINE('',#30650,#4955);
#4120=LINE('',#30688,#4956);
#4121=LINE('',#30724,#4957);
#4122=LINE('',#30762,#4958);
#4123=LINE('',#30800,#4959);
#4124=LINE('',#30836,#4960);
#4125=LINE('',#30874,#4961);
#4126=LINE('',#30912,#4962);
#4127=LINE('',#30948,#4963);
#4128=LINE('',#30986,#4964);
#4129=LINE('',#31023,#4965);
#4130=LINE('',#31060,#4966);
#4131=LINE('',#31080,#4967);
#4132=LINE('',#31092,#4968);
#4133=LINE('',#31115,#4969);
#4134=LINE('',#31205,#4970);
#4135=LINE('',#31292,#4971);
#4136=LINE('',#31379,#4972);
#4137=LINE('',#31466,#4973);
#4138=LINE('',#31553,#4974);
#4139=LINE('',#31643,#4975);
#4140=LINE('',#31730,#4976);
#4141=LINE('',#31817,#4977);
#4142=LINE('',#31904,#4978);
#4143=LINE('',#31991,#4979);
#4144=LINE('',#32081,#4980);
#4145=LINE('',#32168,#4981);
#4146=LINE('',#32255,#4982);
#4147=LINE('',#32342,#4983);
#4148=LINE('',#32429,#4984);
#4149=LINE('',#32516,#4985);
#4150=LINE('',#32603,#4986);
#4151=LINE('',#32690,#4987);
#4152=LINE('',#32765,#4988);
#4153=LINE('',#32813,#4989);
#4154=LINE('',#32870,#4990);
#4155=LINE('',#32957,#4991);
#4156=LINE('',#33044,#4992);
#4157=LINE('',#33131,#4993);
#4158=LINE('',#33218,#4994);
#4159=LINE('',#33305,#4995);
#4160=LINE('',#33395,#4996);
#4161=LINE('',#33482,#4997);
#4162=LINE('',#33569,#4998);
#4163=LINE('',#33656,#4999);
#4164=LINE('',#33743,#5000);
#4165=LINE('',#33833,#5001);
#4166=LINE('',#33920,#5002);
#4167=LINE('',#34007,#5003);
#4168=LINE('',#34094,#5004);
#4169=LINE('',#34181,#5005);
#4170=LINE('',#34271,#5006);
#4171=LINE('',#34358,#5007);
#4172=LINE('',#34427,#5008);
#4173=LINE('',#34460,#5009);
#4174=LINE('',#34497,#5010);
#4175=LINE('',#34535,#5011);
#4176=LINE('',#34571,#5012);
#4177=LINE('',#34609,#5013);
#4178=LINE('',#34646,#5014);
#4179=LINE('',#34683,#5015);
#4180=LINE('',#34721,#5016);
#4181=LINE('',#34757,#5017);
#4182=LINE('',#34795,#5018);
#4183=LINE('',#34832,#5019);
#4184=LINE('',#34869,#5020);
#4185=LINE('',#34907,#5021);
#4186=LINE('',#34943,#5022);
#4187=LINE('',#34981,#5023);
#4188=LINE('',#35018,#5024);
#4189=LINE('',#35055,#5025);
#4190=LINE('',#35093,#5026);
#4191=LINE('',#35129,#5027);
#4192=LINE('',#35156,#5028);
#4193=LINE('',#35180,#5029);
#4194=LINE('',#35213,#5030);
#4195=LINE('',#35251,#5031);
#4196=LINE('',#35287,#5032);
#4197=LINE('',#35325,#5033);
#4198=LINE('',#35361,#5034);
#4199=LINE('',#35399,#5035);
#4200=LINE('',#35437,#5036);
#4201=LINE('',#35473,#5037);
#4202=LINE('',#35511,#5038);
#4203=LINE('',#35547,#5039);
#4204=LINE('',#35585,#5040);
#4205=LINE('',#35623,#5041);
#4206=LINE('',#35659,#5042);
#4207=LINE('',#35697,#5043);
#4208=LINE('',#35733,#5044);
#4209=LINE('',#35771,#5045);
#4210=LINE('',#35809,#5046);
#4211=LINE('',#35845,#5047);
#4212=LINE('',#43512,#5048);
#4213=LINE('',#43515,#5049);
#4214=LINE('',#43518,#5050);
#4215=LINE('',#43520,#5051);
#4216=LINE('',#43521,#5052);
#4217=LINE('',#43524,#5053);
#4218=LINE('',#43528,#5054);
#4219=LINE('',#43532,#5055);
#4220=LINE('',#43536,#5056);
#4221=LINE('',#43540,#5057);
#4222=LINE('',#43544,#5058);
#4223=LINE('',#43548,#5059);
#4224=LINE('',#43552,#5060);
#4225=LINE('',#43556,#5061);
#4226=LINE('',#43560,#5062);
#4227=LINE('',#43564,#5063);
#4228=LINE('',#43568,#5064);
#4229=LINE('',#43572,#5065);
#4230=LINE('',#43576,#5066);
#4231=LINE('',#43580,#5067);
#4232=LINE('',#43584,#5068);
#4233=LINE('',#43588,#5069);
#4234=LINE('',#43592,#5070);
#4235=LINE('',#43596,#5071);
#4236=LINE('',#43600,#5072);
#4237=LINE('',#43604,#5073);
#4238=LINE('',#43608,#5074);
#4239=LINE('',#43612,#5075);
#4240=LINE('',#43616,#5076);
#4241=LINE('',#43620,#5077);
#4242=LINE('',#43624,#5078);
#4243=LINE('',#43628,#5079);
#4244=LINE('',#43632,#5080);
#4245=LINE('',#43636,#5081);
#4246=LINE('',#43640,#5082);
#4247=LINE('',#43644,#5083);
#4248=LINE('',#43648,#5084);
#4249=LINE('',#43652,#5085);
#4250=LINE('',#43656,#5086);
#4251=LINE('',#43660,#5087);
#4252=LINE('',#43674,#5088);
#4253=LINE('',#43675,#5089);
#4254=LINE('',#43678,#5090);
#4255=LINE('',#43679,#5091);
#4256=LINE('',#43683,#5092);
#4257=LINE('',#43686,#5093);
#4258=LINE('',#43687,#5094);
#4259=LINE('',#43691,#5095);
#4260=LINE('',#43694,#5096);
#4261=LINE('',#43695,#5097);
#4262=LINE('',#43699,#5098);
#4263=LINE('',#43702,#5099);
#4264=LINE('',#43703,#5100);
#4265=LINE('',#43707,#5101);
#4266=LINE('',#43710,#5102);
#4267=LINE('',#43713,#5103);
#4268=LINE('',#43716,#5104);
#4269=LINE('',#43717,#5105);
#4270=LINE('',#43721,#5106);
#4271=LINE('',#43724,#5107);
#4272=LINE('',#43727,#5108);
#4273=LINE('',#43730,#5109);
#4274=LINE('',#43731,#5110);
#4275=LINE('',#43735,#5111);
#4276=LINE('',#43740,#5112);
#4277=LINE('',#43741,#5113);
#4278=LINE('',#43744,#5114);
#4279=LINE('',#43745,#5115);
#4280=LINE('',#43749,#5116);
#4281=LINE('',#43752,#5117);
#4282=LINE('',#43753,#5118);
#4283=LINE('',#43757,#5119);
#4284=LINE('',#43760,#5120);
#4285=LINE('',#43761,#5121);
#4286=LINE('',#43765,#5122);
#4287=LINE('',#43768,#5123);
#4288=LINE('',#43769,#5124);
#4289=LINE('',#43773,#5125);
#4290=LINE('',#43776,#5126);
#4291=LINE('',#43779,#5127);
#4292=LINE('',#43782,#5128);
#4293=LINE('',#43783,#5129);
#4294=LINE('',#43787,#5130);
#4295=LINE('',#43790,#5131);
#4296=LINE('',#43793,#5132);
#4297=LINE('',#43796,#5133);
#4298=LINE('',#43797,#5134);
#4299=LINE('',#43801,#5135);
#4300=LINE('',#43806,#5136);
#4301=LINE('',#43807,#5137);
#4302=LINE('',#43810,#5138);
#4303=LINE('',#43811,#5139);
#4304=LINE('',#43815,#5140);
#4305=LINE('',#43818,#5141);
#4306=LINE('',#43819,#5142);
#4307=LINE('',#43823,#5143);
#4308=LINE('',#43826,#5144);
#4309=LINE('',#43827,#5145);
#4310=LINE('',#43831,#5146);
#4311=LINE('',#43834,#5147);
#4312=LINE('',#43835,#5148);
#4313=LINE('',#43839,#5149);
#4314=LINE('',#43842,#5150);
#4315=LINE('',#43845,#5151);
#4316=LINE('',#43848,#5152);
#4317=LINE('',#43849,#5153);
#4318=LINE('',#43853,#5154);
#4319=LINE('',#43856,#5155);
#4320=LINE('',#43859,#5156);
#4321=LINE('',#43862,#5157);
#4322=LINE('',#43863,#5158);
#4323=LINE('',#43867,#5159);
#4324=LINE('',#43872,#5160);
#4325=LINE('',#43873,#5161);
#4326=LINE('',#43876,#5162);
#4327=LINE('',#43877,#5163);
#4328=LINE('',#43881,#5164);
#4329=LINE('',#43884,#5165);
#4330=LINE('',#43885,#5166);
#4331=LINE('',#43889,#5167);
#4332=LINE('',#43892,#5168);
#4333=LINE('',#43893,#5169);
#4334=LINE('',#43897,#5170);
#4335=LINE('',#43900,#5171);
#4336=LINE('',#43901,#5172);
#4337=LINE('',#43905,#5173);
#4338=LINE('',#43908,#5174);
#4339=LINE('',#43911,#5175);
#4340=LINE('',#43914,#5176);
#4341=LINE('',#43915,#5177);
#4342=LINE('',#43919,#5178);
#4343=LINE('',#43922,#5179);
#4344=LINE('',#43926,#5180);
#4345=LINE('',#43930,#5181);
#4346=LINE('',#43933,#5182);
#4347=LINE('',#43936,#5183);
#4348=LINE('',#43940,#5184);
#4349=LINE('',#43943,#5185);
#4350=LINE('',#43945,#5186);
#4351=LINE('',#43947,#5187);
#4352=LINE('',#43949,#5188);
#4353=LINE('',#43951,#5189);
#4354=LINE('',#43953,#5190);
#4355=LINE('',#43955,#5191);
#4356=LINE('',#43957,#5192);
#4357=LINE('',#43959,#5193);
#4358=LINE('',#43961,#5194);
#4359=LINE('',#43963,#5195);
#4360=LINE('',#43965,#5196);
#4361=LINE('',#43976,#5197);
#4362=LINE('',#43979,#5198);
#4363=LINE('',#43985,#5199);
#4364=LINE('',#43991,#5200);
#4365=LINE('',#43997,#5201);
#4366=LINE('',#44003,#5202);
#4367=LINE('',#44008,#5203);
#4368=LINE('',#44010,#5204);
#4369=LINE('',#44012,#5205);
#4370=LINE('',#44013,#5206);
#4371=LINE('',#44016,#5207);
#4372=LINE('',#44018,#5208);
#4373=LINE('',#44019,#5209);
#4374=LINE('',#44022,#5210);
#4375=LINE('',#44024,#5211);
#4376=LINE('',#44025,#5212);
#4377=LINE('',#44027,#5213);
#4378=LINE('',#44028,#5214);
#4379=LINE('',#44035,#5215);
#4380=LINE('',#44062,#5216);
#4381=LINE('',#44110,#5217);
#4382=LINE('',#44158,#5218);
#4383=LINE('',#44212,#5219);
#4384=LINE('',#44260,#5220);
#4385=LINE('',#44308,#5221);
#4386=LINE('',#44362,#5222);
#4387=LINE('',#44410,#5223);
#4388=LINE('',#44458,#5224);
#4389=LINE('',#44506,#5225);
#4390=LINE('',#44560,#5226);
#4391=LINE('',#44608,#5227);
#4392=LINE('',#44656,#5228);
#4393=LINE('',#44710,#5229);
#4394=LINE('',#44758,#5230);
#4395=LINE('',#44806,#5231);
#4396=LINE('',#44860,#5232);
#4397=LINE('',#44908,#5233);
#4398=LINE('',#44956,#5234);
#4399=LINE('',#44983,#5235);
#4400=LINE('',#45008,#5236);
#4401=LINE('',#45032,#5237);
#4402=LINE('',#45057,#5238);
#4403=LINE('',#45082,#5239);
#4404=LINE('',#45106,#5240);
#4405=LINE('',#45131,#5241);
#4406=LINE('',#45156,#5242);
#4407=LINE('',#45180,#5243);
#4408=LINE('',#45205,#5244);
#4409=LINE('',#45230,#5245);
#4410=LINE('',#45254,#5246);
#4411=LINE('',#45278,#5247);
#4412=LINE('',#45303,#5248);
#4413=LINE('',#45328,#5249);
#4414=LINE('',#45352,#5250);
#4415=LINE('',#45377,#5251);
#4416=LINE('',#45402,#5252);
#4417=LINE('',#45783,#5253);
#4418=LINE('',#47101,#5254);
#4419=LINE('',#47103,#5255);
#4420=LINE('',#47105,#5256);
#4421=LINE('',#47106,#5257);
#4422=LINE('',#47109,#5258);
#4423=LINE('',#47111,#5259);
#4424=LINE('',#47112,#5260);
#4425=LINE('',#47115,#5261);
#4426=LINE('',#47117,#5262);
#4427=LINE('',#47118,#5263);
#4428=LINE('',#47121,#5264);
#4429=LINE('',#47123,#5265);
#4430=LINE('',#47124,#5266);
#4431=LINE('',#47127,#5267);
#4432=LINE('',#47129,#5268);
#4433=LINE('',#47130,#5269);
#4434=LINE('',#47132,#5270);
#4435=LINE('',#47133,#5271);
#4436=LINE('',#47140,#5272);
#4437=LINE('',#47149,#5273);
#4438=LINE('',#47157,#5274);
#4439=LINE('',#47166,#5275);
#4440=LINE('',#47183,#5276);
#4441=LINE('',#47234,#5277);
#4442=LINE('',#47285,#5278);
#4443=LINE('',#47333,#5279);
#4444=LINE('',#47384,#5280);
#4445=LINE('',#47435,#5281);
#4446=LINE('',#47483,#5282);
#4447=LINE('',#47522,#5283);
#4448=LINE('',#47546,#5284);
#4449=LINE('',#47570,#5285);
#4450=LINE('',#47595,#5286);
#4451=LINE('',#47620,#5287);
#4452=LINE('',#47644,#5288);
#4453=LINE('',#47669,#5289);
#4454=LINE('',#47694,#5290);
#4455=LINE('',#47711,#5291);
#4456=LINE('',#47720,#5292);
#4457=LINE('',#47737,#5293);
#4458=LINE('',#47788,#5294);
#4459=LINE('',#47839,#5295);
#4460=LINE('',#47887,#5296);
#4461=LINE('',#47938,#5297);
#4462=LINE('',#47989,#5298);
#4463=LINE('',#48037,#5299);
#4464=LINE('',#48076,#5300);
#4465=LINE('',#48100,#5301);
#4466=LINE('',#48124,#5302);
#4467=LINE('',#48149,#5303);
#4468=LINE('',#48174,#5304);
#4469=LINE('',#48198,#5305);
#4470=LINE('',#48223,#5306);
#4471=LINE('',#48248,#5307);
#4472=LINE('',#48265,#5308);
#4473=LINE('',#48274,#5309);
#4474=LINE('',#48291,#5310);
#4475=LINE('',#48342,#5311);
#4476=LINE('',#48393,#5312);
#4477=LINE('',#48441,#5313);
#4478=LINE('',#48492,#5314);
#4479=LINE('',#48543,#5315);
#4480=LINE('',#48591,#5316);
#4481=LINE('',#48630,#5317);
#4482=LINE('',#48654,#5318);
#4483=LINE('',#48678,#5319);
#4484=LINE('',#48703,#5320);
#4485=LINE('',#48728,#5321);
#4486=LINE('',#48752,#5322);
#4487=LINE('',#48777,#5323);
#4488=LINE('',#48802,#5324);
#4489=LINE('',#51504,#5325);
#4490=LINE('',#51513,#5326);
#4491=LINE('',#51519,#5327);
#4492=LINE('',#51525,#5328);
#4493=LINE('',#51536,#5329);
#4494=LINE('',#51541,#5330);
#4495=LINE('',#51549,#5331);
#4496=LINE('',#51576,#5332);
#4497=LINE('',#51624,#5333);
#4498=LINE('',#51672,#5334);
#4499=LINE('',#51723,#5335);
#4500=LINE('',#51771,#5336);
#4501=LINE('',#51819,#5337);
#4502=LINE('',#51867,#5338);
#4503=LINE('',#51921,#5339);
#4504=LINE('',#51969,#5340);
#4505=LINE('',#52017,#5341);
#4506=LINE('',#52071,#5342);
#4507=LINE('',#52119,#5343);
#4508=LINE('',#52167,#5344);
#4509=LINE('',#52218,#5345);
#4510=LINE('',#52269,#5346);
#4511=LINE('',#52317,#5347);
#4512=LINE('',#52365,#5348);
#4513=LINE('',#52419,#5349);
#4514=LINE('',#52467,#5350);
#4515=LINE('',#52515,#5351);
#4516=LINE('',#52569,#5352);
#4517=LINE('',#52617,#5353);
#4518=LINE('',#52665,#5354);
#4519=LINE('',#52713,#5355);
#4520=LINE('',#52767,#5356);
#4521=LINE('',#52815,#5357);
#4522=LINE('',#52863,#5358);
#4523=LINE('',#52917,#5359);
#4524=LINE('',#52965,#5360);
#4525=LINE('',#53013,#5361);
#4526=LINE('',#53067,#5362);
#4527=LINE('',#53115,#5363);
#4528=LINE('',#53163,#5364);
#4529=LINE('',#53211,#5365);
#4530=LINE('',#53265,#5366);
#4531=LINE('',#53313,#5367);
#4532=LINE('',#53361,#5368);
#4533=LINE('',#53415,#5369);
#4534=LINE('',#53463,#5370);
#4535=LINE('',#53511,#5371);
#4536=LINE('',#53565,#5372);
#4537=LINE('',#53613,#5373);
#4538=LINE('',#53661,#5374);
#4539=LINE('',#53709,#5375);
#4540=LINE('',#53763,#5376);
#4541=LINE('',#53811,#5377);
#4542=LINE('',#53859,#5378);
#4543=LINE('',#53913,#5379);
#4544=LINE('',#53961,#5380);
#4545=LINE('',#54009,#5381);
#4546=LINE('',#54063,#5382);
#4547=LINE('',#54111,#5383);
#4548=LINE('',#54159,#5384);
#4549=LINE('',#54207,#5385);
#4550=LINE('',#54261,#5386);
#4551=LINE('',#54309,#5387);
#4552=LINE('',#54357,#5388);
#4553=LINE('',#54411,#5389);
#4554=LINE('',#54459,#5390);
#4555=LINE('',#54507,#5391);
#4556=LINE('',#54525,#5392);
#4557=LINE('',#54550,#5393);
#4558=LINE('',#54574,#5394);
#4559=LINE('',#54599,#5395);
#4560=LINE('',#54624,#5396);
#4561=LINE('',#54648,#5397);
#4562=LINE('',#54673,#5398);
#4563=LINE('',#54698,#5399);
#4564=LINE('',#54722,#5400);
#4565=LINE('',#54746,#5401);
#4566=LINE('',#54771,#5402);
#4567=LINE('',#54796,#5403);
#4568=LINE('',#54820,#5404);
#4569=LINE('',#54845,#5405);
#4570=LINE('',#54870,#5406);
#4571=LINE('',#54894,#5407);
#4572=LINE('',#54919,#5408);
#4573=LINE('',#54944,#5409);
#4574=LINE('',#54968,#5410);
#4575=LINE('',#54992,#5411);
#4576=LINE('',#55017,#5412);
#4577=LINE('',#55042,#5413);
#4578=LINE('',#55066,#5414);
#4579=LINE('',#55091,#5415);
#4580=LINE('',#55116,#5416);
#4581=LINE('',#55140,#5417);
#4582=LINE('',#55165,#5418);
#4583=LINE('',#55190,#5419);
#4584=LINE('',#55214,#5420);
#4585=LINE('',#55238,#5421);
#4586=LINE('',#55263,#5422);
#4587=LINE('',#55288,#5423);
#4588=LINE('',#55312,#5424);
#4589=LINE('',#55337,#5425);
#4590=LINE('',#55362,#5426);
#4591=LINE('',#55386,#5427);
#4592=LINE('',#55411,#5428);
#4593=LINE('',#55436,#5429);
#4594=LINE('',#55460,#5430);
#4595=LINE('',#55484,#5431);
#4596=LINE('',#55509,#5432);
#4597=LINE('',#55534,#5433);
#4598=LINE('',#55558,#5434);
#4599=LINE('',#55583,#5435);
#4600=LINE('',#55608,#5436);
#4601=LINE('',#55632,#5437);
#4602=LINE('',#55657,#5438);
#4603=LINE('',#55681,#5439);
#4604=LINE('',#55706,#5440);
#4605=LINE('',#55730,#5441);
#4606=LINE('',#55755,#5442);
#4607=LINE('',#55780,#5443);
#4608=LINE('',#55804,#5444);
#4609=LINE('',#55829,#5445);
#4610=LINE('',#55854,#5446);
#4611=LINE('',#55878,#5447);
#4612=LINE('',#55903,#5448);
#4613=LINE('',#55927,#5449);
#4614=LINE('',#55952,#5450);
#4615=LINE('',#59547,#5451);
#4616=LINE('',#59549,#5452);
#4617=LINE('',#59551,#5453);
#4618=LINE('',#59553,#5454);
#4619=LINE('',#59555,#5455);
#4620=LINE('',#59556,#5456);
#4621=LINE('',#59560,#5457);
#4622=LINE('',#59562,#5458);
#4623=LINE('',#59564,#5459);
#4624=LINE('',#59566,#5460);
#4625=LINE('',#59568,#5461);
#4626=LINE('',#59569,#5462);
#4627=LINE('',#59573,#5463);
#4628=LINE('',#59574,#5464);
#4629=LINE('',#59576,#5465);
#4630=LINE('',#59578,#5466);
#4631=LINE('',#59580,#5467);
#4632=LINE('',#59582,#5468);
#4633=LINE('',#59586,#5469);
#4634=LINE('',#59596,#5470);
#4635=LINE('',#59620,#5471);
#4636=LINE('',#59671,#5472);
#4637=LINE('',#59722,#5473);
#4638=LINE('',#59770,#5474);
#4639=LINE('',#59821,#5475);
#4640=LINE('',#59872,#5476);
#4641=LINE('',#59920,#5477);
#4642=LINE('',#59962,#5478);
#4643=LINE('',#59987,#5479);
#4644=LINE('',#60011,#5480);
#4645=LINE('',#60036,#5481);
#4646=LINE('',#60061,#5482);
#4647=LINE('',#60085,#5483);
#4648=LINE('',#60110,#5484);
#4649=LINE('',#60135,#5485);
#4650=LINE('',#61107,#5486);
#4651=LINE('',#61109,#5487);
#4652=LINE('',#61111,#5488);
#4653=LINE('',#61113,#5489);
#4654=LINE('',#61115,#5490);
#4655=LINE('',#61116,#5491);
#4656=LINE('',#61121,#5492);
#4657=LINE('',#61122,#5493);
#4658=LINE('',#61123,#5494);
#4659=LINE('',#61126,#5495);
#4660=LINE('',#61127,#5496);
#4661=LINE('',#61130,#5497);
#4662=LINE('',#61131,#5498);
#4663=LINE('',#61134,#5499);
#4664=LINE('',#61135,#5500);
#4665=LINE('',#61138,#5501);
#4666=LINE('',#61139,#5502);
#4667=LINE('',#61141,#5503);
#4668=LINE('',#61148,#5504);
#4669=LINE('',#61154,#5505);
#4670=LINE('',#61162,#5506);
#4671=LINE('',#61186,#5507);
#4672=LINE('',#61234,#5508);
#4673=LINE('',#61282,#5509);
#4674=LINE('',#61336,#5510);
#4675=LINE('',#61384,#5511);
#4676=LINE('',#61432,#5512);
#4677=LINE('',#61486,#5513);
#4678=LINE('',#61534,#5514);
#4679=LINE('',#61582,#5515);
#4680=LINE('',#61636,#5516);
#4681=LINE('',#61684,#5517);
#4682=LINE('',#61732,#5518);
#4683=LINE('',#61786,#5519);
#4684=LINE('',#61834,#5520);
#4685=LINE('',#61882,#5521);
#4686=LINE('',#61907,#5522);
#4687=LINE('',#61932,#5523);
#4688=LINE('',#61956,#5524);
#4689=LINE('',#61981,#5525);
#4690=LINE('',#62006,#5526);
#4691=LINE('',#62030,#5527);
#4692=LINE('',#62055,#5528);
#4693=LINE('',#62080,#5529);
#4694=LINE('',#62104,#5530);
#4695=LINE('',#62129,#5531);
#4696=LINE('',#62154,#5532);
#4697=LINE('',#62178,#5533);
#4698=LINE('',#62203,#5534);
#4699=LINE('',#62228,#5535);
#4700=LINE('',#62570,#5536);
#4701=LINE('',#63638,#5537);
#4702=LINE('',#63640,#5538);
#4703=LINE('',#63642,#5539);
#4704=LINE('',#63643,#5540);
#4705=LINE('',#63646,#5541);
#4706=LINE('',#63648,#5542);
#4707=LINE('',#63649,#5543);
#4708=LINE('',#63652,#5544);
#4709=LINE('',#63654,#5545);
#4710=LINE('',#63655,#5546);
#4711=LINE('',#63658,#5547);
#4712=LINE('',#63660,#5548);
#4713=LINE('',#63661,#5549);
#4714=LINE('',#63664,#5550);
#4715=LINE('',#63666,#5551);
#4716=LINE('',#63667,#5552);
#4717=LINE('',#63669,#5553);
#4718=LINE('',#63670,#5554);
#4719=LINE('',#63677,#5555);
#4720=LINE('',#63686,#5556);
#4721=LINE('',#63692,#5557);
#4722=VECTOR('',#15523,10.);
#4723=VECTOR('',#15524,10.);
#4724=VECTOR('',#15525,10.);
#4725=VECTOR('',#15526,10.);
#4726=VECTOR('',#15529,10.);
#4727=VECTOR('',#15530,10.);
#4728=VECTOR('',#15531,10.);
#4729=VECTOR('',#15534,10.);
#4730=VECTOR('',#15535,10.);
#4731=VECTOR('',#15536,10.);
#4732=VECTOR('',#15539,10.);
#4733=VECTOR('',#15540,10.);
#4734=VECTOR('',#15543,10.);
#4735=VECTOR('',#15544,10.);
#4736=VECTOR('',#15545,10.);
#4737=VECTOR('',#15546,10.);
#4738=VECTOR('',#15549,10.);
#4739=VECTOR('',#15550,10.);
#4740=VECTOR('',#15551,10.);
#4741=VECTOR('',#15554,10.);
#4742=VECTOR('',#15555,10.);
#4743=VECTOR('',#15556,10.);
#4744=VECTOR('',#15559,10.);
#4745=VECTOR('',#15560,10.);
#4746=VECTOR('',#15569,10.);
#4747=VECTOR('',#15570,10.);
#4748=VECTOR('',#15571,10.);
#4749=VECTOR('',#15572,10.);
#4750=VECTOR('',#15575,10.);
#4751=VECTOR('',#15576,10.);
#4752=VECTOR('',#15577,10.);
#4753=VECTOR('',#15580,10.);
#4754=VECTOR('',#15581,10.);
#4755=VECTOR('',#15582,10.);
#4756=VECTOR('',#15585,10.);
#4757=VECTOR('',#15586,10.);
#4758=VECTOR('',#15589,10.);
#4759=VECTOR('',#15590,10.);
#4760=VECTOR('',#15591,10.);
#4761=VECTOR('',#15592,10.);
#4762=VECTOR('',#15595,10.);
#4763=VECTOR('',#15596,10.);
#4764=VECTOR('',#15597,10.);
#4765=VECTOR('',#15600,10.);
#4766=VECTOR('',#15601,10.);
#4767=VECTOR('',#15602,10.);
#4768=VECTOR('',#15605,10.);
#4769=VECTOR('',#15606,10.);
#4770=VECTOR('',#15615,4.);
#4771=VECTOR('',#15620,4.);
#4772=VECTOR('',#15623,4.);
#4773=VECTOR('',#15626,4.);
#4774=VECTOR('',#15629,4.);
#4775=VECTOR('',#15632,4.);
#4776=VECTOR('',#15635,4.);
#4777=VECTOR('',#15638,4.);
#4778=VECTOR('',#15643,4.);
#4779=VECTOR('',#15648,4.);
#4780=VECTOR('',#15651,4.);
#4781=VECTOR('',#15654,4.);
#4782=VECTOR('',#15657,4.);
#4783=VECTOR('',#15660,4.);
#4784=VECTOR('',#15663,4.);
#4785=VECTOR('',#15666,4.);
#4786=VECTOR('',#15671,4.);
#4787=VECTOR('',#15676,4.);
#4788=VECTOR('',#15679,4.);
#4789=VECTOR('',#15682,4.);
#4790=VECTOR('',#15685,4.);
#4791=VECTOR('',#15688,4.);
#4792=VECTOR('',#15691,4.);
#4793=VECTOR('',#15694,4.);
#4794=VECTOR('',#15699,4.);
#4795=VECTOR('',#15704,4.);
#4796=VECTOR('',#15707,4.);
#4797=VECTOR('',#15710,4.);
#4798=VECTOR('',#15713,4.);
#4799=VECTOR('',#15716,4.);
#4800=VECTOR('',#15719,4.);
#4801=VECTOR('',#15722,4.);
#4802=VECTOR('',#15727,4.07350000000001);
#4803=VECTOR('',#15732,4.07350000000001);
#4804=VECTOR('',#15735,4.07350000000001);
#4805=VECTOR('',#15738,4.07350000000001);
#4806=VECTOR('',#15741,4.07350000000001);
#4807=VECTOR('',#15744,4.07350000000001);
#4808=VECTOR('',#15747,4.07350000000001);
#4809=VECTOR('',#15750,4.07350000000001);
#4810=VECTOR('',#15755,4.07350000000001);
#4811=VECTOR('',#15760,4.07350000000001);
#4812=VECTOR('',#15763,4.07350000000001);
#4813=VECTOR('',#15766,4.07350000000001);
#4814=VECTOR('',#15769,4.07350000000001);
#4815=VECTOR('',#15772,4.07350000000001);
#4816=VECTOR('',#15775,4.07350000000001);
#4817=VECTOR('',#15778,4.07350000000001);
#4818=VECTOR('',#15783,4.0735);
#4819=VECTOR('',#15788,4.0735);
#4820=VECTOR('',#15791,4.0735);
#4821=VECTOR('',#15794,4.0735);
#4822=VECTOR('',#15797,4.0735);
#4823=VECTOR('',#15800,4.0735);
#4824=VECTOR('',#15803,4.0735);
#4825=VECTOR('',#15806,4.0735);
#4826=VECTOR('',#15811,4.0735);
#4827=VECTOR('',#15816,4.0735);
#4828=VECTOR('',#15819,4.0735);
#4829=VECTOR('',#15822,4.0735);
#4830=VECTOR('',#15825,4.0735);
#4831=VECTOR('',#15828,4.0735);
#4832=VECTOR('',#15831,4.0735);
#4833=VECTOR('',#15834,4.0735);
#4834=VECTOR('',#15841,10.);
#4835=VECTOR('',#15842,10.);
#4836=VECTOR('',#15843,10.);
#4837=VECTOR('',#15844,10.);
#4838=VECTOR('',#15861,10.);
#4839=VECTOR('',#15862,10.);
#4840=VECTOR('',#15863,10.);
#4841=VECTOR('',#15866,10.);
#4842=VECTOR('',#15867,10.);
#4843=VECTOR('',#15870,10.);
#4844=VECTOR('',#15871,10.);
#4845=VECTOR('',#15874,10.);
#4846=VECTOR('',#15881,4.);
#4847=VECTOR('',#15886,4.);
#4848=VECTOR('',#15889,4.);
#4849=VECTOR('',#15892,4.);
#4850=VECTOR('',#15895,4.);
#4851=VECTOR('',#15898,4.);
#4852=VECTOR('',#15901,4.);
#4853=VECTOR('',#15904,4.);
#4854=VECTOR('',#15907,4.);
#4855=VECTOR('',#15910,4.);
#4856=VECTOR('',#15913,4.);
#4857=VECTOR('',#15916,4.);
#4858=VECTOR('',#15919,4.);
#4859=VECTOR('',#15922,4.);
#4860=VECTOR('',#15925,4.);
#4861=VECTOR('',#15928,4.);
#4862=VECTOR('',#15931,4.);
#4863=VECTOR('',#15934,4.);
#4864=VECTOR('',#15937,4.);
#4865=VECTOR('',#15940,4.);
#4866=VECTOR('',#15943,4.);
#4867=VECTOR('',#15946,4.);
#4868=VECTOR('',#15949,4.);
#4869=VECTOR('',#15952,4.);
#4870=VECTOR('',#15955,3.37175);
#4871=VECTOR('',#15960,3.37175);
#4872=VECTOR('',#15963,3.37175);
#4873=VECTOR('',#15966,3.37175);
#4874=VECTOR('',#15969,3.37175);
#4875=VECTOR('',#15972,3.37175);
#4876=VECTOR('',#15975,3.37175);
#4877=VECTOR('',#15978,3.37175);
#4878=VECTOR('',#15981,3.37175);
#4879=VECTOR('',#15984,3.37175);
#4880=VECTOR('',#15987,3.37175);
#4881=VECTOR('',#15990,3.37175);
#4882=VECTOR('',#15993,3.37175);
#4883=VECTOR('',#15996,3.37175);
#4884=VECTOR('',#15999,3.37175);
#4885=VECTOR('',#16002,3.37175);
#4886=VECTOR('',#16005,3.37175);
#4887=VECTOR('',#16008,3.37175);
#4888=VECTOR('',#16011,3.37175);
#4889=VECTOR('',#16014,3.37175);
#4890=VECTOR('',#16017,3.37175);
#4891=VECTOR('',#16020,3.37175);
#4892=VECTOR('',#16023,3.37175);
#4893=VECTOR('',#16026,3.37175);
#4894=VECTOR('',#16031,3.5);
#4895=VECTOR('',#16042,10.);
#4896=VECTOR('',#16043,10.);
#4897=VECTOR('',#16044,10.);
#4898=VECTOR('',#16045,10.);
#4899=VECTOR('',#16048,10.);
#4900=VECTOR('',#16049,10.);
#4901=VECTOR('',#16050,10.);
#4902=VECTOR('',#16053,10.);
#4903=VECTOR('',#16054,10.);
#4904=VECTOR('',#16055,10.);
#4905=VECTOR('',#16058,10.);
#4906=VECTOR('',#16059,10.);
#4907=VECTOR('',#16060,10.);
#4908=VECTOR('',#16063,10.);
#4909=VECTOR('',#16064,10.);
#4910=VECTOR('',#16065,10.);
#4911=VECTOR('',#16068,10.);
#4912=VECTOR('',#16069,10.);
#4913=VECTOR('',#16078,6.5);
#4914=VECTOR('',#16091,4.5);
#4915=VECTOR('',#16098,9.);
#4916=VECTOR('',#16191,5.);
#4917=VECTOR('',#16194,5.);
#4918=VECTOR('',#16201,5.);
#4919=VECTOR('',#16204,5.);
#4920=VECTOR('',#16207,5.);
#4921=VECTOR('',#16210,5.);
#4922=VECTOR('',#16213,5.);
#4923=VECTOR('',#16216,5.);
#4924=VECTOR('',#16219,5.);
#4925=VECTOR('',#16222,5.);
#4926=VECTOR('',#16225,5.);
#4927=VECTOR('',#16228,5.);
#4928=VECTOR('',#16231,5.);
#4929=VECTOR('',#16234,5.);
#4930=VECTOR('',#16237,5.);
#4931=VECTOR('',#16240,5.);
#4932=VECTOR('',#16243,5.);
#4933=VECTOR('',#16246,5.);
#4934=VECTOR('',#16249,5.);
#4935=VECTOR('',#16252,5.);
#4936=VECTOR('',#16255,5.);
#4937=VECTOR('',#16258,5.);
#4938=VECTOR('',#16261,5.);
#4939=VECTOR('',#16264,5.);
#4940=VECTOR('',#16267,5.);
#4941=VECTOR('',#16270,5.);
#4942=VECTOR('',#16275,5.0736);
#4943=VECTOR('',#16280,5.0736);
#4944=VECTOR('',#16283,5.0736);
#4945=VECTOR('',#16286,5.0736);
#4946=VECTOR('',#16289,5.0736);
#4947=VECTOR('',#16292,5.0736);
#4948=VECTOR('',#16295,5.0736);
#4949=VECTOR('',#16298,5.0736);
#4950=VECTOR('',#16301,5.0736);
#4951=VECTOR('',#16304,5.0736);
#4952=VECTOR('',#16307,5.0736);
#4953=VECTOR('',#16310,5.0736);
#4954=VECTOR('',#16313,5.0736);
#4955=VECTOR('',#16316,5.0736);
#4956=VECTOR('',#16319,5.0736);
#4957=VECTOR('',#16322,5.0736);
#4958=VECTOR('',#16325,5.0736);
#4959=VECTOR('',#16328,5.0736);
#4960=VECTOR('',#16331,5.0736);
#4961=VECTOR('',#16334,5.0736);
#4962=VECTOR('',#16337,5.0736);
#4963=VECTOR('',#16340,5.0736);
#4964=VECTOR('',#16343,5.0736);
#4965=VECTOR('',#16346,5.0736);
#4966=VECTOR('',#16349,5.0736);
#4967=VECTOR('',#16354,5.);
#4968=VECTOR('',#16357,5.);
#4969=VECTOR('',#16364,5.);
#4970=VECTOR('',#16367,5.);
#4971=VECTOR('',#16370,5.);
#4972=VECTOR('',#16373,5.);
#4973=VECTOR('',#16376,5.);
#4974=VECTOR('',#16379,5.);
#4975=VECTOR('',#16382,5.);
#4976=VECTOR('',#16385,5.);
#4977=VECTOR('',#16388,5.);
#4978=VECTOR('',#16391,5.);
#4979=VECTOR('',#16394,5.);
#4980=VECTOR('',#16397,5.);
#4981=VECTOR('',#16400,5.);
#4982=VECTOR('',#16403,5.);
#4983=VECTOR('',#16406,5.);
#4984=VECTOR('',#16409,5.);
#4985=VECTOR('',#16412,5.);
#4986=VECTOR('',#16415,5.);
#4987=VECTOR('',#16418,5.);
#4988=VECTOR('',#16421,5.);
#4989=VECTOR('',#16424,5.);
#4990=VECTOR('',#16427,5.);
#4991=VECTOR('',#16430,5.);
#4992=VECTOR('',#16433,5.);
#4993=VECTOR('',#16436,5.);
#4994=VECTOR('',#16439,5.);
#4995=VECTOR('',#16442,5.);
#4996=VECTOR('',#16445,5.);
#4997=VECTOR('',#16448,5.);
#4998=VECTOR('',#16451,5.);
#4999=VECTOR('',#16454,5.);
#5000=VECTOR('',#16457,5.);
#5001=VECTOR('',#16460,5.);
#5002=VECTOR('',#16463,5.);
#5003=VECTOR('',#16466,5.);
#5004=VECTOR('',#16469,5.);
#5005=VECTOR('',#16472,5.);
#5006=VECTOR('',#16475,5.);
#5007=VECTOR('',#16478,5.);
#5008=VECTOR('',#16483,5.0736);
#5009=VECTOR('',#16488,5.0736);
#5010=VECTOR('',#16491,5.0736);
#5011=VECTOR('',#16494,5.0736);
#5012=VECTOR('',#16497,5.0736);
#5013=VECTOR('',#16500,5.0736);
#5014=VECTOR('',#16503,5.0736);
#5015=VECTOR('',#16506,5.0736);
#5016=VECTOR('',#16509,5.0736);
#5017=VECTOR('',#16512,5.0736);
#5018=VECTOR('',#16515,5.0736);
#5019=VECTOR('',#16518,5.0736);
#5020=VECTOR('',#16521,5.0736);
#5021=VECTOR('',#16524,5.0736);
#5022=VECTOR('',#16527,5.0736);
#5023=VECTOR('',#16530,5.0736);
#5024=VECTOR('',#16533,5.0736);
#5025=VECTOR('',#16536,5.0736);
#5026=VECTOR('',#16539,5.0736);
#5027=VECTOR('',#16542,5.0736);
#5028=VECTOR('',#16545,5.0736);
#5029=VECTOR('',#16548,5.0736);
#5030=VECTOR('',#16551,5.0736);
#5031=VECTOR('',#16554,5.0736);
#5032=VECTOR('',#16557,5.0736);
#5033=VECTOR('',#16560,5.0736);
#5034=VECTOR('',#16563,5.0736);
#5035=VECTOR('',#16566,5.0736);
#5036=VECTOR('',#16569,5.0736);
#5037=VECTOR('',#16572,5.0736);
#5038=VECTOR('',#16575,5.0736);
#5039=VECTOR('',#16578,5.0736);
#5040=VECTOR('',#16581,5.0736);
#5041=VECTOR('',#16584,5.0736);
#5042=VECTOR('',#16587,5.0736);
#5043=VECTOR('',#16590,5.0736);
#5044=VECTOR('',#16593,5.0736);
#5045=VECTOR('',#16596,5.0736);
#5046=VECTOR('',#16599,5.0736);
#5047=VECTOR('',#16602,5.0736);
#5048=VECTOR('',#16629,10.);
#5049=VECTOR('',#16632,10.);
#5050=VECTOR('',#16635,10.);
#5051=VECTOR('',#16636,10.);
#5052=VECTOR('',#16637,10.);
#5053=VECTOR('',#16640,10.);
#5054=VECTOR('',#16643,10.);
#5055=VECTOR('',#16646,10.);
#5056=VECTOR('',#16649,10.);
#5057=VECTOR('',#16652,10.);
#5058=VECTOR('',#16655,10.);
#5059=VECTOR('',#16658,10.);
#5060=VECTOR('',#16661,10.);
#5061=VECTOR('',#16664,10.);
#5062=VECTOR('',#16667,10.);
#5063=VECTOR('',#16670,10.);
#5064=VECTOR('',#16673,10.);
#5065=VECTOR('',#16676,10.);
#5066=VECTOR('',#16679,10.);
#5067=VECTOR('',#16682,10.);
#5068=VECTOR('',#16685,10.);
#5069=VECTOR('',#16688,10.);
#5070=VECTOR('',#16691,10.);
#5071=VECTOR('',#16694,10.);
#5072=VECTOR('',#16697,10.);
#5073=VECTOR('',#16700,10.);
#5074=VECTOR('',#16703,10.);
#5075=VECTOR('',#16706,10.);
#5076=VECTOR('',#16709,10.);
#5077=VECTOR('',#16712,10.);
#5078=VECTOR('',#16715,10.);
#5079=VECTOR('',#16718,10.);
#5080=VECTOR('',#16721,10.);
#5081=VECTOR('',#16724,10.);
#5082=VECTOR('',#16727,10.);
#5083=VECTOR('',#16730,10.);
#5084=VECTOR('',#16733,10.);
#5085=VECTOR('',#16736,10.);
#5086=VECTOR('',#16739,10.);
#5087=VECTOR('',#16742,10.);
#5088=VECTOR('',#16757,10.);
#5089=VECTOR('',#16758,10.);
#5090=VECTOR('',#16761,10.);
#5091=VECTOR('',#16762,10.);
#5092=VECTOR('',#16767,10.);
#5093=VECTOR('',#16770,10.);
#5094=VECTOR('',#16771,10.);
#5095=VECTOR('',#16776,10.);
#5096=VECTOR('',#16779,10.);
#5097=VECTOR('',#16780,10.);
#5098=VECTOR('',#16785,10.);
#5099=VECTOR('',#16788,10.);
#5100=VECTOR('',#16789,10.);
#5101=VECTOR('',#16794,10.);
#5102=VECTOR('',#16797,10.);
#5103=VECTOR('',#16800,10.);
#5104=VECTOR('',#16803,10.);
#5105=VECTOR('',#16804,10.);
#5106=VECTOR('',#16809,10.);
#5107=VECTOR('',#16812,10.);
#5108=VECTOR('',#16815,10.);
#5109=VECTOR('',#16818,10.);
#5110=VECTOR('',#16819,10.);
#5111=VECTOR('',#16824,10.);
#5112=VECTOR('',#16829,10.);
#5113=VECTOR('',#16830,10.);
#5114=VECTOR('',#16833,10.);
#5115=VECTOR('',#16834,10.);
#5116=VECTOR('',#16839,10.);
#5117=VECTOR('',#16842,10.);
#5118=VECTOR('',#16843,10.);
#5119=VECTOR('',#16848,10.);
#5120=VECTOR('',#16851,10.);
#5121=VECTOR('',#16852,10.);
#5122=VECTOR('',#16857,10.);
#5123=VECTOR('',#16860,10.);
#5124=VECTOR('',#16861,10.);
#5125=VECTOR('',#16866,10.);
#5126=VECTOR('',#16869,10.);
#5127=VECTOR('',#16872,10.);
#5128=VECTOR('',#16875,10.);
#5129=VECTOR('',#16876,10.);
#5130=VECTOR('',#16881,10.);
#5131=VECTOR('',#16884,10.);
#5132=VECTOR('',#16887,10.);
#5133=VECTOR('',#16890,10.);
#5134=VECTOR('',#16891,10.);
#5135=VECTOR('',#16896,10.);
#5136=VECTOR('',#16901,10.);
#5137=VECTOR('',#16902,10.);
#5138=VECTOR('',#16905,10.);
#5139=VECTOR('',#16906,10.);
#5140=VECTOR('',#16911,10.);
#5141=VECTOR('',#16914,10.);
#5142=VECTOR('',#16915,10.);
#5143=VECTOR('',#16920,10.);
#5144=VECTOR('',#16923,10.);
#5145=VECTOR('',#16924,10.);
#5146=VECTOR('',#16929,10.);
#5147=VECTOR('',#16932,10.);
#5148=VECTOR('',#16933,10.);
#5149=VECTOR('',#16938,10.);
#5150=VECTOR('',#16941,10.);
#5151=VECTOR('',#16944,10.);
#5152=VECTOR('',#16947,10.);
#5153=VECTOR('',#16948,10.);
#5154=VECTOR('',#16953,10.);
#5155=VECTOR('',#16956,10.);
#5156=VECTOR('',#16959,10.);
#5157=VECTOR('',#16962,10.);
#5158=VECTOR('',#16963,10.);
#5159=VECTOR('',#16968,10.);
#5160=VECTOR('',#16973,10.);
#5161=VECTOR('',#16974,10.);
#5162=VECTOR('',#16977,10.);
#5163=VECTOR('',#16978,10.);
#5164=VECTOR('',#16983,10.);
#5165=VECTOR('',#16986,10.);
#5166=VECTOR('',#16987,10.);
#5167=VECTOR('',#16992,10.);
#5168=VECTOR('',#16995,10.);
#5169=VECTOR('',#16996,10.);
#5170=VECTOR('',#17001,10.);
#5171=VECTOR('',#17004,10.);
#5172=VECTOR('',#17005,10.);
#5173=VECTOR('',#17010,10.);
#5174=VECTOR('',#17013,10.);
#5175=VECTOR('',#17016,10.);
#5176=VECTOR('',#17019,10.);
#5177=VECTOR('',#17020,10.);
#5178=VECTOR('',#17025,10.);
#5179=VECTOR('',#17028,10.);
#5180=VECTOR('',#17033,3.);
#5181=VECTOR('',#17038,3.);
#5182=VECTOR('',#17043,4.);
#5183=VECTOR('',#17046,3.);
#5184=VECTOR('',#17051,3.);
#5185=VECTOR('',#17056,10.);
#5186=VECTOR('',#17059,10.);
#5187=VECTOR('',#17062,10.);
#5188=VECTOR('',#17065,10.);
#5189=VECTOR('',#17068,10.);
#5190=VECTOR('',#17071,10.);
#5191=VECTOR('',#17074,10.);
#5192=VECTOR('',#17077,10.);
#5193=VECTOR('',#17080,10.);
#5194=VECTOR('',#17083,10.);
#5195=VECTOR('',#17086,10.);
#5196=VECTOR('',#17089,10.);
#5197=VECTOR('',#17104,8.5);
#5198=VECTOR('',#17107,5.5);
#5199=VECTOR('',#17114,4.5);
#5200=VECTOR('',#17121,4.5);
#5201=VECTOR('',#17128,4.5);
#5202=VECTOR('',#17135,4.5);
#5203=VECTOR('',#17140,10.);
#5204=VECTOR('',#17141,10.);
#5205=VECTOR('',#17142,10.);
#5206=VECTOR('',#17143,10.);
#5207=VECTOR('',#17146,10.);
#5208=VECTOR('',#17147,10.);
#5209=VECTOR('',#17148,10.);
#5210=VECTOR('',#17151,10.);
#5211=VECTOR('',#17152,10.);
#5212=VECTOR('',#17153,10.);
#5213=VECTOR('',#17156,10.);
#5214=VECTOR('',#17157,10.);
#5215=VECTOR('',#17166,5.);
#5216=VECTOR('',#17171,5.);
#5217=VECTOR('',#17174,5.);
#5218=VECTOR('',#17177,5.);
#5219=VECTOR('',#17180,5.);
#5220=VECTOR('',#17183,5.);
#5221=VECTOR('',#17186,5.);
#5222=VECTOR('',#17189,5.);
#5223=VECTOR('',#17192,5.);
#5224=VECTOR('',#17195,5.);
#5225=VECTOR('',#17198,5.);
#5226=VECTOR('',#17201,5.);
#5227=VECTOR('',#17204,5.);
#5228=VECTOR('',#17207,5.);
#5229=VECTOR('',#17210,5.);
#5230=VECTOR('',#17213,5.);
#5231=VECTOR('',#17216,5.);
#5232=VECTOR('',#17219,5.);
#5233=VECTOR('',#17222,5.);
#5234=VECTOR('',#17225,4.372);
#5235=VECTOR('',#17230,4.372);
#5236=VECTOR('',#17233,4.372);
#5237=VECTOR('',#17236,4.372);
#5238=VECTOR('',#17239,4.372);
#5239=VECTOR('',#17242,4.372);
#5240=VECTOR('',#17245,4.372);
#5241=VECTOR('',#17248,4.372);
#5242=VECTOR('',#17251,4.372);
#5243=VECTOR('',#17254,4.372);
#5244=VECTOR('',#17257,4.372);
#5245=VECTOR('',#17260,4.372);
#5246=VECTOR('',#17263,4.372);
#5247=VECTOR('',#17266,4.372);
#5248=VECTOR('',#17269,4.372);
#5249=VECTOR('',#17272,4.372);
#5250=VECTOR('',#17275,4.372);
#5251=VECTOR('',#17278,4.372);
#5252=VECTOR('',#17281,4.372);
#5253=VECTOR('',#17286,4.5);
#5254=VECTOR('',#17297,10.);
#5255=VECTOR('',#17298,10.);
#5256=VECTOR('',#17299,10.);
#5257=VECTOR('',#17300,10.);
#5258=VECTOR('',#17303,10.);
#5259=VECTOR('',#17304,10.);
#5260=VECTOR('',#17305,10.);
#5261=VECTOR('',#17308,10.);
#5262=VECTOR('',#17309,10.);
#5263=VECTOR('',#17310,10.);
#5264=VECTOR('',#17313,10.);
#5265=VECTOR('',#17314,10.);
#5266=VECTOR('',#17315,10.);
#5267=VECTOR('',#17318,10.);
#5268=VECTOR('',#17319,10.);
#5269=VECTOR('',#17320,10.);
#5270=VECTOR('',#17323,10.);
#5271=VECTOR('',#17324,10.);
#5272=VECTOR('',#17333,8.);
#5273=VECTOR('',#17346,30.);
#5274=VECTOR('',#17357,3.);
#5275=VECTOR('',#17360,3.);
#5276=VECTOR('',#17367,3.);
#5277=VECTOR('',#17370,3.);
#5278=VECTOR('',#17373,3.);
#5279=VECTOR('',#17376,3.);
#5280=VECTOR('',#17379,3.);
#5281=VECTOR('',#17382,3.);
#5282=VECTOR('',#17385,3.);
#5283=VECTOR('',#17390,3.0735);
#5284=VECTOR('',#17395,3.0735);
#5285=VECTOR('',#17398,3.0735);
#5286=VECTOR('',#17401,3.0735);
#5287=VECTOR('',#17404,3.0735);
#5288=VECTOR('',#17407,3.0735);
#5289=VECTOR('',#17410,3.0735);
#5290=VECTOR('',#17413,3.0735);
#5291=VECTOR('',#17418,3.);
#5292=VECTOR('',#17421,3.);
#5293=VECTOR('',#17428,3.);
#5294=VECTOR('',#17431,3.);
#5295=VECTOR('',#17434,3.);
#5296=VECTOR('',#17437,3.);
#5297=VECTOR('',#17440,3.);
#5298=VECTOR('',#17443,3.);
#5299=VECTOR('',#17446,3.);
#5300=VECTOR('',#17451,3.0735);
#5301=VECTOR('',#17456,3.0735);
#5302=VECTOR('',#17459,3.0735);
#5303=VECTOR('',#17462,3.0735);
#5304=VECTOR('',#17465,3.0735);
#5305=VECTOR('',#17468,3.0735);
#5306=VECTOR('',#17471,3.0735);
#5307=VECTOR('',#17474,3.0735);
#5308=VECTOR('',#17479,3.);
#5309=VECTOR('',#17482,3.);
#5310=VECTOR('',#17489,3.);
#5311=VECTOR('',#17492,3.);
#5312=VECTOR('',#17495,3.);
#5313=VECTOR('',#17498,3.);
#5314=VECTOR('',#17501,3.);
#5315=VECTOR('',#17504,3.);
#5316=VECTOR('',#17507,3.);
#5317=VECTOR('',#17512,3.0735);
#5318=VECTOR('',#17517,3.0735);
#5319=VECTOR('',#17520,3.0735);
#5320=VECTOR('',#17523,3.0735);
#5321=VECTOR('',#17526,3.0735);
#5322=VECTOR('',#17529,3.0735);
#5323=VECTOR('',#17532,3.0735);
#5324=VECTOR('',#17535,3.0735);
#5325=VECTOR('',#17572,30.);
#5326=VECTOR('',#17585,3.5);
#5327=VECTOR('',#17592,3.5);
#5328=VECTOR('',#17599,3.5);
#5329=VECTOR('',#17614,5.5);
#5330=VECTOR('',#17619,22.);
#5331=VECTOR('',#17630,5.);
#5332=VECTOR('',#17635,5.);
#5333=VECTOR('',#17638,5.);
#5334=VECTOR('',#17641,5.);
#5335=VECTOR('',#17644,5.);
#5336=VECTOR('',#17647,5.);
#5337=VECTOR('',#17650,5.);
#5338=VECTOR('',#17653,5.);
#5339=VECTOR('',#17656,5.);
#5340=VECTOR('',#17659,5.);
#5341=VECTOR('',#17662,5.);
#5342=VECTOR('',#17665,5.);
#5343=VECTOR('',#17668,5.);
#5344=VECTOR('',#17671,5.);
#5345=VECTOR('',#17674,5.);
#5346=VECTOR('',#17677,5.);
#5347=VECTOR('',#17680,5.);
#5348=VECTOR('',#17683,5.);
#5349=VECTOR('',#17686,5.);
#5350=VECTOR('',#17689,5.);
#5351=VECTOR('',#17692,5.);
#5352=VECTOR('',#17695,5.);
#5353=VECTOR('',#17698,5.);
#5354=VECTOR('',#17701,5.);
#5355=VECTOR('',#17704,5.);
#5356=VECTOR('',#17707,5.);
#5357=VECTOR('',#17710,5.);
#5358=VECTOR('',#17713,5.);
#5359=VECTOR('',#17716,5.);
#5360=VECTOR('',#17719,5.);
#5361=VECTOR('',#17722,5.);
#5362=VECTOR('',#17725,5.);
#5363=VECTOR('',#17728,5.);
#5364=VECTOR('',#17731,5.);
#5365=VECTOR('',#17734,5.);
#5366=VECTOR('',#17737,5.);
#5367=VECTOR('',#17740,5.);
#5368=VECTOR('',#17743,5.);
#5369=VECTOR('',#17746,5.);
#5370=VECTOR('',#17749,5.);
#5371=VECTOR('',#17752,5.);
#5372=VECTOR('',#17755,5.);
#5373=VECTOR('',#17758,5.);
#5374=VECTOR('',#17761,5.);
#5375=VECTOR('',#17764,5.);
#5376=VECTOR('',#17767,5.);
#5377=VECTOR('',#17770,5.);
#5378=VECTOR('',#17773,5.);
#5379=VECTOR('',#17776,5.);
#5380=VECTOR('',#17779,5.);
#5381=VECTOR('',#17782,5.);
#5382=VECTOR('',#17785,5.);
#5383=VECTOR('',#17788,5.);
#5384=VECTOR('',#17791,5.);
#5385=VECTOR('',#17794,5.);
#5386=VECTOR('',#17797,5.);
#5387=VECTOR('',#17800,5.);
#5388=VECTOR('',#17803,5.);
#5389=VECTOR('',#17806,5.);
#5390=VECTOR('',#17809,5.);
#5391=VECTOR('',#17812,4.372);
#5392=VECTOR('',#17817,4.372);
#5393=VECTOR('',#17820,4.372);
#5394=VECTOR('',#17823,4.372);
#5395=VECTOR('',#17826,4.372);
#5396=VECTOR('',#17829,4.372);
#5397=VECTOR('',#17832,4.372);
#5398=VECTOR('',#17835,4.372);
#5399=VECTOR('',#17838,4.372);
#5400=VECTOR('',#17841,4.372);
#5401=VECTOR('',#17844,4.372);
#5402=VECTOR('',#17847,4.372);
#5403=VECTOR('',#17850,4.372);
#5404=VECTOR('',#17853,4.372);
#5405=VECTOR('',#17856,4.372);
#5406=VECTOR('',#17859,4.372);
#5407=VECTOR('',#17862,4.372);
#5408=VECTOR('',#17865,4.372);
#5409=VECTOR('',#17868,4.372);
#5410=VECTOR('',#17871,4.372);
#5411=VECTOR('',#17874,4.372);
#5412=VECTOR('',#17877,4.372);
#5413=VECTOR('',#17880,4.372);
#5414=VECTOR('',#17883,4.372);
#5415=VECTOR('',#17886,4.372);
#5416=VECTOR('',#17889,4.372);
#5417=VECTOR('',#17892,4.372);
#5418=VECTOR('',#17895,4.372);
#5419=VECTOR('',#17898,4.372);
#5420=VECTOR('',#17901,4.372);
#5421=VECTOR('',#17904,4.372);
#5422=VECTOR('',#17907,4.372);
#5423=VECTOR('',#17910,4.372);
#5424=VECTOR('',#17913,4.372);
#5425=VECTOR('',#17916,4.372);
#5426=VECTOR('',#17919,4.372);
#5427=VECTOR('',#17922,4.372);
#5428=VECTOR('',#17925,4.372);
#5429=VECTOR('',#17928,4.372);
#5430=VECTOR('',#17931,4.372);
#5431=VECTOR('',#17934,4.372);
#5432=VECTOR('',#17937,4.372);
#5433=VECTOR('',#17940,4.372);
#5434=VECTOR('',#17943,4.372);
#5435=VECTOR('',#17946,4.372);
#5436=VECTOR('',#17949,4.372);
#5437=VECTOR('',#17952,4.372);
#5438=VECTOR('',#17955,4.372);
#5439=VECTOR('',#17958,4.372);
#5440=VECTOR('',#17961,4.372);
#5441=VECTOR('',#17964,4.372);
#5442=VECTOR('',#17967,4.372);
#5443=VECTOR('',#17970,4.372);
#5444=VECTOR('',#17973,4.372);
#5445=VECTOR('',#17976,4.372);
#5446=VECTOR('',#17979,4.372);
#5447=VECTOR('',#17982,4.372);
#5448=VECTOR('',#17985,4.372);
#5449=VECTOR('',#17988,4.372);
#5450=VECTOR('',#17991,4.372);
#5451=VECTOR('',#18002,10.);
#5452=VECTOR('',#18003,10.);
#5453=VECTOR('',#18004,10.);
#5454=VECTOR('',#18005,10.);
#5455=VECTOR('',#18006,10.);
#5456=VECTOR('',#18007,10.);
#5457=VECTOR('',#18010,10.);
#5458=VECTOR('',#18011,10.);
#5459=VECTOR('',#18012,10.);
#5460=VECTOR('',#18013,10.);
#5461=VECTOR('',#18014,10.);
#5462=VECTOR('',#18015,10.);
#5463=VECTOR('',#18020,10.);
#5464=VECTOR('',#18021,10.);
#5465=VECTOR('',#18024,10.);
#5466=VECTOR('',#18027,10.);
#5467=VECTOR('',#18030,10.);
#5468=VECTOR('',#18033,10.);
#5469=VECTOR('',#18038,5.);
#5470=VECTOR('',#18051,5.);
#5471=VECTOR('',#18056,5.);
#5472=VECTOR('',#18059,5.);
#5473=VECTOR('',#18062,5.);
#5474=VECTOR('',#18065,5.);
#5475=VECTOR('',#18068,5.);
#5476=VECTOR('',#18071,5.);
#5477=VECTOR('',#18074,5.);
#5478=VECTOR('',#18079,5.0736);
#5479=VECTOR('',#18084,5.0736);
#5480=VECTOR('',#18087,5.0736);
#5481=VECTOR('',#18090,5.0736);
#5482=VECTOR('',#18093,5.0736);
#5483=VECTOR('',#18096,5.0736);
#5484=VECTOR('',#18099,5.0736);
#5485=VECTOR('',#18102,5.0736);
#5486=VECTOR('',#18109,10.);
#5487=VECTOR('',#18110,10.);
#5488=VECTOR('',#18111,10.);
#5489=VECTOR('',#18112,10.);
#5490=VECTOR('',#18113,10.);
#5491=VECTOR('',#18114,10.);
#5492=VECTOR('',#18119,10.);
#5493=VECTOR('',#18120,10.);
#5494=VECTOR('',#18121,10.);
#5495=VECTOR('',#18124,10.);
#5496=VECTOR('',#18125,10.);
#5497=VECTOR('',#18128,10.);
#5498=VECTOR('',#18129,10.);
#5499=VECTOR('',#18132,10.);
#5500=VECTOR('',#18133,10.);
#5501=VECTOR('',#18136,10.);
#5502=VECTOR('',#18137,10.);
#5503=VECTOR('',#18140,10.);
#5504=VECTOR('',#18149,5.5);
#5505=VECTOR('',#18156,11.);
#5506=VECTOR('',#18167,3.);
#5507=VECTOR('',#18172,3.);
#5508=VECTOR('',#18175,3.);
#5509=VECTOR('',#18178,3.);
#5510=VECTOR('',#18181,3.);
#5511=VECTOR('',#18184,3.);
#5512=VECTOR('',#18187,3.);
#5513=VECTOR('',#18190,3.);
#5514=VECTOR('',#18193,3.);
#5515=VECTOR('',#18196,3.);
#5516=VECTOR('',#18199,3.);
#5517=VECTOR('',#18202,3.);
#5518=VECTOR('',#18205,3.);
#5519=VECTOR('',#18208,3.);
#5520=VECTOR('',#18211,3.);
#5521=VECTOR('',#18214,2.37175);
#5522=VECTOR('',#18219,2.37175);
#5523=VECTOR('',#18222,2.37175);
#5524=VECTOR('',#18225,2.37175);
#5525=VECTOR('',#18228,2.37175);
#5526=VECTOR('',#18231,2.37175);
#5527=VECTOR('',#18234,2.37175);
#5528=VECTOR('',#18237,2.37175);
#5529=VECTOR('',#18240,2.37175);
#5530=VECTOR('',#18243,2.37175);
#5531=VECTOR('',#18246,2.37175);
#5532=VECTOR('',#18249,2.37175);
#5533=VECTOR('',#18252,2.37175);
#5534=VECTOR('',#18255,2.37175);
#5535=VECTOR('',#18258,2.37175);
#5536=VECTOR('',#18263,2.5);
#5537=VECTOR('',#18274,10.);
#5538=VECTOR('',#18275,10.);
#5539=VECTOR('',#18276,10.);
#5540=VECTOR('',#18277,10.);
#5541=VECTOR('',#18280,10.);
#5542=VECTOR('',#18281,10.);
#5543=VECTOR('',#18282,10.);
#5544=VECTOR('',#18285,10.);
#5545=VECTOR('',#18286,10.);
#5546=VECTOR('',#18287,10.);
#5547=VECTOR('',#18290,10.);
#5548=VECTOR('',#18291,10.);
#5549=VECTOR('',#18292,10.);
#5550=VECTOR('',#18295,10.);
#5551=VECTOR('',#18296,10.);
#5552=VECTOR('',#18297,10.);
#5553=VECTOR('',#18300,10.);
#5554=VECTOR('',#18301,10.);
#5555=VECTOR('',#18310,5.);
#5556=VECTOR('',#18323,3.5);
#5557=VECTOR('',#18330,7.);
#5558=VERTEX_POINT('',#18381);
#5559=VERTEX_POINT('',#18382);
#5560=VERTEX_POINT('',#18384);
#5561=VERTEX_POINT('',#18386);
#5562=VERTEX_POINT('',#18390);
#5563=VERTEX_POINT('',#18392);
#5564=VERTEX_POINT('',#18396);
#5565=VERTEX_POINT('',#18398);
#5566=VERTEX_POINT('',#18405);
#5567=VERTEX_POINT('',#18406);
#5568=VERTEX_POINT('',#18408);
#5569=VERTEX_POINT('',#18410);
#5570=VERTEX_POINT('',#18414);
#5571=VERTEX_POINT('',#18416);
#5572=VERTEX_POINT('',#18420);
#5573=VERTEX_POINT('',#18422);
#5574=VERTEX_POINT('',#18432);
#5575=VERTEX_POINT('',#18433);
#5576=VERTEX_POINT('',#18435);
#5577=VERTEX_POINT('',#18437);
#5578=VERTEX_POINT('',#18441);
#5579=VERTEX_POINT('',#18443);
#5580=VERTEX_POINT('',#18447);
#5581=VERTEX_POINT('',#18449);
#5582=VERTEX_POINT('',#18456);
#5583=VERTEX_POINT('',#18457);
#5584=VERTEX_POINT('',#18459);
#5585=VERTEX_POINT('',#18461);
#5586=VERTEX_POINT('',#18465);
#5587=VERTEX_POINT('',#18467);
#5588=VERTEX_POINT('',#18471);
#5589=VERTEX_POINT('',#18473);
#5590=VERTEX_POINT('',#18483);
#5591=VERTEX_POINT('',#18484);
#5592=VERTEX_POINT('',#18486);
#5593=VERTEX_POINT('',#18491);
#5594=VERTEX_POINT('',#18504);
#5595=VERTEX_POINT('',#18505);
#5596=VERTEX_POINT('',#18555);
#5597=VERTEX_POINT('',#18556);
#5598=VERTEX_POINT('',#18606);
#5599=VERTEX_POINT('',#18607);
#5600=VERTEX_POINT('',#18654);
#5601=VERTEX_POINT('',#18655);
#5602=VERTEX_POINT('',#18705);
#5603=VERTEX_POINT('',#18706);
#5604=VERTEX_POINT('',#18756);
#5605=VERTEX_POINT('',#18757);
#5606=VERTEX_POINT('',#18804);
#5607=VERTEX_POINT('',#18805);
#5608=VERTEX_POINT('',#18807);
#5609=VERTEX_POINT('',#18821);
#5610=VERTEX_POINT('',#18843);
#5611=VERTEX_POINT('',#18844);
#5612=VERTEX_POINT('',#18846);
#5613=VERTEX_POINT('',#18851);
#5614=VERTEX_POINT('',#18864);
#5615=VERTEX_POINT('',#18865);
#5616=VERTEX_POINT('',#18915);
#5617=VERTEX_POINT('',#18916);
#5618=VERTEX_POINT('',#18966);
#5619=VERTEX_POINT('',#18967);
#5620=VERTEX_POINT('',#19014);
#5621=VERTEX_POINT('',#19015);
#5622=VERTEX_POINT('',#19065);
#5623=VERTEX_POINT('',#19066);
#5624=VERTEX_POINT('',#19116);
#5625=VERTEX_POINT('',#19117);
#5626=VERTEX_POINT('',#19164);
#5627=VERTEX_POINT('',#19165);
#5628=VERTEX_POINT('',#19167);
#5629=VERTEX_POINT('',#19181);
#5630=VERTEX_POINT('',#19203);
#5631=VERTEX_POINT('',#19204);
#5632=VERTEX_POINT('',#19206);
#5633=VERTEX_POINT('',#19211);
#5634=VERTEX_POINT('',#19224);
#5635=VERTEX_POINT('',#19225);
#5636=VERTEX_POINT('',#19275);
#5637=VERTEX_POINT('',#19276);
#5638=VERTEX_POINT('',#19326);
#5639=VERTEX_POINT('',#19327);
#5640=VERTEX_POINT('',#19374);
#5641=VERTEX_POINT('',#19375);
#5642=VERTEX_POINT('',#19425);
#5643=VERTEX_POINT('',#19426);
#5644=VERTEX_POINT('',#19476);
#5645=VERTEX_POINT('',#19477);
#5646=VERTEX_POINT('',#19524);
#5647=VERTEX_POINT('',#19525);
#5648=VERTEX_POINT('',#19527);
#5649=VERTEX_POINT('',#19541);
#5650=VERTEX_POINT('',#19563);
#5651=VERTEX_POINT('',#19564);
#5652=VERTEX_POINT('',#19566);
#5653=VERTEX_POINT('',#19571);
#5654=VERTEX_POINT('',#19584);
#5655=VERTEX_POINT('',#19585);
#5656=VERTEX_POINT('',#19635);
#5657=VERTEX_POINT('',#19636);
#5658=VERTEX_POINT('',#19686);
#5659=VERTEX_POINT('',#19687);
#5660=VERTEX_POINT('',#19734);
#5661=VERTEX_POINT('',#19735);
#5662=VERTEX_POINT('',#19785);
#5663=VERTEX_POINT('',#19786);
#5664=VERTEX_POINT('',#19836);
#5665=VERTEX_POINT('',#19837);
#5666=VERTEX_POINT('',#19884);
#5667=VERTEX_POINT('',#19885);
#5668=VERTEX_POINT('',#19887);
#5669=VERTEX_POINT('',#19901);
#5670=VERTEX_POINT('',#19923);
#5671=VERTEX_POINT('',#19924);
#5672=VERTEX_POINT('',#19926);
#5673=VERTEX_POINT('',#19935);
#5674=VERTEX_POINT('',#19947);
#5675=VERTEX_POINT('',#19948);
#5676=VERTEX_POINT('',#19971);
#5677=VERTEX_POINT('',#19972);
#5678=VERTEX_POINT('',#19996);
#5679=VERTEX_POINT('',#19997);
#5680=VERTEX_POINT('',#20021);
#5681=VERTEX_POINT('',#20022);
#5682=VERTEX_POINT('',#20045);
#5683=VERTEX_POINT('',#20046);
#5684=VERTEX_POINT('',#20070);
#5685=VERTEX_POINT('',#20071);
#5686=VERTEX_POINT('',#20095);
#5687=VERTEX_POINT('',#20096);
#5688=VERTEX_POINT('',#20098);
#5689=VERTEX_POINT('',#20104);
#5690=VERTEX_POINT('',#20112);
#5691=VERTEX_POINT('',#20113);
#5692=VERTEX_POINT('',#20115);
#5693=VERTEX_POINT('',#20124);
#5694=VERTEX_POINT('',#20136);
#5695=VERTEX_POINT('',#20137);
#5696=VERTEX_POINT('',#20160);
#5697=VERTEX_POINT('',#20161);
#5698=VERTEX_POINT('',#20185);
#5699=VERTEX_POINT('',#20186);
#5700=VERTEX_POINT('',#20210);
#5701=VERTEX_POINT('',#20211);
#5702=VERTEX_POINT('',#20234);
#5703=VERTEX_POINT('',#20235);
#5704=VERTEX_POINT('',#20259);
#5705=VERTEX_POINT('',#20260);
#5706=VERTEX_POINT('',#20284);
#5707=VERTEX_POINT('',#20285);
#5708=VERTEX_POINT('',#20287);
#5709=VERTEX_POINT('',#20293);
#5710=VERTEX_POINT('',#20301);
#5711=VERTEX_POINT('',#20302);
#5712=VERTEX_POINT('',#20304);
#5713=VERTEX_POINT('',#20313);
#5714=VERTEX_POINT('',#20325);
#5715=VERTEX_POINT('',#20326);
#5716=VERTEX_POINT('',#20349);
#5717=VERTEX_POINT('',#20350);
#5718=VERTEX_POINT('',#20374);
#5719=VERTEX_POINT('',#20375);
#5720=VERTEX_POINT('',#20399);
#5721=VERTEX_POINT('',#20400);
#5722=VERTEX_POINT('',#20423);
#5723=VERTEX_POINT('',#20424);
#5724=VERTEX_POINT('',#20448);
#5725=VERTEX_POINT('',#20449);
#5726=VERTEX_POINT('',#20473);
#5727=VERTEX_POINT('',#20474);
#5728=VERTEX_POINT('',#20476);
#5729=VERTEX_POINT('',#20482);
#5730=VERTEX_POINT('',#20490);
#5731=VERTEX_POINT('',#20491);
#5732=VERTEX_POINT('',#20493);
#5733=VERTEX_POINT('',#20502);
#5734=VERTEX_POINT('',#20514);
#5735=VERTEX_POINT('',#20515);
#5736=VERTEX_POINT('',#20538);
#5737=VERTEX_POINT('',#20539);
#5738=VERTEX_POINT('',#20563);
#5739=VERTEX_POINT('',#20564);
#5740=VERTEX_POINT('',#20588);
#5741=VERTEX_POINT('',#20589);
#5742=VERTEX_POINT('',#20612);
#5743=VERTEX_POINT('',#20613);
#5744=VERTEX_POINT('',#20637);
#5745=VERTEX_POINT('',#20638);
#5746=VERTEX_POINT('',#20662);
#5747=VERTEX_POINT('',#20663);
#5748=VERTEX_POINT('',#20665);
#5749=VERTEX_POINT('',#20671);
#5750=VERTEX_POINT('',#21581);
#5751=VERTEX_POINT('',#21582);
#5752=VERTEX_POINT('',#21584);
#5753=VERTEX_POINT('',#21586);
#5754=VERTEX_POINT('',#24300);
#5755=VERTEX_POINT('',#24301);
#5756=VERTEX_POINT('',#24306);
#5757=VERTEX_POINT('',#24310);
#5758=VERTEX_POINT('',#24318);
#5759=VERTEX_POINT('',#24319);
#5760=VERTEX_POINT('',#24321);
#5761=VERTEX_POINT('',#24332);
#5762=VERTEX_POINT('',#24342);
#5763=VERTEX_POINT('',#24343);
#5764=VERTEX_POINT('',#24390);
#5765=VERTEX_POINT('',#24391);
#5766=VERTEX_POINT('',#24438);
#5767=VERTEX_POINT('',#24439);
#5768=VERTEX_POINT('',#24486);
#5769=VERTEX_POINT('',#24487);
#5770=VERTEX_POINT('',#24540);
#5771=VERTEX_POINT('',#24541);
#5772=VERTEX_POINT('',#24588);
#5773=VERTEX_POINT('',#24589);
#5774=VERTEX_POINT('',#24636);
#5775=VERTEX_POINT('',#24637);
#5776=VERTEX_POINT('',#24690);
#5777=VERTEX_POINT('',#24691);
#5778=VERTEX_POINT('',#24738);
#5779=VERTEX_POINT('',#24739);
#5780=VERTEX_POINT('',#24786);
#5781=VERTEX_POINT('',#24787);
#5782=VERTEX_POINT('',#24840);
#5783=VERTEX_POINT('',#24841);
#5784=VERTEX_POINT('',#24888);
#5785=VERTEX_POINT('',#24889);
#5786=VERTEX_POINT('',#24936);
#5787=VERTEX_POINT('',#24937);
#5788=VERTEX_POINT('',#24984);
#5789=VERTEX_POINT('',#24985);
#5790=VERTEX_POINT('',#25038);
#5791=VERTEX_POINT('',#25039);
#5792=VERTEX_POINT('',#25086);
#5793=VERTEX_POINT('',#25087);
#5794=VERTEX_POINT('',#25134);
#5795=VERTEX_POINT('',#25135);
#5796=VERTEX_POINT('',#25188);
#5797=VERTEX_POINT('',#25189);
#5798=VERTEX_POINT('',#25236);
#5799=VERTEX_POINT('',#25237);
#5800=VERTEX_POINT('',#25284);
#5801=VERTEX_POINT('',#25285);
#5802=VERTEX_POINT('',#25332);
#5803=VERTEX_POINT('',#25333);
#5804=VERTEX_POINT('',#25386);
#5805=VERTEX_POINT('',#25387);
#5806=VERTEX_POINT('',#25434);
#5807=VERTEX_POINT('',#25435);
#5808=VERTEX_POINT('',#25482);
#5809=VERTEX_POINT('',#25483);
#5810=VERTEX_POINT('',#25485);
#5811=VERTEX_POINT('',#25496);
#5812=VERTEX_POINT('',#25507);
#5813=VERTEX_POINT('',#25508);
#5814=VERTEX_POINT('',#25532);
#5815=VERTEX_POINT('',#25533);
#5816=VERTEX_POINT('',#25556);
#5817=VERTEX_POINT('',#25557);
#5818=VERTEX_POINT('',#25581);
#5819=VERTEX_POINT('',#25582);
#5820=VERTEX_POINT('',#25606);
#5821=VERTEX_POINT('',#25607);
#5822=VERTEX_POINT('',#25630);
#5823=VERTEX_POINT('',#25631);
#5824=VERTEX_POINT('',#25654);
#5825=VERTEX_POINT('',#25655);
#5826=VERTEX_POINT('',#25679);
#5827=VERTEX_POINT('',#25680);
#5828=VERTEX_POINT('',#25704);
#5829=VERTEX_POINT('',#25705);
#5830=VERTEX_POINT('',#25728);
#5831=VERTEX_POINT('',#25729);
#5832=VERTEX_POINT('',#25753);
#5833=VERTEX_POINT('',#25754);
#5834=VERTEX_POINT('',#25778);
#5835=VERTEX_POINT('',#25779);
#5836=VERTEX_POINT('',#25802);
#5837=VERTEX_POINT('',#25803);
#5838=VERTEX_POINT('',#25826);
#5839=VERTEX_POINT('',#25827);
#5840=VERTEX_POINT('',#25851);
#5841=VERTEX_POINT('',#25852);
#5842=VERTEX_POINT('',#25876);
#5843=VERTEX_POINT('',#25877);
#5844=VERTEX_POINT('',#25900);
#5845=VERTEX_POINT('',#25901);
#5846=VERTEX_POINT('',#25925);
#5847=VERTEX_POINT('',#25926);
#5848=VERTEX_POINT('',#25950);
#5849=VERTEX_POINT('',#25951);
#5850=VERTEX_POINT('',#25974);
#5851=VERTEX_POINT('',#25975);
#5852=VERTEX_POINT('',#25999);
#5853=VERTEX_POINT('',#26000);
#5854=VERTEX_POINT('',#26024);
#5855=VERTEX_POINT('',#26025);
#5856=VERTEX_POINT('',#26048);
#5857=VERTEX_POINT('',#26049);
#5858=VERTEX_POINT('',#26072);
#5859=VERTEX_POINT('',#26305);
#5860=VERTEX_POINT('',#26373);
#5861=VERTEX_POINT('',#26406);
#5862=VERTEX_POINT('',#27041);
#5863=VERTEX_POINT('',#27167);
#5864=VERTEX_POINT('',#27939);
#5865=VERTEX_POINT('',#27940);
#5866=VERTEX_POINT('',#27942);
#5867=VERTEX_POINT('',#27944);
#5868=VERTEX_POINT('',#27948);
#5869=VERTEX_POINT('',#27950);
#5870=VERTEX_POINT('',#27954);
#5871=VERTEX_POINT('',#27956);
#5872=VERTEX_POINT('',#27960);
#5873=VERTEX_POINT('',#27962);
#5874=VERTEX_POINT('',#27966);
#5875=VERTEX_POINT('',#27968);
#5876=VERTEX_POINT('',#27976);
#5877=VERTEX_POINT('',#27979);
#5878=VERTEX_POINT('',#27986);
#5879=VERTEX_POINT('',#27988);
#5880=VERTEX_POINT('',#27992);
#5881=VERTEX_POINT('',#27994);
#5882=VERTEX_POINT('',#28042);
#5883=VERTEX_POINT('',#28043);
#5884=VERTEX_POINT('',#28045);
#5885=VERTEX_POINT('',#28053);
#5886=VERTEX_POINT('',#28055);
#5887=VERTEX_POINT('',#28058);
#5888=VERTEX_POINT('',#28077);
#5889=VERTEX_POINT('',#28078);
#5890=VERTEX_POINT('',#28167);
#5891=VERTEX_POINT('',#28168);
#5892=VERTEX_POINT('',#28254);
#5893=VERTEX_POINT('',#28255);
#5894=VERTEX_POINT('',#28341);
#5895=VERTEX_POINT('',#28342);
#5896=VERTEX_POINT('',#28428);
#5897=VERTEX_POINT('',#28429);
#5898=VERTEX_POINT('',#28518);
#5899=VERTEX_POINT('',#28519);
#5900=VERTEX_POINT('',#28605);
#5901=VERTEX_POINT('',#28606);
#5902=VERTEX_POINT('',#28692);
#5903=VERTEX_POINT('',#28693);
#5904=VERTEX_POINT('',#28782);
#5905=VERTEX_POINT('',#28783);
#5906=VERTEX_POINT('',#28869);
#5907=VERTEX_POINT('',#28870);
#5908=VERTEX_POINT('',#28956);
#5909=VERTEX_POINT('',#28957);
#5910=VERTEX_POINT('',#29043);
#5911=VERTEX_POINT('',#29044);
#5912=VERTEX_POINT('',#29133);
#5913=VERTEX_POINT('',#29134);
#5914=VERTEX_POINT('',#29220);
#5915=VERTEX_POINT('',#29221);
#5916=VERTEX_POINT('',#29307);
#5917=VERTEX_POINT('',#29308);
#5918=VERTEX_POINT('',#29394);
#5919=VERTEX_POINT('',#29395);
#5920=VERTEX_POINT('',#29484);
#5921=VERTEX_POINT('',#29485);
#5922=VERTEX_POINT('',#29571);
#5923=VERTEX_POINT('',#29572);
#5924=VERTEX_POINT('',#29658);
#5925=VERTEX_POINT('',#29659);
#5926=VERTEX_POINT('',#29748);
#5927=VERTEX_POINT('',#29749);
#5928=VERTEX_POINT('',#29835);
#5929=VERTEX_POINT('',#29836);
#5930=VERTEX_POINT('',#29922);
#5931=VERTEX_POINT('',#29923);
#5932=VERTEX_POINT('',#30009);
#5933=VERTEX_POINT('',#30010);
#5934=VERTEX_POINT('',#30099);
#5935=VERTEX_POINT('',#30100);
#5936=VERTEX_POINT('',#30102);
#5937=VERTEX_POINT('',#30128);
#5938=VERTEX_POINT('',#30168);
#5939=VERTEX_POINT('',#30169);
#5940=VERTEX_POINT('',#30171);
#5941=VERTEX_POINT('',#30184);
#5942=VERTEX_POINT('',#30201);
#5943=VERTEX_POINT('',#30202);
#5944=VERTEX_POINT('',#30238);
#5945=VERTEX_POINT('',#30239);
#5946=VERTEX_POINT('',#30276);
#5947=VERTEX_POINT('',#30277);
#5948=VERTEX_POINT('',#30312);
#5949=VERTEX_POINT('',#30313);
#5950=VERTEX_POINT('',#30350);
#5951=VERTEX_POINT('',#30351);
#5952=VERTEX_POINT('',#30388);
#5953=VERTEX_POINT('',#30389);
#5954=VERTEX_POINT('',#30424);
#5955=VERTEX_POINT('',#30425);
#5956=VERTEX_POINT('',#30462);
#5957=VERTEX_POINT('',#30463);
#5958=VERTEX_POINT('',#30500);
#5959=VERTEX_POINT('',#30501);
#5960=VERTEX_POINT('',#30536);
#5961=VERTEX_POINT('',#30537);
#5962=VERTEX_POINT('',#30574);
#5963=VERTEX_POINT('',#30575);
#5964=VERTEX_POINT('',#30611);
#5965=VERTEX_POINT('',#30612);
#5966=VERTEX_POINT('',#30648);
#5967=VERTEX_POINT('',#30649);
#5968=VERTEX_POINT('',#30686);
#5969=VERTEX_POINT('',#30687);
#5970=VERTEX_POINT('',#30722);
#5971=VERTEX_POINT('',#30723);
#5972=VERTEX_POINT('',#30760);
#5973=VERTEX_POINT('',#30761);
#5974=VERTEX_POINT('',#30798);
#5975=VERTEX_POINT('',#30799);
#5976=VERTEX_POINT('',#30834);
#5977=VERTEX_POINT('',#30835);
#5978=VERTEX_POINT('',#30872);
#5979=VERTEX_POINT('',#30873);
#5980=VERTEX_POINT('',#30910);
#5981=VERTEX_POINT('',#30911);
#5982=VERTEX_POINT('',#30946);
#5983=VERTEX_POINT('',#30947);
#5984=VERTEX_POINT('',#30984);
#5985=VERTEX_POINT('',#30985);
#5986=VERTEX_POINT('',#31021);
#5987=VERTEX_POINT('',#31022);
#5988=VERTEX_POINT('',#31058);
#5989=VERTEX_POINT('',#31059);
#5990=VERTEX_POINT('',#31061);
#5991=VERTEX_POINT('',#31068);
#5992=VERTEX_POINT('',#31078);
#5993=VERTEX_POINT('',#31079);
#5994=VERTEX_POINT('',#31081);
#5995=VERTEX_POINT('',#31089);
#5996=VERTEX_POINT('',#31091);
#5997=VERTEX_POINT('',#31094);
#5998=VERTEX_POINT('',#31113);
#5999=VERTEX_POINT('',#31114);
#6000=VERTEX_POINT('',#31203);
#6001=VERTEX_POINT('',#31204);
#6002=VERTEX_POINT('',#31290);
#6003=VERTEX_POINT('',#31291);
#6004=VERTEX_POINT('',#31377);
#6005=VERTEX_POINT('',#31378);
#6006=VERTEX_POINT('',#31464);
#6007=VERTEX_POINT('',#31465);
#6008=VERTEX_POINT('',#31551);
#6009=VERTEX_POINT('',#31552);
#6010=VERTEX_POINT('',#31641);
#6011=VERTEX_POINT('',#31642);
#6012=VERTEX_POINT('',#31728);
#6013=VERTEX_POINT('',#31729);
#6014=VERTEX_POINT('',#31815);
#6015=VERTEX_POINT('',#31816);
#6016=VERTEX_POINT('',#31902);
#6017=VERTEX_POINT('',#31903);
#6018=VERTEX_POINT('',#31989);
#6019=VERTEX_POINT('',#31990);
#6020=VERTEX_POINT('',#32079);
#6021=VERTEX_POINT('',#32080);
#6022=VERTEX_POINT('',#32166);
#6023=VERTEX_POINT('',#32167);
#6024=VERTEX_POINT('',#32253);
#6025=VERTEX_POINT('',#32254);
#6026=VERTEX_POINT('',#32340);
#6027=VERTEX_POINT('',#32341);
#6028=VERTEX_POINT('',#32427);
#6029=VERTEX_POINT('',#32428);
#6030=VERTEX_POINT('',#32514);
#6031=VERTEX_POINT('',#32515);
#6032=VERTEX_POINT('',#32601);
#6033=VERTEX_POINT('',#32602);
#6034=VERTEX_POINT('',#32688);
#6035=VERTEX_POINT('',#32689);
#6036=VERTEX_POINT('',#32763);
#6037=VERTEX_POINT('',#32764);
#6038=VERTEX_POINT('',#32811);
#6039=VERTEX_POINT('',#32812);
#6040=VERTEX_POINT('',#32868);
#6041=VERTEX_POINT('',#32869);
#6042=VERTEX_POINT('',#32955);
#6043=VERTEX_POINT('',#32956);
#6044=VERTEX_POINT('',#33042);
#6045=VERTEX_POINT('',#33043);
#6046=VERTEX_POINT('',#33129);
#6047=VERTEX_POINT('',#33130);
#6048=VERTEX_POINT('',#33216);
#6049=VERTEX_POINT('',#33217);
#6050=VERTEX_POINT('',#33303);
#6051=VERTEX_POINT('',#33304);
#6052=VERTEX_POINT('',#33393);
#6053=VERTEX_POINT('',#33394);
#6054=VERTEX_POINT('',#33480);
#6055=VERTEX_POINT('',#33481);
#6056=VERTEX_POINT('',#33567);
#6057=VERTEX_POINT('',#33568);
#6058=VERTEX_POINT('',#33654);
#6059=VERTEX_POINT('',#33655);
#6060=VERTEX_POINT('',#33741);
#6061=VERTEX_POINT('',#33742);
#6062=VERTEX_POINT('',#33831);
#6063=VERTEX_POINT('',#33832);
#6064=VERTEX_POINT('',#33918);
#6065=VERTEX_POINT('',#33919);
#6066=VERTEX_POINT('',#34005);
#6067=VERTEX_POINT('',#34006);
#6068=VERTEX_POINT('',#34092);
#6069=VERTEX_POINT('',#34093);
#6070=VERTEX_POINT('',#34179);
#6071=VERTEX_POINT('',#34180);
#6072=VERTEX_POINT('',#34269);
#6073=VERTEX_POINT('',#34270);
#6074=VERTEX_POINT('',#34356);
#6075=VERTEX_POINT('',#34357);
#6076=VERTEX_POINT('',#34359);
#6077=VERTEX_POINT('',#34385);
#6078=VERTEX_POINT('',#34425);
#6079=VERTEX_POINT('',#34426);
#6080=VERTEX_POINT('',#34428);
#6081=VERTEX_POINT('',#34441);
#6082=VERTEX_POINT('',#34458);
#6083=VERTEX_POINT('',#34459);
#6084=VERTEX_POINT('',#34495);
#6085=VERTEX_POINT('',#34496);
#6086=VERTEX_POINT('',#34533);
#6087=VERTEX_POINT('',#34534);
#6088=VERTEX_POINT('',#34569);
#6089=VERTEX_POINT('',#34570);
#6090=VERTEX_POINT('',#34607);
#6091=VERTEX_POINT('',#34608);
#6092=VERTEX_POINT('',#34644);
#6093=VERTEX_POINT('',#34645);
#6094=VERTEX_POINT('',#34681);
#6095=VERTEX_POINT('',#34682);
#6096=VERTEX_POINT('',#34719);
#6097=VERTEX_POINT('',#34720);
#6098=VERTEX_POINT('',#34755);
#6099=VERTEX_POINT('',#34756);
#6100=VERTEX_POINT('',#34793);
#6101=VERTEX_POINT('',#34794);
#6102=VERTEX_POINT('',#34830);
#6103=VERTEX_POINT('',#34831);
#6104=VERTEX_POINT('',#34867);
#6105=VERTEX_POINT('',#34868);
#6106=VERTEX_POINT('',#34905);
#6107=VERTEX_POINT('',#34906);
#6108=VERTEX_POINT('',#34941);
#6109=VERTEX_POINT('',#34942);
#6110=VERTEX_POINT('',#34979);
#6111=VERTEX_POINT('',#34980);
#6112=VERTEX_POINT('',#35016);
#6113=VERTEX_POINT('',#35017);
#6114=VERTEX_POINT('',#35053);
#6115=VERTEX_POINT('',#35054);
#6116=VERTEX_POINT('',#35091);
#6117=VERTEX_POINT('',#35092);
#6118=VERTEX_POINT('',#35127);
#6119=VERTEX_POINT('',#35128);
#6120=VERTEX_POINT('',#35154);
#6121=VERTEX_POINT('',#35155);
#6122=VERTEX_POINT('',#35178);
#6123=VERTEX_POINT('',#35179);
#6124=VERTEX_POINT('',#35211);
#6125=VERTEX_POINT('',#35212);
#6126=VERTEX_POINT('',#35249);
#6127=VERTEX_POINT('',#35250);
#6128=VERTEX_POINT('',#35285);
#6129=VERTEX_POINT('',#35286);
#6130=VERTEX_POINT('',#35323);
#6131=VERTEX_POINT('',#35324);
#6132=VERTEX_POINT('',#35359);
#6133=VERTEX_POINT('',#35360);
#6134=VERTEX_POINT('',#35397);
#6135=VERTEX_POINT('',#35398);
#6136=VERTEX_POINT('',#35435);
#6137=VERTEX_POINT('',#35436);
#6138=VERTEX_POINT('',#35471);
#6139=VERTEX_POINT('',#35472);
#6140=VERTEX_POINT('',#35509);
#6141=VERTEX_POINT('',#35510);
#6142=VERTEX_POINT('',#35545);
#6143=VERTEX_POINT('',#35546);
#6144=VERTEX_POINT('',#35583);
#6145=VERTEX_POINT('',#35584);
#6146=VERTEX_POINT('',#35621);
#6147=VERTEX_POINT('',#35622);
#6148=VERTEX_POINT('',#35657);
#6149=VERTEX_POINT('',#35658);
#6150=VERTEX_POINT('',#35695);
#6151=VERTEX_POINT('',#35696);
#6152=VERTEX_POINT('',#35731);
#6153=VERTEX_POINT('',#35732);
#6154=VERTEX_POINT('',#35769);
#6155=VERTEX_POINT('',#35770);
#6156=VERTEX_POINT('',#35807);
#6157=VERTEX_POINT('',#35808);
#6158=VERTEX_POINT('',#35843);
#6159=VERTEX_POINT('',#35844);
#6160=VERTEX_POINT('',#35846);
#6161=VERTEX_POINT('',#35853);
#6162=VERTEX_POINT('',#40380);
#6163=VERTEX_POINT('',#43505);
#6164=VERTEX_POINT('',#43508);
#6165=VERTEX_POINT('',#43509);
#6166=VERTEX_POINT('',#43511);
#6167=VERTEX_POINT('',#43513);
#6168=VERTEX_POINT('',#43517);
#6169=VERTEX_POINT('',#43519);
#6170=VERTEX_POINT('',#43523);
#6171=VERTEX_POINT('',#43525);
#6172=VERTEX_POINT('',#43527);
#6173=VERTEX_POINT('',#43529);
#6174=VERTEX_POINT('',#43531);
#6175=VERTEX_POINT('',#43533);
#6176=VERTEX_POINT('',#43535);
#6177=VERTEX_POINT('',#43537);
#6178=VERTEX_POINT('',#43539);
#6179=VERTEX_POINT('',#43541);
#6180=VERTEX_POINT('',#43543);
#6181=VERTEX_POINT('',#43545);
#6182=VERTEX_POINT('',#43547);
#6183=VERTEX_POINT('',#43549);
#6184=VERTEX_POINT('',#43551);
#6185=VERTEX_POINT('',#43553);
#6186=VERTEX_POINT('',#43555);
#6187=VERTEX_POINT('',#43557);
#6188=VERTEX_POINT('',#43559);
#6189=VERTEX_POINT('',#43561);
#6190=VERTEX_POINT('',#43563);
#6191=VERTEX_POINT('',#43565);
#6192=VERTEX_POINT('',#43567);
#6193=VERTEX_POINT('',#43569);
#6194=VERTEX_POINT('',#43571);
#6195=VERTEX_POINT('',#43573);
#6196=VERTEX_POINT('',#43575);
#6197=VERTEX_POINT('',#43577);
#6198=VERTEX_POINT('',#43579);
#6199=VERTEX_POINT('',#43581);
#6200=VERTEX_POINT('',#43583);
#6201=VERTEX_POINT('',#43585);
#6202=VERTEX_POINT('',#43587);
#6203=VERTEX_POINT('',#43589);
#6204=VERTEX_POINT('',#43591);
#6205=VERTEX_POINT('',#43593);
#6206=VERTEX_POINT('',#43595);
#6207=VERTEX_POINT('',#43597);
#6208=VERTEX_POINT('',#43599);
#6209=VERTEX_POINT('',#43601);
#6210=VERTEX_POINT('',#43603);
#6211=VERTEX_POINT('',#43605);
#6212=VERTEX_POINT('',#43607);
#6213=VERTEX_POINT('',#43609);
#6214=VERTEX_POINT('',#43611);
#6215=VERTEX_POINT('',#43613);
#6216=VERTEX_POINT('',#43615);
#6217=VERTEX_POINT('',#43617);
#6218=VERTEX_POINT('',#43619);
#6219=VERTEX_POINT('',#43621);
#6220=VERTEX_POINT('',#43623);
#6221=VERTEX_POINT('',#43625);
#6222=VERTEX_POINT('',#43627);
#6223=VERTEX_POINT('',#43629);
#6224=VERTEX_POINT('',#43631);
#6225=VERTEX_POINT('',#43633);
#6226=VERTEX_POINT('',#43635);
#6227=VERTEX_POINT('',#43637);
#6228=VERTEX_POINT('',#43639);
#6229=VERTEX_POINT('',#43641);
#6230=VERTEX_POINT('',#43643);
#6231=VERTEX_POINT('',#43645);
#6232=VERTEX_POINT('',#43647);
#6233=VERTEX_POINT('',#43649);
#6234=VERTEX_POINT('',#43651);
#6235=VERTEX_POINT('',#43653);
#6236=VERTEX_POINT('',#43655);
#6237=VERTEX_POINT('',#43657);
#6238=VERTEX_POINT('',#43659);
#6239=VERTEX_POINT('',#43662);
#6240=VERTEX_POINT('',#43664);
#6241=VERTEX_POINT('',#43666);
#6242=VERTEX_POINT('',#43668);
#6243=VERTEX_POINT('',#43671);
#6244=VERTEX_POINT('',#43672);
#6245=VERTEX_POINT('',#43677);
#6246=VERTEX_POINT('',#43681);
#6247=VERTEX_POINT('',#43685);
#6248=VERTEX_POINT('',#43689);
#6249=VERTEX_POINT('',#43693);
#6250=VERTEX_POINT('',#43697);
#6251=VERTEX_POINT('',#43701);
#6252=VERTEX_POINT('',#43705);
#6253=VERTEX_POINT('',#43709);
#6254=VERTEX_POINT('',#43711);
#6255=VERTEX_POINT('',#43715);
#6256=VERTEX_POINT('',#43719);
#6257=VERTEX_POINT('',#43723);
#6258=VERTEX_POINT('',#43725);
#6259=VERTEX_POINT('',#43729);
#6260=VERTEX_POINT('',#43733);
#6261=VERTEX_POINT('',#43737);
#6262=VERTEX_POINT('',#43738);
#6263=VERTEX_POINT('',#43743);
#6264=VERTEX_POINT('',#43747);
#6265=VERTEX_POINT('',#43751);
#6266=VERTEX_POINT('',#43755);
#6267=VERTEX_POINT('',#43759);
#6268=VERTEX_POINT('',#43763);
#6269=VERTEX_POINT('',#43767);
#6270=VERTEX_POINT('',#43771);
#6271=VERTEX_POINT('',#43775);
#6272=VERTEX_POINT('',#43777);
#6273=VERTEX_POINT('',#43781);
#6274=VERTEX_POINT('',#43785);
#6275=VERTEX_POINT('',#43789);
#6276=VERTEX_POINT('',#43791);
#6277=VERTEX_POINT('',#43795);
#6278=VERTEX_POINT('',#43799);
#6279=VERTEX_POINT('',#43803);
#6280=VERTEX_POINT('',#43804);
#6281=VERTEX_POINT('',#43809);
#6282=VERTEX_POINT('',#43813);
#6283=VERTEX_POINT('',#43817);
#6284=VERTEX_POINT('',#43821);
#6285=VERTEX_POINT('',#43825);
#6286=VERTEX_POINT('',#43829);
#6287=VERTEX_POINT('',#43833);
#6288=VERTEX_POINT('',#43837);
#6289=VERTEX_POINT('',#43841);
#6290=VERTEX_POINT('',#43843);
#6291=VERTEX_POINT('',#43847);
#6292=VERTEX_POINT('',#43851);
#6293=VERTEX_POINT('',#43855);
#6294=VERTEX_POINT('',#43857);
#6295=VERTEX_POINT('',#43861);
#6296=VERTEX_POINT('',#43865);
#6297=VERTEX_POINT('',#43869);
#6298=VERTEX_POINT('',#43870);
#6299=VERTEX_POINT('',#43875);
#6300=VERTEX_POINT('',#43879);
#6301=VERTEX_POINT('',#43883);
#6302=VERTEX_POINT('',#43887);
#6303=VERTEX_POINT('',#43891);
#6304=VERTEX_POINT('',#43895);
#6305=VERTEX_POINT('',#43899);
#6306=VERTEX_POINT('',#43903);
#6307=VERTEX_POINT('',#43907);
#6308=VERTEX_POINT('',#43909);
#6309=VERTEX_POINT('',#43913);
#6310=VERTEX_POINT('',#43917);
#6311=VERTEX_POINT('',#43921);
#6312=VERTEX_POINT('',#43925);
#6313=VERTEX_POINT('',#43929);
#6314=VERTEX_POINT('',#43935);
#6315=VERTEX_POINT('',#43939);
#6316=VERTEX_POINT('',#43969);
#6317=VERTEX_POINT('',#43971);
#6318=VERTEX_POINT('',#43974);
#6319=VERTEX_POINT('',#43978);
#6320=VERTEX_POINT('',#43982);
#6321=VERTEX_POINT('',#43984);
#6322=VERTEX_POINT('',#43988);
#6323=VERTEX_POINT('',#43990);
#6324=VERTEX_POINT('',#43994);
#6325=VERTEX_POINT('',#43996);
#6326=VERTEX_POINT('',#44000);
#6327=VERTEX_POINT('',#44002);
#6328=VERTEX_POINT('',#44006);
#6329=VERTEX_POINT('',#44007);
#6330=VERTEX_POINT('',#44009);
#6331=VERTEX_POINT('',#44011);
#6332=VERTEX_POINT('',#44015);
#6333=VERTEX_POINT('',#44017);
#6334=VERTEX_POINT('',#44021);
#6335=VERTEX_POINT('',#44023);
#6336=VERTEX_POINT('',#44033);
#6337=VERTEX_POINT('',#44034);
#6338=VERTEX_POINT('',#44036);
#6339=VERTEX_POINT('',#44047);
#6340=VERTEX_POINT('',#44060);
#6341=VERTEX_POINT('',#44061);
#6342=VERTEX_POINT('',#44108);
#6343=VERTEX_POINT('',#44109);
#6344=VERTEX_POINT('',#44156);
#6345=VERTEX_POINT('',#44157);
#6346=VERTEX_POINT('',#44210);
#6347=VERTEX_POINT('',#44211);
#6348=VERTEX_POINT('',#44258);
#6349=VERTEX_POINT('',#44259);
#6350=VERTEX_POINT('',#44306);
#6351=VERTEX_POINT('',#44307);
#6352=VERTEX_POINT('',#44360);
#6353=VERTEX_POINT('',#44361);
#6354=VERTEX_POINT('',#44408);
#6355=VERTEX_POINT('',#44409);
#6356=VERTEX_POINT('',#44456);
#6357=VERTEX_POINT('',#44457);
#6358=VERTEX_POINT('',#44504);
#6359=VERTEX_POINT('',#44505);
#6360=VERTEX_POINT('',#44558);
#6361=VERTEX_POINT('',#44559);
#6362=VERTEX_POINT('',#44606);
#6363=VERTEX_POINT('',#44607);
#6364=VERTEX_POINT('',#44654);
#6365=VERTEX_POINT('',#44655);
#6366=VERTEX_POINT('',#44708);
#6367=VERTEX_POINT('',#44709);
#6368=VERTEX_POINT('',#44756);
#6369=VERTEX_POINT('',#44757);
#6370=VERTEX_POINT('',#44804);
#6371=VERTEX_POINT('',#44805);
#6372=VERTEX_POINT('',#44858);
#6373=VERTEX_POINT('',#44859);
#6374=VERTEX_POINT('',#44906);
#6375=VERTEX_POINT('',#44907);
#6376=VERTEX_POINT('',#44954);
#6377=VERTEX_POINT('',#44955);
#6378=VERTEX_POINT('',#44957);
#6379=VERTEX_POINT('',#44969);
#6380=VERTEX_POINT('',#44981);
#6381=VERTEX_POINT('',#44982);
#6382=VERTEX_POINT('',#45006);
#6383=VERTEX_POINT('',#45007);
#6384=VERTEX_POINT('',#45030);
#6385=VERTEX_POINT('',#45031);
#6386=VERTEX_POINT('',#45055);
#6387=VERTEX_POINT('',#45056);
#6388=VERTEX_POINT('',#45080);
#6389=VERTEX_POINT('',#45081);
#6390=VERTEX_POINT('',#45104);
#6391=VERTEX_POINT('',#45105);
#6392=VERTEX_POINT('',#45129);
#6393=VERTEX_POINT('',#45130);
#6394=VERTEX_POINT('',#45154);
#6395=VERTEX_POINT('',#45155);
#6396=VERTEX_POINT('',#45178);
#6397=VERTEX_POINT('',#45179);
#6398=VERTEX_POINT('',#45203);
#6399=VERTEX_POINT('',#45204);
#6400=VERTEX_POINT('',#45228);
#6401=VERTEX_POINT('',#45229);
#6402=VERTEX_POINT('',#45252);
#6403=VERTEX_POINT('',#45253);
#6404=VERTEX_POINT('',#45276);
#6405=VERTEX_POINT('',#45277);
#6406=VERTEX_POINT('',#45301);
#6407=VERTEX_POINT('',#45302);
#6408=VERTEX_POINT('',#45326);
#6409=VERTEX_POINT('',#45327);
#6410=VERTEX_POINT('',#45350);
#6411=VERTEX_POINT('',#45351);
#6412=VERTEX_POINT('',#45375);
#6413=VERTEX_POINT('',#45376);
#6414=VERTEX_POINT('',#45400);
#6415=VERTEX_POINT('',#45401);
#6416=VERTEX_POINT('',#45424);
#6417=VERTEX_POINT('',#45669);
#6418=VERTEX_POINT('',#45743);
#6419=VERTEX_POINT('',#45782);
#6420=VERTEX_POINT('',#46301);
#6421=VERTEX_POINT('',#46434);
#6422=VERTEX_POINT('',#47099);
#6423=VERTEX_POINT('',#47100);
#6424=VERTEX_POINT('',#47102);
#6425=VERTEX_POINT('',#47104);
#6426=VERTEX_POINT('',#47108);
#6427=VERTEX_POINT('',#47110);
#6428=VERTEX_POINT('',#47114);
#6429=VERTEX_POINT('',#47116);
#6430=VERTEX_POINT('',#47120);
#6431=VERTEX_POINT('',#47122);
#6432=VERTEX_POINT('',#47126);
#6433=VERTEX_POINT('',#47128);
#6434=VERTEX_POINT('',#47136);
#6435=VERTEX_POINT('',#47139);
#6436=VERTEX_POINT('',#47146);
#6437=VERTEX_POINT('',#47148);
#6438=VERTEX_POINT('',#47155);
#6439=VERTEX_POINT('',#47156);
#6440=VERTEX_POINT('',#47158);
#6441=VERTEX_POINT('',#47163);
#6442=VERTEX_POINT('',#47165);
#6443=VERTEX_POINT('',#47168);
#6444=VERTEX_POINT('',#47181);
#6445=VERTEX_POINT('',#47182);
#6446=VERTEX_POINT('',#47232);
#6447=VERTEX_POINT('',#47233);
#6448=VERTEX_POINT('',#47283);
#6449=VERTEX_POINT('',#47284);
#6450=VERTEX_POINT('',#47331);
#6451=VERTEX_POINT('',#47332);
#6452=VERTEX_POINT('',#47382);
#6453=VERTEX_POINT('',#47383);
#6454=VERTEX_POINT('',#47433);
#6455=VERTEX_POINT('',#47434);
#6456=VERTEX_POINT('',#47481);
#6457=VERTEX_POINT('',#47482);
#6458=VERTEX_POINT('',#47484);
#6459=VERTEX_POINT('',#47498);
#6460=VERTEX_POINT('',#47520);
#6461=VERTEX_POINT('',#47521);
#6462=VERTEX_POINT('',#47523);
#6463=VERTEX_POINT('',#47532);
#6464=VERTEX_POINT('',#47544);
#6465=VERTEX_POINT('',#47545);
#6466=VERTEX_POINT('',#47568);
#6467=VERTEX_POINT('',#47569);
#6468=VERTEX_POINT('',#47593);
#6469=VERTEX_POINT('',#47594);
#6470=VERTEX_POINT('',#47618);
#6471=VERTEX_POINT('',#47619);
#6472=VERTEX_POINT('',#47642);
#6473=VERTEX_POINT('',#47643);
#6474=VERTEX_POINT('',#47667);
#6475=VERTEX_POINT('',#47668);
#6476=VERTEX_POINT('',#47692);
#6477=VERTEX_POINT('',#47693);
#6478=VERTEX_POINT('',#47695);
#6479=VERTEX_POINT('',#47701);
#6480=VERTEX_POINT('',#47709);
#6481=VERTEX_POINT('',#47710);
#6482=VERTEX_POINT('',#47712);
#6483=VERTEX_POINT('',#47717);
#6484=VERTEX_POINT('',#47719);
#6485=VERTEX_POINT('',#47722);
#6486=VERTEX_POINT('',#47735);
#6487=VERTEX_POINT('',#47736);
#6488=VERTEX_POINT('',#47786);
#6489=VERTEX_POINT('',#47787);
#6490=VERTEX_POINT('',#47837);
#6491=VERTEX_POINT('',#47838);
#6492=VERTEX_POINT('',#47885);
#6493=VERTEX_POINT('',#47886);
#6494=VERTEX_POINT('',#47936);
#6495=VERTEX_POINT('',#47937);
#6496=VERTEX_POINT('',#47987);
#6497=VERTEX_POINT('',#47988);
#6498=VERTEX_POINT('',#48035);
#6499=VERTEX_POINT('',#48036);
#6500=VERTEX_POINT('',#48038);
#6501=VERTEX_POINT('',#48052);
#6502=VERTEX_POINT('',#48074);
#6503=VERTEX_POINT('',#48075);
#6504=VERTEX_POINT('',#48077);
#6505=VERTEX_POINT('',#48086);
#6506=VERTEX_POINT('',#48098);
#6507=VERTEX_POINT('',#48099);
#6508=VERTEX_POINT('',#48122);
#6509=VERTEX_POINT('',#48123);
#6510=VERTEX_POINT('',#48147);
#6511=VERTEX_POINT('',#48148);
#6512=VERTEX_POINT('',#48172);
#6513=VERTEX_POINT('',#48173);
#6514=VERTEX_POINT('',#48196);
#6515=VERTEX_POINT('',#48197);
#6516=VERTEX_POINT('',#48221);
#6517=VERTEX_POINT('',#48222);
#6518=VERTEX_POINT('',#48246);
#6519=VERTEX_POINT('',#48247);
#6520=VERTEX_POINT('',#48249);
#6521=VERTEX_POINT('',#48255);
#6522=VERTEX_POINT('',#48263);
#6523=VERTEX_POINT('',#48264);
#6524=VERTEX_POINT('',#48266);
#6525=VERTEX_POINT('',#48271);
#6526=VERTEX_POINT('',#48273);
#6527=VERTEX_POINT('',#48276);
#6528=VERTEX_POINT('',#48289);
#6529=VERTEX_POINT('',#48290);
#6530=VERTEX_POINT('',#48340);
#6531=VERTEX_POINT('',#48341);
#6532=VERTEX_POINT('',#48391);
#6533=VERTEX_POINT('',#48392);
#6534=VERTEX_POINT('',#48439);
#6535=VERTEX_POINT('',#48440);
#6536=VERTEX_POINT('',#48490);
#6537=VERTEX_POINT('',#48491);
#6538=VERTEX_POINT('',#48541);
#6539=VERTEX_POINT('',#48542);
#6540=VERTEX_POINT('',#48589);
#6541=VERTEX_POINT('',#48590);
#6542=VERTEX_POINT('',#48592);
#6543=VERTEX_POINT('',#48606);
#6544=VERTEX_POINT('',#48628);
#6545=VERTEX_POINT('',#48629);
#6546=VERTEX_POINT('',#48631);
#6547=VERTEX_POINT('',#48640);
#6548=VERTEX_POINT('',#48652);
#6549=VERTEX_POINT('',#48653);
#6550=VERTEX_POINT('',#48676);
#6551=VERTEX_POINT('',#48677);
#6552=VERTEX_POINT('',#48701);
#6553=VERTEX_POINT('',#48702);
#6554=VERTEX_POINT('',#48726);
#6555=VERTEX_POINT('',#48727);
#6556=VERTEX_POINT('',#48750);
#6557=VERTEX_POINT('',#48751);
#6558=VERTEX_POINT('',#48775);
#6559=VERTEX_POINT('',#48776);
#6560=VERTEX_POINT('',#48800);
#6561=VERTEX_POINT('',#48801);
#6562=VERTEX_POINT('',#48803);
#6563=VERTEX_POINT('',#48809);
#6564=VERTEX_POINT('',#51496);
#6565=VERTEX_POINT('',#51498);
#6566=VERTEX_POINT('',#51501);
#6567=VERTEX_POINT('',#51503);
#6568=VERTEX_POINT('',#51510);
#6569=VERTEX_POINT('',#51512);
#6570=VERTEX_POINT('',#51516);
#6571=VERTEX_POINT('',#51518);
#6572=VERTEX_POINT('',#51522);
#6573=VERTEX_POINT('',#51524);
#6574=VERTEX_POINT('',#51528);
#6575=VERTEX_POINT('',#51530);
#6576=VERTEX_POINT('',#51534);
#6577=VERTEX_POINT('',#51538);
#6578=VERTEX_POINT('',#51540);
#6579=VERTEX_POINT('',#51547);
#6580=VERTEX_POINT('',#51548);
#6581=VERTEX_POINT('',#51550);
#6582=VERTEX_POINT('',#51561);
#6583=VERTEX_POINT('',#51574);
#6584=VERTEX_POINT('',#51575);
#6585=VERTEX_POINT('',#51622);
#6586=VERTEX_POINT('',#51623);
#6587=VERTEX_POINT('',#51670);
#6588=VERTEX_POINT('',#51671);
#6589=VERTEX_POINT('',#51721);
#6590=VERTEX_POINT('',#51722);
#6591=VERTEX_POINT('',#51769);
#6592=VERTEX_POINT('',#51770);
#6593=VERTEX_POINT('',#51817);
#6594=VERTEX_POINT('',#51818);
#6595=VERTEX_POINT('',#51865);
#6596=VERTEX_POINT('',#51866);
#6597=VERTEX_POINT('',#51919);
#6598=VERTEX_POINT('',#51920);
#6599=VERTEX_POINT('',#51967);
#6600=VERTEX_POINT('',#51968);
#6601=VERTEX_POINT('',#52015);
#6602=VERTEX_POINT('',#52016);
#6603=VERTEX_POINT('',#52069);
#6604=VERTEX_POINT('',#52070);
#6605=VERTEX_POINT('',#52117);
#6606=VERTEX_POINT('',#52118);
#6607=VERTEX_POINT('',#52165);
#6608=VERTEX_POINT('',#52166);
#6609=VERTEX_POINT('',#52216);
#6610=VERTEX_POINT('',#52217);
#6611=VERTEX_POINT('',#52267);
#6612=VERTEX_POINT('',#52268);
#6613=VERTEX_POINT('',#52315);
#6614=VERTEX_POINT('',#52316);
#6615=VERTEX_POINT('',#52363);
#6616=VERTEX_POINT('',#52364);
#6617=VERTEX_POINT('',#52417);
#6618=VERTEX_POINT('',#52418);
#6619=VERTEX_POINT('',#52465);
#6620=VERTEX_POINT('',#52466);
#6621=VERTEX_POINT('',#52513);
#6622=VERTEX_POINT('',#52514);
#6623=VERTEX_POINT('',#52567);
#6624=VERTEX_POINT('',#52568);
#6625=VERTEX_POINT('',#52615);
#6626=VERTEX_POINT('',#52616);
#6627=VERTEX_POINT('',#52663);
#6628=VERTEX_POINT('',#52664);
#6629=VERTEX_POINT('',#52711);
#6630=VERTEX_POINT('',#52712);
#6631=VERTEX_POINT('',#52765);
#6632=VERTEX_POINT('',#52766);
#6633=VERTEX_POINT('',#52813);
#6634=VERTEX_POINT('',#52814);
#6635=VERTEX_POINT('',#52861);
#6636=VERTEX_POINT('',#52862);
#6637=VERTEX_POINT('',#52915);
#6638=VERTEX_POINT('',#52916);
#6639=VERTEX_POINT('',#52963);
#6640=VERTEX_POINT('',#52964);
#6641=VERTEX_POINT('',#53011);
#6642=VERTEX_POINT('',#53012);
#6643=VERTEX_POINT('',#53065);
#6644=VERTEX_POINT('',#53066);
#6645=VERTEX_POINT('',#53113);
#6646=VERTEX_POINT('',#53114);
#6647=VERTEX_POINT('',#53161);
#6648=VERTEX_POINT('',#53162);
#6649=VERTEX_POINT('',#53209);
#6650=VERTEX_POINT('',#53210);
#6651=VERTEX_POINT('',#53263);
#6652=VERTEX_POINT('',#53264);
#6653=VERTEX_POINT('',#53311);
#6654=VERTEX_POINT('',#53312);
#6655=VERTEX_POINT('',#53359);
#6656=VERTEX_POINT('',#53360);
#6657=VERTEX_POINT('',#53413);
#6658=VERTEX_POINT('',#53414);
#6659=VERTEX_POINT('',#53461);
#6660=VERTEX_POINT('',#53462);
#6661=VERTEX_POINT('',#53509);
#6662=VERTEX_POINT('',#53510);
#6663=VERTEX_POINT('',#53563);
#6664=VERTEX_POINT('',#53564);
#6665=VERTEX_POINT('',#53611);
#6666=VERTEX_POINT('',#53612);
#6667=VERTEX_POINT('',#53659);
#6668=VERTEX_POINT('',#53660);
#6669=VERTEX_POINT('',#53707);
#6670=VERTEX_POINT('',#53708);
#6671=VERTEX_POINT('',#53761);
#6672=VERTEX_POINT('',#53762);
#6673=VERTEX_POINT('',#53809);
#6674=VERTEX_POINT('',#53810);
#6675=VERTEX_POINT('',#53857);
#6676=VERTEX_POINT('',#53858);
#6677=VERTEX_POINT('',#53911);
#6678=VERTEX_POINT('',#53912);
#6679=VERTEX_POINT('',#53959);
#6680=VERTEX_POINT('',#53960);
#6681=VERTEX_POINT('',#54007);
#6682=VERTEX_POINT('',#54008);
#6683=VERTEX_POINT('',#54061);
#6684=VERTEX_POINT('',#54062);
#6685=VERTEX_POINT('',#54109);
#6686=VERTEX_POINT('',#54110);
#6687=VERTEX_POINT('',#54157);
#6688=VERTEX_POINT('',#54158);
#6689=VERTEX_POINT('',#54205);
#6690=VERTEX_POINT('',#54206);
#6691=VERTEX_POINT('',#54259);
#6692=VERTEX_POINT('',#54260);
#6693=VERTEX_POINT('',#54307);
#6694=VERTEX_POINT('',#54308);
#6695=VERTEX_POINT('',#54355);
#6696=VERTEX_POINT('',#54356);
#6697=VERTEX_POINT('',#54409);
#6698=VERTEX_POINT('',#54410);
#6699=VERTEX_POINT('',#54457);
#6700=VERTEX_POINT('',#54458);
#6701=VERTEX_POINT('',#54505);
#6702=VERTEX_POINT('',#54506);
#6703=VERTEX_POINT('',#54508);
#6704=VERTEX_POINT('',#54515);
#6705=VERTEX_POINT('',#54523);
#6706=VERTEX_POINT('',#54524);
#6707=VERTEX_POINT('',#54548);
#6708=VERTEX_POINT('',#54549);
#6709=VERTEX_POINT('',#54572);
#6710=VERTEX_POINT('',#54573);
#6711=VERTEX_POINT('',#54597);
#6712=VERTEX_POINT('',#54598);
#6713=VERTEX_POINT('',#54622);
#6714=VERTEX_POINT('',#54623);
#6715=VERTEX_POINT('',#54646);
#6716=VERTEX_POINT('',#54647);
#6717=VERTEX_POINT('',#54671);
#6718=VERTEX_POINT('',#54672);
#6719=VERTEX_POINT('',#54696);
#6720=VERTEX_POINT('',#54697);
#6721=VERTEX_POINT('',#54720);
#6722=VERTEX_POINT('',#54721);
#6723=VERTEX_POINT('',#54744);
#6724=VERTEX_POINT('',#54745);
#6725=VERTEX_POINT('',#54769);
#6726=VERTEX_POINT('',#54770);
#6727=VERTEX_POINT('',#54794);
#6728=VERTEX_POINT('',#54795);
#6729=VERTEX_POINT('',#54818);
#6730=VERTEX_POINT('',#54819);
#6731=VERTEX_POINT('',#54843);
#6732=VERTEX_POINT('',#54844);
#6733=VERTEX_POINT('',#54868);
#6734=VERTEX_POINT('',#54869);
#6735=VERTEX_POINT('',#54892);
#6736=VERTEX_POINT('',#54893);
#6737=VERTEX_POINT('',#54917);
#6738=VERTEX_POINT('',#54918);
#6739=VERTEX_POINT('',#54942);
#6740=VERTEX_POINT('',#54943);
#6741=VERTEX_POINT('',#54966);
#6742=VERTEX_POINT('',#54967);
#6743=VERTEX_POINT('',#54990);
#6744=VERTEX_POINT('',#54991);
#6745=VERTEX_POINT('',#55015);
#6746=VERTEX_POINT('',#55016);
#6747=VERTEX_POINT('',#55040);
#6748=VERTEX_POINT('',#55041);
#6749=VERTEX_POINT('',#55064);
#6750=VERTEX_POINT('',#55065);
#6751=VERTEX_POINT('',#55089);
#6752=VERTEX_POINT('',#55090);
#6753=VERTEX_POINT('',#55114);
#6754=VERTEX_POINT('',#55115);
#6755=VERTEX_POINT('',#55138);
#6756=VERTEX_POINT('',#55139);
#6757=VERTEX_POINT('',#55163);
#6758=VERTEX_POINT('',#55164);
#6759=VERTEX_POINT('',#55188);
#6760=VERTEX_POINT('',#55189);
#6761=VERTEX_POINT('',#55212);
#6762=VERTEX_POINT('',#55213);
#6763=VERTEX_POINT('',#55236);
#6764=VERTEX_POINT('',#55237);
#6765=VERTEX_POINT('',#55261);
#6766=VERTEX_POINT('',#55262);
#6767=VERTEX_POINT('',#55286);
#6768=VERTEX_POINT('',#55287);
#6769=VERTEX_POINT('',#55310);
#6770=VERTEX_POINT('',#55311);
#6771=VERTEX_POINT('',#55335);
#6772=VERTEX_POINT('',#55336);
#6773=VERTEX_POINT('',#55360);
#6774=VERTEX_POINT('',#55361);
#6775=VERTEX_POINT('',#55384);
#6776=VERTEX_POINT('',#55385);
#6777=VERTEX_POINT('',#55409);
#6778=VERTEX_POINT('',#55410);
#6779=VERTEX_POINT('',#55434);
#6780=VERTEX_POINT('',#55435);
#6781=VERTEX_POINT('',#55458);
#6782=VERTEX_POINT('',#55459);
#6783=VERTEX_POINT('',#55482);
#6784=VERTEX_POINT('',#55483);
#6785=VERTEX_POINT('',#55507);
#6786=VERTEX_POINT('',#55508);
#6787=VERTEX_POINT('',#55532);
#6788=VERTEX_POINT('',#55533);
#6789=VERTEX_POINT('',#55556);
#6790=VERTEX_POINT('',#55557);
#6791=VERTEX_POINT('',#55581);
#6792=VERTEX_POINT('',#55582);
#6793=VERTEX_POINT('',#55606);
#6794=VERTEX_POINT('',#55607);
#6795=VERTEX_POINT('',#55630);
#6796=VERTEX_POINT('',#55631);
#6797=VERTEX_POINT('',#55655);
#6798=VERTEX_POINT('',#55656);
#6799=VERTEX_POINT('',#55679);
#6800=VERTEX_POINT('',#55680);
#6801=VERTEX_POINT('',#55704);
#6802=VERTEX_POINT('',#55705);
#6803=VERTEX_POINT('',#55728);
#6804=VERTEX_POINT('',#55729);
#6805=VERTEX_POINT('',#55753);
#6806=VERTEX_POINT('',#55754);
#6807=VERTEX_POINT('',#55778);
#6808=VERTEX_POINT('',#55779);
#6809=VERTEX_POINT('',#55802);
#6810=VERTEX_POINT('',#55803);
#6811=VERTEX_POINT('',#55827);
#6812=VERTEX_POINT('',#55828);
#6813=VERTEX_POINT('',#55852);
#6814=VERTEX_POINT('',#55853);
#6815=VERTEX_POINT('',#55876);
#6816=VERTEX_POINT('',#55877);
#6817=VERTEX_POINT('',#55901);
#6818=VERTEX_POINT('',#55902);
#6819=VERTEX_POINT('',#55925);
#6820=VERTEX_POINT('',#55926);
#6821=VERTEX_POINT('',#55950);
#6822=VERTEX_POINT('',#55951);
#6823=VERTEX_POINT('',#57513);
#6824=VERTEX_POINT('',#57642);
#6825=VERTEX_POINT('',#57759);
#6826=VERTEX_POINT('',#59310);
#6827=VERTEX_POINT('',#59545);
#6828=VERTEX_POINT('',#59546);
#6829=VERTEX_POINT('',#59548);
#6830=VERTEX_POINT('',#59550);
#6831=VERTEX_POINT('',#59552);
#6832=VERTEX_POINT('',#59554);
#6833=VERTEX_POINT('',#59558);
#6834=VERTEX_POINT('',#59559);
#6835=VERTEX_POINT('',#59561);
#6836=VERTEX_POINT('',#59563);
#6837=VERTEX_POINT('',#59565);
#6838=VERTEX_POINT('',#59567);
#6839=VERTEX_POINT('',#59570);
#6840=VERTEX_POINT('',#59585);
#6841=VERTEX_POINT('',#59590);
#6842=VERTEX_POINT('',#59594);
#6843=VERTEX_POINT('',#59595);
#6844=VERTEX_POINT('',#59597);
#6845=VERTEX_POINT('',#59605);
#6846=VERTEX_POINT('',#59618);
#6847=VERTEX_POINT('',#59619);
#6848=VERTEX_POINT('',#59669);
#6849=VERTEX_POINT('',#59670);
#6850=VERTEX_POINT('',#59720);
#6851=VERTEX_POINT('',#59721);
#6852=VERTEX_POINT('',#59768);
#6853=VERTEX_POINT('',#59769);
#6854=VERTEX_POINT('',#59819);
#6855=VERTEX_POINT('',#59820);
#6856=VERTEX_POINT('',#59870);
#6857=VERTEX_POINT('',#59871);
#6858=VERTEX_POINT('',#59918);
#6859=VERTEX_POINT('',#59919);
#6860=VERTEX_POINT('',#59921);
#6861=VERTEX_POINT('',#59938);
#6862=VERTEX_POINT('',#59960);
#6863=VERTEX_POINT('',#59961);
#6864=VERTEX_POINT('',#59963);
#6865=VERTEX_POINT('',#59973);
#6866=VERTEX_POINT('',#59985);
#6867=VERTEX_POINT('',#59986);
#6868=VERTEX_POINT('',#60009);
#6869=VERTEX_POINT('',#60010);
#6870=VERTEX_POINT('',#60034);
#6871=VERTEX_POINT('',#60035);
#6872=VERTEX_POINT('',#60059);
#6873=VERTEX_POINT('',#60060);
#6874=VERTEX_POINT('',#60083);
#6875=VERTEX_POINT('',#60084);
#6876=VERTEX_POINT('',#60108);
#6877=VERTEX_POINT('',#60109);
#6878=VERTEX_POINT('',#60133);
#6879=VERTEX_POINT('',#60134);
#6880=VERTEX_POINT('',#60136);
#6881=VERTEX_POINT('',#60143);
#6882=VERTEX_POINT('',#61105);
#6883=VERTEX_POINT('',#61106);
#6884=VERTEX_POINT('',#61108);
#6885=VERTEX_POINT('',#61110);
#6886=VERTEX_POINT('',#61112);
#6887=VERTEX_POINT('',#61114);
#6888=VERTEX_POINT('',#61119);
#6889=VERTEX_POINT('',#61120);
#6890=VERTEX_POINT('',#61125);
#6891=VERTEX_POINT('',#61129);
#6892=VERTEX_POINT('',#61133);
#6893=VERTEX_POINT('',#61137);
#6894=VERTEX_POINT('',#61145);
#6895=VERTEX_POINT('',#61147);
#6896=VERTEX_POINT('',#61151);
#6897=VERTEX_POINT('',#61153);
#6898=VERTEX_POINT('',#61160);
#6899=VERTEX_POINT('',#61161);
#6900=VERTEX_POINT('',#61163);
#6901=VERTEX_POINT('',#61174);
#6902=VERTEX_POINT('',#61184);
#6903=VERTEX_POINT('',#61185);
#6904=VERTEX_POINT('',#61232);
#6905=VERTEX_POINT('',#61233);
#6906=VERTEX_POINT('',#61280);
#6907=VERTEX_POINT('',#61281);
#6908=VERTEX_POINT('',#61334);
#6909=VERTEX_POINT('',#61335);
#6910=VERTEX_POINT('',#61382);
#6911=VERTEX_POINT('',#61383);
#6912=VERTEX_POINT('',#61430);
#6913=VERTEX_POINT('',#61431);
#6914=VERTEX_POINT('',#61484);
#6915=VERTEX_POINT('',#61485);
#6916=VERTEX_POINT('',#61532);
#6917=VERTEX_POINT('',#61533);
#6918=VERTEX_POINT('',#61580);
#6919=VERTEX_POINT('',#61581);
#6920=VERTEX_POINT('',#61634);
#6921=VERTEX_POINT('',#61635);
#6922=VERTEX_POINT('',#61682);
#6923=VERTEX_POINT('',#61683);
#6924=VERTEX_POINT('',#61730);
#6925=VERTEX_POINT('',#61731);
#6926=VERTEX_POINT('',#61784);
#6927=VERTEX_POINT('',#61785);
#6928=VERTEX_POINT('',#61832);
#6929=VERTEX_POINT('',#61833);
#6930=VERTEX_POINT('',#61880);
#6931=VERTEX_POINT('',#61881);
#6932=VERTEX_POINT('',#61883);
#6933=VERTEX_POINT('',#61894);
#6934=VERTEX_POINT('',#61905);
#6935=VERTEX_POINT('',#61906);
#6936=VERTEX_POINT('',#61930);
#6937=VERTEX_POINT('',#61931);
#6938=VERTEX_POINT('',#61954);
#6939=VERTEX_POINT('',#61955);
#6940=VERTEX_POINT('',#61979);
#6941=VERTEX_POINT('',#61980);
#6942=VERTEX_POINT('',#62004);
#6943=VERTEX_POINT('',#62005);
#6944=VERTEX_POINT('',#62028);
#6945=VERTEX_POINT('',#62029);
#6946=VERTEX_POINT('',#62053);
#6947=VERTEX_POINT('',#62054);
#6948=VERTEX_POINT('',#62078);
#6949=VERTEX_POINT('',#62079);
#6950=VERTEX_POINT('',#62102);
#6951=VERTEX_POINT('',#62103);
#6952=VERTEX_POINT('',#62127);
#6953=VERTEX_POINT('',#62128);
#6954=VERTEX_POINT('',#62152);
#6955=VERTEX_POINT('',#62153);
#6956=VERTEX_POINT('',#62176);
#6957=VERTEX_POINT('',#62177);
#6958=VERTEX_POINT('',#62201);
#6959=VERTEX_POINT('',#62202);
#6960=VERTEX_POINT('',#62226);
#6961=VERTEX_POINT('',#62227);
#6962=VERTEX_POINT('',#62250);
#6963=VERTEX_POINT('',#62471);
#6964=VERTEX_POINT('',#62536);
#6965=VERTEX_POINT('',#62569);
#6966=VERTEX_POINT('',#62980);
#6967=VERTEX_POINT('',#63097);
#6968=VERTEX_POINT('',#63636);
#6969=VERTEX_POINT('',#63637);
#6970=VERTEX_POINT('',#63639);
#6971=VERTEX_POINT('',#63641);
#6972=VERTEX_POINT('',#63645);
#6973=VERTEX_POINT('',#63647);
#6974=VERTEX_POINT('',#63651);
#6975=VERTEX_POINT('',#63653);
#6976=VERTEX_POINT('',#63657);
#6977=VERTEX_POINT('',#63659);
#6978=VERTEX_POINT('',#63663);
#6979=VERTEX_POINT('',#63665);
#6980=VERTEX_POINT('',#63673);
#6981=VERTEX_POINT('',#63676);
#6982=VERTEX_POINT('',#63683);
#6983=VERTEX_POINT('',#63685);
#6984=VERTEX_POINT('',#63689);
#6985=VERTEX_POINT('',#63691);
#6986=EDGE_CURVE('',#5558,#5559,#3886,.T.);
#6987=EDGE_CURVE('',#5559,#5560,#3887,.T.);
#6988=EDGE_CURVE('',#5561,#5560,#3888,.T.);
#6989=EDGE_CURVE('',#5558,#5561,#3889,.T.);
#6990=EDGE_CURVE('',#5562,#5558,#3890,.T.);
#6991=EDGE_CURVE('',#5563,#5561,#3891,.T.);
#6992=EDGE_CURVE('',#5562,#5563,#3892,.T.);
#6993=EDGE_CURVE('',#5564,#5562,#3893,.T.);
#6994=EDGE_CURVE('',#5565,#5563,#3894,.T.);
#6995=EDGE_CURVE('',#5564,#5565,#3895,.T.);
#6996=EDGE_CURVE('',#5559,#5564,#3896,.T.);
#6997=EDGE_CURVE('',#5560,#5565,#3897,.T.);
#6998=EDGE_CURVE('',#5566,#5567,#3898,.T.);
#6999=EDGE_CURVE('',#5567,#5568,#3899,.T.);
#7000=EDGE_CURVE('',#5569,#5568,#3900,.T.);
#7001=EDGE_CURVE('',#5566,#5569,#3901,.T.);
#7002=EDGE_CURVE('',#5570,#5566,#3902,.T.);
#7003=EDGE_CURVE('',#5571,#5569,#3903,.T.);
#7004=EDGE_CURVE('',#5570,#5571,#3904,.T.);
#7005=EDGE_CURVE('',#5572,#5570,#3905,.T.);
#7006=EDGE_CURVE('',#5573,#5571,#3906,.T.);
#7007=EDGE_CURVE('',#5572,#5573,#3907,.T.);
#7008=EDGE_CURVE('',#5567,#5572,#3908,.T.);
#7009=EDGE_CURVE('',#5568,#5573,#3909,.T.);
#7010=EDGE_CURVE('',#5574,#5575,#3910,.T.);
#7011=EDGE_CURVE('',#5575,#5576,#3911,.T.);
#7012=EDGE_CURVE('',#5577,#5576,#3912,.T.);
#7013=EDGE_CURVE('',#5574,#5577,#3913,.T.);
#7014=EDGE_CURVE('',#5578,#5574,#3914,.T.);
#7015=EDGE_CURVE('',#5579,#5577,#3915,.T.);
#7016=EDGE_CURVE('',#5578,#5579,#3916,.T.);
#7017=EDGE_CURVE('',#5580,#5578,#3917,.T.);
#7018=EDGE_CURVE('',#5581,#5579,#3918,.T.);
#7019=EDGE_CURVE('',#5580,#5581,#3919,.T.);
#7020=EDGE_CURVE('',#5575,#5580,#3920,.T.);
#7021=EDGE_CURVE('',#5576,#5581,#3921,.T.);
#7022=EDGE_CURVE('',#5582,#5583,#3922,.T.);
#7023=EDGE_CURVE('',#5583,#5584,#3923,.T.);
#7024=EDGE_CURVE('',#5585,#5584,#3924,.T.);
#7025=EDGE_CURVE('',#5582,#5585,#3925,.T.);
#7026=EDGE_CURVE('',#5586,#5582,#3926,.T.);
#7027=EDGE_CURVE('',#5587,#5585,#3927,.T.);
#7028=EDGE_CURVE('',#5586,#5587,#3928,.T.);
#7029=EDGE_CURVE('',#5588,#5586,#3929,.T.);
#7030=EDGE_CURVE('',#5589,#5587,#3930,.T.);
#7031=EDGE_CURVE('',#5588,#5589,#3931,.T.);
#7032=EDGE_CURVE('',#5583,#5588,#3932,.T.);
#7033=EDGE_CURVE('',#5584,#5589,#3933,.T.);
#7034=EDGE_CURVE('',#5590,#5591,#3934,.T.);
#7035=EDGE_CURVE('',#5591,#5592,#487,.T.);
#7036=EDGE_CURVE('',#5593,#5592,#285,.F.);
#7037=EDGE_CURVE('',#5593,#5590,#488,.T.);
#7038=EDGE_CURVE('',#5594,#5595,#3935,.T.);
#7039=EDGE_CURVE('',#5595,#5591,#489,.T.);
#7040=EDGE_CURVE('',#5590,#5594,#490,.T.);
#7041=EDGE_CURVE('',#5596,#5597,#3936,.T.);
#7042=EDGE_CURVE('',#5597,#5595,#491,.T.);
#7043=EDGE_CURVE('',#5594,#5596,#492,.T.);
#7044=EDGE_CURVE('',#5598,#5599,#3937,.T.);
#7045=EDGE_CURVE('',#5599,#5597,#493,.T.);
#7046=EDGE_CURVE('',#5596,#5598,#494,.T.);
#7047=EDGE_CURVE('',#5600,#5601,#3938,.T.);
#7048=EDGE_CURVE('',#5601,#5599,#495,.T.);
#7049=EDGE_CURVE('',#5598,#5600,#496,.T.);
#7050=EDGE_CURVE('',#5602,#5603,#3939,.T.);
#7051=EDGE_CURVE('',#5603,#5601,#497,.T.);
#7052=EDGE_CURVE('',#5600,#5602,#498,.T.);
#7053=EDGE_CURVE('',#5604,#5605,#3940,.T.);
#7054=EDGE_CURVE('',#5605,#5603,#499,.T.);
#7055=EDGE_CURVE('',#5602,#5604,#500,.T.);
#7056=EDGE_CURVE('',#5606,#5607,#3941,.T.);
#7057=EDGE_CURVE('',#5606,#5608,#501,.T.);
#7058=EDGE_CURVE('',#5609,#5608,#286,.T.);
#7059=EDGE_CURVE('',#5609,#5607,#502,.T.);
#7060=EDGE_CURVE('',#5610,#5611,#3942,.T.);
#7061=EDGE_CURVE('',#5611,#5612,#503,.T.);
#7062=EDGE_CURVE('',#5613,#5612,#287,.F.);
#7063=EDGE_CURVE('',#5613,#5610,#504,.T.);
#7064=EDGE_CURVE('',#5614,#5615,#3943,.T.);
#7065=EDGE_CURVE('',#5615,#5611,#505,.T.);
#7066=EDGE_CURVE('',#5610,#5614,#506,.T.);
#7067=EDGE_CURVE('',#5616,#5617,#3944,.T.);
#7068=EDGE_CURVE('',#5617,#5615,#507,.T.);
#7069=EDGE_CURVE('',#5614,#5616,#508,.T.);
#7070=EDGE_CURVE('',#5618,#5619,#3945,.T.);
#7071=EDGE_CURVE('',#5619,#5617,#509,.T.);
#7072=EDGE_CURVE('',#5616,#5618,#510,.T.);
#7073=EDGE_CURVE('',#5620,#5621,#3946,.T.);
#7074=EDGE_CURVE('',#5621,#5619,#511,.T.);
#7075=EDGE_CURVE('',#5618,#5620,#512,.T.);
#7076=EDGE_CURVE('',#5622,#5623,#3947,.T.);
#7077=EDGE_CURVE('',#5623,#5621,#513,.T.);
#7078=EDGE_CURVE('',#5620,#5622,#514,.T.);
#7079=EDGE_CURVE('',#5624,#5625,#3948,.T.);
#7080=EDGE_CURVE('',#5625,#5623,#515,.T.);
#7081=EDGE_CURVE('',#5622,#5624,#516,.T.);
#7082=EDGE_CURVE('',#5626,#5627,#3949,.T.);
#7083=EDGE_CURVE('',#5626,#5628,#517,.T.);
#7084=EDGE_CURVE('',#5629,#5628,#288,.T.);
#7085=EDGE_CURVE('',#5629,#5627,#518,.T.);
#7086=EDGE_CURVE('',#5630,#5631,#3950,.T.);
#7087=EDGE_CURVE('',#5631,#5632,#519,.T.);
#7088=EDGE_CURVE('',#5633,#5632,#289,.F.);
#7089=EDGE_CURVE('',#5633,#5630,#520,.T.);
#7090=EDGE_CURVE('',#5634,#5635,#3951,.T.);
#7091=EDGE_CURVE('',#5635,#5631,#521,.T.);
#7092=EDGE_CURVE('',#5630,#5634,#522,.T.);
#7093=EDGE_CURVE('',#5636,#5637,#3952,.T.);
#7094=EDGE_CURVE('',#5637,#5635,#523,.T.);
#7095=EDGE_CURVE('',#5634,#5636,#524,.T.);
#7096=EDGE_CURVE('',#5638,#5639,#3953,.T.);
#7097=EDGE_CURVE('',#5639,#5637,#525,.T.);
#7098=EDGE_CURVE('',#5636,#5638,#526,.T.);
#7099=EDGE_CURVE('',#5640,#5641,#3954,.T.);
#7100=EDGE_CURVE('',#5641,#5639,#527,.T.);
#7101=EDGE_CURVE('',#5638,#5640,#528,.T.);
#7102=EDGE_CURVE('',#5642,#5643,#3955,.T.);
#7103=EDGE_CURVE('',#5643,#5641,#529,.T.);
#7104=EDGE_CURVE('',#5640,#5642,#530,.T.);
#7105=EDGE_CURVE('',#5644,#5645,#3956,.T.);
#7106=EDGE_CURVE('',#5645,#5643,#531,.T.);
#7107=EDGE_CURVE('',#5642,#5644,#532,.T.);
#7108=EDGE_CURVE('',#5646,#5647,#3957,.T.);
#7109=EDGE_CURVE('',#5646,#5648,#533,.T.);
#7110=EDGE_CURVE('',#5649,#5648,#290,.T.);
#7111=EDGE_CURVE('',#5649,#5647,#534,.T.);
#7112=EDGE_CURVE('',#5650,#5651,#3958,.T.);
#7113=EDGE_CURVE('',#5651,#5652,#535,.T.);
#7114=EDGE_CURVE('',#5653,#5652,#291,.F.);
#7115=EDGE_CURVE('',#5653,#5650,#536,.T.);
#7116=EDGE_CURVE('',#5654,#5655,#3959,.T.);
#7117=EDGE_CURVE('',#5655,#5651,#537,.T.);
#7118=EDGE_CURVE('',#5650,#5654,#538,.T.);
#7119=EDGE_CURVE('',#5656,#5657,#3960,.T.);
#7120=EDGE_CURVE('',#5657,#5655,#539,.T.);
#7121=EDGE_CURVE('',#5654,#5656,#540,.T.);
#7122=EDGE_CURVE('',#5658,#5659,#3961,.T.);
#7123=EDGE_CURVE('',#5659,#5657,#541,.T.);
#7124=EDGE_CURVE('',#5656,#5658,#542,.T.);
#7125=EDGE_CURVE('',#5660,#5661,#3962,.T.);
#7126=EDGE_CURVE('',#5661,#5659,#543,.T.);
#7127=EDGE_CURVE('',#5658,#5660,#544,.T.);
#7128=EDGE_CURVE('',#5662,#5663,#3963,.T.);
#7129=EDGE_CURVE('',#5663,#5661,#545,.T.);
#7130=EDGE_CURVE('',#5660,#5662,#546,.T.);
#7131=EDGE_CURVE('',#5664,#5665,#3964,.T.);
#7132=EDGE_CURVE('',#5665,#5663,#547,.T.);
#7133=EDGE_CURVE('',#5662,#5664,#548,.T.);
#7134=EDGE_CURVE('',#5666,#5667,#3965,.T.);
#7135=EDGE_CURVE('',#5666,#5668,#549,.T.);
#7136=EDGE_CURVE('',#5669,#5668,#292,.T.);
#7137=EDGE_CURVE('',#5669,#5667,#550,.T.);
#7138=EDGE_CURVE('',#5670,#5671,#3966,.T.);
#7139=EDGE_CURVE('',#5671,#5672,#551,.T.);
#7140=EDGE_CURVE('',#5673,#5672,#293,.T.);
#7141=EDGE_CURVE('',#5670,#5673,#552,.T.);
#7142=EDGE_CURVE('',#5674,#5675,#3967,.T.);
#7143=EDGE_CURVE('',#5675,#5671,#553,.T.);
#7144=EDGE_CURVE('',#5674,#5670,#554,.T.);
#7145=EDGE_CURVE('',#5676,#5677,#3968,.T.);
#7146=EDGE_CURVE('',#5677,#5675,#555,.T.);
#7147=EDGE_CURVE('',#5676,#5674,#556,.T.);
#7148=EDGE_CURVE('',#5678,#5679,#3969,.T.);
#7149=EDGE_CURVE('',#5679,#5677,#557,.T.);
#7150=EDGE_CURVE('',#5678,#5676,#558,.T.);
#7151=EDGE_CURVE('',#5680,#5681,#3970,.T.);
#7152=EDGE_CURVE('',#5681,#5679,#559,.T.);
#7153=EDGE_CURVE('',#5680,#5678,#560,.T.);
#7154=EDGE_CURVE('',#5682,#5683,#3971,.T.);
#7155=EDGE_CURVE('',#5683,#5681,#561,.T.);
#7156=EDGE_CURVE('',#5682,#5680,#562,.T.);
#7157=EDGE_CURVE('',#5684,#5685,#3972,.T.);
#7158=EDGE_CURVE('',#5685,#5683,#563,.T.);
#7159=EDGE_CURVE('',#5684,#5682,#564,.T.);
#7160=EDGE_CURVE('',#5686,#5687,#3973,.T.);
#7161=EDGE_CURVE('',#5688,#5686,#565,.T.);
#7162=EDGE_CURVE('',#5689,#5688,#294,.T.);
#7163=EDGE_CURVE('',#5689,#5687,#566,.T.);
#7164=EDGE_CURVE('',#5690,#5691,#3974,.T.);
#7165=EDGE_CURVE('',#5691,#5692,#567,.T.);
#7166=EDGE_CURVE('',#5693,#5692,#295,.T.);
#7167=EDGE_CURVE('',#5690,#5693,#568,.T.);
#7168=EDGE_CURVE('',#5694,#5695,#3975,.T.);
#7169=EDGE_CURVE('',#5695,#5691,#569,.T.);
#7170=EDGE_CURVE('',#5694,#5690,#570,.T.);
#7171=EDGE_CURVE('',#5696,#5697,#3976,.T.);
#7172=EDGE_CURVE('',#5697,#5695,#571,.T.);
#7173=EDGE_CURVE('',#5696,#5694,#572,.T.);
#7174=EDGE_CURVE('',#5698,#5699,#3977,.T.);
#7175=EDGE_CURVE('',#5699,#5697,#573,.T.);
#7176=EDGE_CURVE('',#5698,#5696,#574,.T.);
#7177=EDGE_CURVE('',#5700,#5701,#3978,.T.);
#7178=EDGE_CURVE('',#5701,#5699,#575,.T.);
#7179=EDGE_CURVE('',#5700,#5698,#576,.T.);
#7180=EDGE_CURVE('',#5702,#5703,#3979,.T.);
#7181=EDGE_CURVE('',#5703,#5701,#577,.T.);
#7182=EDGE_CURVE('',#5702,#5700,#578,.T.);
#7183=EDGE_CURVE('',#5704,#5705,#3980,.T.);
#7184=EDGE_CURVE('',#5705,#5703,#579,.T.);
#7185=EDGE_CURVE('',#5704,#5702,#580,.T.);
#7186=EDGE_CURVE('',#5706,#5707,#3981,.T.);
#7187=EDGE_CURVE('',#5708,#5706,#581,.T.);
#7188=EDGE_CURVE('',#5709,#5708,#296,.T.);
#7189=EDGE_CURVE('',#5709,#5707,#582,.T.);
#7190=EDGE_CURVE('',#5710,#5711,#3982,.T.);
#7191=EDGE_CURVE('',#5711,#5712,#583,.T.);
#7192=EDGE_CURVE('',#5713,#5712,#297,.T.);
#7193=EDGE_CURVE('',#5710,#5713,#584,.T.);
#7194=EDGE_CURVE('',#5714,#5715,#3983,.T.);
#7195=EDGE_CURVE('',#5715,#5711,#585,.T.);
#7196=EDGE_CURVE('',#5714,#5710,#586,.T.);
#7197=EDGE_CURVE('',#5716,#5717,#3984,.T.);
#7198=EDGE_CURVE('',#5717,#5715,#587,.T.);
#7199=EDGE_CURVE('',#5716,#5714,#588,.T.);
#7200=EDGE_CURVE('',#5718,#5719,#3985,.T.);
#7201=EDGE_CURVE('',#5719,#5717,#589,.T.);
#7202=EDGE_CURVE('',#5718,#5716,#590,.T.);
#7203=EDGE_CURVE('',#5720,#5721,#3986,.T.);
#7204=EDGE_CURVE('',#5721,#5719,#591,.T.);
#7205=EDGE_CURVE('',#5720,#5718,#592,.T.);
#7206=EDGE_CURVE('',#5722,#5723,#3987,.T.);
#7207=EDGE_CURVE('',#5723,#5721,#593,.T.);
#7208=EDGE_CURVE('',#5722,#5720,#594,.T.);
#7209=EDGE_CURVE('',#5724,#5725,#3988,.T.);
#7210=EDGE_CURVE('',#5725,#5723,#595,.T.);
#7211=EDGE_CURVE('',#5724,#5722,#596,.T.);
#7212=EDGE_CURVE('',#5726,#5727,#3989,.T.);
#7213=EDGE_CURVE('',#5728,#5726,#597,.T.);
#7214=EDGE_CURVE('',#5729,#5728,#298,.T.);
#7215=EDGE_CURVE('',#5729,#5727,#598,.T.);
#7216=EDGE_CURVE('',#5730,#5731,#3990,.T.);
#7217=EDGE_CURVE('',#5731,#5732,#599,.T.);
#7218=EDGE_CURVE('',#5733,#5732,#299,.T.);
#7219=EDGE_CURVE('',#5730,#5733,#600,.T.);
#7220=EDGE_CURVE('',#5734,#5735,#3991,.T.);
#7221=EDGE_CURVE('',#5735,#5731,#601,.T.);
#7222=EDGE_CURVE('',#5734,#5730,#602,.T.);
#7223=EDGE_CURVE('',#5736,#5737,#3992,.T.);
#7224=EDGE_CURVE('',#5737,#5735,#603,.T.);
#7225=EDGE_CURVE('',#5736,#5734,#604,.T.);
#7226=EDGE_CURVE('',#5738,#5739,#3993,.T.);
#7227=EDGE_CURVE('',#5739,#5737,#605,.T.);
#7228=EDGE_CURVE('',#5738,#5736,#606,.T.);
#7229=EDGE_CURVE('',#5740,#5741,#3994,.T.);
#7230=EDGE_CURVE('',#5741,#5739,#607,.T.);
#7231=EDGE_CURVE('',#5740,#5738,#608,.T.);
#7232=EDGE_CURVE('',#5742,#5743,#3995,.T.);
#7233=EDGE_CURVE('',#5743,#5741,#609,.T.);
#7234=EDGE_CURVE('',#5742,#5740,#610,.T.);
#7235=EDGE_CURVE('',#5744,#5745,#3996,.T.);
#7236=EDGE_CURVE('',#5745,#5743,#611,.T.);
#7237=EDGE_CURVE('',#5744,#5742,#612,.T.);
#7238=EDGE_CURVE('',#5746,#5747,#3997,.T.);
#7239=EDGE_CURVE('',#5748,#5746,#613,.T.);
#7240=EDGE_CURVE('',#5749,#5748,#300,.T.);
#7241=EDGE_CURVE('',#5749,#5747,#614,.T.);
#7242=EDGE_CURVE('',#5747,#5745,#615,.T.);
#7243=EDGE_CURVE('',#5746,#5744,#616,.T.);
#7244=EDGE_CURVE('',#5732,#5653,#617,.T.);
#7245=EDGE_CURVE('',#5668,#5749,#618,.T.);
#7246=EDGE_CURVE('',#5664,#5666,#619,.T.);
#7247=EDGE_CURVE('',#5652,#5733,#620,.T.);
#7248=EDGE_CURVE('',#5667,#5665,#621,.T.);
#7249=EDGE_CURVE('',#5748,#5669,#622,.T.);
#7250=EDGE_CURVE('',#5750,#5751,#3998,.T.);
#7251=EDGE_CURVE('',#5751,#5752,#3999,.T.);
#7252=EDGE_CURVE('',#5752,#5753,#4000,.T.);
#7253=EDGE_CURVE('',#5753,#5750,#4001,.T.);
#7254=EDGE_CURVE('',#5648,#5729,#623,.T.);
#7255=EDGE_CURVE('',#5728,#5649,#624,.T.);
#7256=EDGE_CURVE('',#5628,#5689,#625,.T.);
#7257=EDGE_CURVE('',#5688,#5629,#626,.T.);
#7258=EDGE_CURVE('',#5608,#5709,#627,.T.);
#7259=EDGE_CURVE('',#5708,#5609,#628,.T.);
#7260=EDGE_CURVE('',#5727,#5725,#629,.T.);
#7261=EDGE_CURVE('',#5726,#5724,#630,.T.);
#7262=EDGE_CURVE('',#5712,#5633,#631,.T.);
#7263=EDGE_CURVE('',#5644,#5646,#632,.T.);
#7264=EDGE_CURVE('',#5632,#5713,#633,.T.);
#7265=EDGE_CURVE('',#5647,#5645,#634,.T.);
#7266=EDGE_CURVE('',#5707,#5705,#635,.T.);
#7267=EDGE_CURVE('',#5706,#5704,#636,.T.);
#7268=EDGE_CURVE('',#5692,#5593,#637,.T.);
#7269=EDGE_CURVE('',#5604,#5606,#638,.T.);
#7270=EDGE_CURVE('',#5592,#5693,#639,.T.);
#7271=EDGE_CURVE('',#5607,#5605,#640,.T.);
#7272=EDGE_CURVE('',#5687,#5685,#641,.T.);
#7273=EDGE_CURVE('',#5686,#5684,#642,.T.);
#7274=EDGE_CURVE('',#5672,#5613,#643,.T.);
#7275=EDGE_CURVE('',#5624,#5626,#644,.T.);
#7276=EDGE_CURVE('',#5612,#5673,#645,.T.);
#7277=EDGE_CURVE('',#5627,#5625,#646,.T.);
#7278=EDGE_CURVE('',#5754,#5755,#4002,.T.);
#7279=EDGE_CURVE('',#5755,#5750,#4003,.T.);
#7280=EDGE_CURVE('',#5754,#5753,#4004,.T.);
#7281=EDGE_CURVE('',#5756,#5754,#4005,.T.);
#7282=EDGE_CURVE('',#5756,#5752,#4006,.T.);
#7283=EDGE_CURVE('',#5757,#5756,#4007,.T.);
#7284=EDGE_CURVE('',#5757,#5751,#4008,.T.);
#7285=EDGE_CURVE('',#5755,#5757,#4009,.T.);
#7286=EDGE_CURVE('',#5758,#5759,#4010,.T.);
#7287=EDGE_CURVE('',#5758,#5760,#647,.T.);
#7288=EDGE_CURVE('',#5760,#5761,#301,.F.);
#7289=EDGE_CURVE('',#5761,#5759,#648,.T.);
#7290=EDGE_CURVE('',#5762,#5763,#4011,.T.);
#7291=EDGE_CURVE('',#5762,#5758,#649,.T.);
#7292=EDGE_CURVE('',#5759,#5763,#650,.T.);
#7293=EDGE_CURVE('',#5764,#5765,#4012,.T.);
#7294=EDGE_CURVE('',#5764,#5762,#651,.T.);
#7295=EDGE_CURVE('',#5763,#5765,#652,.T.);
#7296=EDGE_CURVE('',#5766,#5767,#4013,.T.);
#7297=EDGE_CURVE('',#5766,#5764,#653,.T.);
#7298=EDGE_CURVE('',#5765,#5767,#654,.T.);
#7299=EDGE_CURVE('',#5768,#5769,#4014,.T.);
#7300=EDGE_CURVE('',#5768,#5766,#655,.T.);
#7301=EDGE_CURVE('',#5767,#5769,#656,.T.);
#7302=EDGE_CURVE('',#5770,#5771,#4015,.T.);
#7303=EDGE_CURVE('',#5770,#5768,#657,.T.);
#7304=EDGE_CURVE('',#5769,#5771,#658,.T.);
#7305=EDGE_CURVE('',#5772,#5773,#4016,.T.);
#7306=EDGE_CURVE('',#5772,#5770,#659,.T.);
#7307=EDGE_CURVE('',#5771,#5773,#660,.T.);
#7308=EDGE_CURVE('',#5774,#5775,#4017,.T.);
#7309=EDGE_CURVE('',#5774,#5772,#661,.T.);
#7310=EDGE_CURVE('',#5773,#5775,#662,.T.);
#7311=EDGE_CURVE('',#5776,#5777,#4018,.T.);
#7312=EDGE_CURVE('',#5776,#5774,#663,.T.);
#7313=EDGE_CURVE('',#5775,#5777,#664,.T.);
#7314=EDGE_CURVE('',#5778,#5779,#4019,.T.);
#7315=EDGE_CURVE('',#5778,#5776,#665,.T.);
#7316=EDGE_CURVE('',#5777,#5779,#666,.T.);
#7317=EDGE_CURVE('',#5780,#5781,#4020,.T.);
#7318=EDGE_CURVE('',#5780,#5778,#667,.T.);
#7319=EDGE_CURVE('',#5779,#5781,#668,.T.);
#7320=EDGE_CURVE('',#5782,#5783,#4021,.T.);
#7321=EDGE_CURVE('',#5782,#5780,#669,.T.);
#7322=EDGE_CURVE('',#5781,#5783,#670,.T.);
#7323=EDGE_CURVE('',#5784,#5785,#4022,.T.);
#7324=EDGE_CURVE('',#5784,#5782,#671,.T.);
#7325=EDGE_CURVE('',#5783,#5785,#672,.T.);
#7326=EDGE_CURVE('',#5786,#5787,#4023,.T.);
#7327=EDGE_CURVE('',#5786,#5784,#673,.T.);
#7328=EDGE_CURVE('',#5785,#5787,#674,.T.);
#7329=EDGE_CURVE('',#5788,#5789,#4024,.T.);
#7330=EDGE_CURVE('',#5788,#5786,#675,.T.);
#7331=EDGE_CURVE('',#5787,#5789,#676,.T.);
#7332=EDGE_CURVE('',#5790,#5791,#4025,.T.);
#7333=EDGE_CURVE('',#5790,#5788,#677,.T.);
#7334=EDGE_CURVE('',#5789,#5791,#678,.T.);
#7335=EDGE_CURVE('',#5792,#5793,#4026,.T.);
#7336=EDGE_CURVE('',#5792,#5790,#679,.T.);
#7337=EDGE_CURVE('',#5791,#5793,#680,.T.);
#7338=EDGE_CURVE('',#5794,#5795,#4027,.T.);
#7339=EDGE_CURVE('',#5794,#5792,#681,.T.);
#7340=EDGE_CURVE('',#5793,#5795,#682,.T.);
#7341=EDGE_CURVE('',#5796,#5797,#4028,.T.);
#7342=EDGE_CURVE('',#5796,#5794,#683,.T.);
#7343=EDGE_CURVE('',#5795,#5797,#684,.T.);
#7344=EDGE_CURVE('',#5798,#5799,#4029,.T.);
#7345=EDGE_CURVE('',#5798,#5796,#685,.T.);
#7346=EDGE_CURVE('',#5797,#5799,#686,.T.);
#7347=EDGE_CURVE('',#5800,#5801,#4030,.T.);
#7348=EDGE_CURVE('',#5800,#5798,#687,.T.);
#7349=EDGE_CURVE('',#5799,#5801,#688,.T.);
#7350=EDGE_CURVE('',#5802,#5803,#4031,.T.);
#7351=EDGE_CURVE('',#5802,#5800,#689,.T.);
#7352=EDGE_CURVE('',#5801,#5803,#690,.T.);
#7353=EDGE_CURVE('',#5804,#5805,#4032,.T.);
#7354=EDGE_CURVE('',#5804,#5802,#691,.T.);
#7355=EDGE_CURVE('',#5803,#5805,#692,.T.);
#7356=EDGE_CURVE('',#5806,#5807,#4033,.T.);
#7357=EDGE_CURVE('',#5806,#5804,#693,.T.);
#7358=EDGE_CURVE('',#5805,#5807,#694,.T.);
#7359=EDGE_CURVE('',#5808,#5809,#4034,.T.);
#7360=EDGE_CURVE('',#5808,#5810,#695,.T.);
#7361=EDGE_CURVE('',#5810,#5811,#302,.T.);
#7362=EDGE_CURVE('',#5809,#5811,#696,.T.);
#7363=EDGE_CURVE('',#5812,#5813,#4035,.T.);
#7364=EDGE_CURVE('',#5812,#5808,#697,.T.);
#7365=EDGE_CURVE('',#5813,#5809,#698,.T.);
#7366=EDGE_CURVE('',#5814,#5815,#4036,.T.);
#7367=EDGE_CURVE('',#5814,#5812,#699,.T.);
#7368=EDGE_CURVE('',#5815,#5813,#700,.T.);
#7369=EDGE_CURVE('',#5816,#5817,#4037,.T.);
#7370=EDGE_CURVE('',#5816,#5814,#701,.T.);
#7371=EDGE_CURVE('',#5817,#5815,#702,.T.);
#7372=EDGE_CURVE('',#5818,#5819,#4038,.T.);
#7373=EDGE_CURVE('',#5818,#5816,#703,.T.);
#7374=EDGE_CURVE('',#5819,#5817,#704,.T.);
#7375=EDGE_CURVE('',#5820,#5821,#4039,.T.);
#7376=EDGE_CURVE('',#5820,#5818,#705,.T.);
#7377=EDGE_CURVE('',#5821,#5819,#706,.T.);
#7378=EDGE_CURVE('',#5822,#5823,#4040,.T.);
#7379=EDGE_CURVE('',#5822,#5820,#707,.T.);
#7380=EDGE_CURVE('',#5823,#5821,#708,.T.);
#7381=EDGE_CURVE('',#5824,#5825,#4041,.T.);
#7382=EDGE_CURVE('',#5824,#5822,#709,.T.);
#7383=EDGE_CURVE('',#5825,#5823,#710,.T.);
#7384=EDGE_CURVE('',#5826,#5827,#4042,.T.);
#7385=EDGE_CURVE('',#5826,#5824,#711,.T.);
#7386=EDGE_CURVE('',#5827,#5825,#712,.T.);
#7387=EDGE_CURVE('',#5828,#5829,#4043,.T.);
#7388=EDGE_CURVE('',#5828,#5826,#713,.T.);
#7389=EDGE_CURVE('',#5829,#5827,#714,.T.);
#7390=EDGE_CURVE('',#5830,#5831,#4044,.T.);
#7391=EDGE_CURVE('',#5830,#5828,#715,.T.);
#7392=EDGE_CURVE('',#5831,#5829,#716,.T.);
#7393=EDGE_CURVE('',#5832,#5833,#4045,.T.);
#7394=EDGE_CURVE('',#5832,#5830,#717,.T.);
#7395=EDGE_CURVE('',#5833,#5831,#718,.T.);
#7396=EDGE_CURVE('',#5834,#5835,#4046,.T.);
#7397=EDGE_CURVE('',#5834,#5832,#719,.T.);
#7398=EDGE_CURVE('',#5835,#5833,#720,.T.);
#7399=EDGE_CURVE('',#5836,#5837,#4047,.T.);
#7400=EDGE_CURVE('',#5836,#5834,#721,.T.);
#7401=EDGE_CURVE('',#5837,#5835,#722,.T.);
#7402=EDGE_CURVE('',#5838,#5839,#4048,.T.);
#7403=EDGE_CURVE('',#5838,#5836,#723,.T.);
#7404=EDGE_CURVE('',#5839,#5837,#724,.T.);
#7405=EDGE_CURVE('',#5840,#5841,#4049,.T.);
#7406=EDGE_CURVE('',#5840,#5838,#725,.T.);
#7407=EDGE_CURVE('',#5841,#5839,#726,.T.);
#7408=EDGE_CURVE('',#5842,#5843,#4050,.T.);
#7409=EDGE_CURVE('',#5842,#5840,#727,.T.);
#7410=EDGE_CURVE('',#5843,#5841,#728,.T.);
#7411=EDGE_CURVE('',#5844,#5845,#4051,.T.);
#7412=EDGE_CURVE('',#5844,#5842,#729,.T.);
#7413=EDGE_CURVE('',#5845,#5843,#730,.T.);
#7414=EDGE_CURVE('',#5846,#5847,#4052,.T.);
#7415=EDGE_CURVE('',#5846,#5844,#731,.T.);
#7416=EDGE_CURVE('',#5847,#5845,#732,.T.);
#7417=EDGE_CURVE('',#5848,#5849,#4053,.T.);
#7418=EDGE_CURVE('',#5848,#5846,#733,.T.);
#7419=EDGE_CURVE('',#5849,#5847,#734,.T.);
#7420=EDGE_CURVE('',#5850,#5851,#4054,.T.);
#7421=EDGE_CURVE('',#5850,#5848,#735,.T.);
#7422=EDGE_CURVE('',#5851,#5849,#736,.T.);
#7423=EDGE_CURVE('',#5852,#5853,#4055,.T.);
#7424=EDGE_CURVE('',#5852,#5850,#737,.T.);
#7425=EDGE_CURVE('',#5853,#5851,#738,.T.);
#7426=EDGE_CURVE('',#5854,#5855,#4056,.T.);
#7427=EDGE_CURVE('',#5854,#5852,#739,.T.);
#7428=EDGE_CURVE('',#5855,#5853,#740,.T.);
#7429=EDGE_CURVE('',#5856,#5857,#4057,.T.);
#7430=EDGE_CURVE('',#5856,#5854,#741,.T.);
#7431=EDGE_CURVE('',#5857,#5855,#742,.T.);
#7432=EDGE_CURVE('',#5811,#5858,#743,.T.);
#7433=EDGE_CURVE('',#5859,#5810,#744,.T.);
#7434=EDGE_CURVE('',#5860,#5859,#303,.T.);
#7435=EDGE_CURVE('',#5858,#5860,#745,.T.);
#7436=EDGE_CURVE('',#5858,#5861,#4058,.T.);
#7437=EDGE_CURVE('',#5861,#5861,#304,.T.);
#7438=EDGE_CURVE('',#5862,#5856,#746,.T.);
#7439=EDGE_CURVE('',#5760,#5862,#747,.T.);
#7440=EDGE_CURVE('',#5859,#5806,#748,.T.);
#7441=EDGE_CURVE('',#5863,#5857,#749,.T.);
#7442=EDGE_CURVE('',#5862,#5863,#305,.T.);
#7443=EDGE_CURVE('',#5807,#5860,#750,.T.);
#7444=EDGE_CURVE('',#5863,#5761,#751,.T.);
#7445=EDGE_CURVE('',#5864,#5865,#4059,.T.);
#7446=EDGE_CURVE('',#5864,#5866,#4060,.T.);
#7447=EDGE_CURVE('',#5866,#5867,#4061,.T.);
#7448=EDGE_CURVE('',#5865,#5867,#4062,.T.);
#7449=EDGE_CURVE('',#5868,#5864,#4063,.T.);
#7450=EDGE_CURVE('',#5868,#5869,#4064,.T.);
#7451=EDGE_CURVE('',#5869,#5866,#4065,.T.);
#7452=EDGE_CURVE('',#5870,#5868,#4066,.T.);
#7453=EDGE_CURVE('',#5870,#5871,#4067,.T.);
#7454=EDGE_CURVE('',#5871,#5869,#4068,.T.);
#7455=EDGE_CURVE('',#5872,#5870,#4069,.T.);
#7456=EDGE_CURVE('',#5872,#5873,#4070,.T.);
#7457=EDGE_CURVE('',#5873,#5871,#4071,.T.);
#7458=EDGE_CURVE('',#5874,#5872,#4072,.T.);
#7459=EDGE_CURVE('',#5874,#5875,#4073,.T.);
#7460=EDGE_CURVE('',#5875,#5873,#4074,.T.);
#7461=EDGE_CURVE('',#5865,#5874,#4075,.T.);
#7462=EDGE_CURVE('',#5867,#5875,#4076,.T.);
#7463=EDGE_CURVE('',#5876,#5876,#306,.T.);
#7464=EDGE_CURVE('',#5876,#5877,#4077,.T.);
#7465=EDGE_CURVE('',#5877,#5877,#307,.T.);
#7466=EDGE_CURVE('',#5878,#5878,#308,.T.);
#7467=EDGE_CURVE('',#5878,#5879,#4078,.T.);
#7468=EDGE_CURVE('',#5879,#5879,#309,.T.);
#7469=EDGE_CURVE('',#5880,#5880,#310,.T.);
#7470=EDGE_CURVE('',#5880,#5881,#4079,.T.);
#7471=EDGE_CURVE('',#5881,#5881,#311,.T.);
#7472=EDGE_CURVE('',#5882,#5883,#4080,.T.);
#7473=EDGE_CURVE('',#5883,#5884,#752,.T.);
#7474=EDGE_CURVE('',#5884,#5885,#312,.T.);
#7475=EDGE_CURVE('',#5885,#5886,#4081,.T.);
#7476=EDGE_CURVE('',#5886,#5886,#313,.F.);
#7477=EDGE_CURVE('',#5885,#5887,#314,.T.);
#7478=EDGE_CURVE('',#5887,#5882,#753,.T.);
#7479=EDGE_CURVE('',#5888,#5889,#4082,.T.);
#7480=EDGE_CURVE('',#5889,#5883,#754,.T.);
#7481=EDGE_CURVE('',#5882,#5888,#755,.T.);
#7482=EDGE_CURVE('',#5890,#5891,#4083,.T.);
#7483=EDGE_CURVE('',#5891,#5889,#756,.T.);
#7484=EDGE_CURVE('',#5888,#5890,#757,.T.);
#7485=EDGE_CURVE('',#5892,#5893,#4084,.T.);
#7486=EDGE_CURVE('',#5893,#5891,#758,.T.);
#7487=EDGE_CURVE('',#5890,#5892,#759,.T.);
#7488=EDGE_CURVE('',#5894,#5895,#4085,.T.);
#7489=EDGE_CURVE('',#5895,#5893,#760,.T.);
#7490=EDGE_CURVE('',#5892,#5894,#761,.T.);
#7491=EDGE_CURVE('',#5896,#5897,#4086,.T.);
#7492=EDGE_CURVE('',#5897,#5895,#762,.T.);
#7493=EDGE_CURVE('',#5894,#5896,#763,.T.);
#7494=EDGE_CURVE('',#5898,#5899,#4087,.T.);
#7495=EDGE_CURVE('',#5899,#5897,#764,.T.);
#7496=EDGE_CURVE('',#5896,#5898,#765,.T.);
#7497=EDGE_CURVE('',#5900,#5901,#4088,.T.);
#7498=EDGE_CURVE('',#5901,#5899,#766,.T.);
#7499=EDGE_CURVE('',#5898,#5900,#767,.T.);
#7500=EDGE_CURVE('',#5902,#5903,#4089,.T.);
#7501=EDGE_CURVE('',#5903,#5901,#768,.T.);
#7502=EDGE_CURVE('',#5900,#5902,#769,.T.);
#7503=EDGE_CURVE('',#5904,#5905,#4090,.T.);
#7504=EDGE_CURVE('',#5905,#5903,#770,.T.);
#7505=EDGE_CURVE('',#5902,#5904,#771,.T.);
#7506=EDGE_CURVE('',#5906,#5907,#4091,.T.);
#7507=EDGE_CURVE('',#5907,#5905,#772,.T.);
#7508=EDGE_CURVE('',#5904,#5906,#773,.T.);
#7509=EDGE_CURVE('',#5908,#5909,#4092,.T.);
#7510=EDGE_CURVE('',#5909,#5907,#774,.T.);
#7511=EDGE_CURVE('',#5906,#5908,#775,.T.);
#7512=EDGE_CURVE('',#5910,#5911,#4093,.T.);
#7513=EDGE_CURVE('',#5911,#5909,#776,.T.);
#7514=EDGE_CURVE('',#5908,#5910,#777,.T.);
#7515=EDGE_CURVE('',#5912,#5913,#4094,.T.);
#7516=EDGE_CURVE('',#5913,#5911,#778,.T.);
#7517=EDGE_CURVE('',#5910,#5912,#779,.T.);
#7518=EDGE_CURVE('',#5914,#5915,#4095,.T.);
#7519=EDGE_CURVE('',#5915,#5913,#780,.T.);
#7520=EDGE_CURVE('',#5912,#5914,#781,.T.);
#7521=EDGE_CURVE('',#5916,#5917,#4096,.T.);
#7522=EDGE_CURVE('',#5917,#5915,#782,.T.);
#7523=EDGE_CURVE('',#5914,#5916,#783,.T.);
#7524=EDGE_CURVE('',#5918,#5919,#4097,.T.);
#7525=EDGE_CURVE('',#5919,#5917,#784,.T.);
#7526=EDGE_CURVE('',#5916,#5918,#785,.T.);
#7527=EDGE_CURVE('',#5920,#5921,#4098,.T.);
#7528=EDGE_CURVE('',#5921,#5919,#786,.T.);
#7529=EDGE_CURVE('',#5918,#5920,#787,.T.);
#7530=EDGE_CURVE('',#5922,#5923,#4099,.T.);
#7531=EDGE_CURVE('',#5923,#5921,#788,.T.);
#7532=EDGE_CURVE('',#5920,#5922,#789,.T.);
#7533=EDGE_CURVE('',#5924,#5925,#4100,.T.);
#7534=EDGE_CURVE('',#5925,#5923,#790,.T.);
#7535=EDGE_CURVE('',#5922,#5924,#791,.T.);
#7536=EDGE_CURVE('',#5926,#5927,#4101,.T.);
#7537=EDGE_CURVE('',#5927,#5925,#792,.T.);
#7538=EDGE_CURVE('',#5924,#5926,#793,.T.);
#7539=EDGE_CURVE('',#5928,#5929,#4102,.T.);
#7540=EDGE_CURVE('',#5929,#5927,#794,.T.);
#7541=EDGE_CURVE('',#5926,#5928,#795,.T.);
#7542=EDGE_CURVE('',#5930,#5931,#4103,.T.);
#7543=EDGE_CURVE('',#5931,#5929,#796,.T.);
#7544=EDGE_CURVE('',#5928,#5930,#797,.T.);
#7545=EDGE_CURVE('',#5932,#5933,#4104,.T.);
#7546=EDGE_CURVE('',#5933,#5931,#798,.T.);
#7547=EDGE_CURVE('',#5930,#5932,#799,.T.);
#7548=EDGE_CURVE('',#5934,#5935,#4105,.T.);
#7549=EDGE_CURVE('',#5934,#5936,#800,.T.);
#7550=EDGE_CURVE('',#5937,#5936,#315,.T.);
#7551=EDGE_CURVE('',#5937,#5935,#801,.T.);
#7552=EDGE_CURVE('',#5938,#5939,#4106,.T.);
#7553=EDGE_CURVE('',#5939,#5940,#802,.T.);
#7554=EDGE_CURVE('',#5941,#5940,#316,.T.);
#7555=EDGE_CURVE('',#5938,#5941,#803,.T.);
#7556=EDGE_CURVE('',#5942,#5943,#4107,.T.);
#7557=EDGE_CURVE('',#5943,#5939,#804,.T.);
#7558=EDGE_CURVE('',#5942,#5938,#805,.T.);
#7559=EDGE_CURVE('',#5944,#5945,#4108,.T.);
#7560=EDGE_CURVE('',#5945,#5943,#806,.T.);
#7561=EDGE_CURVE('',#5944,#5942,#807,.T.);
#7562=EDGE_CURVE('',#5946,#5947,#4109,.T.);
#7563=EDGE_CURVE('',#5947,#5945,#808,.T.);
#7564=EDGE_CURVE('',#5946,#5944,#809,.T.);
#7565=EDGE_CURVE('',#5948,#5949,#4110,.T.);
#7566=EDGE_CURVE('',#5949,#5947,#810,.T.);
#7567=EDGE_CURVE('',#5948,#5946,#811,.T.);
#7568=EDGE_CURVE('',#5950,#5951,#4111,.T.);
#7569=EDGE_CURVE('',#5951,#5949,#812,.T.);
#7570=EDGE_CURVE('',#5950,#5948,#813,.T.);
#7571=EDGE_CURVE('',#5952,#5953,#4112,.T.);
#7572=EDGE_CURVE('',#5953,#5951,#814,.T.);
#7573=EDGE_CURVE('',#5952,#5950,#815,.T.);
#7574=EDGE_CURVE('',#5954,#5955,#4113,.T.);
#7575=EDGE_CURVE('',#5955,#5953,#816,.T.);
#7576=EDGE_CURVE('',#5954,#5952,#817,.T.);
#7577=EDGE_CURVE('',#5956,#5957,#4114,.T.);
#7578=EDGE_CURVE('',#5957,#5955,#818,.T.);
#7579=EDGE_CURVE('',#5956,#5954,#819,.T.);
#7580=EDGE_CURVE('',#5958,#5959,#4115,.T.);
#7581=EDGE_CURVE('',#5959,#5957,#820,.T.);
#7582=EDGE_CURVE('',#5958,#5956,#821,.T.);
#7583=EDGE_CURVE('',#5960,#5961,#4116,.T.);
#7584=EDGE_CURVE('',#5961,#5959,#822,.T.);
#7585=EDGE_CURVE('',#5960,#5958,#823,.T.);
#7586=EDGE_CURVE('',#5962,#5963,#4117,.T.);
#7587=EDGE_CURVE('',#5963,#5961,#824,.T.);
#7588=EDGE_CURVE('',#5962,#5960,#825,.T.);
#7589=EDGE_CURVE('',#5964,#5965,#4118,.T.);
#7590=EDGE_CURVE('',#5965,#5963,#826,.T.);
#7591=EDGE_CURVE('',#5964,#5962,#827,.T.);
#7592=EDGE_CURVE('',#5966,#5967,#4119,.T.);
#7593=EDGE_CURVE('',#5967,#5965,#828,.T.);
#7594=EDGE_CURVE('',#5966,#5964,#829,.T.);
#7595=EDGE_CURVE('',#5968,#5969,#4120,.T.);
#7596=EDGE_CURVE('',#5969,#5967,#830,.T.);
#7597=EDGE_CURVE('',#5968,#5966,#831,.T.);
#7598=EDGE_CURVE('',#5970,#5971,#4121,.T.);
#7599=EDGE_CURVE('',#5971,#5969,#832,.T.);
#7600=EDGE_CURVE('',#5970,#5968,#833,.T.);
#7601=EDGE_CURVE('',#5972,#5973,#4122,.T.);
#7602=EDGE_CURVE('',#5973,#5971,#834,.T.);
#7603=EDGE_CURVE('',#5972,#5970,#835,.T.);
#7604=EDGE_CURVE('',#5974,#5975,#4123,.T.);
#7605=EDGE_CURVE('',#5975,#5973,#836,.T.);
#7606=EDGE_CURVE('',#5974,#5972,#837,.T.);
#7607=EDGE_CURVE('',#5976,#5977,#4124,.T.);
#7608=EDGE_CURVE('',#5977,#5975,#838,.T.);
#7609=EDGE_CURVE('',#5976,#5974,#839,.T.);
#7610=EDGE_CURVE('',#5978,#5979,#4125,.T.);
#7611=EDGE_CURVE('',#5979,#5977,#840,.T.);
#7612=EDGE_CURVE('',#5978,#5976,#841,.T.);
#7613=EDGE_CURVE('',#5980,#5981,#4126,.T.);
#7614=EDGE_CURVE('',#5981,#5979,#842,.T.);
#7615=EDGE_CURVE('',#5980,#5978,#843,.T.);
#7616=EDGE_CURVE('',#5982,#5983,#4127,.T.);
#7617=EDGE_CURVE('',#5983,#5981,#844,.T.);
#7618=EDGE_CURVE('',#5982,#5980,#845,.T.);
#7619=EDGE_CURVE('',#5984,#5985,#4128,.T.);
#7620=EDGE_CURVE('',#5985,#5983,#846,.T.);
#7621=EDGE_CURVE('',#5984,#5982,#847,.T.);
#7622=EDGE_CURVE('',#5986,#5987,#4129,.T.);
#7623=EDGE_CURVE('',#5987,#5985,#848,.T.);
#7624=EDGE_CURVE('',#5986,#5984,#849,.T.);
#7625=EDGE_CURVE('',#5988,#5989,#4130,.T.);
#7626=EDGE_CURVE('',#5990,#5988,#850,.T.);
#7627=EDGE_CURVE('',#5991,#5990,#317,.T.);
#7628=EDGE_CURVE('',#5991,#5989,#851,.T.);
#7629=EDGE_CURVE('',#5992,#5993,#4131,.T.);
#7630=EDGE_CURVE('',#5993,#5994,#852,.T.);
#7631=EDGE_CURVE('',#5994,#5995,#318,.T.);
#7632=EDGE_CURVE('',#5995,#5996,#4132,.T.);
#7633=EDGE_CURVE('',#5996,#5996,#319,.F.);
#7634=EDGE_CURVE('',#5995,#5997,#320,.T.);
#7635=EDGE_CURVE('',#5997,#5992,#853,.T.);
#7636=EDGE_CURVE('',#5998,#5999,#4133,.T.);
#7637=EDGE_CURVE('',#5999,#5993,#854,.T.);
#7638=EDGE_CURVE('',#5992,#5998,#855,.T.);
#7639=EDGE_CURVE('',#6000,#6001,#4134,.T.);
#7640=EDGE_CURVE('',#6001,#5999,#856,.T.);
#7641=EDGE_CURVE('',#5998,#6000,#857,.T.);
#7642=EDGE_CURVE('',#6002,#6003,#4135,.T.);
#7643=EDGE_CURVE('',#6003,#6001,#858,.T.);
#7644=EDGE_CURVE('',#6000,#6002,#859,.T.);
#7645=EDGE_CURVE('',#6004,#6005,#4136,.T.);
#7646=EDGE_CURVE('',#6005,#6003,#860,.T.);
#7647=EDGE_CURVE('',#6002,#6004,#861,.T.);
#7648=EDGE_CURVE('',#6006,#6007,#4137,.T.);
#7649=EDGE_CURVE('',#6007,#6005,#862,.T.);
#7650=EDGE_CURVE('',#6004,#6006,#863,.T.);
#7651=EDGE_CURVE('',#6008,#6009,#4138,.T.);
#7652=EDGE_CURVE('',#6009,#6007,#864,.T.);
#7653=EDGE_CURVE('',#6006,#6008,#865,.T.);
#7654=EDGE_CURVE('',#6010,#6011,#4139,.T.);
#7655=EDGE_CURVE('',#6011,#6009,#866,.T.);
#7656=EDGE_CURVE('',#6008,#6010,#867,.T.);
#7657=EDGE_CURVE('',#6012,#6013,#4140,.T.);
#7658=EDGE_CURVE('',#6013,#6011,#868,.T.);
#7659=EDGE_CURVE('',#6010,#6012,#869,.T.);
#7660=EDGE_CURVE('',#6014,#6015,#4141,.T.);
#7661=EDGE_CURVE('',#6015,#6013,#870,.T.);
#7662=EDGE_CURVE('',#6012,#6014,#871,.T.);
#7663=EDGE_CURVE('',#6016,#6017,#4142,.T.);
#7664=EDGE_CURVE('',#6017,#6015,#872,.T.);
#7665=EDGE_CURVE('',#6014,#6016,#873,.T.);
#7666=EDGE_CURVE('',#6018,#6019,#4143,.T.);
#7667=EDGE_CURVE('',#6019,#6017,#874,.T.);
#7668=EDGE_CURVE('',#6016,#6018,#875,.T.);
#7669=EDGE_CURVE('',#6020,#6021,#4144,.T.);
#7670=EDGE_CURVE('',#6021,#6019,#876,.T.);
#7671=EDGE_CURVE('',#6018,#6020,#877,.T.);
#7672=EDGE_CURVE('',#6022,#6023,#4145,.T.);
#7673=EDGE_CURVE('',#6023,#6021,#878,.T.);
#7674=EDGE_CURVE('',#6020,#6022,#879,.T.);
#7675=EDGE_CURVE('',#6024,#6025,#4146,.T.);
#7676=EDGE_CURVE('',#6025,#6023,#880,.T.);
#7677=EDGE_CURVE('',#6022,#6024,#881,.T.);
#7678=EDGE_CURVE('',#6026,#6027,#4147,.T.);
#7679=EDGE_CURVE('',#6027,#6025,#882,.T.);
#7680=EDGE_CURVE('',#6024,#6026,#883,.T.);
#7681=EDGE_CURVE('',#6028,#6029,#4148,.T.);
#7682=EDGE_CURVE('',#6029,#6027,#884,.T.);
#7683=EDGE_CURVE('',#6026,#6028,#885,.T.);
#7684=EDGE_CURVE('',#6030,#6031,#4149,.T.);
#7685=EDGE_CURVE('',#6031,#6029,#886,.T.);
#7686=EDGE_CURVE('',#6028,#6030,#887,.T.);
#7687=EDGE_CURVE('',#6032,#6033,#4150,.T.);
#7688=EDGE_CURVE('',#6033,#6031,#888,.T.);
#7689=EDGE_CURVE('',#6030,#6032,#889,.T.);
#7690=EDGE_CURVE('',#6034,#6035,#4151,.T.);
#7691=EDGE_CURVE('',#6035,#6033,#890,.T.);
#7692=EDGE_CURVE('',#6032,#6034,#891,.T.);
#7693=EDGE_CURVE('',#6036,#6037,#4152,.T.);
#7694=EDGE_CURVE('',#6037,#6035,#892,.T.);
#7695=EDGE_CURVE('',#6034,#6036,#893,.T.);
#7696=EDGE_CURVE('',#6038,#6039,#4153,.T.);
#7697=EDGE_CURVE('',#6039,#6037,#894,.T.);
#7698=EDGE_CURVE('',#6036,#6038,#895,.T.);
#7699=EDGE_CURVE('',#6040,#6041,#4154,.T.);
#7700=EDGE_CURVE('',#6041,#6039,#896,.T.);
#7701=EDGE_CURVE('',#6038,#6040,#897,.T.);
#7702=EDGE_CURVE('',#6042,#6043,#4155,.T.);
#7703=EDGE_CURVE('',#6043,#6041,#898,.T.);
#7704=EDGE_CURVE('',#6040,#6042,#899,.T.);
#7705=EDGE_CURVE('',#6044,#6045,#4156,.T.);
#7706=EDGE_CURVE('',#6045,#6043,#900,.T.);
#7707=EDGE_CURVE('',#6042,#6044,#901,.T.);
#7708=EDGE_CURVE('',#6046,#6047,#4157,.T.);
#7709=EDGE_CURVE('',#6047,#6045,#902,.T.);
#7710=EDGE_CURVE('',#6044,#6046,#903,.T.);
#7711=EDGE_CURVE('',#6048,#6049,#4158,.T.);
#7712=EDGE_CURVE('',#6049,#6047,#904,.T.);
#7713=EDGE_CURVE('',#6046,#6048,#905,.T.);
#7714=EDGE_CURVE('',#6050,#6051,#4159,.T.);
#7715=EDGE_CURVE('',#6051,#6049,#906,.T.);
#7716=EDGE_CURVE('',#6048,#6050,#907,.T.);
#7717=EDGE_CURVE('',#6052,#6053,#4160,.T.);
#7718=EDGE_CURVE('',#6053,#6051,#908,.T.);
#7719=EDGE_CURVE('',#6050,#6052,#909,.T.);
#7720=EDGE_CURVE('',#6054,#6055,#4161,.T.);
#7721=EDGE_CURVE('',#6055,#6053,#910,.T.);
#7722=EDGE_CURVE('',#6052,#6054,#911,.T.);
#7723=EDGE_CURVE('',#6056,#6057,#4162,.T.);
#7724=EDGE_CURVE('',#6057,#6055,#912,.T.);
#7725=EDGE_CURVE('',#6054,#6056,#913,.T.);
#7726=EDGE_CURVE('',#6058,#6059,#4163,.T.);
#7727=EDGE_CURVE('',#6059,#6057,#914,.T.);
#7728=EDGE_CURVE('',#6056,#6058,#915,.T.);
#7729=EDGE_CURVE('',#6060,#6061,#4164,.T.);
#7730=EDGE_CURVE('',#6061,#6059,#916,.T.);
#7731=EDGE_CURVE('',#6058,#6060,#917,.T.);
#7732=EDGE_CURVE('',#6062,#6063,#4165,.T.);
#7733=EDGE_CURVE('',#6063,#6061,#918,.T.);
#7734=EDGE_CURVE('',#6060,#6062,#919,.T.);
#7735=EDGE_CURVE('',#6064,#6065,#4166,.T.);
#7736=EDGE_CURVE('',#6065,#6063,#920,.T.);
#7737=EDGE_CURVE('',#6062,#6064,#921,.T.);
#7738=EDGE_CURVE('',#6066,#6067,#4167,.T.);
#7739=EDGE_CURVE('',#6067,#6065,#922,.T.);
#7740=EDGE_CURVE('',#6064,#6066,#923,.T.);
#7741=EDGE_CURVE('',#6068,#6069,#4168,.T.);
#7742=EDGE_CURVE('',#6069,#6067,#924,.T.);
#7743=EDGE_CURVE('',#6066,#6068,#925,.T.);
#7744=EDGE_CURVE('',#6070,#6071,#4169,.T.);
#7745=EDGE_CURVE('',#6071,#6069,#926,.T.);
#7746=EDGE_CURVE('',#6068,#6070,#927,.T.);
#7747=EDGE_CURVE('',#6072,#6073,#4170,.T.);
#7748=EDGE_CURVE('',#6073,#6071,#928,.T.);
#7749=EDGE_CURVE('',#6070,#6072,#929,.T.);
#7750=EDGE_CURVE('',#6074,#6075,#4171,.T.);
#7751=EDGE_CURVE('',#6074,#6076,#930,.T.);
#7752=EDGE_CURVE('',#6077,#6076,#321,.F.);
#7753=EDGE_CURVE('',#6077,#6075,#931,.T.);
#7754=EDGE_CURVE('',#6078,#6079,#4172,.T.);
#7755=EDGE_CURVE('',#6079,#6080,#932,.T.);
#7756=EDGE_CURVE('',#6081,#6080,#322,.T.);
#7757=EDGE_CURVE('',#6078,#6081,#933,.T.);
#7758=EDGE_CURVE('',#6082,#6083,#4173,.T.);
#7759=EDGE_CURVE('',#6083,#6079,#934,.T.);
#7760=EDGE_CURVE('',#6082,#6078,#935,.T.);
#7761=EDGE_CURVE('',#6084,#6085,#4174,.T.);
#7762=EDGE_CURVE('',#6085,#6083,#936,.T.);
#7763=EDGE_CURVE('',#6084,#6082,#937,.T.);
#7764=EDGE_CURVE('',#6086,#6087,#4175,.T.);
#7765=EDGE_CURVE('',#6087,#6085,#938,.T.);
#7766=EDGE_CURVE('',#6086,#6084,#939,.T.);
#7767=EDGE_CURVE('',#6088,#6089,#4176,.T.);
#7768=EDGE_CURVE('',#6089,#6087,#940,.T.);
#7769=EDGE_CURVE('',#6088,#6086,#941,.T.);
#7770=EDGE_CURVE('',#6090,#6091,#4177,.T.);
#7771=EDGE_CURVE('',#6091,#6089,#942,.T.);
#7772=EDGE_CURVE('',#6090,#6088,#943,.T.);
#7773=EDGE_CURVE('',#6092,#6093,#4178,.T.);
#7774=EDGE_CURVE('',#6093,#6091,#944,.T.);
#7775=EDGE_CURVE('',#6092,#6090,#945,.T.);
#7776=EDGE_CURVE('',#6094,#6095,#4179,.T.);
#7777=EDGE_CURVE('',#6095,#6093,#946,.T.);
#7778=EDGE_CURVE('',#6094,#6092,#947,.T.);
#7779=EDGE_CURVE('',#6096,#6097,#4180,.T.);
#7780=EDGE_CURVE('',#6097,#6095,#948,.T.);
#7781=EDGE_CURVE('',#6096,#6094,#949,.T.);
#7782=EDGE_CURVE('',#6098,#6099,#4181,.T.);
#7783=EDGE_CURVE('',#6099,#6097,#950,.T.);
#7784=EDGE_CURVE('',#6098,#6096,#951,.T.);
#7785=EDGE_CURVE('',#6100,#6101,#4182,.T.);
#7786=EDGE_CURVE('',#6101,#6099,#952,.T.);
#7787=EDGE_CURVE('',#6100,#6098,#953,.T.);
#7788=EDGE_CURVE('',#6102,#6103,#4183,.T.);
#7789=EDGE_CURVE('',#6103,#6101,#954,.T.);
#7790=EDGE_CURVE('',#6102,#6100,#955,.T.);
#7791=EDGE_CURVE('',#6104,#6105,#4184,.T.);
#7792=EDGE_CURVE('',#6105,#6103,#956,.T.);
#7793=EDGE_CURVE('',#6104,#6102,#957,.T.);
#7794=EDGE_CURVE('',#6106,#6107,#4185,.T.);
#7795=EDGE_CURVE('',#6107,#6105,#958,.T.);
#7796=EDGE_CURVE('',#6106,#6104,#959,.T.);
#7797=EDGE_CURVE('',#6108,#6109,#4186,.T.);
#7798=EDGE_CURVE('',#6109,#6107,#960,.T.);
#7799=EDGE_CURVE('',#6108,#6106,#961,.T.);
#7800=EDGE_CURVE('',#6110,#6111,#4187,.T.);
#7801=EDGE_CURVE('',#6111,#6109,#962,.T.);
#7802=EDGE_CURVE('',#6110,#6108,#963,.T.);
#7803=EDGE_CURVE('',#6112,#6113,#4188,.T.);
#7804=EDGE_CURVE('',#6113,#6111,#964,.T.);
#7805=EDGE_CURVE('',#6112,#6110,#965,.T.);
#7806=EDGE_CURVE('',#6114,#6115,#4189,.T.);
#7807=EDGE_CURVE('',#6115,#6113,#966,.T.);
#7808=EDGE_CURVE('',#6114,#6112,#967,.T.);
#7809=EDGE_CURVE('',#6116,#6117,#4190,.T.);
#7810=EDGE_CURVE('',#6117,#6115,#968,.T.);
#7811=EDGE_CURVE('',#6116,#6114,#969,.T.);
#7812=EDGE_CURVE('',#6118,#6119,#4191,.T.);
#7813=EDGE_CURVE('',#6119,#6117,#970,.T.);
#7814=EDGE_CURVE('',#6118,#6116,#971,.T.);
#7815=EDGE_CURVE('',#6120,#6121,#4192,.T.);
#7816=EDGE_CURVE('',#6121,#6119,#972,.T.);
#7817=EDGE_CURVE('',#6120,#6118,#973,.T.);
#7818=EDGE_CURVE('',#6122,#6123,#4193,.T.);
#7819=EDGE_CURVE('',#6123,#6121,#974,.T.);
#7820=EDGE_CURVE('',#6122,#6120,#975,.T.);
#7821=EDGE_CURVE('',#6124,#6125,#4194,.T.);
#7822=EDGE_CURVE('',#6125,#6123,#976,.T.);
#7823=EDGE_CURVE('',#6124,#6122,#977,.T.);
#7824=EDGE_CURVE('',#6126,#6127,#4195,.T.);
#7825=EDGE_CURVE('',#6127,#6125,#978,.T.);
#7826=EDGE_CURVE('',#6126,#6124,#979,.T.);
#7827=EDGE_CURVE('',#6128,#6129,#4196,.T.);
#7828=EDGE_CURVE('',#6129,#6127,#980,.T.);
#7829=EDGE_CURVE('',#6128,#6126,#981,.T.);
#7830=EDGE_CURVE('',#6130,#6131,#4197,.T.);
#7831=EDGE_CURVE('',#6131,#6129,#982,.T.);
#7832=EDGE_CURVE('',#6130,#6128,#983,.T.);
#7833=EDGE_CURVE('',#6132,#6133,#4198,.T.);
#7834=EDGE_CURVE('',#6133,#6131,#984,.T.);
#7835=EDGE_CURVE('',#6132,#6130,#985,.T.);
#7836=EDGE_CURVE('',#6134,#6135,#4199,.T.);
#7837=EDGE_CURVE('',#6135,#6133,#986,.T.);
#7838=EDGE_CURVE('',#6134,#6132,#987,.T.);
#7839=EDGE_CURVE('',#6136,#6137,#4200,.T.);
#7840=EDGE_CURVE('',#6137,#6135,#988,.T.);
#7841=EDGE_CURVE('',#6136,#6134,#989,.T.);
#7842=EDGE_CURVE('',#6138,#6139,#4201,.T.);
#7843=EDGE_CURVE('',#6139,#6137,#990,.T.);
#7844=EDGE_CURVE('',#6138,#6136,#991,.T.);
#7845=EDGE_CURVE('',#6140,#6141,#4202,.T.);
#7846=EDGE_CURVE('',#6141,#6139,#992,.T.);
#7847=EDGE_CURVE('',#6140,#6138,#993,.T.);
#7848=EDGE_CURVE('',#6142,#6143,#4203,.T.);
#7849=EDGE_CURVE('',#6143,#6141,#994,.T.);
#7850=EDGE_CURVE('',#6142,#6140,#995,.T.);
#7851=EDGE_CURVE('',#6144,#6145,#4204,.T.);
#7852=EDGE_CURVE('',#6145,#6143,#996,.T.);
#7853=EDGE_CURVE('',#6144,#6142,#997,.T.);
#7854=EDGE_CURVE('',#6146,#6147,#4205,.T.);
#7855=EDGE_CURVE('',#6147,#6145,#998,.T.);
#7856=EDGE_CURVE('',#6146,#6144,#999,.T.);
#7857=EDGE_CURVE('',#6148,#6149,#4206,.T.);
#7858=EDGE_CURVE('',#6149,#6147,#1000,.T.);
#7859=EDGE_CURVE('',#6148,#6146,#1001,.T.);
#7860=EDGE_CURVE('',#6150,#6151,#4207,.T.);
#7861=EDGE_CURVE('',#6151,#6149,#1002,.T.);
#7862=EDGE_CURVE('',#6150,#6148,#1003,.T.);
#7863=EDGE_CURVE('',#6152,#6153,#4208,.T.);
#7864=EDGE_CURVE('',#6153,#6151,#1004,.T.);
#7865=EDGE_CURVE('',#6152,#6150,#1005,.T.);
#7866=EDGE_CURVE('',#6154,#6155,#4209,.T.);
#7867=EDGE_CURVE('',#6155,#6153,#1006,.T.);
#7868=EDGE_CURVE('',#6154,#6152,#1007,.T.);
#7869=EDGE_CURVE('',#6156,#6157,#4210,.T.);
#7870=EDGE_CURVE('',#6157,#6155,#1008,.T.);
#7871=EDGE_CURVE('',#6156,#6154,#1009,.T.);
#7872=EDGE_CURVE('',#6158,#6159,#4211,.T.);
#7873=EDGE_CURVE('',#6160,#6158,#1010,.T.);
#7874=EDGE_CURVE('',#6161,#6160,#323,.T.);
#7875=EDGE_CURVE('',#6161,#6159,#1011,.T.);
#7876=EDGE_CURVE('',#5994,#6081,#1012,.T.);
#7877=EDGE_CURVE('',#6080,#5997,#1013,.T.);
#7878=EDGE_CURVE('',#6159,#6157,#1014,.T.);
#7879=EDGE_CURVE('',#6158,#6156,#1015,.T.);
#7880=EDGE_CURVE('',#6076,#6161,#1016,.T.);
#7881=EDGE_CURVE('',#6072,#6074,#1017,.T.);
#7882=EDGE_CURVE('',#6075,#6073,#1018,.T.);
#7883=EDGE_CURVE('',#6160,#6077,#1019,.T.);
#7884=EDGE_CURVE('',#6162,#6162,#324,.T.);
#7885=EDGE_CURVE('',#5884,#5941,#1020,.T.);
#7886=EDGE_CURVE('',#5940,#5887,#1021,.T.);
#7887=EDGE_CURVE('',#5989,#5987,#1022,.T.);
#7888=EDGE_CURVE('',#5988,#5986,#1023,.T.);
#7889=EDGE_CURVE('',#5936,#5991,#1024,.T.);
#7890=EDGE_CURVE('',#5932,#5934,#1025,.T.);
#7891=EDGE_CURVE('',#5935,#5933,#1026,.T.);
#7892=EDGE_CURVE('',#5990,#5937,#1027,.T.);
#7893=EDGE_CURVE('',#6163,#6163,#325,.T.);
#7894=EDGE_CURVE('',#6164,#6165,#326,.T.);
#7895=EDGE_CURVE('',#6165,#6166,#4212,.T.);
#7896=EDGE_CURVE('',#6166,#6167,#327,.T.);
#7897=EDGE_CURVE('',#6167,#6164,#4213,.T.);
#7898=EDGE_CURVE('',#6168,#6165,#4214,.T.);
#7899=EDGE_CURVE('',#6169,#6168,#4215,.T.);
#7900=EDGE_CURVE('',#6166,#6169,#4216,.T.);
#7901=EDGE_CURVE('',#6164,#6170,#4217,.T.);
#7902=EDGE_CURVE('',#6171,#6170,#328,.T.);
#7903=EDGE_CURVE('',#6171,#6172,#4218,.T.);
#7904=EDGE_CURVE('',#6173,#6172,#329,.T.);
#7905=EDGE_CURVE('',#6173,#6174,#4219,.T.);
#7906=EDGE_CURVE('',#6175,#6174,#330,.T.);
#7907=EDGE_CURVE('',#6175,#6176,#4220,.T.);
#7908=EDGE_CURVE('',#6177,#6176,#331,.T.);
#7909=EDGE_CURVE('',#6177,#6178,#4221,.T.);
#7910=EDGE_CURVE('',#6179,#6178,#332,.T.);
#7911=EDGE_CURVE('',#6179,#6180,#4222,.T.);
#7912=EDGE_CURVE('',#6181,#6180,#333,.T.);
#7913=EDGE_CURVE('',#6181,#6182,#4223,.T.);
#7914=EDGE_CURVE('',#6183,#6182,#334,.T.);
#7915=EDGE_CURVE('',#6183,#6184,#4224,.T.);
#7916=EDGE_CURVE('',#6185,#6184,#335,.T.);
#7917=EDGE_CURVE('',#6185,#6186,#4225,.T.);
#7918=EDGE_CURVE('',#6187,#6186,#336,.T.);
#7919=EDGE_CURVE('',#6187,#6188,#4226,.T.);
#7920=EDGE_CURVE('',#6189,#6188,#337,.T.);
#7921=EDGE_CURVE('',#6189,#6190,#4227,.T.);
#7922=EDGE_CURVE('',#6191,#6190,#338,.T.);
#7923=EDGE_CURVE('',#6191,#6192,#4228,.T.);
#7924=EDGE_CURVE('',#6193,#6192,#339,.T.);
#7925=EDGE_CURVE('',#6193,#6194,#4229,.T.);
#7926=EDGE_CURVE('',#6195,#6194,#340,.T.);
#7927=EDGE_CURVE('',#6195,#6196,#4230,.T.);
#7928=EDGE_CURVE('',#6197,#6196,#341,.T.);
#7929=EDGE_CURVE('',#6197,#6198,#4231,.T.);
#7930=EDGE_CURVE('',#6199,#6198,#342,.T.);
#7931=EDGE_CURVE('',#6199,#6200,#4232,.T.);
#7932=EDGE_CURVE('',#6201,#6200,#343,.T.);
#7933=EDGE_CURVE('',#6201,#6202,#4233,.T.);
#7934=EDGE_CURVE('',#6203,#6202,#344,.T.);
#7935=EDGE_CURVE('',#6203,#6204,#4234,.T.);
#7936=EDGE_CURVE('',#6205,#6204,#345,.T.);
#7937=EDGE_CURVE('',#6205,#6206,#4235,.T.);
#7938=EDGE_CURVE('',#6207,#6206,#346,.T.);
#7939=EDGE_CURVE('',#6207,#6208,#4236,.T.);
#7940=EDGE_CURVE('',#6209,#6208,#347,.T.);
#7941=EDGE_CURVE('',#6209,#6210,#4237,.T.);
#7942=EDGE_CURVE('',#6211,#6210,#348,.T.);
#7943=EDGE_CURVE('',#6211,#6212,#4238,.T.);
#7944=EDGE_CURVE('',#6213,#6212,#349,.T.);
#7945=EDGE_CURVE('',#6213,#6214,#4239,.T.);
#7946=EDGE_CURVE('',#6215,#6214,#350,.T.);
#7947=EDGE_CURVE('',#6215,#6216,#4240,.T.);
#7948=EDGE_CURVE('',#6217,#6216,#351,.T.);
#7949=EDGE_CURVE('',#6217,#6218,#4241,.T.);
#7950=EDGE_CURVE('',#6219,#6218,#352,.T.);
#7951=EDGE_CURVE('',#6219,#6220,#4242,.T.);
#7952=EDGE_CURVE('',#6221,#6220,#353,.T.);
#7953=EDGE_CURVE('',#6221,#6222,#4243,.T.);
#7954=EDGE_CURVE('',#6223,#6222,#354,.T.);
#7955=EDGE_CURVE('',#6223,#6224,#4244,.T.);
#7956=EDGE_CURVE('',#6225,#6224,#355,.T.);
#7957=EDGE_CURVE('',#6225,#6226,#4245,.T.);
#7958=EDGE_CURVE('',#6227,#6226,#356,.T.);
#7959=EDGE_CURVE('',#6227,#6228,#4246,.T.);
#7960=EDGE_CURVE('',#6229,#6228,#357,.T.);
#7961=EDGE_CURVE('',#6229,#6230,#4247,.T.);
#7962=EDGE_CURVE('',#6231,#6230,#358,.T.);
#7963=EDGE_CURVE('',#6231,#6232,#4248,.T.);
#7964=EDGE_CURVE('',#6233,#6232,#359,.T.);
#7965=EDGE_CURVE('',#6233,#6234,#4249,.T.);
#7966=EDGE_CURVE('',#6235,#6234,#360,.T.);
#7967=EDGE_CURVE('',#6235,#6236,#4250,.T.);
#7968=EDGE_CURVE('',#6237,#6236,#361,.T.);
#7969=EDGE_CURVE('',#6237,#6238,#4251,.T.);
#7970=EDGE_CURVE('',#6168,#6238,#362,.T.);
#7971=EDGE_CURVE('',#6239,#6239,#363,.T.);
#7972=EDGE_CURVE('',#6240,#6240,#364,.T.);
#7973=EDGE_CURVE('',#6241,#6241,#365,.T.);
#7974=EDGE_CURVE('',#6242,#6242,#366,.T.);
#7975=EDGE_CURVE('',#6243,#6244,#367,.T.);
#7976=EDGE_CURVE('',#6244,#6171,#4252,.T.);
#7977=EDGE_CURVE('',#6170,#6243,#4253,.T.);
#7978=EDGE_CURVE('',#6245,#6244,#4254,.T.);
#7979=EDGE_CURVE('',#6172,#6245,#4255,.T.);
#7980=EDGE_CURVE('',#6245,#6246,#368,.T.);
#7981=EDGE_CURVE('',#6246,#6173,#4256,.T.);
#7982=EDGE_CURVE('',#6247,#6246,#4257,.T.);
#7983=EDGE_CURVE('',#6174,#6247,#4258,.T.);
#7984=EDGE_CURVE('',#6247,#6248,#369,.T.);
#7985=EDGE_CURVE('',#6248,#6175,#4259,.T.);
#7986=EDGE_CURVE('',#6249,#6248,#4260,.T.);
#7987=EDGE_CURVE('',#6176,#6249,#4261,.T.);
#7988=EDGE_CURVE('',#6249,#6250,#370,.T.);
#7989=EDGE_CURVE('',#6250,#6177,#4262,.T.);
#7990=EDGE_CURVE('',#6251,#6250,#4263,.T.);
#7991=EDGE_CURVE('',#6178,#6251,#4264,.T.);
#7992=EDGE_CURVE('',#6251,#6252,#371,.T.);
#7993=EDGE_CURVE('',#6252,#6179,#4265,.T.);
#7994=EDGE_CURVE('',#6180,#6253,#4266,.T.);
#7995=EDGE_CURVE('',#6253,#6254,#372,.T.);
#7996=EDGE_CURVE('',#6254,#6181,#4267,.T.);
#7997=EDGE_CURVE('',#6255,#6254,#4268,.T.);
#7998=EDGE_CURVE('',#6182,#6255,#4269,.T.);
#7999=EDGE_CURVE('',#6255,#6256,#373,.T.);
#8000=EDGE_CURVE('',#6256,#6183,#4270,.T.);
#8001=EDGE_CURVE('',#6184,#6257,#4271,.T.);
#8002=EDGE_CURVE('',#6257,#6258,#374,.T.);
#8003=EDGE_CURVE('',#6258,#6185,#4272,.T.);
#8004=EDGE_CURVE('',#6259,#6258,#4273,.T.);
#8005=EDGE_CURVE('',#6186,#6259,#4274,.T.);
#8006=EDGE_CURVE('',#6259,#6260,#375,.T.);
#8007=EDGE_CURVE('',#6260,#6187,#4275,.T.);
#8008=EDGE_CURVE('',#6261,#6262,#376,.T.);
#8009=EDGE_CURVE('',#6262,#6189,#4276,.T.);
#8010=EDGE_CURVE('',#6188,#6261,#4277,.T.);
#8011=EDGE_CURVE('',#6263,#6262,#4278,.T.);
#8012=EDGE_CURVE('',#6190,#6263,#4279,.T.);
#8013=EDGE_CURVE('',#6263,#6264,#377,.T.);
#8014=EDGE_CURVE('',#6264,#6191,#4280,.T.);
#8015=EDGE_CURVE('',#6265,#6264,#4281,.T.);
#8016=EDGE_CURVE('',#6192,#6265,#4282,.T.);
#8017=EDGE_CURVE('',#6265,#6266,#378,.T.);
#8018=EDGE_CURVE('',#6266,#6193,#4283,.T.);
#8019=EDGE_CURVE('',#6267,#6266,#4284,.T.);
#8020=EDGE_CURVE('',#6194,#6267,#4285,.T.);
#8021=EDGE_CURVE('',#6267,#6268,#379,.T.);
#8022=EDGE_CURVE('',#6268,#6195,#4286,.T.);
#8023=EDGE_CURVE('',#6269,#6268,#4287,.T.);
#8024=EDGE_CURVE('',#6196,#6269,#4288,.T.);
#8025=EDGE_CURVE('',#6269,#6270,#380,.T.);
#8026=EDGE_CURVE('',#6270,#6197,#4289,.T.);
#8027=EDGE_CURVE('',#6198,#6271,#4290,.T.);
#8028=EDGE_CURVE('',#6271,#6272,#381,.T.);
#8029=EDGE_CURVE('',#6272,#6199,#4291,.T.);
#8030=EDGE_CURVE('',#6273,#6272,#4292,.T.);
#8031=EDGE_CURVE('',#6200,#6273,#4293,.T.);
#8032=EDGE_CURVE('',#6273,#6274,#382,.T.);
#8033=EDGE_CURVE('',#6274,#6201,#4294,.T.);
#8034=EDGE_CURVE('',#6202,#6275,#4295,.T.);
#8035=EDGE_CURVE('',#6275,#6276,#383,.T.);
#8036=EDGE_CURVE('',#6276,#6203,#4296,.T.);
#8037=EDGE_CURVE('',#6277,#6276,#4297,.T.);
#8038=EDGE_CURVE('',#6204,#6277,#4298,.T.);
#8039=EDGE_CURVE('',#6277,#6278,#384,.T.);
#8040=EDGE_CURVE('',#6278,#6205,#4299,.T.);
#8041=EDGE_CURVE('',#6279,#6280,#385,.T.);
#8042=EDGE_CURVE('',#6280,#6207,#4300,.T.);
#8043=EDGE_CURVE('',#6206,#6279,#4301,.T.);
#8044=EDGE_CURVE('',#6281,#6280,#4302,.T.);
#8045=EDGE_CURVE('',#6208,#6281,#4303,.T.);
#8046=EDGE_CURVE('',#6281,#6282,#386,.T.);
#8047=EDGE_CURVE('',#6282,#6209,#4304,.T.);
#8048=EDGE_CURVE('',#6283,#6282,#4305,.T.);
#8049=EDGE_CURVE('',#6210,#6283,#4306,.T.);
#8050=EDGE_CURVE('',#6283,#6284,#387,.T.);
#8051=EDGE_CURVE('',#6284,#6211,#4307,.T.);
#8052=EDGE_CURVE('',#6285,#6284,#4308,.T.);
#8053=EDGE_CURVE('',#6212,#6285,#4309,.T.);
#8054=EDGE_CURVE('',#6285,#6286,#388,.T.);
#8055=EDGE_CURVE('',#6286,#6213,#4310,.T.);
#8056=EDGE_CURVE('',#6287,#6286,#4311,.T.);
#8057=EDGE_CURVE('',#6214,#6287,#4312,.T.);
#8058=EDGE_CURVE('',#6287,#6288,#389,.T.);
#8059=EDGE_CURVE('',#6288,#6215,#4313,.T.);
#8060=EDGE_CURVE('',#6216,#6289,#4314,.T.);
#8061=EDGE_CURVE('',#6289,#6290,#390,.T.);
#8062=EDGE_CURVE('',#6290,#6217,#4315,.T.);
#8063=EDGE_CURVE('',#6291,#6290,#4316,.T.);
#8064=EDGE_CURVE('',#6218,#6291,#4317,.T.);
#8065=EDGE_CURVE('',#6291,#6292,#391,.T.);
#8066=EDGE_CURVE('',#6292,#6219,#4318,.T.);
#8067=EDGE_CURVE('',#6220,#6293,#4319,.T.);
#8068=EDGE_CURVE('',#6293,#6294,#392,.T.);
#8069=EDGE_CURVE('',#6294,#6221,#4320,.T.);
#8070=EDGE_CURVE('',#6295,#6294,#4321,.T.);
#8071=EDGE_CURVE('',#6222,#6295,#4322,.T.);
#8072=EDGE_CURVE('',#6295,#6296,#393,.T.);
#8073=EDGE_CURVE('',#6296,#6223,#4323,.T.);
#8074=EDGE_CURVE('',#6297,#6298,#394,.T.);
#8075=EDGE_CURVE('',#6298,#6225,#4324,.T.);
#8076=EDGE_CURVE('',#6224,#6297,#4325,.T.);
#8077=EDGE_CURVE('',#6299,#6298,#4326,.T.);
#8078=EDGE_CURVE('',#6226,#6299,#4327,.T.);
#8079=EDGE_CURVE('',#6299,#6300,#395,.T.);
#8080=EDGE_CURVE('',#6300,#6227,#4328,.T.);
#8081=EDGE_CURVE('',#6301,#6300,#4329,.T.);
#8082=EDGE_CURVE('',#6228,#6301,#4330,.T.);
#8083=EDGE_CURVE('',#6301,#6302,#396,.T.);
#8084=EDGE_CURVE('',#6302,#6229,#4331,.T.);
#8085=EDGE_CURVE('',#6303,#6302,#4332,.T.);
#8086=EDGE_CURVE('',#6230,#6303,#4333,.T.);
#8087=EDGE_CURVE('',#6303,#6304,#397,.T.);
#8088=EDGE_CURVE('',#6304,#6231,#4334,.T.);
#8089=EDGE_CURVE('',#6305,#6304,#4335,.T.);
#8090=EDGE_CURVE('',#6232,#6305,#4336,.T.);
#8091=EDGE_CURVE('',#6305,#6306,#398,.T.);
#8092=EDGE_CURVE('',#6306,#6233,#4337,.T.);
#8093=EDGE_CURVE('',#6234,#6307,#4338,.T.);
#8094=EDGE_CURVE('',#6307,#6308,#399,.T.);
#8095=EDGE_CURVE('',#6308,#6235,#4339,.T.);
#8096=EDGE_CURVE('',#6309,#6308,#4340,.T.);
#8097=EDGE_CURVE('',#6236,#6309,#4341,.T.);
#8098=EDGE_CURVE('',#6309,#6310,#400,.T.);
#8099=EDGE_CURVE('',#6310,#6237,#4342,.T.);
#8100=EDGE_CURVE('',#6238,#6311,#4343,.T.);
#8101=EDGE_CURVE('',#6311,#6169,#401,.T.);
#8102=EDGE_CURVE('',#6242,#6312,#4344,.T.);
#8103=EDGE_CURVE('',#6312,#6312,#402,.T.);
#8104=EDGE_CURVE('',#6241,#6313,#4345,.T.);
#8105=EDGE_CURVE('',#6313,#6313,#403,.T.);
#8106=EDGE_CURVE('',#6163,#6162,#4346,.T.);
#8107=EDGE_CURVE('',#6240,#6314,#4347,.T.);
#8108=EDGE_CURVE('',#6314,#6314,#404,.T.);
#8109=EDGE_CURVE('',#6239,#6315,#4348,.T.);
#8110=EDGE_CURVE('',#6315,#6315,#405,.T.);
#8111=EDGE_CURVE('',#6311,#6310,#4349,.T.);
#8112=EDGE_CURVE('',#6307,#6306,#4350,.T.);
#8113=EDGE_CURVE('',#6297,#6296,#4351,.T.);
#8114=EDGE_CURVE('',#6293,#6292,#4352,.T.);
#8115=EDGE_CURVE('',#6289,#6288,#4353,.T.);
#8116=EDGE_CURVE('',#6279,#6278,#4354,.T.);
#8117=EDGE_CURVE('',#6275,#6274,#4355,.T.);
#8118=EDGE_CURVE('',#6271,#6270,#4356,.T.);
#8119=EDGE_CURVE('',#6261,#6260,#4357,.T.);
#8120=EDGE_CURVE('',#6257,#6256,#4358,.T.);
#8121=EDGE_CURVE('',#6253,#6252,#4359,.T.);
#8122=EDGE_CURVE('',#6243,#6167,#4360,.T.);
#8123=EDGE_CURVE('',#6316,#6316,#406,.T.);
#8124=EDGE_CURVE('',#6317,#6317,#407,.T.);
#8125=EDGE_CURVE('',#6318,#6318,#408,.T.);
#8126=EDGE_CURVE('',#6318,#6316,#4361,.T.);
#8127=EDGE_CURVE('',#6317,#6319,#4362,.T.);
#8128=EDGE_CURVE('',#6319,#6319,#409,.T.);
#8129=EDGE_CURVE('',#6320,#6320,#410,.T.);
#8130=EDGE_CURVE('',#6320,#6321,#4363,.T.);
#8131=EDGE_CURVE('',#6321,#6321,#411,.T.);
#8132=EDGE_CURVE('',#6322,#6322,#412,.T.);
#8133=EDGE_CURVE('',#6322,#6323,#4364,.T.);
#8134=EDGE_CURVE('',#6323,#6323,#413,.T.);
#8135=EDGE_CURVE('',#6324,#6324,#414,.T.);
#8136=EDGE_CURVE('',#6324,#6325,#4365,.T.);
#8137=EDGE_CURVE('',#6325,#6325,#415,.T.);
#8138=EDGE_CURVE('',#6326,#6326,#416,.T.);
#8139=EDGE_CURVE('',#6326,#6327,#4366,.T.);
#8140=EDGE_CURVE('',#6327,#6327,#417,.T.);
#8141=EDGE_CURVE('',#6328,#6329,#4367,.T.);
#8142=EDGE_CURVE('',#6329,#6330,#4368,.T.);
#8143=EDGE_CURVE('',#6331,#6330,#4369,.T.);
#8144=EDGE_CURVE('',#6328,#6331,#4370,.T.);
#8145=EDGE_CURVE('',#6332,#6328,#4371,.T.);
#8146=EDGE_CURVE('',#6333,#6331,#4372,.T.);
#8147=EDGE_CURVE('',#6332,#6333,#4373,.T.);
#8148=EDGE_CURVE('',#6334,#6332,#4374,.T.);
#8149=EDGE_CURVE('',#6335,#6333,#4375,.T.);
#8150=EDGE_CURVE('',#6334,#6335,#4376,.T.);
#8151=EDGE_CURVE('',#6329,#6334,#4377,.T.);
#8152=EDGE_CURVE('',#6330,#6335,#4378,.T.);
#8153=EDGE_CURVE('',#6336,#6337,#4379,.T.);
#8154=EDGE_CURVE('',#6336,#6338,#1028,.T.);
#8155=EDGE_CURVE('',#6338,#6339,#418,.F.);
#8156=EDGE_CURVE('',#6339,#6337,#1029,.T.);
#8157=EDGE_CURVE('',#6340,#6341,#4380,.T.);
#8158=EDGE_CURVE('',#6340,#6336,#1030,.T.);
#8159=EDGE_CURVE('',#6337,#6341,#1031,.T.);
#8160=EDGE_CURVE('',#6342,#6343,#4381,.T.);
#8161=EDGE_CURVE('',#6342,#6340,#1032,.T.);
#8162=EDGE_CURVE('',#6341,#6343,#1033,.T.);
#8163=EDGE_CURVE('',#6344,#6345,#4382,.T.);
#8164=EDGE_CURVE('',#6344,#6342,#1034,.T.);
#8165=EDGE_CURVE('',#6343,#6345,#1035,.T.);
#8166=EDGE_CURVE('',#6346,#6347,#4383,.T.);
#8167=EDGE_CURVE('',#6346,#6344,#1036,.T.);
#8168=EDGE_CURVE('',#6345,#6347,#1037,.T.);
#8169=EDGE_CURVE('',#6348,#6349,#4384,.T.);
#8170=EDGE_CURVE('',#6348,#6346,#1038,.T.);
#8171=EDGE_CURVE('',#6347,#6349,#1039,.T.);
#8172=EDGE_CURVE('',#6350,#6351,#4385,.T.);
#8173=EDGE_CURVE('',#6350,#6348,#1040,.T.);
#8174=EDGE_CURVE('',#6349,#6351,#1041,.T.);
#8175=EDGE_CURVE('',#6352,#6353,#4386,.T.);
#8176=EDGE_CURVE('',#6352,#6350,#1042,.T.);
#8177=EDGE_CURVE('',#6351,#6353,#1043,.T.);
#8178=EDGE_CURVE('',#6354,#6355,#4387,.T.);
#8179=EDGE_CURVE('',#6354,#6352,#1044,.T.);
#8180=EDGE_CURVE('',#6353,#6355,#1045,.T.);
#8181=EDGE_CURVE('',#6356,#6357,#4388,.T.);
#8182=EDGE_CURVE('',#6356,#6354,#1046,.T.);
#8183=EDGE_CURVE('',#6355,#6357,#1047,.T.);
#8184=EDGE_CURVE('',#6358,#6359,#4389,.T.);
#8185=EDGE_CURVE('',#6358,#6356,#1048,.T.);
#8186=EDGE_CURVE('',#6357,#6359,#1049,.T.);
#8187=EDGE_CURVE('',#6360,#6361,#4390,.T.);
#8188=EDGE_CURVE('',#6360,#6358,#1050,.T.);
#8189=EDGE_CURVE('',#6359,#6361,#1051,.T.);
#8190=EDGE_CURVE('',#6362,#6363,#4391,.T.);
#8191=EDGE_CURVE('',#6362,#6360,#1052,.T.);
#8192=EDGE_CURVE('',#6361,#6363,#1053,.T.);
#8193=EDGE_CURVE('',#6364,#6365,#4392,.T.);
#8194=EDGE_CURVE('',#6364,#6362,#1054,.T.);
#8195=EDGE_CURVE('',#6363,#6365,#1055,.T.);
#8196=EDGE_CURVE('',#6366,#6367,#4393,.T.);
#8197=EDGE_CURVE('',#6366,#6364,#1056,.T.);
#8198=EDGE_CURVE('',#6365,#6367,#1057,.T.);
#8199=EDGE_CURVE('',#6368,#6369,#4394,.T.);
#8200=EDGE_CURVE('',#6368,#6366,#1058,.T.);
#8201=EDGE_CURVE('',#6367,#6369,#1059,.T.);
#8202=EDGE_CURVE('',#6370,#6371,#4395,.T.);
#8203=EDGE_CURVE('',#6370,#6368,#1060,.T.);
#8204=EDGE_CURVE('',#6369,#6371,#1061,.T.);
#8205=EDGE_CURVE('',#6372,#6373,#4396,.T.);
#8206=EDGE_CURVE('',#6372,#6370,#1062,.T.);
#8207=EDGE_CURVE('',#6371,#6373,#1063,.T.);
#8208=EDGE_CURVE('',#6374,#6375,#4397,.T.);
#8209=EDGE_CURVE('',#6374,#6372,#1064,.T.);
#8210=EDGE_CURVE('',#6373,#6375,#1065,.T.);
#8211=EDGE_CURVE('',#6376,#6377,#4398,.T.);
#8212=EDGE_CURVE('',#6376,#6378,#1066,.T.);
#8213=EDGE_CURVE('',#6378,#6379,#419,.T.);
#8214=EDGE_CURVE('',#6377,#6379,#1067,.T.);
#8215=EDGE_CURVE('',#6380,#6381,#4399,.T.);
#8216=EDGE_CURVE('',#6380,#6376,#1068,.T.);
#8217=EDGE_CURVE('',#6381,#6377,#1069,.T.);
#8218=EDGE_CURVE('',#6382,#6383,#4400,.T.);
#8219=EDGE_CURVE('',#6382,#6380,#1070,.T.);
#8220=EDGE_CURVE('',#6383,#6381,#1071,.T.);
#8221=EDGE_CURVE('',#6384,#6385,#4401,.T.);
#8222=EDGE_CURVE('',#6384,#6382,#1072,.T.);
#8223=EDGE_CURVE('',#6385,#6383,#1073,.T.);
#8224=EDGE_CURVE('',#6386,#6387,#4402,.T.);
#8225=EDGE_CURVE('',#6386,#6384,#1074,.T.);
#8226=EDGE_CURVE('',#6387,#6385,#1075,.T.);
#8227=EDGE_CURVE('',#6388,#6389,#4403,.T.);
#8228=EDGE_CURVE('',#6388,#6386,#1076,.T.);
#8229=EDGE_CURVE('',#6389,#6387,#1077,.T.);
#8230=EDGE_CURVE('',#6390,#6391,#4404,.T.);
#8231=EDGE_CURVE('',#6390,#6388,#1078,.T.);
#8232=EDGE_CURVE('',#6391,#6389,#1079,.T.);
#8233=EDGE_CURVE('',#6392,#6393,#4405,.T.);
#8234=EDGE_CURVE('',#6392,#6390,#1080,.T.);
#8235=EDGE_CURVE('',#6393,#6391,#1081,.T.);
#8236=EDGE_CURVE('',#6394,#6395,#4406,.T.);
#8237=EDGE_CURVE('',#6394,#6392,#1082,.T.);
#8238=EDGE_CURVE('',#6395,#6393,#1083,.T.);
#8239=EDGE_CURVE('',#6396,#6397,#4407,.T.);
#8240=EDGE_CURVE('',#6396,#6394,#1084,.T.);
#8241=EDGE_CURVE('',#6397,#6395,#1085,.T.);
#8242=EDGE_CURVE('',#6398,#6399,#4408,.T.);
#8243=EDGE_CURVE('',#6398,#6396,#1086,.T.);
#8244=EDGE_CURVE('',#6399,#6397,#1087,.T.);
#8245=EDGE_CURVE('',#6400,#6401,#4409,.T.);
#8246=EDGE_CURVE('',#6400,#6398,#1088,.T.);
#8247=EDGE_CURVE('',#6401,#6399,#1089,.T.);
#8248=EDGE_CURVE('',#6402,#6403,#4410,.T.);
#8249=EDGE_CURVE('',#6402,#6400,#1090,.T.);
#8250=EDGE_CURVE('',#6403,#6401,#1091,.T.);
#8251=EDGE_CURVE('',#6404,#6405,#4411,.T.);
#8252=EDGE_CURVE('',#6404,#6402,#1092,.T.);
#8253=EDGE_CURVE('',#6405,#6403,#1093,.T.);
#8254=EDGE_CURVE('',#6406,#6407,#4412,.T.);
#8255=EDGE_CURVE('',#6406,#6404,#1094,.T.);
#8256=EDGE_CURVE('',#6407,#6405,#1095,.T.);
#8257=EDGE_CURVE('',#6408,#6409,#4413,.T.);
#8258=EDGE_CURVE('',#6408,#6406,#1096,.T.);
#8259=EDGE_CURVE('',#6409,#6407,#1097,.T.);
#8260=EDGE_CURVE('',#6410,#6411,#4414,.T.);
#8261=EDGE_CURVE('',#6410,#6408,#1098,.T.);
#8262=EDGE_CURVE('',#6411,#6409,#1099,.T.);
#8263=EDGE_CURVE('',#6412,#6413,#4415,.T.);
#8264=EDGE_CURVE('',#6412,#6410,#1100,.T.);
#8265=EDGE_CURVE('',#6413,#6411,#1101,.T.);
#8266=EDGE_CURVE('',#6414,#6415,#4416,.T.);
#8267=EDGE_CURVE('',#6414,#6412,#1102,.T.);
#8268=EDGE_CURVE('',#6415,#6413,#1103,.T.);
#8269=EDGE_CURVE('',#6379,#6416,#1104,.T.);
#8270=EDGE_CURVE('',#6417,#6378,#1105,.T.);
#8271=EDGE_CURVE('',#6418,#6417,#420,.T.);
#8272=EDGE_CURVE('',#6416,#6418,#1106,.T.);
#8273=EDGE_CURVE('',#6416,#6419,#4417,.T.);
#8274=EDGE_CURVE('',#6419,#6419,#421,.T.);
#8275=EDGE_CURVE('',#6420,#6414,#1107,.T.);
#8276=EDGE_CURVE('',#6338,#6420,#1108,.T.);
#8277=EDGE_CURVE('',#6417,#6374,#1109,.T.);
#8278=EDGE_CURVE('',#6421,#6415,#1110,.T.);
#8279=EDGE_CURVE('',#6420,#6421,#422,.T.);
#8280=EDGE_CURVE('',#6375,#6418,#1111,.T.);
#8281=EDGE_CURVE('',#6421,#6339,#1112,.T.);
#8282=EDGE_CURVE('',#6422,#6423,#4418,.T.);
#8283=EDGE_CURVE('',#6422,#6424,#4419,.T.);
#8284=EDGE_CURVE('',#6424,#6425,#4420,.T.);
#8285=EDGE_CURVE('',#6423,#6425,#4421,.T.);
#8286=EDGE_CURVE('',#6426,#6422,#4422,.T.);
#8287=EDGE_CURVE('',#6426,#6427,#4423,.T.);
#8288=EDGE_CURVE('',#6427,#6424,#4424,.T.);
#8289=EDGE_CURVE('',#6428,#6426,#4425,.T.);
#8290=EDGE_CURVE('',#6428,#6429,#4426,.T.);
#8291=EDGE_CURVE('',#6429,#6427,#4427,.T.);
#8292=EDGE_CURVE('',#6430,#6428,#4428,.T.);
#8293=EDGE_CURVE('',#6430,#6431,#4429,.T.);
#8294=EDGE_CURVE('',#6431,#6429,#4430,.T.);
#8295=EDGE_CURVE('',#6432,#6430,#4431,.T.);
#8296=EDGE_CURVE('',#6432,#6433,#4432,.T.);
#8297=EDGE_CURVE('',#6433,#6431,#4433,.T.);
#8298=EDGE_CURVE('',#6423,#6432,#4434,.T.);
#8299=EDGE_CURVE('',#6425,#6433,#4435,.T.);
#8300=EDGE_CURVE('',#6434,#6434,#423,.T.);
#8301=EDGE_CURVE('',#6434,#6435,#4436,.T.);
#8302=EDGE_CURVE('',#6435,#6435,#424,.T.);
#8303=EDGE_CURVE('',#6436,#6436,#425,.T.);
#8304=EDGE_CURVE('',#6436,#6437,#4437,.T.);
#8305=EDGE_CURVE('',#6437,#6437,#426,.T.);
#8306=EDGE_CURVE('',#6438,#6439,#4438,.T.);
#8307=EDGE_CURVE('',#6439,#6440,#1113,.T.);
#8308=EDGE_CURVE('',#6440,#6441,#427,.T.);
#8309=EDGE_CURVE('',#6441,#6442,#4439,.T.);
#8310=EDGE_CURVE('',#6442,#6442,#428,.F.);
#8311=EDGE_CURVE('',#6441,#6443,#429,.T.);
#8312=EDGE_CURVE('',#6443,#6438,#1114,.T.);
#8313=EDGE_CURVE('',#6444,#6445,#4440,.T.);
#8314=EDGE_CURVE('',#6445,#6439,#1115,.T.);
#8315=EDGE_CURVE('',#6438,#6444,#1116,.T.);
#8316=EDGE_CURVE('',#6446,#6447,#4441,.T.);
#8317=EDGE_CURVE('',#6447,#6445,#1117,.T.);
#8318=EDGE_CURVE('',#6444,#6446,#1118,.T.);
#8319=EDGE_CURVE('',#6448,#6449,#4442,.T.);
#8320=EDGE_CURVE('',#6449,#6447,#1119,.T.);
#8321=EDGE_CURVE('',#6446,#6448,#1120,.T.);
#8322=EDGE_CURVE('',#6450,#6451,#4443,.T.);
#8323=EDGE_CURVE('',#6451,#6449,#1121,.T.);
#8324=EDGE_CURVE('',#6448,#6450,#1122,.T.);
#8325=EDGE_CURVE('',#6452,#6453,#4444,.T.);
#8326=EDGE_CURVE('',#6453,#6451,#1123,.T.);
#8327=EDGE_CURVE('',#6450,#6452,#1124,.T.);
#8328=EDGE_CURVE('',#6454,#6455,#4445,.T.);
#8329=EDGE_CURVE('',#6455,#6453,#1125,.T.);
#8330=EDGE_CURVE('',#6452,#6454,#1126,.T.);
#8331=EDGE_CURVE('',#6456,#6457,#4446,.T.);
#8332=EDGE_CURVE('',#6456,#6458,#1127,.T.);
#8333=EDGE_CURVE('',#6459,#6458,#430,.T.);
#8334=EDGE_CURVE('',#6459,#6457,#1128,.T.);
#8335=EDGE_CURVE('',#6460,#6461,#4447,.T.);
#8336=EDGE_CURVE('',#6461,#6462,#1129,.T.);
#8337=EDGE_CURVE('',#6463,#6462,#431,.T.);
#8338=EDGE_CURVE('',#6460,#6463,#1130,.T.);
#8339=EDGE_CURVE('',#6464,#6465,#4448,.T.);
#8340=EDGE_CURVE('',#6465,#6461,#1131,.T.);
#8341=EDGE_CURVE('',#6464,#6460,#1132,.T.);
#8342=EDGE_CURVE('',#6466,#6467,#4449,.T.);
#8343=EDGE_CURVE('',#6467,#6465,#1133,.T.);
#8344=EDGE_CURVE('',#6466,#6464,#1134,.T.);
#8345=EDGE_CURVE('',#6468,#6469,#4450,.T.);
#8346=EDGE_CURVE('',#6469,#6467,#1135,.T.);
#8347=EDGE_CURVE('',#6468,#6466,#1136,.T.);
#8348=EDGE_CURVE('',#6470,#6471,#4451,.T.);
#8349=EDGE_CURVE('',#6471,#6469,#1137,.T.);
#8350=EDGE_CURVE('',#6470,#6468,#1138,.T.);
#8351=EDGE_CURVE('',#6472,#6473,#4452,.T.);
#8352=EDGE_CURVE('',#6473,#6471,#1139,.T.);
#8353=EDGE_CURVE('',#6472,#6470,#1140,.T.);
#8354=EDGE_CURVE('',#6474,#6475,#4453,.T.);
#8355=EDGE_CURVE('',#6475,#6473,#1141,.T.);
#8356=EDGE_CURVE('',#6474,#6472,#1142,.T.);
#8357=EDGE_CURVE('',#6476,#6477,#4454,.T.);
#8358=EDGE_CURVE('',#6478,#6476,#1143,.T.);
#8359=EDGE_CURVE('',#6479,#6478,#432,.T.);
#8360=EDGE_CURVE('',#6479,#6477,#1144,.T.);
#8361=EDGE_CURVE('',#6480,#6481,#4455,.T.);
#8362=EDGE_CURVE('',#6481,#6482,#1145,.T.);
#8363=EDGE_CURVE('',#6482,#6483,#433,.T.);
#8364=EDGE_CURVE('',#6483,#6484,#4456,.T.);
#8365=EDGE_CURVE('',#6484,#6484,#434,.F.);
#8366=EDGE_CURVE('',#6483,#6485,#435,.T.);
#8367=EDGE_CURVE('',#6485,#6480,#1146,.T.);
#8368=EDGE_CURVE('',#6486,#6487,#4457,.T.);
#8369=EDGE_CURVE('',#6487,#6481,#1147,.T.);
#8370=EDGE_CURVE('',#6480,#6486,#1148,.T.);
#8371=EDGE_CURVE('',#6488,#6489,#4458,.T.);
#8372=EDGE_CURVE('',#6489,#6487,#1149,.T.);
#8373=EDGE_CURVE('',#6486,#6488,#1150,.T.);
#8374=EDGE_CURVE('',#6490,#6491,#4459,.T.);
#8375=EDGE_CURVE('',#6491,#6489,#1151,.T.);
#8376=EDGE_CURVE('',#6488,#6490,#1152,.T.);
#8377=EDGE_CURVE('',#6492,#6493,#4460,.T.);
#8378=EDGE_CURVE('',#6493,#6491,#1153,.T.);
#8379=EDGE_CURVE('',#6490,#6492,#1154,.T.);
#8380=EDGE_CURVE('',#6494,#6495,#4461,.T.);
#8381=EDGE_CURVE('',#6495,#6493,#1155,.T.);
#8382=EDGE_CURVE('',#6492,#6494,#1156,.T.);
#8383=EDGE_CURVE('',#6496,#6497,#4462,.T.);
#8384=EDGE_CURVE('',#6497,#6495,#1157,.T.);
#8385=EDGE_CURVE('',#6494,#6496,#1158,.T.);
#8386=EDGE_CURVE('',#6498,#6499,#4463,.T.);
#8387=EDGE_CURVE('',#6498,#6500,#1159,.T.);
#8388=EDGE_CURVE('',#6501,#6500,#436,.T.);
#8389=EDGE_CURVE('',#6501,#6499,#1160,.T.);
#8390=EDGE_CURVE('',#6502,#6503,#4464,.T.);
#8391=EDGE_CURVE('',#6503,#6504,#1161,.T.);
#8392=EDGE_CURVE('',#6505,#6504,#437,.T.);
#8393=EDGE_CURVE('',#6502,#6505,#1162,.T.);
#8394=EDGE_CURVE('',#6506,#6507,#4465,.T.);
#8395=EDGE_CURVE('',#6507,#6503,#1163,.T.);
#8396=EDGE_CURVE('',#6506,#6502,#1164,.T.);
#8397=EDGE_CURVE('',#6508,#6509,#4466,.T.);
#8398=EDGE_CURVE('',#6509,#6507,#1165,.T.);
#8399=EDGE_CURVE('',#6508,#6506,#1166,.T.);
#8400=EDGE_CURVE('',#6510,#6511,#4467,.T.);
#8401=EDGE_CURVE('',#6511,#6509,#1167,.T.);
#8402=EDGE_CURVE('',#6510,#6508,#1168,.T.);
#8403=EDGE_CURVE('',#6512,#6513,#4468,.T.);
#8404=EDGE_CURVE('',#6513,#6511,#1169,.T.);
#8405=EDGE_CURVE('',#6512,#6510,#1170,.T.);
#8406=EDGE_CURVE('',#6514,#6515,#4469,.T.);
#8407=EDGE_CURVE('',#6515,#6513,#1171,.T.);
#8408=EDGE_CURVE('',#6514,#6512,#1172,.T.);
#8409=EDGE_CURVE('',#6516,#6517,#4470,.T.);
#8410=EDGE_CURVE('',#6517,#6515,#1173,.T.);
#8411=EDGE_CURVE('',#6516,#6514,#1174,.T.);
#8412=EDGE_CURVE('',#6518,#6519,#4471,.T.);
#8413=EDGE_CURVE('',#6520,#6518,#1175,.T.);
#8414=EDGE_CURVE('',#6521,#6520,#438,.T.);
#8415=EDGE_CURVE('',#6521,#6519,#1176,.T.);
#8416=EDGE_CURVE('',#6522,#6523,#4472,.T.);
#8417=EDGE_CURVE('',#6523,#6524,#1177,.T.);
#8418=EDGE_CURVE('',#6524,#6525,#439,.T.);
#8419=EDGE_CURVE('',#6525,#6526,#4473,.T.);
#8420=EDGE_CURVE('',#6526,#6526,#440,.F.);
#8421=EDGE_CURVE('',#6525,#6527,#441,.T.);
#8422=EDGE_CURVE('',#6527,#6522,#1178,.T.);
#8423=EDGE_CURVE('',#6528,#6529,#4474,.T.);
#8424=EDGE_CURVE('',#6529,#6523,#1179,.T.);
#8425=EDGE_CURVE('',#6522,#6528,#1180,.T.);
#8426=EDGE_CURVE('',#6530,#6531,#4475,.T.);
#8427=EDGE_CURVE('',#6531,#6529,#1181,.T.);
#8428=EDGE_CURVE('',#6528,#6530,#1182,.T.);
#8429=EDGE_CURVE('',#6532,#6533,#4476,.T.);
#8430=EDGE_CURVE('',#6533,#6531,#1183,.T.);
#8431=EDGE_CURVE('',#6530,#6532,#1184,.T.);
#8432=EDGE_CURVE('',#6534,#6535,#4477,.T.);
#8433=EDGE_CURVE('',#6535,#6533,#1185,.T.);
#8434=EDGE_CURVE('',#6532,#6534,#1186,.T.);
#8435=EDGE_CURVE('',#6536,#6537,#4478,.T.);
#8436=EDGE_CURVE('',#6537,#6535,#1187,.T.);
#8437=EDGE_CURVE('',#6534,#6536,#1188,.T.);
#8438=EDGE_CURVE('',#6538,#6539,#4479,.T.);
#8439=EDGE_CURVE('',#6539,#6537,#1189,.T.);
#8440=EDGE_CURVE('',#6536,#6538,#1190,.T.);
#8441=EDGE_CURVE('',#6540,#6541,#4480,.T.);
#8442=EDGE_CURVE('',#6540,#6542,#1191,.T.);
#8443=EDGE_CURVE('',#6543,#6542,#442,.T.);
#8444=EDGE_CURVE('',#6543,#6541,#1192,.T.);
#8445=EDGE_CURVE('',#6544,#6545,#4481,.T.);
#8446=EDGE_CURVE('',#6545,#6546,#1193,.T.);
#8447=EDGE_CURVE('',#6547,#6546,#443,.T.);
#8448=EDGE_CURVE('',#6544,#6547,#1194,.T.);
#8449=EDGE_CURVE('',#6548,#6549,#4482,.T.);
#8450=EDGE_CURVE('',#6549,#6545,#1195,.T.);
#8451=EDGE_CURVE('',#6548,#6544,#1196,.T.);
#8452=EDGE_CURVE('',#6550,#6551,#4483,.T.);
#8453=EDGE_CURVE('',#6551,#6549,#1197,.T.);
#8454=EDGE_CURVE('',#6550,#6548,#1198,.T.);
#8455=EDGE_CURVE('',#6552,#6553,#4484,.T.);
#8456=EDGE_CURVE('',#6553,#6551,#1199,.T.);
#8457=EDGE_CURVE('',#6552,#6550,#1200,.T.);
#8458=EDGE_CURVE('',#6554,#6555,#4485,.T.);
#8459=EDGE_CURVE('',#6555,#6553,#1201,.T.);
#8460=EDGE_CURVE('',#6554,#6552,#1202,.T.);
#8461=EDGE_CURVE('',#6556,#6557,#4486,.T.);
#8462=EDGE_CURVE('',#6557,#6555,#1203,.T.);
#8463=EDGE_CURVE('',#6556,#6554,#1204,.T.);
#8464=EDGE_CURVE('',#6558,#6559,#4487,.T.);
#8465=EDGE_CURVE('',#6559,#6557,#1205,.T.);
#8466=EDGE_CURVE('',#6558,#6556,#1206,.T.);
#8467=EDGE_CURVE('',#6560,#6561,#4488,.T.);
#8468=EDGE_CURVE('',#6562,#6560,#1207,.T.);
#8469=EDGE_CURVE('',#6563,#6562,#444,.T.);
#8470=EDGE_CURVE('',#6563,#6561,#1208,.T.);
#8471=EDGE_CURVE('',#6524,#6547,#1209,.T.);
#8472=EDGE_CURVE('',#6546,#6527,#1210,.T.);
#8473=EDGE_CURVE('',#6561,#6559,#1211,.T.);
#8474=EDGE_CURVE('',#6560,#6558,#1212,.T.);
#8475=EDGE_CURVE('',#6542,#6563,#1213,.T.);
#8476=EDGE_CURVE('',#6538,#6540,#1214,.T.);
#8477=EDGE_CURVE('',#6541,#6539,#1215,.T.);
#8478=EDGE_CURVE('',#6562,#6543,#1216,.T.);
#8479=EDGE_CURVE('',#6482,#6505,#1217,.T.);
#8480=EDGE_CURVE('',#6504,#6485,#1218,.T.);
#8481=EDGE_CURVE('',#6519,#6517,#1219,.T.);
#8482=EDGE_CURVE('',#6518,#6516,#1220,.T.);
#8483=EDGE_CURVE('',#6500,#6521,#1221,.T.);
#8484=EDGE_CURVE('',#6496,#6498,#1222,.T.);
#8485=EDGE_CURVE('',#6499,#6497,#1223,.T.);
#8486=EDGE_CURVE('',#6520,#6501,#1224,.T.);
#8487=EDGE_CURVE('',#6440,#6463,#1225,.T.);
#8488=EDGE_CURVE('',#6462,#6443,#1226,.T.);
#8489=EDGE_CURVE('',#6477,#6475,#1227,.T.);
#8490=EDGE_CURVE('',#6476,#6474,#1228,.T.);
#8491=EDGE_CURVE('',#6458,#6479,#1229,.T.);
#8492=EDGE_CURVE('',#6454,#6456,#1230,.T.);
#8493=EDGE_CURVE('',#6457,#6455,#1231,.T.);
#8494=EDGE_CURVE('',#6478,#6459,#1232,.T.);
#8495=EDGE_CURVE('',#6564,#6564,#445,.T.);
#8496=EDGE_CURVE('',#6565,#6564,#446,.T.);
#8497=EDGE_CURVE('',#6566,#6566,#447,.T.);
#8498=EDGE_CURVE('',#6566,#6567,#4489,.T.);
#8499=EDGE_CURVE('',#6567,#6567,#448,.T.);
#8500=EDGE_CURVE('',#6568,#6568,#449,.T.);
#8501=EDGE_CURVE('',#6568,#6569,#4490,.T.);
#8502=EDGE_CURVE('',#6569,#6569,#450,.T.);
#8503=EDGE_CURVE('',#6570,#6570,#451,.T.);
#8504=EDGE_CURVE('',#6570,#6571,#4491,.T.);
#8505=EDGE_CURVE('',#6571,#6571,#452,.T.);
#8506=EDGE_CURVE('',#6572,#6572,#453,.T.);
#8507=EDGE_CURVE('',#6572,#6573,#4492,.T.);
#8508=EDGE_CURVE('',#6573,#6573,#454,.T.);
#8509=EDGE_CURVE('',#6574,#6574,#455,.T.);
#8510=EDGE_CURVE('',#6574,#6575,#456,.T.);
#8511=EDGE_CURVE('',#6575,#6575,#457,.T.);
#8512=EDGE_CURVE('',#6576,#6576,#458,.T.);
#8513=EDGE_CURVE('',#6576,#6575,#4493,.T.);
#8514=EDGE_CURVE('',#6577,#6577,#459,.T.);
#8515=EDGE_CURVE('',#6577,#6578,#4494,.T.);
#8516=EDGE_CURVE('',#6578,#6578,#460,.T.);
#8517=EDGE_CURVE('',#6579,#6580,#4495,.T.);
#8518=EDGE_CURVE('',#6579,#6581,#1233,.T.);
#8519=EDGE_CURVE('',#6581,#6582,#461,.F.);
#8520=EDGE_CURVE('',#6582,#6580,#1234,.T.);
#8521=EDGE_CURVE('',#6583,#6584,#4496,.T.);
#8522=EDGE_CURVE('',#6583,#6579,#1235,.T.);
#8523=EDGE_CURVE('',#6580,#6584,#1236,.T.);
#8524=EDGE_CURVE('',#6585,#6586,#4497,.T.);
#8525=EDGE_CURVE('',#6585,#6583,#1237,.T.);
#8526=EDGE_CURVE('',#6584,#6586,#1238,.T.);
#8527=EDGE_CURVE('',#6587,#6588,#4498,.T.);
#8528=EDGE_CURVE('',#6587,#6585,#1239,.T.);
#8529=EDGE_CURVE('',#6586,#6588,#1240,.T.);
#8530=EDGE_CURVE('',#6589,#6590,#4499,.T.);
#8531=EDGE_CURVE('',#6589,#6587,#1241,.T.);
#8532=EDGE_CURVE('',#6588,#6590,#1242,.T.);
#8533=EDGE_CURVE('',#6591,#6592,#4500,.T.);
#8534=EDGE_CURVE('',#6591,#6589,#1243,.T.);
#8535=EDGE_CURVE('',#6590,#6592,#1244,.T.);
#8536=EDGE_CURVE('',#6593,#6594,#4501,.T.);
#8537=EDGE_CURVE('',#6593,#6591,#1245,.T.);
#8538=EDGE_CURVE('',#6592,#6594,#1246,.T.);
#8539=EDGE_CURVE('',#6595,#6596,#4502,.T.);
#8540=EDGE_CURVE('',#6595,#6593,#1247,.T.);
#8541=EDGE_CURVE('',#6594,#6596,#1248,.T.);
#8542=EDGE_CURVE('',#6597,#6598,#4503,.T.);
#8543=EDGE_CURVE('',#6597,#6595,#1249,.T.);
#8544=EDGE_CURVE('',#6596,#6598,#1250,.T.);
#8545=EDGE_CURVE('',#6599,#6600,#4504,.T.);
#8546=EDGE_CURVE('',#6599,#6597,#1251,.T.);
#8547=EDGE_CURVE('',#6598,#6600,#1252,.T.);
#8548=EDGE_CURVE('',#6601,#6602,#4505,.T.);
#8549=EDGE_CURVE('',#6601,#6599,#1253,.T.);
#8550=EDGE_CURVE('',#6600,#6602,#1254,.T.);
#8551=EDGE_CURVE('',#6603,#6604,#4506,.T.);
#8552=EDGE_CURVE('',#6603,#6601,#1255,.T.);
#8553=EDGE_CURVE('',#6602,#6604,#1256,.T.);
#8554=EDGE_CURVE('',#6605,#6606,#4507,.T.);
#8555=EDGE_CURVE('',#6605,#6603,#1257,.T.);
#8556=EDGE_CURVE('',#6604,#6606,#1258,.T.);
#8557=EDGE_CURVE('',#6607,#6608,#4508,.T.);
#8558=EDGE_CURVE('',#6607,#6605,#1259,.T.);
#8559=EDGE_CURVE('',#6606,#6608,#1260,.T.);
#8560=EDGE_CURVE('',#6609,#6610,#4509,.T.);
#8561=EDGE_CURVE('',#6609,#6607,#1261,.T.);
#8562=EDGE_CURVE('',#6608,#6610,#1262,.T.);
#8563=EDGE_CURVE('',#6611,#6612,#4510,.T.);
#8564=EDGE_CURVE('',#6611,#6609,#1263,.T.);
#8565=EDGE_CURVE('',#6610,#6612,#1264,.T.);
#8566=EDGE_CURVE('',#6613,#6614,#4511,.T.);
#8567=EDGE_CURVE('',#6613,#6611,#1265,.T.);
#8568=EDGE_CURVE('',#6612,#6614,#1266,.T.);
#8569=EDGE_CURVE('',#6615,#6616,#4512,.T.);
#8570=EDGE_CURVE('',#6615,#6613,#1267,.T.);
#8571=EDGE_CURVE('',#6614,#6616,#1268,.T.);
#8572=EDGE_CURVE('',#6617,#6618,#4513,.T.);
#8573=EDGE_CURVE('',#6617,#6615,#1269,.T.);
#8574=EDGE_CURVE('',#6616,#6618,#1270,.T.);
#8575=EDGE_CURVE('',#6619,#6620,#4514,.T.);
#8576=EDGE_CURVE('',#6619,#6617,#1271,.T.);
#8577=EDGE_CURVE('',#6618,#6620,#1272,.T.);
#8578=EDGE_CURVE('',#6621,#6622,#4515,.T.);
#8579=EDGE_CURVE('',#6621,#6619,#1273,.T.);
#8580=EDGE_CURVE('',#6620,#6622,#1274,.T.);
#8581=EDGE_CURVE('',#6623,#6624,#4516,.T.);
#8582=EDGE_CURVE('',#6623,#6621,#1275,.T.);
#8583=EDGE_CURVE('',#6622,#6624,#1276,.T.);
#8584=EDGE_CURVE('',#6625,#6626,#4517,.T.);
#8585=EDGE_CURVE('',#6625,#6623,#1277,.T.);
#8586=EDGE_CURVE('',#6624,#6626,#1278,.T.);
#8587=EDGE_CURVE('',#6627,#6628,#4518,.T.);
#8588=EDGE_CURVE('',#6627,#6625,#1279,.T.);
#8589=EDGE_CURVE('',#6626,#6628,#1280,.T.);
#8590=EDGE_CURVE('',#6629,#6630,#4519,.T.);
#8591=EDGE_CURVE('',#6629,#6627,#1281,.T.);
#8592=EDGE_CURVE('',#6628,#6630,#1282,.T.);
#8593=EDGE_CURVE('',#6631,#6632,#4520,.T.);
#8594=EDGE_CURVE('',#6631,#6629,#1283,.T.);
#8595=EDGE_CURVE('',#6630,#6632,#1284,.T.);
#8596=EDGE_CURVE('',#6633,#6634,#4521,.T.);
#8597=EDGE_CURVE('',#6633,#6631,#1285,.T.);
#8598=EDGE_CURVE('',#6632,#6634,#1286,.T.);
#8599=EDGE_CURVE('',#6635,#6636,#4522,.T.);
#8600=EDGE_CURVE('',#6635,#6633,#1287,.T.);
#8601=EDGE_CURVE('',#6634,#6636,#1288,.T.);
#8602=EDGE_CURVE('',#6637,#6638,#4523,.T.);
#8603=EDGE_CURVE('',#6637,#6635,#1289,.T.);
#8604=EDGE_CURVE('',#6636,#6638,#1290,.T.);
#8605=EDGE_CURVE('',#6639,#6640,#4524,.T.);
#8606=EDGE_CURVE('',#6639,#6637,#1291,.T.);
#8607=EDGE_CURVE('',#6638,#6640,#1292,.T.);
#8608=EDGE_CURVE('',#6641,#6642,#4525,.T.);
#8609=EDGE_CURVE('',#6641,#6639,#1293,.T.);
#8610=EDGE_CURVE('',#6640,#6642,#1294,.T.);
#8611=EDGE_CURVE('',#6643,#6644,#4526,.T.);
#8612=EDGE_CURVE('',#6643,#6641,#1295,.T.);
#8613=EDGE_CURVE('',#6642,#6644,#1296,.T.);
#8614=EDGE_CURVE('',#6645,#6646,#4527,.T.);
#8615=EDGE_CURVE('',#6645,#6643,#1297,.T.);
#8616=EDGE_CURVE('',#6644,#6646,#1298,.T.);
#8617=EDGE_CURVE('',#6647,#6648,#4528,.T.);
#8618=EDGE_CURVE('',#6647,#6645,#1299,.T.);
#8619=EDGE_CURVE('',#6646,#6648,#1300,.T.);
#8620=EDGE_CURVE('',#6649,#6650,#4529,.T.);
#8621=EDGE_CURVE('',#6649,#6647,#1301,.T.);
#8622=EDGE_CURVE('',#6648,#6650,#1302,.T.);
#8623=EDGE_CURVE('',#6651,#6652,#4530,.T.);
#8624=EDGE_CURVE('',#6651,#6649,#1303,.T.);
#8625=EDGE_CURVE('',#6650,#6652,#1304,.T.);
#8626=EDGE_CURVE('',#6653,#6654,#4531,.T.);
#8627=EDGE_CURVE('',#6653,#6651,#1305,.T.);
#8628=EDGE_CURVE('',#6652,#6654,#1306,.T.);
#8629=EDGE_CURVE('',#6655,#6656,#4532,.T.);
#8630=EDGE_CURVE('',#6655,#6653,#1307,.T.);
#8631=EDGE_CURVE('',#6654,#6656,#1308,.T.);
#8632=EDGE_CURVE('',#6657,#6658,#4533,.T.);
#8633=EDGE_CURVE('',#6657,#6655,#1309,.T.);
#8634=EDGE_CURVE('',#6656,#6658,#1310,.T.);
#8635=EDGE_CURVE('',#6659,#6660,#4534,.T.);
#8636=EDGE_CURVE('',#6659,#6657,#1311,.T.);
#8637=EDGE_CURVE('',#6658,#6660,#1312,.T.);
#8638=EDGE_CURVE('',#6661,#6662,#4535,.T.);
#8639=EDGE_CURVE('',#6661,#6659,#1313,.T.);
#8640=EDGE_CURVE('',#6660,#6662,#1314,.T.);
#8641=EDGE_CURVE('',#6663,#6664,#4536,.T.);
#8642=EDGE_CURVE('',#6663,#6661,#1315,.T.);
#8643=EDGE_CURVE('',#6662,#6664,#1316,.T.);
#8644=EDGE_CURVE('',#6665,#6666,#4537,.T.);
#8645=EDGE_CURVE('',#6665,#6663,#1317,.T.);
#8646=EDGE_CURVE('',#6664,#6666,#1318,.T.);
#8647=EDGE_CURVE('',#6667,#6668,#4538,.T.);
#8648=EDGE_CURVE('',#6667,#6665,#1319,.T.);
#8649=EDGE_CURVE('',#6666,#6668,#1320,.T.);
#8650=EDGE_CURVE('',#6669,#6670,#4539,.T.);
#8651=EDGE_CURVE('',#6669,#6667,#1321,.T.);
#8652=EDGE_CURVE('',#6668,#6670,#1322,.T.);
#8653=EDGE_CURVE('',#6671,#6672,#4540,.T.);
#8654=EDGE_CURVE('',#6671,#6669,#1323,.T.);
#8655=EDGE_CURVE('',#6670,#6672,#1324,.T.);
#8656=EDGE_CURVE('',#6673,#6674,#4541,.T.);
#8657=EDGE_CURVE('',#6673,#6671,#1325,.T.);
#8658=EDGE_CURVE('',#6672,#6674,#1326,.T.);
#8659=EDGE_CURVE('',#6675,#6676,#4542,.T.);
#8660=EDGE_CURVE('',#6675,#6673,#1327,.T.);
#8661=EDGE_CURVE('',#6674,#6676,#1328,.T.);
#8662=EDGE_CURVE('',#6677,#6678,#4543,.T.);
#8663=EDGE_CURVE('',#6677,#6675,#1329,.T.);
#8664=EDGE_CURVE('',#6676,#6678,#1330,.T.);
#8665=EDGE_CURVE('',#6679,#6680,#4544,.T.);
#8666=EDGE_CURVE('',#6679,#6677,#1331,.T.);
#8667=EDGE_CURVE('',#6678,#6680,#1332,.T.);
#8668=EDGE_CURVE('',#6681,#6682,#4545,.T.);
#8669=EDGE_CURVE('',#6681,#6679,#1333,.T.);
#8670=EDGE_CURVE('',#6680,#6682,#1334,.T.);
#8671=EDGE_CURVE('',#6683,#6684,#4546,.T.);
#8672=EDGE_CURVE('',#6683,#6681,#1335,.T.);
#8673=EDGE_CURVE('',#6682,#6684,#1336,.T.);
#8674=EDGE_CURVE('',#6685,#6686,#4547,.T.);
#8675=EDGE_CURVE('',#6685,#6683,#1337,.T.);
#8676=EDGE_CURVE('',#6684,#6686,#1338,.T.);
#8677=EDGE_CURVE('',#6687,#6688,#4548,.T.);
#8678=EDGE_CURVE('',#6687,#6685,#1339,.T.);
#8679=EDGE_CURVE('',#6686,#6688,#1340,.T.);
#8680=EDGE_CURVE('',#6689,#6690,#4549,.T.);
#8681=EDGE_CURVE('',#6689,#6687,#1341,.T.);
#8682=EDGE_CURVE('',#6688,#6690,#1342,.T.);
#8683=EDGE_CURVE('',#6691,#6692,#4550,.T.);
#8684=EDGE_CURVE('',#6691,#6689,#1343,.T.);
#8685=EDGE_CURVE('',#6690,#6692,#1344,.T.);
#8686=EDGE_CURVE('',#6693,#6694,#4551,.T.);
#8687=EDGE_CURVE('',#6693,#6691,#1345,.T.);
#8688=EDGE_CURVE('',#6692,#6694,#1346,.T.);
#8689=EDGE_CURVE('',#6695,#6696,#4552,.T.);
#8690=EDGE_CURVE('',#6695,#6693,#1347,.T.);
#8691=EDGE_CURVE('',#6694,#6696,#1348,.T.);
#8692=EDGE_CURVE('',#6697,#6698,#4553,.T.);
#8693=EDGE_CURVE('',#6697,#6695,#1349,.T.);
#8694=EDGE_CURVE('',#6696,#6698,#1350,.T.);
#8695=EDGE_CURVE('',#6699,#6700,#4554,.T.);
#8696=EDGE_CURVE('',#6699,#6697,#1351,.T.);
#8697=EDGE_CURVE('',#6698,#6700,#1352,.T.);
#8698=EDGE_CURVE('',#6701,#6702,#4555,.T.);
#8699=EDGE_CURVE('',#6701,#6703,#1353,.T.);
#8700=EDGE_CURVE('',#6704,#6703,#462,.T.);
#8701=EDGE_CURVE('',#6702,#6704,#1354,.T.);
#8702=EDGE_CURVE('',#6705,#6706,#4556,.T.);
#8703=EDGE_CURVE('',#6705,#6701,#1355,.T.);
#8704=EDGE_CURVE('',#6706,#6702,#1356,.T.);
#8705=EDGE_CURVE('',#6707,#6708,#4557,.T.);
#8706=EDGE_CURVE('',#6707,#6705,#1357,.T.);
#8707=EDGE_CURVE('',#6708,#6706,#1358,.T.);
#8708=EDGE_CURVE('',#6709,#6710,#4558,.T.);
#8709=EDGE_CURVE('',#6709,#6707,#1359,.T.);
#8710=EDGE_CURVE('',#6710,#6708,#1360,.T.);
#8711=EDGE_CURVE('',#6711,#6712,#4559,.T.);
#8712=EDGE_CURVE('',#6711,#6709,#1361,.T.);
#8713=EDGE_CURVE('',#6712,#6710,#1362,.T.);
#8714=EDGE_CURVE('',#6713,#6714,#4560,.T.);
#8715=EDGE_CURVE('',#6713,#6711,#1363,.T.);
#8716=EDGE_CURVE('',#6714,#6712,#1364,.T.);
#8717=EDGE_CURVE('',#6715,#6716,#4561,.T.);
#8718=EDGE_CURVE('',#6715,#6713,#1365,.T.);
#8719=EDGE_CURVE('',#6716,#6714,#1366,.T.);
#8720=EDGE_CURVE('',#6717,#6718,#4562,.T.);
#8721=EDGE_CURVE('',#6717,#6715,#1367,.T.);
#8722=EDGE_CURVE('',#6718,#6716,#1368,.T.);
#8723=EDGE_CURVE('',#6719,#6720,#4563,.T.);
#8724=EDGE_CURVE('',#6719,#6717,#1369,.T.);
#8725=EDGE_CURVE('',#6720,#6718,#1370,.T.);
#8726=EDGE_CURVE('',#6721,#6722,#4564,.T.);
#8727=EDGE_CURVE('',#6721,#6719,#1371,.T.);
#8728=EDGE_CURVE('',#6722,#6720,#1372,.T.);
#8729=EDGE_CURVE('',#6723,#6724,#4565,.T.);
#8730=EDGE_CURVE('',#6723,#6721,#1373,.T.);
#8731=EDGE_CURVE('',#6724,#6722,#1374,.T.);
#8732=EDGE_CURVE('',#6725,#6726,#4566,.T.);
#8733=EDGE_CURVE('',#6725,#6723,#1375,.T.);
#8734=EDGE_CURVE('',#6726,#6724,#1376,.T.);
#8735=EDGE_CURVE('',#6727,#6728,#4567,.T.);
#8736=EDGE_CURVE('',#6727,#6725,#1377,.T.);
#8737=EDGE_CURVE('',#6728,#6726,#1378,.T.);
#8738=EDGE_CURVE('',#6729,#6730,#4568,.T.);
#8739=EDGE_CURVE('',#6729,#6727,#1379,.T.);
#8740=EDGE_CURVE('',#6730,#6728,#1380,.T.);
#8741=EDGE_CURVE('',#6731,#6732,#4569,.T.);
#8742=EDGE_CURVE('',#6731,#6729,#1381,.T.);
#8743=EDGE_CURVE('',#6732,#6730,#1382,.T.);
#8744=EDGE_CURVE('',#6733,#6734,#4570,.T.);
#8745=EDGE_CURVE('',#6733,#6731,#1383,.T.);
#8746=EDGE_CURVE('',#6734,#6732,#1384,.T.);
#8747=EDGE_CURVE('',#6735,#6736,#4571,.T.);
#8748=EDGE_CURVE('',#6735,#6733,#1385,.T.);
#8749=EDGE_CURVE('',#6736,#6734,#1386,.T.);
#8750=EDGE_CURVE('',#6737,#6738,#4572,.T.);
#8751=EDGE_CURVE('',#6737,#6735,#1387,.T.);
#8752=EDGE_CURVE('',#6738,#6736,#1388,.T.);
#8753=EDGE_CURVE('',#6739,#6740,#4573,.T.);
#8754=EDGE_CURVE('',#6739,#6737,#1389,.T.);
#8755=EDGE_CURVE('',#6740,#6738,#1390,.T.);
#8756=EDGE_CURVE('',#6741,#6742,#4574,.T.);
#8757=EDGE_CURVE('',#6741,#6739,#1391,.T.);
#8758=EDGE_CURVE('',#6742,#6740,#1392,.T.);
#8759=EDGE_CURVE('',#6743,#6744,#4575,.T.);
#8760=EDGE_CURVE('',#6743,#6741,#1393,.T.);
#8761=EDGE_CURVE('',#6744,#6742,#1394,.T.);
#8762=EDGE_CURVE('',#6745,#6746,#4576,.T.);
#8763=EDGE_CURVE('',#6745,#6743,#1395,.T.);
#8764=EDGE_CURVE('',#6746,#6744,#1396,.T.);
#8765=EDGE_CURVE('',#6747,#6748,#4577,.T.);
#8766=EDGE_CURVE('',#6747,#6745,#1397,.T.);
#8767=EDGE_CURVE('',#6748,#6746,#1398,.T.);
#8768=EDGE_CURVE('',#6749,#6750,#4578,.T.);
#8769=EDGE_CURVE('',#6749,#6747,#1399,.T.);
#8770=EDGE_CURVE('',#6750,#6748,#1400,.T.);
#8771=EDGE_CURVE('',#6751,#6752,#4579,.T.);
#8772=EDGE_CURVE('',#6751,#6749,#1401,.T.);
#8773=EDGE_CURVE('',#6752,#6750,#1402,.T.);
#8774=EDGE_CURVE('',#6753,#6754,#4580,.T.);
#8775=EDGE_CURVE('',#6753,#6751,#1403,.T.);
#8776=EDGE_CURVE('',#6754,#6752,#1404,.T.);
#8777=EDGE_CURVE('',#6755,#6756,#4581,.T.);
#8778=EDGE_CURVE('',#6755,#6753,#1405,.T.);
#8779=EDGE_CURVE('',#6756,#6754,#1406,.T.);
#8780=EDGE_CURVE('',#6757,#6758,#4582,.T.);
#8781=EDGE_CURVE('',#6757,#6755,#1407,.T.);
#8782=EDGE_CURVE('',#6758,#6756,#1408,.T.);
#8783=EDGE_CURVE('',#6759,#6760,#4583,.T.);
#8784=EDGE_CURVE('',#6759,#6757,#1409,.T.);
#8785=EDGE_CURVE('',#6760,#6758,#1410,.T.);
#8786=EDGE_CURVE('',#6761,#6762,#4584,.T.);
#8787=EDGE_CURVE('',#6761,#6759,#1411,.T.);
#8788=EDGE_CURVE('',#6762,#6760,#1412,.T.);
#8789=EDGE_CURVE('',#6763,#6764,#4585,.T.);
#8790=EDGE_CURVE('',#6763,#6761,#1413,.T.);
#8791=EDGE_CURVE('',#6764,#6762,#1414,.T.);
#8792=EDGE_CURVE('',#6765,#6766,#4586,.T.);
#8793=EDGE_CURVE('',#6765,#6763,#1415,.T.);
#8794=EDGE_CURVE('',#6766,#6764,#1416,.T.);
#8795=EDGE_CURVE('',#6767,#6768,#4587,.T.);
#8796=EDGE_CURVE('',#6767,#6765,#1417,.T.);
#8797=EDGE_CURVE('',#6768,#6766,#1418,.T.);
#8798=EDGE_CURVE('',#6769,#6770,#4588,.T.);
#8799=EDGE_CURVE('',#6769,#6767,#1419,.T.);
#8800=EDGE_CURVE('',#6770,#6768,#1420,.T.);
#8801=EDGE_CURVE('',#6771,#6772,#4589,.T.);
#8802=EDGE_CURVE('',#6771,#6769,#1421,.T.);
#8803=EDGE_CURVE('',#6772,#6770,#1422,.T.);
#8804=EDGE_CURVE('',#6773,#6774,#4590,.T.);
#8805=EDGE_CURVE('',#6773,#6771,#1423,.T.);
#8806=EDGE_CURVE('',#6774,#6772,#1424,.T.);
#8807=EDGE_CURVE('',#6775,#6776,#4591,.T.);
#8808=EDGE_CURVE('',#6775,#6773,#1425,.T.);
#8809=EDGE_CURVE('',#6776,#6774,#1426,.T.);
#8810=EDGE_CURVE('',#6777,#6778,#4592,.T.);
#8811=EDGE_CURVE('',#6777,#6775,#1427,.T.);
#8812=EDGE_CURVE('',#6778,#6776,#1428,.T.);
#8813=EDGE_CURVE('',#6779,#6780,#4593,.T.);
#8814=EDGE_CURVE('',#6779,#6777,#1429,.T.);
#8815=EDGE_CURVE('',#6780,#6778,#1430,.T.);
#8816=EDGE_CURVE('',#6781,#6782,#4594,.T.);
#8817=EDGE_CURVE('',#6781,#6779,#1431,.T.);
#8818=EDGE_CURVE('',#6782,#6780,#1432,.T.);
#8819=EDGE_CURVE('',#6783,#6784,#4595,.T.);
#8820=EDGE_CURVE('',#6783,#6781,#1433,.T.);
#8821=EDGE_CURVE('',#6784,#6782,#1434,.T.);
#8822=EDGE_CURVE('',#6785,#6786,#4596,.T.);
#8823=EDGE_CURVE('',#6785,#6783,#1435,.T.);
#8824=EDGE_CURVE('',#6786,#6784,#1436,.T.);
#8825=EDGE_CURVE('',#6787,#6788,#4597,.T.);
#8826=EDGE_CURVE('',#6787,#6785,#1437,.T.);
#8827=EDGE_CURVE('',#6788,#6786,#1438,.T.);
#8828=EDGE_CURVE('',#6789,#6790,#4598,.T.);
#8829=EDGE_CURVE('',#6789,#6787,#1439,.T.);
#8830=EDGE_CURVE('',#6790,#6788,#1440,.T.);
#8831=EDGE_CURVE('',#6791,#6792,#4599,.T.);
#8832=EDGE_CURVE('',#6791,#6789,#1441,.T.);
#8833=EDGE_CURVE('',#6792,#6790,#1442,.T.);
#8834=EDGE_CURVE('',#6793,#6794,#4600,.T.);
#8835=EDGE_CURVE('',#6793,#6791,#1443,.T.);
#8836=EDGE_CURVE('',#6794,#6792,#1444,.T.);
#8837=EDGE_CURVE('',#6795,#6796,#4601,.T.);
#8838=EDGE_CURVE('',#6795,#6793,#1445,.T.);
#8839=EDGE_CURVE('',#6796,#6794,#1446,.T.);
#8840=EDGE_CURVE('',#6797,#6798,#4602,.T.);
#8841=EDGE_CURVE('',#6797,#6795,#1447,.T.);
#8842=EDGE_CURVE('',#6798,#6796,#1448,.T.);
#8843=EDGE_CURVE('',#6799,#6800,#4603,.T.);
#8844=EDGE_CURVE('',#6799,#6797,#1449,.T.);
#8845=EDGE_CURVE('',#6800,#6798,#1450,.T.);
#8846=EDGE_CURVE('',#6801,#6802,#4604,.T.);
#8847=EDGE_CURVE('',#6801,#6799,#1451,.T.);
#8848=EDGE_CURVE('',#6802,#6800,#1452,.T.);
#8849=EDGE_CURVE('',#6803,#6804,#4605,.T.);
#8850=EDGE_CURVE('',#6803,#6801,#1453,.T.);
#8851=EDGE_CURVE('',#6804,#6802,#1454,.T.);
#8852=EDGE_CURVE('',#6805,#6806,#4606,.T.);
#8853=EDGE_CURVE('',#6805,#6803,#1455,.T.);
#8854=EDGE_CURVE('',#6806,#6804,#1456,.T.);
#8855=EDGE_CURVE('',#6807,#6808,#4607,.T.);
#8856=EDGE_CURVE('',#6807,#6805,#1457,.T.);
#8857=EDGE_CURVE('',#6808,#6806,#1458,.T.);
#8858=EDGE_CURVE('',#6809,#6810,#4608,.T.);
#8859=EDGE_CURVE('',#6809,#6807,#1459,.T.);
#8860=EDGE_CURVE('',#6810,#6808,#1460,.T.);
#8861=EDGE_CURVE('',#6811,#6812,#4609,.T.);
#8862=EDGE_CURVE('',#6811,#6809,#1461,.T.);
#8863=EDGE_CURVE('',#6812,#6810,#1462,.T.);
#8864=EDGE_CURVE('',#6813,#6814,#4610,.T.);
#8865=EDGE_CURVE('',#6813,#6811,#1463,.T.);
#8866=EDGE_CURVE('',#6814,#6812,#1464,.T.);
#8867=EDGE_CURVE('',#6815,#6816,#4611,.T.);
#8868=EDGE_CURVE('',#6815,#6813,#1465,.T.);
#8869=EDGE_CURVE('',#6816,#6814,#1466,.T.);
#8870=EDGE_CURVE('',#6817,#6818,#4612,.T.);
#8871=EDGE_CURVE('',#6817,#6815,#1467,.T.);
#8872=EDGE_CURVE('',#6818,#6816,#1468,.T.);
#8873=EDGE_CURVE('',#6819,#6820,#4613,.T.);
#8874=EDGE_CURVE('',#6819,#6817,#1469,.T.);
#8875=EDGE_CURVE('',#6820,#6818,#1470,.T.);
#8876=EDGE_CURVE('',#6821,#6822,#4614,.T.);
#8877=EDGE_CURVE('',#6821,#6819,#1471,.T.);
#8878=EDGE_CURVE('',#6822,#6820,#1472,.T.);
#8879=EDGE_CURVE('',#6823,#6704,#1473,.T.);
#8880=EDGE_CURVE('',#6700,#6823,#1474,.T.);
#8881=EDGE_CURVE('',#6824,#6582,#1475,.T.);
#8882=EDGE_CURVE('',#6824,#6822,#1476,.T.);
#8883=EDGE_CURVE('',#6825,#6824,#463,.T.);
#8884=EDGE_CURVE('',#6825,#6821,#1477,.T.);
#8885=EDGE_CURVE('',#6703,#6826,#1478,.T.);
#8886=EDGE_CURVE('',#6581,#6825,#1479,.T.);
#8887=EDGE_CURVE('',#6826,#6699,#1480,.T.);
#8888=EDGE_CURVE('',#6826,#6823,#464,.F.);
#8889=EDGE_CURVE('',#6827,#6828,#4615,.T.);
#8890=EDGE_CURVE('',#6828,#6829,#4616,.T.);
#8891=EDGE_CURVE('',#6829,#6830,#4617,.T.);
#8892=EDGE_CURVE('',#6830,#6831,#4618,.T.);
#8893=EDGE_CURVE('',#6831,#6832,#4619,.T.);
#8894=EDGE_CURVE('',#6832,#6827,#4620,.T.);
#8895=EDGE_CURVE('',#6833,#6834,#4621,.T.);
#8896=EDGE_CURVE('',#6835,#6833,#4622,.T.);
#8897=EDGE_CURVE('',#6836,#6835,#4623,.T.);
#8898=EDGE_CURVE('',#6837,#6836,#4624,.T.);
#8899=EDGE_CURVE('',#6838,#6837,#4625,.T.);
#8900=EDGE_CURVE('',#6834,#6838,#4626,.T.);
#8901=EDGE_CURVE('',#6839,#6839,#465,.T.);
#8902=EDGE_CURVE('',#6833,#6827,#4627,.T.);
#8903=EDGE_CURVE('',#6835,#6832,#4628,.T.);
#8904=EDGE_CURVE('',#6836,#6831,#4629,.T.);
#8905=EDGE_CURVE('',#6837,#6830,#4630,.T.);
#8906=EDGE_CURVE('',#6838,#6829,#4631,.T.);
#8907=EDGE_CURVE('',#6834,#6828,#4632,.T.);
#8908=EDGE_CURVE('',#6839,#6840,#4633,.T.);
#8909=EDGE_CURVE('',#6840,#6840,#466,.T.);
#8910=EDGE_CURVE('',#6840,#6841,#467,.T.);
#8911=EDGE_CURVE('',#6842,#6843,#4634,.T.);
#8912=EDGE_CURVE('',#6843,#6844,#1481,.T.);
#8913=EDGE_CURVE('',#6845,#6844,#468,.F.);
#8914=EDGE_CURVE('',#6845,#6842,#1482,.T.);
#8915=EDGE_CURVE('',#6846,#6847,#4635,.T.);
#8916=EDGE_CURVE('',#6847,#6843,#1483,.T.);
#8917=EDGE_CURVE('',#6842,#6846,#1484,.T.);
#8918=EDGE_CURVE('',#6848,#6849,#4636,.T.);
#8919=EDGE_CURVE('',#6849,#6847,#1485,.T.);
#8920=EDGE_CURVE('',#6846,#6848,#1486,.T.);
#8921=EDGE_CURVE('',#6850,#6851,#4637,.T.);
#8922=EDGE_CURVE('',#6851,#6849,#1487,.T.);
#8923=EDGE_CURVE('',#6848,#6850,#1488,.T.);
#8924=EDGE_CURVE('',#6852,#6853,#4638,.T.);
#8925=EDGE_CURVE('',#6853,#6851,#1489,.T.);
#8926=EDGE_CURVE('',#6850,#6852,#1490,.T.);
#8927=EDGE_CURVE('',#6854,#6855,#4639,.T.);
#8928=EDGE_CURVE('',#6855,#6853,#1491,.T.);
#8929=EDGE_CURVE('',#6852,#6854,#1492,.T.);
#8930=EDGE_CURVE('',#6856,#6857,#4640,.T.);
#8931=EDGE_CURVE('',#6857,#6855,#1493,.T.);
#8932=EDGE_CURVE('',#6854,#6856,#1494,.T.);
#8933=EDGE_CURVE('',#6858,#6859,#4641,.T.);
#8934=EDGE_CURVE('',#6858,#6860,#1495,.T.);
#8935=EDGE_CURVE('',#6861,#6860,#469,.T.);
#8936=EDGE_CURVE('',#6861,#6859,#1496,.T.);
#8937=EDGE_CURVE('',#6862,#6863,#4642,.T.);
#8938=EDGE_CURVE('',#6863,#6864,#1497,.T.);
#8939=EDGE_CURVE('',#6865,#6864,#470,.T.);
#8940=EDGE_CURVE('',#6862,#6865,#1498,.T.);
#8941=EDGE_CURVE('',#6866,#6867,#4643,.T.);
#8942=EDGE_CURVE('',#6867,#6863,#1499,.T.);
#8943=EDGE_CURVE('',#6866,#6862,#1500,.T.);
#8944=EDGE_CURVE('',#6868,#6869,#4644,.T.);
#8945=EDGE_CURVE('',#6869,#6867,#1501,.T.);
#8946=EDGE_CURVE('',#6868,#6866,#1502,.T.);
#8947=EDGE_CURVE('',#6870,#6871,#4645,.T.);
#8948=EDGE_CURVE('',#6871,#6869,#1503,.T.);
#8949=EDGE_CURVE('',#6870,#6868,#1504,.T.);
#8950=EDGE_CURVE('',#6872,#6873,#4646,.T.);
#8951=EDGE_CURVE('',#6873,#6871,#1505,.T.);
#8952=EDGE_CURVE('',#6872,#6870,#1506,.T.);
#8953=EDGE_CURVE('',#6874,#6875,#4647,.T.);
#8954=EDGE_CURVE('',#6875,#6873,#1507,.T.);
#8955=EDGE_CURVE('',#6874,#6872,#1508,.T.);
#8956=EDGE_CURVE('',#6876,#6877,#4648,.T.);
#8957=EDGE_CURVE('',#6877,#6875,#1509,.T.);
#8958=EDGE_CURVE('',#6876,#6874,#1510,.T.);
#8959=EDGE_CURVE('',#6878,#6879,#4649,.T.);
#8960=EDGE_CURVE('',#6880,#6878,#1511,.T.);
#8961=EDGE_CURVE('',#6881,#6880,#471,.T.);
#8962=EDGE_CURVE('',#6881,#6879,#1512,.T.);
#8963=EDGE_CURVE('',#6879,#6877,#1513,.T.);
#8964=EDGE_CURVE('',#6878,#6876,#1514,.T.);
#8965=EDGE_CURVE('',#6864,#6845,#1515,.T.);
#8966=EDGE_CURVE('',#6860,#6881,#1516,.T.);
#8967=EDGE_CURVE('',#6856,#6858,#1517,.T.);
#8968=EDGE_CURVE('',#6844,#6865,#1518,.T.);
#8969=EDGE_CURVE('',#6859,#6857,#1519,.T.);
#8970=EDGE_CURVE('',#6880,#6861,#1520,.T.);
#8971=EDGE_CURVE('',#6882,#6883,#4650,.T.);
#8972=EDGE_CURVE('',#6883,#6884,#4651,.T.);
#8973=EDGE_CURVE('',#6884,#6885,#4652,.T.);
#8974=EDGE_CURVE('',#6885,#6886,#4653,.T.);
#8975=EDGE_CURVE('',#6886,#6887,#4654,.T.);
#8976=EDGE_CURVE('',#6887,#6882,#4655,.T.);
#8977=EDGE_CURVE('',#6888,#6889,#4656,.T.);
#8978=EDGE_CURVE('',#6889,#6882,#4657,.T.);
#8979=EDGE_CURVE('',#6888,#6887,#4658,.T.);
#8980=EDGE_CURVE('',#6890,#6888,#4659,.T.);
#8981=EDGE_CURVE('',#6890,#6886,#4660,.T.);
#8982=EDGE_CURVE('',#6891,#6890,#4661,.T.);
#8983=EDGE_CURVE('',#6891,#6885,#4662,.T.);
#8984=EDGE_CURVE('',#6892,#6891,#4663,.T.);
#8985=EDGE_CURVE('',#6892,#6884,#4664,.T.);
#8986=EDGE_CURVE('',#6893,#6892,#4665,.T.);
#8987=EDGE_CURVE('',#6893,#6883,#4666,.T.);
#8988=EDGE_CURVE('',#6889,#6893,#4667,.T.);
#8989=EDGE_CURVE('',#6894,#6894,#472,.T.);
#8990=EDGE_CURVE('',#6894,#6895,#4668,.T.);
#8991=EDGE_CURVE('',#6895,#6895,#473,.T.);
#8992=EDGE_CURVE('',#6896,#6896,#474,.T.);
#8993=EDGE_CURVE('',#6896,#6897,#4669,.T.);
#8994=EDGE_CURVE('',#6897,#6897,#475,.T.);
#8995=EDGE_CURVE('',#6898,#6899,#4670,.T.);
#8996=EDGE_CURVE('',#6898,#6900,#1521,.T.);
#8997=EDGE_CURVE('',#6900,#6901,#476,.F.);
#8998=EDGE_CURVE('',#6901,#6899,#1522,.T.);
#8999=EDGE_CURVE('',#6902,#6903,#4671,.T.);
#9000=EDGE_CURVE('',#6902,#6898,#1523,.T.);
#9001=EDGE_CURVE('',#6899,#6903,#1524,.T.);
#9002=EDGE_CURVE('',#6904,#6905,#4672,.T.);
#9003=EDGE_CURVE('',#6904,#6902,#1525,.T.);
#9004=EDGE_CURVE('',#6903,#6905,#1526,.T.);
#9005=EDGE_CURVE('',#6906,#6907,#4673,.T.);
#9006=EDGE_CURVE('',#6906,#6904,#1527,.T.);
#9007=EDGE_CURVE('',#6905,#6907,#1528,.T.);
#9008=EDGE_CURVE('',#6908,#6909,#4674,.T.);
#9009=EDGE_CURVE('',#6908,#6906,#1529,.T.);
#9010=EDGE_CURVE('',#6907,#6909,#1530,.T.);
#9011=EDGE_CURVE('',#6910,#6911,#4675,.T.);
#9012=EDGE_CURVE('',#6910,#6908,#1531,.T.);
#9013=EDGE_CURVE('',#6909,#6911,#1532,.T.);
#9014=EDGE_CURVE('',#6912,#6913,#4676,.T.);
#9015=EDGE_CURVE('',#6912,#6910,#1533,.T.);
#9016=EDGE_CURVE('',#6911,#6913,#1534,.T.);
#9017=EDGE_CURVE('',#6914,#6915,#4677,.T.);
#9018=EDGE_CURVE('',#6914,#6912,#1535,.T.);
#9019=EDGE_CURVE('',#6913,#6915,#1536,.T.);
#9020=EDGE_CURVE('',#6916,#6917,#4678,.T.);
#9021=EDGE_CURVE('',#6916,#6914,#1537,.T.);
#9022=EDGE_CURVE('',#6915,#6917,#1538,.T.);
#9023=EDGE_CURVE('',#6918,#6919,#4679,.T.);
#9024=EDGE_CURVE('',#6918,#6916,#1539,.T.);
#9025=EDGE_CURVE('',#6917,#6919,#1540,.T.);
#9026=EDGE_CURVE('',#6920,#6921,#4680,.T.);
#9027=EDGE_CURVE('',#6920,#6918,#1541,.T.);
#9028=EDGE_CURVE('',#6919,#6921,#1542,.T.);
#9029=EDGE_CURVE('',#6922,#6923,#4681,.T.);
#9030=EDGE_CURVE('',#6922,#6920,#1543,.T.);
#9031=EDGE_CURVE('',#6921,#6923,#1544,.T.);
#9032=EDGE_CURVE('',#6924,#6925,#4682,.T.);
#9033=EDGE_CURVE('',#6924,#6922,#1545,.T.);
#9034=EDGE_CURVE('',#6923,#6925,#1546,.T.);
#9035=EDGE_CURVE('',#6926,#6927,#4683,.T.);
#9036=EDGE_CURVE('',#6926,#6924,#1547,.T.);
#9037=EDGE_CURVE('',#6925,#6927,#1548,.T.);
#9038=EDGE_CURVE('',#6928,#6929,#4684,.T.);
#9039=EDGE_CURVE('',#6928,#6926,#1549,.T.);
#9040=EDGE_CURVE('',#6927,#6929,#1550,.T.);
#9041=EDGE_CURVE('',#6930,#6931,#4685,.T.);
#9042=EDGE_CURVE('',#6930,#6932,#1551,.T.);
#9043=EDGE_CURVE('',#6932,#6933,#477,.T.);
#9044=EDGE_CURVE('',#6931,#6933,#1552,.T.);
#9045=EDGE_CURVE('',#6934,#6935,#4686,.T.);
#9046=EDGE_CURVE('',#6934,#6930,#1553,.T.);
#9047=EDGE_CURVE('',#6935,#6931,#1554,.T.);
#9048=EDGE_CURVE('',#6936,#6937,#4687,.T.);
#9049=EDGE_CURVE('',#6936,#6934,#1555,.T.);
#9050=EDGE_CURVE('',#6937,#6935,#1556,.T.);
#9051=EDGE_CURVE('',#6938,#6939,#4688,.T.);
#9052=EDGE_CURVE('',#6938,#6936,#1557,.T.);
#9053=EDGE_CURVE('',#6939,#6937,#1558,.T.);
#9054=EDGE_CURVE('',#6940,#6941,#4689,.T.);
#9055=EDGE_CURVE('',#6940,#6938,#1559,.T.);
#9056=EDGE_CURVE('',#6941,#6939,#1560,.T.);
#9057=EDGE_CURVE('',#6942,#6943,#4690,.T.);
#9058=EDGE_CURVE('',#6942,#6940,#1561,.T.);
#9059=EDGE_CURVE('',#6943,#6941,#1562,.T.);
#9060=EDGE_CURVE('',#6944,#6945,#4691,.T.);
#9061=EDGE_CURVE('',#6944,#6942,#1563,.T.);
#9062=EDGE_CURVE('',#6945,#6943,#1564,.T.);
#9063=EDGE_CURVE('',#6946,#6947,#4692,.T.);
#9064=EDGE_CURVE('',#6946,#6944,#1565,.T.);
#9065=EDGE_CURVE('',#6947,#6945,#1566,.T.);
#9066=EDGE_CURVE('',#6948,#6949,#4693,.T.);
#9067=EDGE_CURVE('',#6948,#6946,#1567,.T.);
#9068=EDGE_CURVE('',#6949,#6947,#1568,.T.);
#9069=EDGE_CURVE('',#6950,#6951,#4694,.T.);
#9070=EDGE_CURVE('',#6950,#6948,#1569,.T.);
#9071=EDGE_CURVE('',#6951,#6949,#1570,.T.);
#9072=EDGE_CURVE('',#6952,#6953,#4695,.T.);
#9073=EDGE_CURVE('',#6952,#6950,#1571,.T.);
#9074=EDGE_CURVE('',#6953,#6951,#1572,.T.);
#9075=EDGE_CURVE('',#6954,#6955,#4696,.T.);
#9076=EDGE_CURVE('',#6954,#6952,#1573,.T.);
#9077=EDGE_CURVE('',#6955,#6953,#1574,.T.);
#9078=EDGE_CURVE('',#6956,#6957,#4697,.T.);
#9079=EDGE_CURVE('',#6956,#6954,#1575,.T.);
#9080=EDGE_CURVE('',#6957,#6955,#1576,.T.);
#9081=EDGE_CURVE('',#6958,#6959,#4698,.T.);
#9082=EDGE_CURVE('',#6958,#6956,#1577,.T.);
#9083=EDGE_CURVE('',#6959,#6957,#1578,.T.);
#9084=EDGE_CURVE('',#6960,#6961,#4699,.T.);
#9085=EDGE_CURVE('',#6960,#6958,#1579,.T.);
#9086=EDGE_CURVE('',#6961,#6959,#1580,.T.);
#9087=EDGE_CURVE('',#6933,#6962,#1581,.T.);
#9088=EDGE_CURVE('',#6963,#6932,#1582,.T.);
#9089=EDGE_CURVE('',#6964,#6963,#478,.T.);
#9090=EDGE_CURVE('',#6962,#6964,#1583,.T.);
#9091=EDGE_CURVE('',#6962,#6965,#4700,.T.);
#9092=EDGE_CURVE('',#6965,#6965,#479,.T.);
#9093=EDGE_CURVE('',#6966,#6960,#1584,.T.);
#9094=EDGE_CURVE('',#6900,#6966,#1585,.T.);
#9095=EDGE_CURVE('',#6963,#6928,#1586,.T.);
#9096=EDGE_CURVE('',#6967,#6961,#1587,.T.);
#9097=EDGE_CURVE('',#6966,#6967,#480,.T.);
#9098=EDGE_CURVE('',#6929,#6964,#1588,.T.);
#9099=EDGE_CURVE('',#6967,#6901,#1589,.T.);
#9100=EDGE_CURVE('',#6968,#6969,#4701,.T.);
#9101=EDGE_CURVE('',#6968,#6970,#4702,.T.);
#9102=EDGE_CURVE('',#6970,#6971,#4703,.T.);
#9103=EDGE_CURVE('',#6969,#6971,#4704,.T.);
#9104=EDGE_CURVE('',#6972,#6968,#4705,.T.);
#9105=EDGE_CURVE('',#6972,#6973,#4706,.T.);
#9106=EDGE_CURVE('',#6973,#6970,#4707,.T.);
#9107=EDGE_CURVE('',#6974,#6972,#4708,.T.);
#9108=EDGE_CURVE('',#6974,#6975,#4709,.T.);
#9109=EDGE_CURVE('',#6975,#6973,#4710,.T.);
#9110=EDGE_CURVE('',#6976,#6974,#4711,.T.);
#9111=EDGE_CURVE('',#6976,#6977,#4712,.T.);
#9112=EDGE_CURVE('',#6977,#6975,#4713,.T.);
#9113=EDGE_CURVE('',#6978,#6976,#4714,.T.);
#9114=EDGE_CURVE('',#6978,#6979,#4715,.T.);
#9115=EDGE_CURVE('',#6979,#6977,#4716,.T.);
#9116=EDGE_CURVE('',#6969,#6978,#4717,.T.);
#9117=EDGE_CURVE('',#6971,#6979,#4718,.T.);
#9118=EDGE_CURVE('',#6980,#6980,#481,.T.);
#9119=EDGE_CURVE('',#6980,#6981,#4719,.T.);
#9120=EDGE_CURVE('',#6981,#6981,#482,.T.);
#9121=EDGE_CURVE('',#6982,#6982,#483,.T.);
#9122=EDGE_CURVE('',#6982,#6983,#4720,.T.);
#9123=EDGE_CURVE('',#6983,#6983,#484,.T.);
#9124=EDGE_CURVE('',#6984,#6984,#485,.T.);
#9125=EDGE_CURVE('',#6984,#6985,#4721,.T.);
#9126=EDGE_CURVE('',#6985,#6985,#486,.T.);
#9127=ORIENTED_EDGE('',*,*,#6986,.T.);
#9128=ORIENTED_EDGE('',*,*,#6987,.T.);
#9129=ORIENTED_EDGE('',*,*,#6988,.F.);
#9130=ORIENTED_EDGE('',*,*,#6989,.F.);
#9131=ORIENTED_EDGE('',*,*,#6990,.T.);
#9132=ORIENTED_EDGE('',*,*,#6989,.T.);
#9133=ORIENTED_EDGE('',*,*,#6991,.F.);
#9134=ORIENTED_EDGE('',*,*,#6992,.F.);
#9135=ORIENTED_EDGE('',*,*,#6993,.T.);
#9136=ORIENTED_EDGE('',*,*,#6992,.T.);
#9137=ORIENTED_EDGE('',*,*,#6994,.F.);
#9138=ORIENTED_EDGE('',*,*,#6995,.F.);
#9139=ORIENTED_EDGE('',*,*,#6996,.T.);
#9140=ORIENTED_EDGE('',*,*,#6995,.T.);
#9141=ORIENTED_EDGE('',*,*,#6997,.F.);
#9142=ORIENTED_EDGE('',*,*,#6987,.F.);
#9143=ORIENTED_EDGE('',*,*,#6998,.T.);
#9144=ORIENTED_EDGE('',*,*,#6999,.T.);
#9145=ORIENTED_EDGE('',*,*,#7000,.F.);
#9146=ORIENTED_EDGE('',*,*,#7001,.F.);
#9147=ORIENTED_EDGE('',*,*,#7002,.T.);
#9148=ORIENTED_EDGE('',*,*,#7001,.T.);
#9149=ORIENTED_EDGE('',*,*,#7003,.F.);
#9150=ORIENTED_EDGE('',*,*,#7004,.F.);
#9151=ORIENTED_EDGE('',*,*,#7005,.T.);
#9152=ORIENTED_EDGE('',*,*,#7004,.T.);
#9153=ORIENTED_EDGE('',*,*,#7006,.F.);
#9154=ORIENTED_EDGE('',*,*,#7007,.F.);
#9155=ORIENTED_EDGE('',*,*,#7008,.T.);
#9156=ORIENTED_EDGE('',*,*,#7007,.T.);
#9157=ORIENTED_EDGE('',*,*,#7009,.F.);
#9158=ORIENTED_EDGE('',*,*,#6999,.F.);
#9159=ORIENTED_EDGE('',*,*,#7009,.T.);
#9160=ORIENTED_EDGE('',*,*,#7006,.T.);
#9161=ORIENTED_EDGE('',*,*,#7003,.T.);
#9162=ORIENTED_EDGE('',*,*,#7000,.T.);
#9163=ORIENTED_EDGE('',*,*,#6997,.T.);
#9164=ORIENTED_EDGE('',*,*,#6994,.T.);
#9165=ORIENTED_EDGE('',*,*,#6991,.T.);
#9166=ORIENTED_EDGE('',*,*,#6988,.T.);
#9167=ORIENTED_EDGE('',*,*,#7008,.F.);
#9168=ORIENTED_EDGE('',*,*,#6998,.F.);
#9169=ORIENTED_EDGE('',*,*,#7002,.F.);
#9170=ORIENTED_EDGE('',*,*,#7005,.F.);
#9171=ORIENTED_EDGE('',*,*,#6996,.F.);
#9172=ORIENTED_EDGE('',*,*,#6986,.F.);
#9173=ORIENTED_EDGE('',*,*,#6990,.F.);
#9174=ORIENTED_EDGE('',*,*,#6993,.F.);
#9175=ORIENTED_EDGE('',*,*,#7010,.T.);
#9176=ORIENTED_EDGE('',*,*,#7011,.T.);
#9177=ORIENTED_EDGE('',*,*,#7012,.F.);
#9178=ORIENTED_EDGE('',*,*,#7013,.F.);
#9179=ORIENTED_EDGE('',*,*,#7014,.T.);
#9180=ORIENTED_EDGE('',*,*,#7013,.T.);
#9181=ORIENTED_EDGE('',*,*,#7015,.F.);
#9182=ORIENTED_EDGE('',*,*,#7016,.F.);
#9183=ORIENTED_EDGE('',*,*,#7017,.T.);
#9184=ORIENTED_EDGE('',*,*,#7016,.T.);
#9185=ORIENTED_EDGE('',*,*,#7018,.F.);
#9186=ORIENTED_EDGE('',*,*,#7019,.F.);
#9187=ORIENTED_EDGE('',*,*,#7020,.T.);
#9188=ORIENTED_EDGE('',*,*,#7019,.T.);
#9189=ORIENTED_EDGE('',*,*,#7021,.F.);
#9190=ORIENTED_EDGE('',*,*,#7011,.F.);
#9191=ORIENTED_EDGE('',*,*,#7022,.T.);
#9192=ORIENTED_EDGE('',*,*,#7023,.T.);
#9193=ORIENTED_EDGE('',*,*,#7024,.F.);
#9194=ORIENTED_EDGE('',*,*,#7025,.F.);
#9195=ORIENTED_EDGE('',*,*,#7026,.T.);
#9196=ORIENTED_EDGE('',*,*,#7025,.T.);
#9197=ORIENTED_EDGE('',*,*,#7027,.F.);
#9198=ORIENTED_EDGE('',*,*,#7028,.F.);
#9199=ORIENTED_EDGE('',*,*,#7029,.T.);
#9200=ORIENTED_EDGE('',*,*,#7028,.T.);
#9201=ORIENTED_EDGE('',*,*,#7030,.F.);
#9202=ORIENTED_EDGE('',*,*,#7031,.F.);
#9203=ORIENTED_EDGE('',*,*,#7032,.T.);
#9204=ORIENTED_EDGE('',*,*,#7031,.T.);
#9205=ORIENTED_EDGE('',*,*,#7033,.F.);
#9206=ORIENTED_EDGE('',*,*,#7023,.F.);
#9207=ORIENTED_EDGE('',*,*,#7033,.T.);
#9208=ORIENTED_EDGE('',*,*,#7030,.T.);
#9209=ORIENTED_EDGE('',*,*,#7027,.T.);
#9210=ORIENTED_EDGE('',*,*,#7024,.T.);
#9211=ORIENTED_EDGE('',*,*,#7021,.T.);
#9212=ORIENTED_EDGE('',*,*,#7018,.T.);
#9213=ORIENTED_EDGE('',*,*,#7015,.T.);
#9214=ORIENTED_EDGE('',*,*,#7012,.T.);
#9215=ORIENTED_EDGE('',*,*,#7032,.F.);
#9216=ORIENTED_EDGE('',*,*,#7022,.F.);
#9217=ORIENTED_EDGE('',*,*,#7026,.F.);
#9218=ORIENTED_EDGE('',*,*,#7029,.F.);
#9219=ORIENTED_EDGE('',*,*,#7020,.F.);
#9220=ORIENTED_EDGE('',*,*,#7010,.F.);
#9221=ORIENTED_EDGE('',*,*,#7014,.F.);
#9222=ORIENTED_EDGE('',*,*,#7017,.F.);
#9223=ORIENTED_EDGE('',*,*,#7034,.T.);
#9224=ORIENTED_EDGE('',*,*,#7035,.T.);
#9225=ORIENTED_EDGE('',*,*,#7036,.F.);
#9226=ORIENTED_EDGE('',*,*,#7037,.T.);
#9227=ORIENTED_EDGE('',*,*,#7038,.T.);
#9228=ORIENTED_EDGE('',*,*,#7039,.T.);
#9229=ORIENTED_EDGE('',*,*,#7034,.F.);
#9230=ORIENTED_EDGE('',*,*,#7040,.T.);
#9231=ORIENTED_EDGE('',*,*,#7041,.T.);
#9232=ORIENTED_EDGE('',*,*,#7042,.T.);
#9233=ORIENTED_EDGE('',*,*,#7038,.F.);
#9234=ORIENTED_EDGE('',*,*,#7043,.T.);
#9235=ORIENTED_EDGE('',*,*,#7044,.T.);
#9236=ORIENTED_EDGE('',*,*,#7045,.T.);
#9237=ORIENTED_EDGE('',*,*,#7041,.F.);
#9238=ORIENTED_EDGE('',*,*,#7046,.T.);
#9239=ORIENTED_EDGE('',*,*,#7047,.T.);
#9240=ORIENTED_EDGE('',*,*,#7048,.T.);
#9241=ORIENTED_EDGE('',*,*,#7044,.F.);
#9242=ORIENTED_EDGE('',*,*,#7049,.T.);
#9243=ORIENTED_EDGE('',*,*,#7050,.T.);
#9244=ORIENTED_EDGE('',*,*,#7051,.T.);
#9245=ORIENTED_EDGE('',*,*,#7047,.F.);
#9246=ORIENTED_EDGE('',*,*,#7052,.T.);
#9247=ORIENTED_EDGE('',*,*,#7053,.T.);
#9248=ORIENTED_EDGE('',*,*,#7054,.T.);
#9249=ORIENTED_EDGE('',*,*,#7050,.F.);
#9250=ORIENTED_EDGE('',*,*,#7055,.T.);
#9251=ORIENTED_EDGE('',*,*,#7056,.F.);
#9252=ORIENTED_EDGE('',*,*,#7057,.T.);
#9253=ORIENTED_EDGE('',*,*,#7058,.F.);
#9254=ORIENTED_EDGE('',*,*,#7059,.T.);
#9255=ORIENTED_EDGE('',*,*,#7060,.T.);
#9256=ORIENTED_EDGE('',*,*,#7061,.T.);
#9257=ORIENTED_EDGE('',*,*,#7062,.F.);
#9258=ORIENTED_EDGE('',*,*,#7063,.T.);
#9259=ORIENTED_EDGE('',*,*,#7064,.T.);
#9260=ORIENTED_EDGE('',*,*,#7065,.T.);
#9261=ORIENTED_EDGE('',*,*,#7060,.F.);
#9262=ORIENTED_EDGE('',*,*,#7066,.T.);
#9263=ORIENTED_EDGE('',*,*,#7067,.T.);
#9264=ORIENTED_EDGE('',*,*,#7068,.T.);
#9265=ORIENTED_EDGE('',*,*,#7064,.F.);
#9266=ORIENTED_EDGE('',*,*,#7069,.T.);
#9267=ORIENTED_EDGE('',*,*,#7070,.T.);
#9268=ORIENTED_EDGE('',*,*,#7071,.T.);
#9269=ORIENTED_EDGE('',*,*,#7067,.F.);
#9270=ORIENTED_EDGE('',*,*,#7072,.T.);
#9271=ORIENTED_EDGE('',*,*,#7073,.T.);
#9272=ORIENTED_EDGE('',*,*,#7074,.T.);
#9273=ORIENTED_EDGE('',*,*,#7070,.F.);
#9274=ORIENTED_EDGE('',*,*,#7075,.T.);
#9275=ORIENTED_EDGE('',*,*,#7076,.T.);
#9276=ORIENTED_EDGE('',*,*,#7077,.T.);
#9277=ORIENTED_EDGE('',*,*,#7073,.F.);
#9278=ORIENTED_EDGE('',*,*,#7078,.T.);
#9279=ORIENTED_EDGE('',*,*,#7079,.T.);
#9280=ORIENTED_EDGE('',*,*,#7080,.T.);
#9281=ORIENTED_EDGE('',*,*,#7076,.F.);
#9282=ORIENTED_EDGE('',*,*,#7081,.T.);
#9283=ORIENTED_EDGE('',*,*,#7082,.F.);
#9284=ORIENTED_EDGE('',*,*,#7083,.T.);
#9285=ORIENTED_EDGE('',*,*,#7084,.F.);
#9286=ORIENTED_EDGE('',*,*,#7085,.T.);
#9287=ORIENTED_EDGE('',*,*,#7086,.T.);
#9288=ORIENTED_EDGE('',*,*,#7087,.T.);
#9289=ORIENTED_EDGE('',*,*,#7088,.F.);
#9290=ORIENTED_EDGE('',*,*,#7089,.T.);
#9291=ORIENTED_EDGE('',*,*,#7090,.T.);
#9292=ORIENTED_EDGE('',*,*,#7091,.T.);
#9293=ORIENTED_EDGE('',*,*,#7086,.F.);
#9294=ORIENTED_EDGE('',*,*,#7092,.T.);
#9295=ORIENTED_EDGE('',*,*,#7093,.T.);
#9296=ORIENTED_EDGE('',*,*,#7094,.T.);
#9297=ORIENTED_EDGE('',*,*,#7090,.F.);
#9298=ORIENTED_EDGE('',*,*,#7095,.T.);
#9299=ORIENTED_EDGE('',*,*,#7096,.T.);
#9300=ORIENTED_EDGE('',*,*,#7097,.T.);
#9301=ORIENTED_EDGE('',*,*,#7093,.F.);
#9302=ORIENTED_EDGE('',*,*,#7098,.T.);
#9303=ORIENTED_EDGE('',*,*,#7099,.T.);
#9304=ORIENTED_EDGE('',*,*,#7100,.T.);
#9305=ORIENTED_EDGE('',*,*,#7096,.F.);
#9306=ORIENTED_EDGE('',*,*,#7101,.T.);
#9307=ORIENTED_EDGE('',*,*,#7102,.T.);
#9308=ORIENTED_EDGE('',*,*,#7103,.T.);
#9309=ORIENTED_EDGE('',*,*,#7099,.F.);
#9310=ORIENTED_EDGE('',*,*,#7104,.T.);
#9311=ORIENTED_EDGE('',*,*,#7105,.T.);
#9312=ORIENTED_EDGE('',*,*,#7106,.T.);
#9313=ORIENTED_EDGE('',*,*,#7102,.F.);
#9314=ORIENTED_EDGE('',*,*,#7107,.T.);
#9315=ORIENTED_EDGE('',*,*,#7108,.F.);
#9316=ORIENTED_EDGE('',*,*,#7109,.T.);
#9317=ORIENTED_EDGE('',*,*,#7110,.F.);
#9318=ORIENTED_EDGE('',*,*,#7111,.T.);
#9319=ORIENTED_EDGE('',*,*,#7112,.T.);
#9320=ORIENTED_EDGE('',*,*,#7113,.T.);
#9321=ORIENTED_EDGE('',*,*,#7114,.F.);
#9322=ORIENTED_EDGE('',*,*,#7115,.T.);
#9323=ORIENTED_EDGE('',*,*,#7116,.T.);
#9324=ORIENTED_EDGE('',*,*,#7117,.T.);
#9325=ORIENTED_EDGE('',*,*,#7112,.F.);
#9326=ORIENTED_EDGE('',*,*,#7118,.T.);
#9327=ORIENTED_EDGE('',*,*,#7119,.T.);
#9328=ORIENTED_EDGE('',*,*,#7120,.T.);
#9329=ORIENTED_EDGE('',*,*,#7116,.F.);
#9330=ORIENTED_EDGE('',*,*,#7121,.T.);
#9331=ORIENTED_EDGE('',*,*,#7122,.T.);
#9332=ORIENTED_EDGE('',*,*,#7123,.T.);
#9333=ORIENTED_EDGE('',*,*,#7119,.F.);
#9334=ORIENTED_EDGE('',*,*,#7124,.T.);
#9335=ORIENTED_EDGE('',*,*,#7125,.T.);
#9336=ORIENTED_EDGE('',*,*,#7126,.T.);
#9337=ORIENTED_EDGE('',*,*,#7122,.F.);
#9338=ORIENTED_EDGE('',*,*,#7127,.T.);
#9339=ORIENTED_EDGE('',*,*,#7128,.T.);
#9340=ORIENTED_EDGE('',*,*,#7129,.T.);
#9341=ORIENTED_EDGE('',*,*,#7125,.F.);
#9342=ORIENTED_EDGE('',*,*,#7130,.T.);
#9343=ORIENTED_EDGE('',*,*,#7131,.T.);
#9344=ORIENTED_EDGE('',*,*,#7132,.T.);
#9345=ORIENTED_EDGE('',*,*,#7128,.F.);
#9346=ORIENTED_EDGE('',*,*,#7133,.T.);
#9347=ORIENTED_EDGE('',*,*,#7134,.F.);
#9348=ORIENTED_EDGE('',*,*,#7135,.T.);
#9349=ORIENTED_EDGE('',*,*,#7136,.F.);
#9350=ORIENTED_EDGE('',*,*,#7137,.T.);
#9351=ORIENTED_EDGE('',*,*,#7138,.T.);
#9352=ORIENTED_EDGE('',*,*,#7139,.T.);
#9353=ORIENTED_EDGE('',*,*,#7140,.F.);
#9354=ORIENTED_EDGE('',*,*,#7141,.F.);
#9355=ORIENTED_EDGE('',*,*,#7142,.T.);
#9356=ORIENTED_EDGE('',*,*,#7143,.T.);
#9357=ORIENTED_EDGE('',*,*,#7138,.F.);
#9358=ORIENTED_EDGE('',*,*,#7144,.F.);
#9359=ORIENTED_EDGE('',*,*,#7145,.T.);
#9360=ORIENTED_EDGE('',*,*,#7146,.T.);
#9361=ORIENTED_EDGE('',*,*,#7142,.F.);
#9362=ORIENTED_EDGE('',*,*,#7147,.F.);
#9363=ORIENTED_EDGE('',*,*,#7148,.T.);
#9364=ORIENTED_EDGE('',*,*,#7149,.T.);
#9365=ORIENTED_EDGE('',*,*,#7145,.F.);
#9366=ORIENTED_EDGE('',*,*,#7150,.F.);
#9367=ORIENTED_EDGE('',*,*,#7151,.T.);
#9368=ORIENTED_EDGE('',*,*,#7152,.T.);
#9369=ORIENTED_EDGE('',*,*,#7148,.F.);
#9370=ORIENTED_EDGE('',*,*,#7153,.F.);
#9371=ORIENTED_EDGE('',*,*,#7154,.T.);
#9372=ORIENTED_EDGE('',*,*,#7155,.T.);
#9373=ORIENTED_EDGE('',*,*,#7151,.F.);
#9374=ORIENTED_EDGE('',*,*,#7156,.F.);
#9375=ORIENTED_EDGE('',*,*,#7157,.T.);
#9376=ORIENTED_EDGE('',*,*,#7158,.T.);
#9377=ORIENTED_EDGE('',*,*,#7154,.F.);
#9378=ORIENTED_EDGE('',*,*,#7159,.F.);
#9379=ORIENTED_EDGE('',*,*,#7160,.F.);
#9380=ORIENTED_EDGE('',*,*,#7161,.F.);
#9381=ORIENTED_EDGE('',*,*,#7162,.F.);
#9382=ORIENTED_EDGE('',*,*,#7163,.T.);
#9383=ORIENTED_EDGE('',*,*,#7164,.T.);
#9384=ORIENTED_EDGE('',*,*,#7165,.T.);
#9385=ORIENTED_EDGE('',*,*,#7166,.F.);
#9386=ORIENTED_EDGE('',*,*,#7167,.F.);
#9387=ORIENTED_EDGE('',*,*,#7168,.T.);
#9388=ORIENTED_EDGE('',*,*,#7169,.T.);
#9389=ORIENTED_EDGE('',*,*,#7164,.F.);
#9390=ORIENTED_EDGE('',*,*,#7170,.F.);
#9391=ORIENTED_EDGE('',*,*,#7171,.T.);
#9392=ORIENTED_EDGE('',*,*,#7172,.T.);
#9393=ORIENTED_EDGE('',*,*,#7168,.F.);
#9394=ORIENTED_EDGE('',*,*,#7173,.F.);
#9395=ORIENTED_EDGE('',*,*,#7174,.T.);
#9396=ORIENTED_EDGE('',*,*,#7175,.T.);
#9397=ORIENTED_EDGE('',*,*,#7171,.F.);
#9398=ORIENTED_EDGE('',*,*,#7176,.F.);
#9399=ORIENTED_EDGE('',*,*,#7177,.T.);
#9400=ORIENTED_EDGE('',*,*,#7178,.T.);
#9401=ORIENTED_EDGE('',*,*,#7174,.F.);
#9402=ORIENTED_EDGE('',*,*,#7179,.F.);
#9403=ORIENTED_EDGE('',*,*,#7180,.T.);
#9404=ORIENTED_EDGE('',*,*,#7181,.T.);
#9405=ORIENTED_EDGE('',*,*,#7177,.F.);
#9406=ORIENTED_EDGE('',*,*,#7182,.F.);
#9407=ORIENTED_EDGE('',*,*,#7183,.T.);
#9408=ORIENTED_EDGE('',*,*,#7184,.T.);
#9409=ORIENTED_EDGE('',*,*,#7180,.F.);
#9410=ORIENTED_EDGE('',*,*,#7185,.F.);
#9411=ORIENTED_EDGE('',*,*,#7186,.F.);
#9412=ORIENTED_EDGE('',*,*,#7187,.F.);
#9413=ORIENTED_EDGE('',*,*,#7188,.F.);
#9414=ORIENTED_EDGE('',*,*,#7189,.T.);
#9415=ORIENTED_EDGE('',*,*,#7190,.T.);
#9416=ORIENTED_EDGE('',*,*,#7191,.T.);
#9417=ORIENTED_EDGE('',*,*,#7192,.F.);
#9418=ORIENTED_EDGE('',*,*,#7193,.F.);
#9419=ORIENTED_EDGE('',*,*,#7194,.T.);
#9420=ORIENTED_EDGE('',*,*,#7195,.T.);
#9421=ORIENTED_EDGE('',*,*,#7190,.F.);
#9422=ORIENTED_EDGE('',*,*,#7196,.F.);
#9423=ORIENTED_EDGE('',*,*,#7197,.T.);
#9424=ORIENTED_EDGE('',*,*,#7198,.T.);
#9425=ORIENTED_EDGE('',*,*,#7194,.F.);
#9426=ORIENTED_EDGE('',*,*,#7199,.F.);
#9427=ORIENTED_EDGE('',*,*,#7200,.T.);
#9428=ORIENTED_EDGE('',*,*,#7201,.T.);
#9429=ORIENTED_EDGE('',*,*,#7197,.F.);
#9430=ORIENTED_EDGE('',*,*,#7202,.F.);
#9431=ORIENTED_EDGE('',*,*,#7203,.T.);
#9432=ORIENTED_EDGE('',*,*,#7204,.T.);
#9433=ORIENTED_EDGE('',*,*,#7200,.F.);
#9434=ORIENTED_EDGE('',*,*,#7205,.F.);
#9435=ORIENTED_EDGE('',*,*,#7206,.T.);
#9436=ORIENTED_EDGE('',*,*,#7207,.T.);
#9437=ORIENTED_EDGE('',*,*,#7203,.F.);
#9438=ORIENTED_EDGE('',*,*,#7208,.F.);
#9439=ORIENTED_EDGE('',*,*,#7209,.T.);
#9440=ORIENTED_EDGE('',*,*,#7210,.T.);
#9441=ORIENTED_EDGE('',*,*,#7206,.F.);
#9442=ORIENTED_EDGE('',*,*,#7211,.F.);
#9443=ORIENTED_EDGE('',*,*,#7212,.F.);
#9444=ORIENTED_EDGE('',*,*,#7213,.F.);
#9445=ORIENTED_EDGE('',*,*,#7214,.F.);
#9446=ORIENTED_EDGE('',*,*,#7215,.T.);
#9447=ORIENTED_EDGE('',*,*,#7216,.T.);
#9448=ORIENTED_EDGE('',*,*,#7217,.T.);
#9449=ORIENTED_EDGE('',*,*,#7218,.F.);
#9450=ORIENTED_EDGE('',*,*,#7219,.F.);
#9451=ORIENTED_EDGE('',*,*,#7220,.T.);
#9452=ORIENTED_EDGE('',*,*,#7221,.T.);
#9453=ORIENTED_EDGE('',*,*,#7216,.F.);
#9454=ORIENTED_EDGE('',*,*,#7222,.F.);
#9455=ORIENTED_EDGE('',*,*,#7223,.T.);
#9456=ORIENTED_EDGE('',*,*,#7224,.T.);
#9457=ORIENTED_EDGE('',*,*,#7220,.F.);
#9458=ORIENTED_EDGE('',*,*,#7225,.F.);
#9459=ORIENTED_EDGE('',*,*,#7226,.T.);
#9460=ORIENTED_EDGE('',*,*,#7227,.T.);
#9461=ORIENTED_EDGE('',*,*,#7223,.F.);
#9462=ORIENTED_EDGE('',*,*,#7228,.F.);
#9463=ORIENTED_EDGE('',*,*,#7229,.T.);
#9464=ORIENTED_EDGE('',*,*,#7230,.T.);
#9465=ORIENTED_EDGE('',*,*,#7226,.F.);
#9466=ORIENTED_EDGE('',*,*,#7231,.F.);
#9467=ORIENTED_EDGE('',*,*,#7232,.T.);
#9468=ORIENTED_EDGE('',*,*,#7233,.T.);
#9469=ORIENTED_EDGE('',*,*,#7229,.F.);
#9470=ORIENTED_EDGE('',*,*,#7234,.F.);
#9471=ORIENTED_EDGE('',*,*,#7235,.T.);
#9472=ORIENTED_EDGE('',*,*,#7236,.T.);
#9473=ORIENTED_EDGE('',*,*,#7232,.F.);
#9474=ORIENTED_EDGE('',*,*,#7237,.F.);
#9475=ORIENTED_EDGE('',*,*,#7238,.F.);
#9476=ORIENTED_EDGE('',*,*,#7239,.F.);
#9477=ORIENTED_EDGE('',*,*,#7240,.F.);
#9478=ORIENTED_EDGE('',*,*,#7241,.T.);
#9479=ORIENTED_EDGE('',*,*,#7238,.T.);
#9480=ORIENTED_EDGE('',*,*,#7242,.T.);
#9481=ORIENTED_EDGE('',*,*,#7235,.F.);
#9482=ORIENTED_EDGE('',*,*,#7243,.F.);
#9483=ORIENTED_EDGE('',*,*,#7244,.F.);
#9484=ORIENTED_EDGE('',*,*,#7217,.F.);
#9485=ORIENTED_EDGE('',*,*,#7221,.F.);
#9486=ORIENTED_EDGE('',*,*,#7224,.F.);
#9487=ORIENTED_EDGE('',*,*,#7227,.F.);
#9488=ORIENTED_EDGE('',*,*,#7230,.F.);
#9489=ORIENTED_EDGE('',*,*,#7233,.F.);
#9490=ORIENTED_EDGE('',*,*,#7236,.F.);
#9491=ORIENTED_EDGE('',*,*,#7242,.F.);
#9492=ORIENTED_EDGE('',*,*,#7241,.F.);
#9493=ORIENTED_EDGE('',*,*,#7245,.F.);
#9494=ORIENTED_EDGE('',*,*,#7135,.F.);
#9495=ORIENTED_EDGE('',*,*,#7246,.F.);
#9496=ORIENTED_EDGE('',*,*,#7133,.F.);
#9497=ORIENTED_EDGE('',*,*,#7130,.F.);
#9498=ORIENTED_EDGE('',*,*,#7127,.F.);
#9499=ORIENTED_EDGE('',*,*,#7124,.F.);
#9500=ORIENTED_EDGE('',*,*,#7121,.F.);
#9501=ORIENTED_EDGE('',*,*,#7118,.F.);
#9502=ORIENTED_EDGE('',*,*,#7115,.F.);
#9503=ORIENTED_EDGE('',*,*,#7247,.F.);
#9504=ORIENTED_EDGE('',*,*,#7113,.F.);
#9505=ORIENTED_EDGE('',*,*,#7117,.F.);
#9506=ORIENTED_EDGE('',*,*,#7120,.F.);
#9507=ORIENTED_EDGE('',*,*,#7123,.F.);
#9508=ORIENTED_EDGE('',*,*,#7126,.F.);
#9509=ORIENTED_EDGE('',*,*,#7129,.F.);
#9510=ORIENTED_EDGE('',*,*,#7132,.F.);
#9511=ORIENTED_EDGE('',*,*,#7248,.F.);
#9512=ORIENTED_EDGE('',*,*,#7137,.F.);
#9513=ORIENTED_EDGE('',*,*,#7249,.F.);
#9514=ORIENTED_EDGE('',*,*,#7239,.T.);
#9515=ORIENTED_EDGE('',*,*,#7243,.T.);
#9516=ORIENTED_EDGE('',*,*,#7237,.T.);
#9517=ORIENTED_EDGE('',*,*,#7234,.T.);
#9518=ORIENTED_EDGE('',*,*,#7231,.T.);
#9519=ORIENTED_EDGE('',*,*,#7228,.T.);
#9520=ORIENTED_EDGE('',*,*,#7225,.T.);
#9521=ORIENTED_EDGE('',*,*,#7222,.T.);
#9522=ORIENTED_EDGE('',*,*,#7219,.T.);
#9523=ORIENTED_EDGE('',*,*,#7250,.T.);
#9524=ORIENTED_EDGE('',*,*,#7251,.T.);
#9525=ORIENTED_EDGE('',*,*,#7252,.T.);
#9526=ORIENTED_EDGE('',*,*,#7253,.T.);
#9527=ORIENTED_EDGE('',*,*,#7245,.T.);
#9528=ORIENTED_EDGE('',*,*,#7240,.T.);
#9529=ORIENTED_EDGE('',*,*,#7249,.T.);
#9530=ORIENTED_EDGE('',*,*,#7136,.T.);
#9531=ORIENTED_EDGE('',*,*,#7254,.T.);
#9532=ORIENTED_EDGE('',*,*,#7214,.T.);
#9533=ORIENTED_EDGE('',*,*,#7255,.T.);
#9534=ORIENTED_EDGE('',*,*,#7110,.T.);
#9535=ORIENTED_EDGE('',*,*,#7256,.T.);
#9536=ORIENTED_EDGE('',*,*,#7162,.T.);
#9537=ORIENTED_EDGE('',*,*,#7257,.T.);
#9538=ORIENTED_EDGE('',*,*,#7084,.T.);
#9539=ORIENTED_EDGE('',*,*,#7258,.T.);
#9540=ORIENTED_EDGE('',*,*,#7188,.T.);
#9541=ORIENTED_EDGE('',*,*,#7259,.T.);
#9542=ORIENTED_EDGE('',*,*,#7058,.T.);
#9543=ORIENTED_EDGE('',*,*,#7212,.T.);
#9544=ORIENTED_EDGE('',*,*,#7260,.T.);
#9545=ORIENTED_EDGE('',*,*,#7209,.F.);
#9546=ORIENTED_EDGE('',*,*,#7261,.F.);
#9547=ORIENTED_EDGE('',*,*,#7262,.F.);
#9548=ORIENTED_EDGE('',*,*,#7191,.F.);
#9549=ORIENTED_EDGE('',*,*,#7195,.F.);
#9550=ORIENTED_EDGE('',*,*,#7198,.F.);
#9551=ORIENTED_EDGE('',*,*,#7201,.F.);
#9552=ORIENTED_EDGE('',*,*,#7204,.F.);
#9553=ORIENTED_EDGE('',*,*,#7207,.F.);
#9554=ORIENTED_EDGE('',*,*,#7210,.F.);
#9555=ORIENTED_EDGE('',*,*,#7260,.F.);
#9556=ORIENTED_EDGE('',*,*,#7215,.F.);
#9557=ORIENTED_EDGE('',*,*,#7254,.F.);
#9558=ORIENTED_EDGE('',*,*,#7109,.F.);
#9559=ORIENTED_EDGE('',*,*,#7263,.F.);
#9560=ORIENTED_EDGE('',*,*,#7107,.F.);
#9561=ORIENTED_EDGE('',*,*,#7104,.F.);
#9562=ORIENTED_EDGE('',*,*,#7101,.F.);
#9563=ORIENTED_EDGE('',*,*,#7098,.F.);
#9564=ORIENTED_EDGE('',*,*,#7095,.F.);
#9565=ORIENTED_EDGE('',*,*,#7092,.F.);
#9566=ORIENTED_EDGE('',*,*,#7089,.F.);
#9567=ORIENTED_EDGE('',*,*,#7264,.F.);
#9568=ORIENTED_EDGE('',*,*,#7087,.F.);
#9569=ORIENTED_EDGE('',*,*,#7091,.F.);
#9570=ORIENTED_EDGE('',*,*,#7094,.F.);
#9571=ORIENTED_EDGE('',*,*,#7097,.F.);
#9572=ORIENTED_EDGE('',*,*,#7100,.F.);
#9573=ORIENTED_EDGE('',*,*,#7103,.F.);
#9574=ORIENTED_EDGE('',*,*,#7106,.F.);
#9575=ORIENTED_EDGE('',*,*,#7265,.F.);
#9576=ORIENTED_EDGE('',*,*,#7111,.F.);
#9577=ORIENTED_EDGE('',*,*,#7255,.F.);
#9578=ORIENTED_EDGE('',*,*,#7213,.T.);
#9579=ORIENTED_EDGE('',*,*,#7261,.T.);
#9580=ORIENTED_EDGE('',*,*,#7211,.T.);
#9581=ORIENTED_EDGE('',*,*,#7208,.T.);
#9582=ORIENTED_EDGE('',*,*,#7205,.T.);
#9583=ORIENTED_EDGE('',*,*,#7202,.T.);
#9584=ORIENTED_EDGE('',*,*,#7199,.T.);
#9585=ORIENTED_EDGE('',*,*,#7196,.T.);
#9586=ORIENTED_EDGE('',*,*,#7193,.T.);
#9587=ORIENTED_EDGE('',*,*,#7186,.T.);
#9588=ORIENTED_EDGE('',*,*,#7266,.T.);
#9589=ORIENTED_EDGE('',*,*,#7183,.F.);
#9590=ORIENTED_EDGE('',*,*,#7267,.F.);
#9591=ORIENTED_EDGE('',*,*,#7268,.F.);
#9592=ORIENTED_EDGE('',*,*,#7165,.F.);
#9593=ORIENTED_EDGE('',*,*,#7169,.F.);
#9594=ORIENTED_EDGE('',*,*,#7172,.F.);
#9595=ORIENTED_EDGE('',*,*,#7175,.F.);
#9596=ORIENTED_EDGE('',*,*,#7178,.F.);
#9597=ORIENTED_EDGE('',*,*,#7181,.F.);
#9598=ORIENTED_EDGE('',*,*,#7184,.F.);
#9599=ORIENTED_EDGE('',*,*,#7266,.F.);
#9600=ORIENTED_EDGE('',*,*,#7189,.F.);
#9601=ORIENTED_EDGE('',*,*,#7258,.F.);
#9602=ORIENTED_EDGE('',*,*,#7057,.F.);
#9603=ORIENTED_EDGE('',*,*,#7269,.F.);
#9604=ORIENTED_EDGE('',*,*,#7055,.F.);
#9605=ORIENTED_EDGE('',*,*,#7052,.F.);
#9606=ORIENTED_EDGE('',*,*,#7049,.F.);
#9607=ORIENTED_EDGE('',*,*,#7046,.F.);
#9608=ORIENTED_EDGE('',*,*,#7043,.F.);
#9609=ORIENTED_EDGE('',*,*,#7040,.F.);
#9610=ORIENTED_EDGE('',*,*,#7037,.F.);
#9611=ORIENTED_EDGE('',*,*,#7270,.F.);
#9612=ORIENTED_EDGE('',*,*,#7035,.F.);
#9613=ORIENTED_EDGE('',*,*,#7039,.F.);
#9614=ORIENTED_EDGE('',*,*,#7042,.F.);
#9615=ORIENTED_EDGE('',*,*,#7045,.F.);
#9616=ORIENTED_EDGE('',*,*,#7048,.F.);
#9617=ORIENTED_EDGE('',*,*,#7051,.F.);
#9618=ORIENTED_EDGE('',*,*,#7054,.F.);
#9619=ORIENTED_EDGE('',*,*,#7271,.F.);
#9620=ORIENTED_EDGE('',*,*,#7059,.F.);
#9621=ORIENTED_EDGE('',*,*,#7259,.F.);
#9622=ORIENTED_EDGE('',*,*,#7187,.T.);
#9623=ORIENTED_EDGE('',*,*,#7267,.T.);
#9624=ORIENTED_EDGE('',*,*,#7185,.T.);
#9625=ORIENTED_EDGE('',*,*,#7182,.T.);
#9626=ORIENTED_EDGE('',*,*,#7179,.T.);
#9627=ORIENTED_EDGE('',*,*,#7176,.T.);
#9628=ORIENTED_EDGE('',*,*,#7173,.T.);
#9629=ORIENTED_EDGE('',*,*,#7170,.T.);
#9630=ORIENTED_EDGE('',*,*,#7167,.T.);
#9631=ORIENTED_EDGE('',*,*,#7160,.T.);
#9632=ORIENTED_EDGE('',*,*,#7272,.T.);
#9633=ORIENTED_EDGE('',*,*,#7157,.F.);
#9634=ORIENTED_EDGE('',*,*,#7273,.F.);
#9635=ORIENTED_EDGE('',*,*,#7274,.F.);
#9636=ORIENTED_EDGE('',*,*,#7139,.F.);
#9637=ORIENTED_EDGE('',*,*,#7143,.F.);
#9638=ORIENTED_EDGE('',*,*,#7146,.F.);
#9639=ORIENTED_EDGE('',*,*,#7149,.F.);
#9640=ORIENTED_EDGE('',*,*,#7152,.F.);
#9641=ORIENTED_EDGE('',*,*,#7155,.F.);
#9642=ORIENTED_EDGE('',*,*,#7158,.F.);
#9643=ORIENTED_EDGE('',*,*,#7272,.F.);
#9644=ORIENTED_EDGE('',*,*,#7163,.F.);
#9645=ORIENTED_EDGE('',*,*,#7256,.F.);
#9646=ORIENTED_EDGE('',*,*,#7083,.F.);
#9647=ORIENTED_EDGE('',*,*,#7275,.F.);
#9648=ORIENTED_EDGE('',*,*,#7081,.F.);
#9649=ORIENTED_EDGE('',*,*,#7078,.F.);
#9650=ORIENTED_EDGE('',*,*,#7075,.F.);
#9651=ORIENTED_EDGE('',*,*,#7072,.F.);
#9652=ORIENTED_EDGE('',*,*,#7069,.F.);
#9653=ORIENTED_EDGE('',*,*,#7066,.F.);
#9654=ORIENTED_EDGE('',*,*,#7063,.F.);
#9655=ORIENTED_EDGE('',*,*,#7276,.F.);
#9656=ORIENTED_EDGE('',*,*,#7061,.F.);
#9657=ORIENTED_EDGE('',*,*,#7065,.F.);
#9658=ORIENTED_EDGE('',*,*,#7068,.F.);
#9659=ORIENTED_EDGE('',*,*,#7071,.F.);
#9660=ORIENTED_EDGE('',*,*,#7074,.F.);
#9661=ORIENTED_EDGE('',*,*,#7077,.F.);
#9662=ORIENTED_EDGE('',*,*,#7080,.F.);
#9663=ORIENTED_EDGE('',*,*,#7277,.F.);
#9664=ORIENTED_EDGE('',*,*,#7085,.F.);
#9665=ORIENTED_EDGE('',*,*,#7257,.F.);
#9666=ORIENTED_EDGE('',*,*,#7161,.T.);
#9667=ORIENTED_EDGE('',*,*,#7273,.T.);
#9668=ORIENTED_EDGE('',*,*,#7159,.T.);
#9669=ORIENTED_EDGE('',*,*,#7156,.T.);
#9670=ORIENTED_EDGE('',*,*,#7153,.T.);
#9671=ORIENTED_EDGE('',*,*,#7150,.T.);
#9672=ORIENTED_EDGE('',*,*,#7147,.T.);
#9673=ORIENTED_EDGE('',*,*,#7144,.T.);
#9674=ORIENTED_EDGE('',*,*,#7141,.T.);
#9675=ORIENTED_EDGE('',*,*,#7134,.T.);
#9676=ORIENTED_EDGE('',*,*,#7248,.T.);
#9677=ORIENTED_EDGE('',*,*,#7131,.F.);
#9678=ORIENTED_EDGE('',*,*,#7246,.T.);
#9679=ORIENTED_EDGE('',*,*,#7108,.T.);
#9680=ORIENTED_EDGE('',*,*,#7265,.T.);
#9681=ORIENTED_EDGE('',*,*,#7105,.F.);
#9682=ORIENTED_EDGE('',*,*,#7263,.T.);
#9683=ORIENTED_EDGE('',*,*,#7082,.T.);
#9684=ORIENTED_EDGE('',*,*,#7277,.T.);
#9685=ORIENTED_EDGE('',*,*,#7079,.F.);
#9686=ORIENTED_EDGE('',*,*,#7275,.T.);
#9687=ORIENTED_EDGE('',*,*,#7056,.T.);
#9688=ORIENTED_EDGE('',*,*,#7271,.T.);
#9689=ORIENTED_EDGE('',*,*,#7053,.F.);
#9690=ORIENTED_EDGE('',*,*,#7269,.T.);
#9691=ORIENTED_EDGE('',*,*,#7278,.T.);
#9692=ORIENTED_EDGE('',*,*,#7279,.T.);
#9693=ORIENTED_EDGE('',*,*,#7253,.F.);
#9694=ORIENTED_EDGE('',*,*,#7280,.F.);
#9695=ORIENTED_EDGE('',*,*,#7281,.T.);
#9696=ORIENTED_EDGE('',*,*,#7280,.T.);
#9697=ORIENTED_EDGE('',*,*,#7252,.F.);
#9698=ORIENTED_EDGE('',*,*,#7282,.F.);
#9699=ORIENTED_EDGE('',*,*,#7283,.T.);
#9700=ORIENTED_EDGE('',*,*,#7282,.T.);
#9701=ORIENTED_EDGE('',*,*,#7251,.F.);
#9702=ORIENTED_EDGE('',*,*,#7284,.F.);
#9703=ORIENTED_EDGE('',*,*,#7285,.T.);
#9704=ORIENTED_EDGE('',*,*,#7284,.T.);
#9705=ORIENTED_EDGE('',*,*,#7250,.F.);
#9706=ORIENTED_EDGE('',*,*,#7279,.F.);
#9707=ORIENTED_EDGE('',*,*,#7285,.F.);
#9708=ORIENTED_EDGE('',*,*,#7278,.F.);
#9709=ORIENTED_EDGE('',*,*,#7281,.F.);
#9710=ORIENTED_EDGE('',*,*,#7283,.F.);
#9711=ORIENTED_EDGE('',*,*,#7244,.T.);
#9712=ORIENTED_EDGE('',*,*,#7114,.T.);
#9713=ORIENTED_EDGE('',*,*,#7247,.T.);
#9714=ORIENTED_EDGE('',*,*,#7218,.T.);
#9715=ORIENTED_EDGE('',*,*,#7262,.T.);
#9716=ORIENTED_EDGE('',*,*,#7088,.T.);
#9717=ORIENTED_EDGE('',*,*,#7264,.T.);
#9718=ORIENTED_EDGE('',*,*,#7192,.T.);
#9719=ORIENTED_EDGE('',*,*,#7268,.T.);
#9720=ORIENTED_EDGE('',*,*,#7036,.T.);
#9721=ORIENTED_EDGE('',*,*,#7270,.T.);
#9722=ORIENTED_EDGE('',*,*,#7166,.T.);
#9723=ORIENTED_EDGE('',*,*,#7274,.T.);
#9724=ORIENTED_EDGE('',*,*,#7062,.T.);
#9725=ORIENTED_EDGE('',*,*,#7276,.T.);
#9726=ORIENTED_EDGE('',*,*,#7140,.T.);
#9727=ORIENTED_EDGE('',*,*,#7286,.F.);
#9728=ORIENTED_EDGE('',*,*,#7287,.T.);
#9729=ORIENTED_EDGE('',*,*,#7288,.T.);
#9730=ORIENTED_EDGE('',*,*,#7289,.T.);
#9731=ORIENTED_EDGE('',*,*,#7290,.F.);
#9732=ORIENTED_EDGE('',*,*,#7291,.T.);
#9733=ORIENTED_EDGE('',*,*,#7286,.T.);
#9734=ORIENTED_EDGE('',*,*,#7292,.T.);
#9735=ORIENTED_EDGE('',*,*,#7293,.F.);
#9736=ORIENTED_EDGE('',*,*,#7294,.T.);
#9737=ORIENTED_EDGE('',*,*,#7290,.T.);
#9738=ORIENTED_EDGE('',*,*,#7295,.T.);
#9739=ORIENTED_EDGE('',*,*,#7296,.F.);
#9740=ORIENTED_EDGE('',*,*,#7297,.T.);
#9741=ORIENTED_EDGE('',*,*,#7293,.T.);
#9742=ORIENTED_EDGE('',*,*,#7298,.T.);
#9743=ORIENTED_EDGE('',*,*,#7299,.F.);
#9744=ORIENTED_EDGE('',*,*,#7300,.T.);
#9745=ORIENTED_EDGE('',*,*,#7296,.T.);
#9746=ORIENTED_EDGE('',*,*,#7301,.T.);
#9747=ORIENTED_EDGE('',*,*,#7302,.F.);
#9748=ORIENTED_EDGE('',*,*,#7303,.T.);
#9749=ORIENTED_EDGE('',*,*,#7299,.T.);
#9750=ORIENTED_EDGE('',*,*,#7304,.T.);
#9751=ORIENTED_EDGE('',*,*,#7305,.F.);
#9752=ORIENTED_EDGE('',*,*,#7306,.T.);
#9753=ORIENTED_EDGE('',*,*,#7302,.T.);
#9754=ORIENTED_EDGE('',*,*,#7307,.T.);
#9755=ORIENTED_EDGE('',*,*,#7308,.F.);
#9756=ORIENTED_EDGE('',*,*,#7309,.T.);
#9757=ORIENTED_EDGE('',*,*,#7305,.T.);
#9758=ORIENTED_EDGE('',*,*,#7310,.T.);
#9759=ORIENTED_EDGE('',*,*,#7311,.F.);
#9760=ORIENTED_EDGE('',*,*,#7312,.T.);
#9761=ORIENTED_EDGE('',*,*,#7308,.T.);
#9762=ORIENTED_EDGE('',*,*,#7313,.T.);
#9763=ORIENTED_EDGE('',*,*,#7314,.F.);
#9764=ORIENTED_EDGE('',*,*,#7315,.T.);
#9765=ORIENTED_EDGE('',*,*,#7311,.T.);
#9766=ORIENTED_EDGE('',*,*,#7316,.T.);
#9767=ORIENTED_EDGE('',*,*,#7317,.F.);
#9768=ORIENTED_EDGE('',*,*,#7318,.T.);
#9769=ORIENTED_EDGE('',*,*,#7314,.T.);
#9770=ORIENTED_EDGE('',*,*,#7319,.T.);
#9771=ORIENTED_EDGE('',*,*,#7320,.F.);
#9772=ORIENTED_EDGE('',*,*,#7321,.T.);
#9773=ORIENTED_EDGE('',*,*,#7317,.T.);
#9774=ORIENTED_EDGE('',*,*,#7322,.T.);
#9775=ORIENTED_EDGE('',*,*,#7323,.F.);
#9776=ORIENTED_EDGE('',*,*,#7324,.T.);
#9777=ORIENTED_EDGE('',*,*,#7320,.T.);
#9778=ORIENTED_EDGE('',*,*,#7325,.T.);
#9779=ORIENTED_EDGE('',*,*,#7326,.F.);
#9780=ORIENTED_EDGE('',*,*,#7327,.T.);
#9781=ORIENTED_EDGE('',*,*,#7323,.T.);
#9782=ORIENTED_EDGE('',*,*,#7328,.T.);
#9783=ORIENTED_EDGE('',*,*,#7329,.F.);
#9784=ORIENTED_EDGE('',*,*,#7330,.T.);
#9785=ORIENTED_EDGE('',*,*,#7326,.T.);
#9786=ORIENTED_EDGE('',*,*,#7331,.T.);
#9787=ORIENTED_EDGE('',*,*,#7332,.F.);
#9788=ORIENTED_EDGE('',*,*,#7333,.T.);
#9789=ORIENTED_EDGE('',*,*,#7329,.T.);
#9790=ORIENTED_EDGE('',*,*,#7334,.T.);
#9791=ORIENTED_EDGE('',*,*,#7335,.F.);
#9792=ORIENTED_EDGE('',*,*,#7336,.T.);
#9793=ORIENTED_EDGE('',*,*,#7332,.T.);
#9794=ORIENTED_EDGE('',*,*,#7337,.T.);
#9795=ORIENTED_EDGE('',*,*,#7338,.F.);
#9796=ORIENTED_EDGE('',*,*,#7339,.T.);
#9797=ORIENTED_EDGE('',*,*,#7335,.T.);
#9798=ORIENTED_EDGE('',*,*,#7340,.T.);
#9799=ORIENTED_EDGE('',*,*,#7341,.F.);
#9800=ORIENTED_EDGE('',*,*,#7342,.T.);
#9801=ORIENTED_EDGE('',*,*,#7338,.T.);
#9802=ORIENTED_EDGE('',*,*,#7343,.T.);
#9803=ORIENTED_EDGE('',*,*,#7344,.F.);
#9804=ORIENTED_EDGE('',*,*,#7345,.T.);
#9805=ORIENTED_EDGE('',*,*,#7341,.T.);
#9806=ORIENTED_EDGE('',*,*,#7346,.T.);
#9807=ORIENTED_EDGE('',*,*,#7347,.F.);
#9808=ORIENTED_EDGE('',*,*,#7348,.T.);
#9809=ORIENTED_EDGE('',*,*,#7344,.T.);
#9810=ORIENTED_EDGE('',*,*,#7349,.T.);
#9811=ORIENTED_EDGE('',*,*,#7350,.F.);
#9812=ORIENTED_EDGE('',*,*,#7351,.T.);
#9813=ORIENTED_EDGE('',*,*,#7347,.T.);
#9814=ORIENTED_EDGE('',*,*,#7352,.T.);
#9815=ORIENTED_EDGE('',*,*,#7353,.F.);
#9816=ORIENTED_EDGE('',*,*,#7354,.T.);
#9817=ORIENTED_EDGE('',*,*,#7350,.T.);
#9818=ORIENTED_EDGE('',*,*,#7355,.T.);
#9819=ORIENTED_EDGE('',*,*,#7356,.F.);
#9820=ORIENTED_EDGE('',*,*,#7357,.T.);
#9821=ORIENTED_EDGE('',*,*,#7353,.T.);
#9822=ORIENTED_EDGE('',*,*,#7358,.T.);
#9823=ORIENTED_EDGE('',*,*,#7359,.F.);
#9824=ORIENTED_EDGE('',*,*,#7360,.T.);
#9825=ORIENTED_EDGE('',*,*,#7361,.T.);
#9826=ORIENTED_EDGE('',*,*,#7362,.F.);
#9827=ORIENTED_EDGE('',*,*,#7363,.F.);
#9828=ORIENTED_EDGE('',*,*,#7364,.T.);
#9829=ORIENTED_EDGE('',*,*,#7359,.T.);
#9830=ORIENTED_EDGE('',*,*,#7365,.F.);
#9831=ORIENTED_EDGE('',*,*,#7366,.F.);
#9832=ORIENTED_EDGE('',*,*,#7367,.T.);
#9833=ORIENTED_EDGE('',*,*,#7363,.T.);
#9834=ORIENTED_EDGE('',*,*,#7368,.F.);
#9835=ORIENTED_EDGE('',*,*,#7369,.F.);
#9836=ORIENTED_EDGE('',*,*,#7370,.T.);
#9837=ORIENTED_EDGE('',*,*,#7366,.T.);
#9838=ORIENTED_EDGE('',*,*,#7371,.F.);
#9839=ORIENTED_EDGE('',*,*,#7372,.F.);
#9840=ORIENTED_EDGE('',*,*,#7373,.T.);
#9841=ORIENTED_EDGE('',*,*,#7369,.T.);
#9842=ORIENTED_EDGE('',*,*,#7374,.F.);
#9843=ORIENTED_EDGE('',*,*,#7375,.F.);
#9844=ORIENTED_EDGE('',*,*,#7376,.T.);
#9845=ORIENTED_EDGE('',*,*,#7372,.T.);
#9846=ORIENTED_EDGE('',*,*,#7377,.F.);
#9847=ORIENTED_EDGE('',*,*,#7378,.F.);
#9848=ORIENTED_EDGE('',*,*,#7379,.T.);
#9849=ORIENTED_EDGE('',*,*,#7375,.T.);
#9850=ORIENTED_EDGE('',*,*,#7380,.F.);
#9851=ORIENTED_EDGE('',*,*,#7381,.F.);
#9852=ORIENTED_EDGE('',*,*,#7382,.T.);
#9853=ORIENTED_EDGE('',*,*,#7378,.T.);
#9854=ORIENTED_EDGE('',*,*,#7383,.F.);
#9855=ORIENTED_EDGE('',*,*,#7384,.F.);
#9856=ORIENTED_EDGE('',*,*,#7385,.T.);
#9857=ORIENTED_EDGE('',*,*,#7381,.T.);
#9858=ORIENTED_EDGE('',*,*,#7386,.F.);
#9859=ORIENTED_EDGE('',*,*,#7387,.F.);
#9860=ORIENTED_EDGE('',*,*,#7388,.T.);
#9861=ORIENTED_EDGE('',*,*,#7384,.T.);
#9862=ORIENTED_EDGE('',*,*,#7389,.F.);
#9863=ORIENTED_EDGE('',*,*,#7390,.F.);
#9864=ORIENTED_EDGE('',*,*,#7391,.T.);
#9865=ORIENTED_EDGE('',*,*,#7387,.T.);
#9866=ORIENTED_EDGE('',*,*,#7392,.F.);
#9867=ORIENTED_EDGE('',*,*,#7393,.F.);
#9868=ORIENTED_EDGE('',*,*,#7394,.T.);
#9869=ORIENTED_EDGE('',*,*,#7390,.T.);
#9870=ORIENTED_EDGE('',*,*,#7395,.F.);
#9871=ORIENTED_EDGE('',*,*,#7396,.F.);
#9872=ORIENTED_EDGE('',*,*,#7397,.T.);
#9873=ORIENTED_EDGE('',*,*,#7393,.T.);
#9874=ORIENTED_EDGE('',*,*,#7398,.F.);
#9875=ORIENTED_EDGE('',*,*,#7399,.F.);
#9876=ORIENTED_EDGE('',*,*,#7400,.T.);
#9877=ORIENTED_EDGE('',*,*,#7396,.T.);
#9878=ORIENTED_EDGE('',*,*,#7401,.F.);
#9879=ORIENTED_EDGE('',*,*,#7402,.F.);
#9880=ORIENTED_EDGE('',*,*,#7403,.T.);
#9881=ORIENTED_EDGE('',*,*,#7399,.T.);
#9882=ORIENTED_EDGE('',*,*,#7404,.F.);
#9883=ORIENTED_EDGE('',*,*,#7405,.F.);
#9884=ORIENTED_EDGE('',*,*,#7406,.T.);
#9885=ORIENTED_EDGE('',*,*,#7402,.T.);
#9886=ORIENTED_EDGE('',*,*,#7407,.F.);
#9887=ORIENTED_EDGE('',*,*,#7408,.F.);
#9888=ORIENTED_EDGE('',*,*,#7409,.T.);
#9889=ORIENTED_EDGE('',*,*,#7405,.T.);
#9890=ORIENTED_EDGE('',*,*,#7410,.F.);
#9891=ORIENTED_EDGE('',*,*,#7411,.F.);
#9892=ORIENTED_EDGE('',*,*,#7412,.T.);
#9893=ORIENTED_EDGE('',*,*,#7408,.T.);
#9894=ORIENTED_EDGE('',*,*,#7413,.F.);
#9895=ORIENTED_EDGE('',*,*,#7414,.F.);
#9896=ORIENTED_EDGE('',*,*,#7415,.T.);
#9897=ORIENTED_EDGE('',*,*,#7411,.T.);
#9898=ORIENTED_EDGE('',*,*,#7416,.F.);
#9899=ORIENTED_EDGE('',*,*,#7417,.F.);
#9900=ORIENTED_EDGE('',*,*,#7418,.T.);
#9901=ORIENTED_EDGE('',*,*,#7414,.T.);
#9902=ORIENTED_EDGE('',*,*,#7419,.F.);
#9903=ORIENTED_EDGE('',*,*,#7420,.F.);
#9904=ORIENTED_EDGE('',*,*,#7421,.T.);
#9905=ORIENTED_EDGE('',*,*,#7417,.T.);
#9906=ORIENTED_EDGE('',*,*,#7422,.F.);
#9907=ORIENTED_EDGE('',*,*,#7423,.F.);
#9908=ORIENTED_EDGE('',*,*,#7424,.T.);
#9909=ORIENTED_EDGE('',*,*,#7420,.T.);
#9910=ORIENTED_EDGE('',*,*,#7425,.F.);
#9911=ORIENTED_EDGE('',*,*,#7426,.F.);
#9912=ORIENTED_EDGE('',*,*,#7427,.T.);
#9913=ORIENTED_EDGE('',*,*,#7423,.T.);
#9914=ORIENTED_EDGE('',*,*,#7428,.F.);
#9915=ORIENTED_EDGE('',*,*,#7429,.F.);
#9916=ORIENTED_EDGE('',*,*,#7430,.T.);
#9917=ORIENTED_EDGE('',*,*,#7426,.T.);
#9918=ORIENTED_EDGE('',*,*,#7431,.F.);
#9919=ORIENTED_EDGE('',*,*,#7432,.F.);
#9920=ORIENTED_EDGE('',*,*,#7361,.F.);
#9921=ORIENTED_EDGE('',*,*,#7433,.F.);
#9922=ORIENTED_EDGE('',*,*,#7434,.F.);
#9923=ORIENTED_EDGE('',*,*,#7435,.F.);
#9924=ORIENTED_EDGE('',*,*,#7436,.T.);
#9925=ORIENTED_EDGE('',*,*,#7437,.F.);
#9926=ORIENTED_EDGE('',*,*,#7436,.F.);
#9927=ORIENTED_EDGE('',*,*,#7433,.T.);
#9928=ORIENTED_EDGE('',*,*,#7360,.F.);
#9929=ORIENTED_EDGE('',*,*,#7364,.F.);
#9930=ORIENTED_EDGE('',*,*,#7367,.F.);
#9931=ORIENTED_EDGE('',*,*,#7370,.F.);
#9932=ORIENTED_EDGE('',*,*,#7373,.F.);
#9933=ORIENTED_EDGE('',*,*,#7376,.F.);
#9934=ORIENTED_EDGE('',*,*,#7379,.F.);
#9935=ORIENTED_EDGE('',*,*,#7382,.F.);
#9936=ORIENTED_EDGE('',*,*,#7385,.F.);
#9937=ORIENTED_EDGE('',*,*,#7388,.F.);
#9938=ORIENTED_EDGE('',*,*,#7391,.F.);
#9939=ORIENTED_EDGE('',*,*,#7394,.F.);
#9940=ORIENTED_EDGE('',*,*,#7397,.F.);
#9941=ORIENTED_EDGE('',*,*,#7400,.F.);
#9942=ORIENTED_EDGE('',*,*,#7403,.F.);
#9943=ORIENTED_EDGE('',*,*,#7406,.F.);
#9944=ORIENTED_EDGE('',*,*,#7409,.F.);
#9945=ORIENTED_EDGE('',*,*,#7412,.F.);
#9946=ORIENTED_EDGE('',*,*,#7415,.F.);
#9947=ORIENTED_EDGE('',*,*,#7418,.F.);
#9948=ORIENTED_EDGE('',*,*,#7421,.F.);
#9949=ORIENTED_EDGE('',*,*,#7424,.F.);
#9950=ORIENTED_EDGE('',*,*,#7427,.F.);
#9951=ORIENTED_EDGE('',*,*,#7430,.F.);
#9952=ORIENTED_EDGE('',*,*,#7438,.F.);
#9953=ORIENTED_EDGE('',*,*,#7439,.F.);
#9954=ORIENTED_EDGE('',*,*,#7287,.F.);
#9955=ORIENTED_EDGE('',*,*,#7291,.F.);
#9956=ORIENTED_EDGE('',*,*,#7294,.F.);
#9957=ORIENTED_EDGE('',*,*,#7297,.F.);
#9958=ORIENTED_EDGE('',*,*,#7300,.F.);
#9959=ORIENTED_EDGE('',*,*,#7303,.F.);
#9960=ORIENTED_EDGE('',*,*,#7306,.F.);
#9961=ORIENTED_EDGE('',*,*,#7309,.F.);
#9962=ORIENTED_EDGE('',*,*,#7312,.F.);
#9963=ORIENTED_EDGE('',*,*,#7315,.F.);
#9964=ORIENTED_EDGE('',*,*,#7318,.F.);
#9965=ORIENTED_EDGE('',*,*,#7321,.F.);
#9966=ORIENTED_EDGE('',*,*,#7324,.F.);
#9967=ORIENTED_EDGE('',*,*,#7327,.F.);
#9968=ORIENTED_EDGE('',*,*,#7330,.F.);
#9969=ORIENTED_EDGE('',*,*,#7333,.F.);
#9970=ORIENTED_EDGE('',*,*,#7336,.F.);
#9971=ORIENTED_EDGE('',*,*,#7339,.F.);
#9972=ORIENTED_EDGE('',*,*,#7342,.F.);
#9973=ORIENTED_EDGE('',*,*,#7345,.F.);
#9974=ORIENTED_EDGE('',*,*,#7348,.F.);
#9975=ORIENTED_EDGE('',*,*,#7351,.F.);
#9976=ORIENTED_EDGE('',*,*,#7354,.F.);
#9977=ORIENTED_EDGE('',*,*,#7357,.F.);
#9978=ORIENTED_EDGE('',*,*,#7440,.F.);
#9979=ORIENTED_EDGE('',*,*,#7429,.T.);
#9980=ORIENTED_EDGE('',*,*,#7441,.F.);
#9981=ORIENTED_EDGE('',*,*,#7442,.F.);
#9982=ORIENTED_EDGE('',*,*,#7438,.T.);
#9983=ORIENTED_EDGE('',*,*,#7432,.T.);
#9984=ORIENTED_EDGE('',*,*,#7435,.T.);
#9985=ORIENTED_EDGE('',*,*,#7443,.F.);
#9986=ORIENTED_EDGE('',*,*,#7358,.F.);
#9987=ORIENTED_EDGE('',*,*,#7355,.F.);
#9988=ORIENTED_EDGE('',*,*,#7352,.F.);
#9989=ORIENTED_EDGE('',*,*,#7349,.F.);
#9990=ORIENTED_EDGE('',*,*,#7346,.F.);
#9991=ORIENTED_EDGE('',*,*,#7343,.F.);
#9992=ORIENTED_EDGE('',*,*,#7340,.F.);
#9993=ORIENTED_EDGE('',*,*,#7337,.F.);
#9994=ORIENTED_EDGE('',*,*,#7334,.F.);
#9995=ORIENTED_EDGE('',*,*,#7331,.F.);
#9996=ORIENTED_EDGE('',*,*,#7328,.F.);
#9997=ORIENTED_EDGE('',*,*,#7325,.F.);
#9998=ORIENTED_EDGE('',*,*,#7322,.F.);
#9999=ORIENTED_EDGE('',*,*,#7319,.F.);
#10000=ORIENTED_EDGE('',*,*,#7316,.F.);
#10001=ORIENTED_EDGE('',*,*,#7313,.F.);
#10002=ORIENTED_EDGE('',*,*,#7310,.F.);
#10003=ORIENTED_EDGE('',*,*,#7307,.F.);
#10004=ORIENTED_EDGE('',*,*,#7304,.F.);
#10005=ORIENTED_EDGE('',*,*,#7301,.F.);
#10006=ORIENTED_EDGE('',*,*,#7298,.F.);
#10007=ORIENTED_EDGE('',*,*,#7295,.F.);
#10008=ORIENTED_EDGE('',*,*,#7292,.F.);
#10009=ORIENTED_EDGE('',*,*,#7289,.F.);
#10010=ORIENTED_EDGE('',*,*,#7444,.F.);
#10011=ORIENTED_EDGE('',*,*,#7441,.T.);
#10012=ORIENTED_EDGE('',*,*,#7431,.T.);
#10013=ORIENTED_EDGE('',*,*,#7428,.T.);
#10014=ORIENTED_EDGE('',*,*,#7425,.T.);
#10015=ORIENTED_EDGE('',*,*,#7422,.T.);
#10016=ORIENTED_EDGE('',*,*,#7419,.T.);
#10017=ORIENTED_EDGE('',*,*,#7416,.T.);
#10018=ORIENTED_EDGE('',*,*,#7413,.T.);
#10019=ORIENTED_EDGE('',*,*,#7410,.T.);
#10020=ORIENTED_EDGE('',*,*,#7407,.T.);
#10021=ORIENTED_EDGE('',*,*,#7404,.T.);
#10022=ORIENTED_EDGE('',*,*,#7401,.T.);
#10023=ORIENTED_EDGE('',*,*,#7398,.T.);
#10024=ORIENTED_EDGE('',*,*,#7395,.T.);
#10025=ORIENTED_EDGE('',*,*,#7392,.T.);
#10026=ORIENTED_EDGE('',*,*,#7389,.T.);
#10027=ORIENTED_EDGE('',*,*,#7386,.T.);
#10028=ORIENTED_EDGE('',*,*,#7383,.T.);
#10029=ORIENTED_EDGE('',*,*,#7380,.T.);
#10030=ORIENTED_EDGE('',*,*,#7377,.T.);
#10031=ORIENTED_EDGE('',*,*,#7374,.T.);
#10032=ORIENTED_EDGE('',*,*,#7371,.T.);
#10033=ORIENTED_EDGE('',*,*,#7368,.T.);
#10034=ORIENTED_EDGE('',*,*,#7365,.T.);
#10035=ORIENTED_EDGE('',*,*,#7362,.T.);
#10036=ORIENTED_EDGE('',*,*,#7356,.T.);
#10037=ORIENTED_EDGE('',*,*,#7443,.T.);
#10038=ORIENTED_EDGE('',*,*,#7434,.T.);
#10039=ORIENTED_EDGE('',*,*,#7440,.T.);
#10040=ORIENTED_EDGE('',*,*,#7445,.F.);
#10041=ORIENTED_EDGE('',*,*,#7446,.T.);
#10042=ORIENTED_EDGE('',*,*,#7447,.T.);
#10043=ORIENTED_EDGE('',*,*,#7448,.F.);
#10044=ORIENTED_EDGE('',*,*,#7449,.F.);
#10045=ORIENTED_EDGE('',*,*,#7450,.T.);
#10046=ORIENTED_EDGE('',*,*,#7451,.T.);
#10047=ORIENTED_EDGE('',*,*,#7446,.F.);
#10048=ORIENTED_EDGE('',*,*,#7452,.F.);
#10049=ORIENTED_EDGE('',*,*,#7453,.T.);
#10050=ORIENTED_EDGE('',*,*,#7454,.T.);
#10051=ORIENTED_EDGE('',*,*,#7450,.F.);
#10052=ORIENTED_EDGE('',*,*,#7455,.F.);
#10053=ORIENTED_EDGE('',*,*,#7456,.T.);
#10054=ORIENTED_EDGE('',*,*,#7457,.T.);
#10055=ORIENTED_EDGE('',*,*,#7453,.F.);
#10056=ORIENTED_EDGE('',*,*,#7458,.F.);
#10057=ORIENTED_EDGE('',*,*,#7459,.T.);
#10058=ORIENTED_EDGE('',*,*,#7460,.T.);
#10059=ORIENTED_EDGE('',*,*,#7456,.F.);
#10060=ORIENTED_EDGE('',*,*,#7461,.F.);
#10061=ORIENTED_EDGE('',*,*,#7448,.T.);
#10062=ORIENTED_EDGE('',*,*,#7462,.T.);
#10063=ORIENTED_EDGE('',*,*,#7459,.F.);
#10064=ORIENTED_EDGE('',*,*,#7462,.F.);
#10065=ORIENTED_EDGE('',*,*,#7447,.F.);
#10066=ORIENTED_EDGE('',*,*,#7451,.F.);
#10067=ORIENTED_EDGE('',*,*,#7454,.F.);
#10068=ORIENTED_EDGE('',*,*,#7457,.F.);
#10069=ORIENTED_EDGE('',*,*,#7460,.F.);
#10070=ORIENTED_EDGE('',*,*,#7463,.T.);
#10071=ORIENTED_EDGE('',*,*,#7439,.T.);
#10072=ORIENTED_EDGE('',*,*,#7442,.T.);
#10073=ORIENTED_EDGE('',*,*,#7444,.T.);
#10074=ORIENTED_EDGE('',*,*,#7288,.F.);
#10075=ORIENTED_EDGE('',*,*,#7463,.F.);
#10076=ORIENTED_EDGE('',*,*,#7464,.T.);
#10077=ORIENTED_EDGE('',*,*,#7465,.T.);
#10078=ORIENTED_EDGE('',*,*,#7464,.F.);
#10079=ORIENTED_EDGE('',*,*,#7465,.F.);
#10080=ORIENTED_EDGE('',*,*,#7445,.T.);
#10081=ORIENTED_EDGE('',*,*,#7461,.T.);
#10082=ORIENTED_EDGE('',*,*,#7458,.T.);
#10083=ORIENTED_EDGE('',*,*,#7455,.T.);
#10084=ORIENTED_EDGE('',*,*,#7452,.T.);
#10085=ORIENTED_EDGE('',*,*,#7449,.T.);
#10086=ORIENTED_EDGE('',*,*,#7437,.T.);
#10087=ORIENTED_EDGE('',*,*,#7466,.F.);
#10088=ORIENTED_EDGE('',*,*,#7467,.T.);
#10089=ORIENTED_EDGE('',*,*,#7468,.T.);
#10090=ORIENTED_EDGE('',*,*,#7467,.F.);
#10091=ORIENTED_EDGE('',*,*,#7469,.F.);
#10092=ORIENTED_EDGE('',*,*,#7470,.T.);
#10093=ORIENTED_EDGE('',*,*,#7471,.T.);
#10094=ORIENTED_EDGE('',*,*,#7470,.F.);
#10095=ORIENTED_EDGE('',*,*,#7469,.T.);
#10096=ORIENTED_EDGE('',*,*,#7466,.T.);
#10097=ORIENTED_EDGE('',*,*,#7471,.F.);
#10098=ORIENTED_EDGE('',*,*,#7468,.F.);
#10099=ORIENTED_EDGE('',*,*,#7472,.T.);
#10100=ORIENTED_EDGE('',*,*,#7473,.T.);
#10101=ORIENTED_EDGE('',*,*,#7474,.T.);
#10102=ORIENTED_EDGE('',*,*,#7475,.T.);
#10103=ORIENTED_EDGE('',*,*,#7476,.T.);
#10104=ORIENTED_EDGE('',*,*,#7475,.F.);
#10105=ORIENTED_EDGE('',*,*,#7477,.T.);
#10106=ORIENTED_EDGE('',*,*,#7478,.T.);
#10107=ORIENTED_EDGE('',*,*,#7479,.T.);
#10108=ORIENTED_EDGE('',*,*,#7480,.T.);
#10109=ORIENTED_EDGE('',*,*,#7472,.F.);
#10110=ORIENTED_EDGE('',*,*,#7481,.T.);
#10111=ORIENTED_EDGE('',*,*,#7482,.T.);
#10112=ORIENTED_EDGE('',*,*,#7483,.T.);
#10113=ORIENTED_EDGE('',*,*,#7479,.F.);
#10114=ORIENTED_EDGE('',*,*,#7484,.T.);
#10115=ORIENTED_EDGE('',*,*,#7485,.T.);
#10116=ORIENTED_EDGE('',*,*,#7486,.T.);
#10117=ORIENTED_EDGE('',*,*,#7482,.F.);
#10118=ORIENTED_EDGE('',*,*,#7487,.T.);
#10119=ORIENTED_EDGE('',*,*,#7488,.T.);
#10120=ORIENTED_EDGE('',*,*,#7489,.T.);
#10121=ORIENTED_EDGE('',*,*,#7485,.F.);
#10122=ORIENTED_EDGE('',*,*,#7490,.T.);
#10123=ORIENTED_EDGE('',*,*,#7491,.T.);
#10124=ORIENTED_EDGE('',*,*,#7492,.T.);
#10125=ORIENTED_EDGE('',*,*,#7488,.F.);
#10126=ORIENTED_EDGE('',*,*,#7493,.T.);
#10127=ORIENTED_EDGE('',*,*,#7494,.T.);
#10128=ORIENTED_EDGE('',*,*,#7495,.T.);
#10129=ORIENTED_EDGE('',*,*,#7491,.F.);
#10130=ORIENTED_EDGE('',*,*,#7496,.T.);
#10131=ORIENTED_EDGE('',*,*,#7497,.T.);
#10132=ORIENTED_EDGE('',*,*,#7498,.T.);
#10133=ORIENTED_EDGE('',*,*,#7494,.F.);
#10134=ORIENTED_EDGE('',*,*,#7499,.T.);
#10135=ORIENTED_EDGE('',*,*,#7500,.T.);
#10136=ORIENTED_EDGE('',*,*,#7501,.T.);
#10137=ORIENTED_EDGE('',*,*,#7497,.F.);
#10138=ORIENTED_EDGE('',*,*,#7502,.T.);
#10139=ORIENTED_EDGE('',*,*,#7503,.T.);
#10140=ORIENTED_EDGE('',*,*,#7504,.T.);
#10141=ORIENTED_EDGE('',*,*,#7500,.F.);
#10142=ORIENTED_EDGE('',*,*,#7505,.T.);
#10143=ORIENTED_EDGE('',*,*,#7506,.T.);
#10144=ORIENTED_EDGE('',*,*,#7507,.T.);
#10145=ORIENTED_EDGE('',*,*,#7503,.F.);
#10146=ORIENTED_EDGE('',*,*,#7508,.T.);
#10147=ORIENTED_EDGE('',*,*,#7509,.T.);
#10148=ORIENTED_EDGE('',*,*,#7510,.T.);
#10149=ORIENTED_EDGE('',*,*,#7506,.F.);
#10150=ORIENTED_EDGE('',*,*,#7511,.T.);
#10151=ORIENTED_EDGE('',*,*,#7512,.T.);
#10152=ORIENTED_EDGE('',*,*,#7513,.T.);
#10153=ORIENTED_EDGE('',*,*,#7509,.F.);
#10154=ORIENTED_EDGE('',*,*,#7514,.T.);
#10155=ORIENTED_EDGE('',*,*,#7515,.T.);
#10156=ORIENTED_EDGE('',*,*,#7516,.T.);
#10157=ORIENTED_EDGE('',*,*,#7512,.F.);
#10158=ORIENTED_EDGE('',*,*,#7517,.T.);
#10159=ORIENTED_EDGE('',*,*,#7518,.T.);
#10160=ORIENTED_EDGE('',*,*,#7519,.T.);
#10161=ORIENTED_EDGE('',*,*,#7515,.F.);
#10162=ORIENTED_EDGE('',*,*,#7520,.T.);
#10163=ORIENTED_EDGE('',*,*,#7521,.T.);
#10164=ORIENTED_EDGE('',*,*,#7522,.T.);
#10165=ORIENTED_EDGE('',*,*,#7518,.F.);
#10166=ORIENTED_EDGE('',*,*,#7523,.T.);
#10167=ORIENTED_EDGE('',*,*,#7524,.T.);
#10168=ORIENTED_EDGE('',*,*,#7525,.T.);
#10169=ORIENTED_EDGE('',*,*,#7521,.F.);
#10170=ORIENTED_EDGE('',*,*,#7526,.T.);
#10171=ORIENTED_EDGE('',*,*,#7527,.T.);
#10172=ORIENTED_EDGE('',*,*,#7528,.T.);
#10173=ORIENTED_EDGE('',*,*,#7524,.F.);
#10174=ORIENTED_EDGE('',*,*,#7529,.T.);
#10175=ORIENTED_EDGE('',*,*,#7530,.T.);
#10176=ORIENTED_EDGE('',*,*,#7531,.T.);
#10177=ORIENTED_EDGE('',*,*,#7527,.F.);
#10178=ORIENTED_EDGE('',*,*,#7532,.T.);
#10179=ORIENTED_EDGE('',*,*,#7533,.T.);
#10180=ORIENTED_EDGE('',*,*,#7534,.T.);
#10181=ORIENTED_EDGE('',*,*,#7530,.F.);
#10182=ORIENTED_EDGE('',*,*,#7535,.T.);
#10183=ORIENTED_EDGE('',*,*,#7536,.T.);
#10184=ORIENTED_EDGE('',*,*,#7537,.T.);
#10185=ORIENTED_EDGE('',*,*,#7533,.F.);
#10186=ORIENTED_EDGE('',*,*,#7538,.T.);
#10187=ORIENTED_EDGE('',*,*,#7539,.T.);
#10188=ORIENTED_EDGE('',*,*,#7540,.T.);
#10189=ORIENTED_EDGE('',*,*,#7536,.F.);
#10190=ORIENTED_EDGE('',*,*,#7541,.T.);
#10191=ORIENTED_EDGE('',*,*,#7542,.T.);
#10192=ORIENTED_EDGE('',*,*,#7543,.T.);
#10193=ORIENTED_EDGE('',*,*,#7539,.F.);
#10194=ORIENTED_EDGE('',*,*,#7544,.T.);
#10195=ORIENTED_EDGE('',*,*,#7545,.T.);
#10196=ORIENTED_EDGE('',*,*,#7546,.T.);
#10197=ORIENTED_EDGE('',*,*,#7542,.F.);
#10198=ORIENTED_EDGE('',*,*,#7547,.T.);
#10199=ORIENTED_EDGE('',*,*,#7548,.F.);
#10200=ORIENTED_EDGE('',*,*,#7549,.T.);
#10201=ORIENTED_EDGE('',*,*,#7550,.F.);
#10202=ORIENTED_EDGE('',*,*,#7551,.T.);
#10203=ORIENTED_EDGE('',*,*,#7552,.T.);
#10204=ORIENTED_EDGE('',*,*,#7553,.T.);
#10205=ORIENTED_EDGE('',*,*,#7554,.F.);
#10206=ORIENTED_EDGE('',*,*,#7555,.F.);
#10207=ORIENTED_EDGE('',*,*,#7556,.T.);
#10208=ORIENTED_EDGE('',*,*,#7557,.T.);
#10209=ORIENTED_EDGE('',*,*,#7552,.F.);
#10210=ORIENTED_EDGE('',*,*,#7558,.F.);
#10211=ORIENTED_EDGE('',*,*,#7559,.T.);
#10212=ORIENTED_EDGE('',*,*,#7560,.T.);
#10213=ORIENTED_EDGE('',*,*,#7556,.F.);
#10214=ORIENTED_EDGE('',*,*,#7561,.F.);
#10215=ORIENTED_EDGE('',*,*,#7562,.T.);
#10216=ORIENTED_EDGE('',*,*,#7563,.T.);
#10217=ORIENTED_EDGE('',*,*,#7559,.F.);
#10218=ORIENTED_EDGE('',*,*,#7564,.F.);
#10219=ORIENTED_EDGE('',*,*,#7565,.T.);
#10220=ORIENTED_EDGE('',*,*,#7566,.T.);
#10221=ORIENTED_EDGE('',*,*,#7562,.F.);
#10222=ORIENTED_EDGE('',*,*,#7567,.F.);
#10223=ORIENTED_EDGE('',*,*,#7568,.T.);
#10224=ORIENTED_EDGE('',*,*,#7569,.T.);
#10225=ORIENTED_EDGE('',*,*,#7565,.F.);
#10226=ORIENTED_EDGE('',*,*,#7570,.F.);
#10227=ORIENTED_EDGE('',*,*,#7571,.T.);
#10228=ORIENTED_EDGE('',*,*,#7572,.T.);
#10229=ORIENTED_EDGE('',*,*,#7568,.F.);
#10230=ORIENTED_EDGE('',*,*,#7573,.F.);
#10231=ORIENTED_EDGE('',*,*,#7574,.T.);
#10232=ORIENTED_EDGE('',*,*,#7575,.T.);
#10233=ORIENTED_EDGE('',*,*,#7571,.F.);
#10234=ORIENTED_EDGE('',*,*,#7576,.F.);
#10235=ORIENTED_EDGE('',*,*,#7577,.T.);
#10236=ORIENTED_EDGE('',*,*,#7578,.T.);
#10237=ORIENTED_EDGE('',*,*,#7574,.F.);
#10238=ORIENTED_EDGE('',*,*,#7579,.F.);
#10239=ORIENTED_EDGE('',*,*,#7580,.T.);
#10240=ORIENTED_EDGE('',*,*,#7581,.T.);
#10241=ORIENTED_EDGE('',*,*,#7577,.F.);
#10242=ORIENTED_EDGE('',*,*,#7582,.F.);
#10243=ORIENTED_EDGE('',*,*,#7583,.T.);
#10244=ORIENTED_EDGE('',*,*,#7584,.T.);
#10245=ORIENTED_EDGE('',*,*,#7580,.F.);
#10246=ORIENTED_EDGE('',*,*,#7585,.F.);
#10247=ORIENTED_EDGE('',*,*,#7586,.T.);
#10248=ORIENTED_EDGE('',*,*,#7587,.T.);
#10249=ORIENTED_EDGE('',*,*,#7583,.F.);
#10250=ORIENTED_EDGE('',*,*,#7588,.F.);
#10251=ORIENTED_EDGE('',*,*,#7589,.T.);
#10252=ORIENTED_EDGE('',*,*,#7590,.T.);
#10253=ORIENTED_EDGE('',*,*,#7586,.F.);
#10254=ORIENTED_EDGE('',*,*,#7591,.F.);
#10255=ORIENTED_EDGE('',*,*,#7592,.T.);
#10256=ORIENTED_EDGE('',*,*,#7593,.T.);
#10257=ORIENTED_EDGE('',*,*,#7589,.F.);
#10258=ORIENTED_EDGE('',*,*,#7594,.F.);
#10259=ORIENTED_EDGE('',*,*,#7595,.T.);
#10260=ORIENTED_EDGE('',*,*,#7596,.T.);
#10261=ORIENTED_EDGE('',*,*,#7592,.F.);
#10262=ORIENTED_EDGE('',*,*,#7597,.F.);
#10263=ORIENTED_EDGE('',*,*,#7598,.T.);
#10264=ORIENTED_EDGE('',*,*,#7599,.T.);
#10265=ORIENTED_EDGE('',*,*,#7595,.F.);
#10266=ORIENTED_EDGE('',*,*,#7600,.F.);
#10267=ORIENTED_EDGE('',*,*,#7601,.T.);
#10268=ORIENTED_EDGE('',*,*,#7602,.T.);
#10269=ORIENTED_EDGE('',*,*,#7598,.F.);
#10270=ORIENTED_EDGE('',*,*,#7603,.F.);
#10271=ORIENTED_EDGE('',*,*,#7604,.T.);
#10272=ORIENTED_EDGE('',*,*,#7605,.T.);
#10273=ORIENTED_EDGE('',*,*,#7601,.F.);
#10274=ORIENTED_EDGE('',*,*,#7606,.F.);
#10275=ORIENTED_EDGE('',*,*,#7607,.T.);
#10276=ORIENTED_EDGE('',*,*,#7608,.T.);
#10277=ORIENTED_EDGE('',*,*,#7604,.F.);
#10278=ORIENTED_EDGE('',*,*,#7609,.F.);
#10279=ORIENTED_EDGE('',*,*,#7610,.T.);
#10280=ORIENTED_EDGE('',*,*,#7611,.T.);
#10281=ORIENTED_EDGE('',*,*,#7607,.F.);
#10282=ORIENTED_EDGE('',*,*,#7612,.F.);
#10283=ORIENTED_EDGE('',*,*,#7613,.T.);
#10284=ORIENTED_EDGE('',*,*,#7614,.T.);
#10285=ORIENTED_EDGE('',*,*,#7610,.F.);
#10286=ORIENTED_EDGE('',*,*,#7615,.F.);
#10287=ORIENTED_EDGE('',*,*,#7616,.T.);
#10288=ORIENTED_EDGE('',*,*,#7617,.T.);
#10289=ORIENTED_EDGE('',*,*,#7613,.F.);
#10290=ORIENTED_EDGE('',*,*,#7618,.F.);
#10291=ORIENTED_EDGE('',*,*,#7619,.T.);
#10292=ORIENTED_EDGE('',*,*,#7620,.T.);
#10293=ORIENTED_EDGE('',*,*,#7616,.F.);
#10294=ORIENTED_EDGE('',*,*,#7621,.F.);
#10295=ORIENTED_EDGE('',*,*,#7622,.T.);
#10296=ORIENTED_EDGE('',*,*,#7623,.T.);
#10297=ORIENTED_EDGE('',*,*,#7619,.F.);
#10298=ORIENTED_EDGE('',*,*,#7624,.F.);
#10299=ORIENTED_EDGE('',*,*,#7625,.F.);
#10300=ORIENTED_EDGE('',*,*,#7626,.F.);
#10301=ORIENTED_EDGE('',*,*,#7627,.F.);
#10302=ORIENTED_EDGE('',*,*,#7628,.T.);
#10303=ORIENTED_EDGE('',*,*,#7629,.T.);
#10304=ORIENTED_EDGE('',*,*,#7630,.T.);
#10305=ORIENTED_EDGE('',*,*,#7631,.T.);
#10306=ORIENTED_EDGE('',*,*,#7632,.T.);
#10307=ORIENTED_EDGE('',*,*,#7633,.T.);
#10308=ORIENTED_EDGE('',*,*,#7632,.F.);
#10309=ORIENTED_EDGE('',*,*,#7634,.T.);
#10310=ORIENTED_EDGE('',*,*,#7635,.T.);
#10311=ORIENTED_EDGE('',*,*,#7636,.T.);
#10312=ORIENTED_EDGE('',*,*,#7637,.T.);
#10313=ORIENTED_EDGE('',*,*,#7629,.F.);
#10314=ORIENTED_EDGE('',*,*,#7638,.T.);
#10315=ORIENTED_EDGE('',*,*,#7639,.T.);
#10316=ORIENTED_EDGE('',*,*,#7640,.T.);
#10317=ORIENTED_EDGE('',*,*,#7636,.F.);
#10318=ORIENTED_EDGE('',*,*,#7641,.T.);
#10319=ORIENTED_EDGE('',*,*,#7642,.T.);
#10320=ORIENTED_EDGE('',*,*,#7643,.T.);
#10321=ORIENTED_EDGE('',*,*,#7639,.F.);
#10322=ORIENTED_EDGE('',*,*,#7644,.T.);
#10323=ORIENTED_EDGE('',*,*,#7645,.T.);
#10324=ORIENTED_EDGE('',*,*,#7646,.T.);
#10325=ORIENTED_EDGE('',*,*,#7642,.F.);
#10326=ORIENTED_EDGE('',*,*,#7647,.T.);
#10327=ORIENTED_EDGE('',*,*,#7648,.T.);
#10328=ORIENTED_EDGE('',*,*,#7649,.T.);
#10329=ORIENTED_EDGE('',*,*,#7645,.F.);
#10330=ORIENTED_EDGE('',*,*,#7650,.T.);
#10331=ORIENTED_EDGE('',*,*,#7651,.T.);
#10332=ORIENTED_EDGE('',*,*,#7652,.T.);
#10333=ORIENTED_EDGE('',*,*,#7648,.F.);
#10334=ORIENTED_EDGE('',*,*,#7653,.T.);
#10335=ORIENTED_EDGE('',*,*,#7654,.T.);
#10336=ORIENTED_EDGE('',*,*,#7655,.T.);
#10337=ORIENTED_EDGE('',*,*,#7651,.F.);
#10338=ORIENTED_EDGE('',*,*,#7656,.T.);
#10339=ORIENTED_EDGE('',*,*,#7657,.T.);
#10340=ORIENTED_EDGE('',*,*,#7658,.T.);
#10341=ORIENTED_EDGE('',*,*,#7654,.F.);
#10342=ORIENTED_EDGE('',*,*,#7659,.T.);
#10343=ORIENTED_EDGE('',*,*,#7660,.T.);
#10344=ORIENTED_EDGE('',*,*,#7661,.T.);
#10345=ORIENTED_EDGE('',*,*,#7657,.F.);
#10346=ORIENTED_EDGE('',*,*,#7662,.T.);
#10347=ORIENTED_EDGE('',*,*,#7663,.T.);
#10348=ORIENTED_EDGE('',*,*,#7664,.T.);
#10349=ORIENTED_EDGE('',*,*,#7660,.F.);
#10350=ORIENTED_EDGE('',*,*,#7665,.T.);
#10351=ORIENTED_EDGE('',*,*,#7666,.T.);
#10352=ORIENTED_EDGE('',*,*,#7667,.T.);
#10353=ORIENTED_EDGE('',*,*,#7663,.F.);
#10354=ORIENTED_EDGE('',*,*,#7668,.T.);
#10355=ORIENTED_EDGE('',*,*,#7669,.T.);
#10356=ORIENTED_EDGE('',*,*,#7670,.T.);
#10357=ORIENTED_EDGE('',*,*,#7666,.F.);
#10358=ORIENTED_EDGE('',*,*,#7671,.T.);
#10359=ORIENTED_EDGE('',*,*,#7672,.T.);
#10360=ORIENTED_EDGE('',*,*,#7673,.T.);
#10361=ORIENTED_EDGE('',*,*,#7669,.F.);
#10362=ORIENTED_EDGE('',*,*,#7674,.T.);
#10363=ORIENTED_EDGE('',*,*,#7675,.T.);
#10364=ORIENTED_EDGE('',*,*,#7676,.T.);
#10365=ORIENTED_EDGE('',*,*,#7672,.F.);
#10366=ORIENTED_EDGE('',*,*,#7677,.T.);
#10367=ORIENTED_EDGE('',*,*,#7678,.T.);
#10368=ORIENTED_EDGE('',*,*,#7679,.T.);
#10369=ORIENTED_EDGE('',*,*,#7675,.F.);
#10370=ORIENTED_EDGE('',*,*,#7680,.T.);
#10371=ORIENTED_EDGE('',*,*,#7681,.T.);
#10372=ORIENTED_EDGE('',*,*,#7682,.T.);
#10373=ORIENTED_EDGE('',*,*,#7678,.F.);
#10374=ORIENTED_EDGE('',*,*,#7683,.T.);
#10375=ORIENTED_EDGE('',*,*,#7684,.T.);
#10376=ORIENTED_EDGE('',*,*,#7685,.T.);
#10377=ORIENTED_EDGE('',*,*,#7681,.F.);
#10378=ORIENTED_EDGE('',*,*,#7686,.T.);
#10379=ORIENTED_EDGE('',*,*,#7687,.T.);
#10380=ORIENTED_EDGE('',*,*,#7688,.T.);
#10381=ORIENTED_EDGE('',*,*,#7684,.F.);
#10382=ORIENTED_EDGE('',*,*,#7689,.T.);
#10383=ORIENTED_EDGE('',*,*,#7690,.T.);
#10384=ORIENTED_EDGE('',*,*,#7691,.T.);
#10385=ORIENTED_EDGE('',*,*,#7687,.F.);
#10386=ORIENTED_EDGE('',*,*,#7692,.T.);
#10387=ORIENTED_EDGE('',*,*,#7693,.T.);
#10388=ORIENTED_EDGE('',*,*,#7694,.T.);
#10389=ORIENTED_EDGE('',*,*,#7690,.F.);
#10390=ORIENTED_EDGE('',*,*,#7695,.T.);
#10391=ORIENTED_EDGE('',*,*,#7696,.T.);
#10392=ORIENTED_EDGE('',*,*,#7697,.T.);
#10393=ORIENTED_EDGE('',*,*,#7693,.F.);
#10394=ORIENTED_EDGE('',*,*,#7698,.T.);
#10395=ORIENTED_EDGE('',*,*,#7699,.T.);
#10396=ORIENTED_EDGE('',*,*,#7700,.T.);
#10397=ORIENTED_EDGE('',*,*,#7696,.F.);
#10398=ORIENTED_EDGE('',*,*,#7701,.T.);
#10399=ORIENTED_EDGE('',*,*,#7702,.T.);
#10400=ORIENTED_EDGE('',*,*,#7703,.T.);
#10401=ORIENTED_EDGE('',*,*,#7699,.F.);
#10402=ORIENTED_EDGE('',*,*,#7704,.T.);
#10403=ORIENTED_EDGE('',*,*,#7705,.T.);
#10404=ORIENTED_EDGE('',*,*,#7706,.T.);
#10405=ORIENTED_EDGE('',*,*,#7702,.F.);
#10406=ORIENTED_EDGE('',*,*,#7707,.T.);
#10407=ORIENTED_EDGE('',*,*,#7708,.T.);
#10408=ORIENTED_EDGE('',*,*,#7709,.T.);
#10409=ORIENTED_EDGE('',*,*,#7705,.F.);
#10410=ORIENTED_EDGE('',*,*,#7710,.T.);
#10411=ORIENTED_EDGE('',*,*,#7711,.T.);
#10412=ORIENTED_EDGE('',*,*,#7712,.T.);
#10413=ORIENTED_EDGE('',*,*,#7708,.F.);
#10414=ORIENTED_EDGE('',*,*,#7713,.T.);
#10415=ORIENTED_EDGE('',*,*,#7714,.T.);
#10416=ORIENTED_EDGE('',*,*,#7715,.T.);
#10417=ORIENTED_EDGE('',*,*,#7711,.F.);
#10418=ORIENTED_EDGE('',*,*,#7716,.T.);
#10419=ORIENTED_EDGE('',*,*,#7717,.T.);
#10420=ORIENTED_EDGE('',*,*,#7718,.T.);
#10421=ORIENTED_EDGE('',*,*,#7714,.F.);
#10422=ORIENTED_EDGE('',*,*,#7719,.T.);
#10423=ORIENTED_EDGE('',*,*,#7720,.T.);
#10424=ORIENTED_EDGE('',*,*,#7721,.T.);
#10425=ORIENTED_EDGE('',*,*,#7717,.F.);
#10426=ORIENTED_EDGE('',*,*,#7722,.T.);
#10427=ORIENTED_EDGE('',*,*,#7723,.T.);
#10428=ORIENTED_EDGE('',*,*,#7724,.T.);
#10429=ORIENTED_EDGE('',*,*,#7720,.F.);
#10430=ORIENTED_EDGE('',*,*,#7725,.T.);
#10431=ORIENTED_EDGE('',*,*,#7726,.T.);
#10432=ORIENTED_EDGE('',*,*,#7727,.T.);
#10433=ORIENTED_EDGE('',*,*,#7723,.F.);
#10434=ORIENTED_EDGE('',*,*,#7728,.T.);
#10435=ORIENTED_EDGE('',*,*,#7729,.T.);
#10436=ORIENTED_EDGE('',*,*,#7730,.T.);
#10437=ORIENTED_EDGE('',*,*,#7726,.F.);
#10438=ORIENTED_EDGE('',*,*,#7731,.T.);
#10439=ORIENTED_EDGE('',*,*,#7732,.T.);
#10440=ORIENTED_EDGE('',*,*,#7733,.T.);
#10441=ORIENTED_EDGE('',*,*,#7729,.F.);
#10442=ORIENTED_EDGE('',*,*,#7734,.T.);
#10443=ORIENTED_EDGE('',*,*,#7735,.T.);
#10444=ORIENTED_EDGE('',*,*,#7736,.T.);
#10445=ORIENTED_EDGE('',*,*,#7732,.F.);
#10446=ORIENTED_EDGE('',*,*,#7737,.T.);
#10447=ORIENTED_EDGE('',*,*,#7738,.T.);
#10448=ORIENTED_EDGE('',*,*,#7739,.T.);
#10449=ORIENTED_EDGE('',*,*,#7735,.F.);
#10450=ORIENTED_EDGE('',*,*,#7740,.T.);
#10451=ORIENTED_EDGE('',*,*,#7741,.T.);
#10452=ORIENTED_EDGE('',*,*,#7742,.T.);
#10453=ORIENTED_EDGE('',*,*,#7738,.F.);
#10454=ORIENTED_EDGE('',*,*,#7743,.T.);
#10455=ORIENTED_EDGE('',*,*,#7744,.T.);
#10456=ORIENTED_EDGE('',*,*,#7745,.T.);
#10457=ORIENTED_EDGE('',*,*,#7741,.F.);
#10458=ORIENTED_EDGE('',*,*,#7746,.T.);
#10459=ORIENTED_EDGE('',*,*,#7747,.T.);
#10460=ORIENTED_EDGE('',*,*,#7748,.T.);
#10461=ORIENTED_EDGE('',*,*,#7744,.F.);
#10462=ORIENTED_EDGE('',*,*,#7749,.T.);
#10463=ORIENTED_EDGE('',*,*,#7750,.F.);
#10464=ORIENTED_EDGE('',*,*,#7751,.T.);
#10465=ORIENTED_EDGE('',*,*,#7752,.F.);
#10466=ORIENTED_EDGE('',*,*,#7753,.T.);
#10467=ORIENTED_EDGE('',*,*,#7754,.T.);
#10468=ORIENTED_EDGE('',*,*,#7755,.T.);
#10469=ORIENTED_EDGE('',*,*,#7756,.F.);
#10470=ORIENTED_EDGE('',*,*,#7757,.F.);
#10471=ORIENTED_EDGE('',*,*,#7758,.T.);
#10472=ORIENTED_EDGE('',*,*,#7759,.T.);
#10473=ORIENTED_EDGE('',*,*,#7754,.F.);
#10474=ORIENTED_EDGE('',*,*,#7760,.F.);
#10475=ORIENTED_EDGE('',*,*,#7761,.T.);
#10476=ORIENTED_EDGE('',*,*,#7762,.T.);
#10477=ORIENTED_EDGE('',*,*,#7758,.F.);
#10478=ORIENTED_EDGE('',*,*,#7763,.F.);
#10479=ORIENTED_EDGE('',*,*,#7764,.T.);
#10480=ORIENTED_EDGE('',*,*,#7765,.T.);
#10481=ORIENTED_EDGE('',*,*,#7761,.F.);
#10482=ORIENTED_EDGE('',*,*,#7766,.F.);
#10483=ORIENTED_EDGE('',*,*,#7767,.T.);
#10484=ORIENTED_EDGE('',*,*,#7768,.T.);
#10485=ORIENTED_EDGE('',*,*,#7764,.F.);
#10486=ORIENTED_EDGE('',*,*,#7769,.F.);
#10487=ORIENTED_EDGE('',*,*,#7770,.T.);
#10488=ORIENTED_EDGE('',*,*,#7771,.T.);
#10489=ORIENTED_EDGE('',*,*,#7767,.F.);
#10490=ORIENTED_EDGE('',*,*,#7772,.F.);
#10491=ORIENTED_EDGE('',*,*,#7773,.T.);
#10492=ORIENTED_EDGE('',*,*,#7774,.T.);
#10493=ORIENTED_EDGE('',*,*,#7770,.F.);
#10494=ORIENTED_EDGE('',*,*,#7775,.F.);
#10495=ORIENTED_EDGE('',*,*,#7776,.T.);
#10496=ORIENTED_EDGE('',*,*,#7777,.T.);
#10497=ORIENTED_EDGE('',*,*,#7773,.F.);
#10498=ORIENTED_EDGE('',*,*,#7778,.F.);
#10499=ORIENTED_EDGE('',*,*,#7779,.T.);
#10500=ORIENTED_EDGE('',*,*,#7780,.T.);
#10501=ORIENTED_EDGE('',*,*,#7776,.F.);
#10502=ORIENTED_EDGE('',*,*,#7781,.F.);
#10503=ORIENTED_EDGE('',*,*,#7782,.T.);
#10504=ORIENTED_EDGE('',*,*,#7783,.T.);
#10505=ORIENTED_EDGE('',*,*,#7779,.F.);
#10506=ORIENTED_EDGE('',*,*,#7784,.F.);
#10507=ORIENTED_EDGE('',*,*,#7785,.T.);
#10508=ORIENTED_EDGE('',*,*,#7786,.T.);
#10509=ORIENTED_EDGE('',*,*,#7782,.F.);
#10510=ORIENTED_EDGE('',*,*,#7787,.F.);
#10511=ORIENTED_EDGE('',*,*,#7788,.T.);
#10512=ORIENTED_EDGE('',*,*,#7789,.T.);
#10513=ORIENTED_EDGE('',*,*,#7785,.F.);
#10514=ORIENTED_EDGE('',*,*,#7790,.F.);
#10515=ORIENTED_EDGE('',*,*,#7791,.T.);
#10516=ORIENTED_EDGE('',*,*,#7792,.T.);
#10517=ORIENTED_EDGE('',*,*,#7788,.F.);
#10518=ORIENTED_EDGE('',*,*,#7793,.F.);
#10519=ORIENTED_EDGE('',*,*,#7794,.T.);
#10520=ORIENTED_EDGE('',*,*,#7795,.T.);
#10521=ORIENTED_EDGE('',*,*,#7791,.F.);
#10522=ORIENTED_EDGE('',*,*,#7796,.F.);
#10523=ORIENTED_EDGE('',*,*,#7797,.T.);
#10524=ORIENTED_EDGE('',*,*,#7798,.T.);
#10525=ORIENTED_EDGE('',*,*,#7794,.F.);
#10526=ORIENTED_EDGE('',*,*,#7799,.F.);
#10527=ORIENTED_EDGE('',*,*,#7800,.T.);
#10528=ORIENTED_EDGE('',*,*,#7801,.T.);
#10529=ORIENTED_EDGE('',*,*,#7797,.F.);
#10530=ORIENTED_EDGE('',*,*,#7802,.F.);
#10531=ORIENTED_EDGE('',*,*,#7803,.T.);
#10532=ORIENTED_EDGE('',*,*,#7804,.T.);
#10533=ORIENTED_EDGE('',*,*,#7800,.F.);
#10534=ORIENTED_EDGE('',*,*,#7805,.F.);
#10535=ORIENTED_EDGE('',*,*,#7806,.T.);
#10536=ORIENTED_EDGE('',*,*,#7807,.T.);
#10537=ORIENTED_EDGE('',*,*,#7803,.F.);
#10538=ORIENTED_EDGE('',*,*,#7808,.F.);
#10539=ORIENTED_EDGE('',*,*,#7809,.T.);
#10540=ORIENTED_EDGE('',*,*,#7810,.T.);
#10541=ORIENTED_EDGE('',*,*,#7806,.F.);
#10542=ORIENTED_EDGE('',*,*,#7811,.F.);
#10543=ORIENTED_EDGE('',*,*,#7812,.T.);
#10544=ORIENTED_EDGE('',*,*,#7813,.T.);
#10545=ORIENTED_EDGE('',*,*,#7809,.F.);
#10546=ORIENTED_EDGE('',*,*,#7814,.F.);
#10547=ORIENTED_EDGE('',*,*,#7815,.T.);
#10548=ORIENTED_EDGE('',*,*,#7816,.T.);
#10549=ORIENTED_EDGE('',*,*,#7812,.F.);
#10550=ORIENTED_EDGE('',*,*,#7817,.F.);
#10551=ORIENTED_EDGE('',*,*,#7818,.T.);
#10552=ORIENTED_EDGE('',*,*,#7819,.T.);
#10553=ORIENTED_EDGE('',*,*,#7815,.F.);
#10554=ORIENTED_EDGE('',*,*,#7820,.F.);
#10555=ORIENTED_EDGE('',*,*,#7821,.T.);
#10556=ORIENTED_EDGE('',*,*,#7822,.T.);
#10557=ORIENTED_EDGE('',*,*,#7818,.F.);
#10558=ORIENTED_EDGE('',*,*,#7823,.F.);
#10559=ORIENTED_EDGE('',*,*,#7824,.T.);
#10560=ORIENTED_EDGE('',*,*,#7825,.T.);
#10561=ORIENTED_EDGE('',*,*,#7821,.F.);
#10562=ORIENTED_EDGE('',*,*,#7826,.F.);
#10563=ORIENTED_EDGE('',*,*,#7827,.T.);
#10564=ORIENTED_EDGE('',*,*,#7828,.T.);
#10565=ORIENTED_EDGE('',*,*,#7824,.F.);
#10566=ORIENTED_EDGE('',*,*,#7829,.F.);
#10567=ORIENTED_EDGE('',*,*,#7830,.T.);
#10568=ORIENTED_EDGE('',*,*,#7831,.T.);
#10569=ORIENTED_EDGE('',*,*,#7827,.F.);
#10570=ORIENTED_EDGE('',*,*,#7832,.F.);
#10571=ORIENTED_EDGE('',*,*,#7833,.T.);
#10572=ORIENTED_EDGE('',*,*,#7834,.T.);
#10573=ORIENTED_EDGE('',*,*,#7830,.F.);
#10574=ORIENTED_EDGE('',*,*,#7835,.F.);
#10575=ORIENTED_EDGE('',*,*,#7836,.T.);
#10576=ORIENTED_EDGE('',*,*,#7837,.T.);
#10577=ORIENTED_EDGE('',*,*,#7833,.F.);
#10578=ORIENTED_EDGE('',*,*,#7838,.F.);
#10579=ORIENTED_EDGE('',*,*,#7839,.T.);
#10580=ORIENTED_EDGE('',*,*,#7840,.T.);
#10581=ORIENTED_EDGE('',*,*,#7836,.F.);
#10582=ORIENTED_EDGE('',*,*,#7841,.F.);
#10583=ORIENTED_EDGE('',*,*,#7842,.T.);
#10584=ORIENTED_EDGE('',*,*,#7843,.T.);
#10585=ORIENTED_EDGE('',*,*,#7839,.F.);
#10586=ORIENTED_EDGE('',*,*,#7844,.F.);
#10587=ORIENTED_EDGE('',*,*,#7845,.T.);
#10588=ORIENTED_EDGE('',*,*,#7846,.T.);
#10589=ORIENTED_EDGE('',*,*,#7842,.F.);
#10590=ORIENTED_EDGE('',*,*,#7847,.F.);
#10591=ORIENTED_EDGE('',*,*,#7848,.T.);
#10592=ORIENTED_EDGE('',*,*,#7849,.T.);
#10593=ORIENTED_EDGE('',*,*,#7845,.F.);
#10594=ORIENTED_EDGE('',*,*,#7850,.F.);
#10595=ORIENTED_EDGE('',*,*,#7851,.T.);
#10596=ORIENTED_EDGE('',*,*,#7852,.T.);
#10597=ORIENTED_EDGE('',*,*,#7848,.F.);
#10598=ORIENTED_EDGE('',*,*,#7853,.F.);
#10599=ORIENTED_EDGE('',*,*,#7854,.T.);
#10600=ORIENTED_EDGE('',*,*,#7855,.T.);
#10601=ORIENTED_EDGE('',*,*,#7851,.F.);
#10602=ORIENTED_EDGE('',*,*,#7856,.F.);
#10603=ORIENTED_EDGE('',*,*,#7857,.T.);
#10604=ORIENTED_EDGE('',*,*,#7858,.T.);
#10605=ORIENTED_EDGE('',*,*,#7854,.F.);
#10606=ORIENTED_EDGE('',*,*,#7859,.F.);
#10607=ORIENTED_EDGE('',*,*,#7860,.T.);
#10608=ORIENTED_EDGE('',*,*,#7861,.T.);
#10609=ORIENTED_EDGE('',*,*,#7857,.F.);
#10610=ORIENTED_EDGE('',*,*,#7862,.F.);
#10611=ORIENTED_EDGE('',*,*,#7863,.T.);
#10612=ORIENTED_EDGE('',*,*,#7864,.T.);
#10613=ORIENTED_EDGE('',*,*,#7860,.F.);
#10614=ORIENTED_EDGE('',*,*,#7865,.F.);
#10615=ORIENTED_EDGE('',*,*,#7866,.T.);
#10616=ORIENTED_EDGE('',*,*,#7867,.T.);
#10617=ORIENTED_EDGE('',*,*,#7863,.F.);
#10618=ORIENTED_EDGE('',*,*,#7868,.F.);
#10619=ORIENTED_EDGE('',*,*,#7869,.T.);
#10620=ORIENTED_EDGE('',*,*,#7870,.T.);
#10621=ORIENTED_EDGE('',*,*,#7866,.F.);
#10622=ORIENTED_EDGE('',*,*,#7871,.F.);
#10623=ORIENTED_EDGE('',*,*,#7872,.F.);
#10624=ORIENTED_EDGE('',*,*,#7873,.F.);
#10625=ORIENTED_EDGE('',*,*,#7874,.F.);
#10626=ORIENTED_EDGE('',*,*,#7875,.T.);
#10627=ORIENTED_EDGE('',*,*,#7631,.F.);
#10628=ORIENTED_EDGE('',*,*,#7876,.T.);
#10629=ORIENTED_EDGE('',*,*,#7756,.T.);
#10630=ORIENTED_EDGE('',*,*,#7877,.T.);
#10631=ORIENTED_EDGE('',*,*,#7634,.F.);
#10632=ORIENTED_EDGE('',*,*,#7872,.T.);
#10633=ORIENTED_EDGE('',*,*,#7878,.T.);
#10634=ORIENTED_EDGE('',*,*,#7869,.F.);
#10635=ORIENTED_EDGE('',*,*,#7879,.F.);
#10636=ORIENTED_EDGE('',*,*,#7877,.F.);
#10637=ORIENTED_EDGE('',*,*,#7755,.F.);
#10638=ORIENTED_EDGE('',*,*,#7759,.F.);
#10639=ORIENTED_EDGE('',*,*,#7762,.F.);
#10640=ORIENTED_EDGE('',*,*,#7765,.F.);
#10641=ORIENTED_EDGE('',*,*,#7768,.F.);
#10642=ORIENTED_EDGE('',*,*,#7771,.F.);
#10643=ORIENTED_EDGE('',*,*,#7774,.F.);
#10644=ORIENTED_EDGE('',*,*,#7777,.F.);
#10645=ORIENTED_EDGE('',*,*,#7780,.F.);
#10646=ORIENTED_EDGE('',*,*,#7783,.F.);
#10647=ORIENTED_EDGE('',*,*,#7786,.F.);
#10648=ORIENTED_EDGE('',*,*,#7789,.F.);
#10649=ORIENTED_EDGE('',*,*,#7792,.F.);
#10650=ORIENTED_EDGE('',*,*,#7795,.F.);
#10651=ORIENTED_EDGE('',*,*,#7798,.F.);
#10652=ORIENTED_EDGE('',*,*,#7801,.F.);
#10653=ORIENTED_EDGE('',*,*,#7804,.F.);
#10654=ORIENTED_EDGE('',*,*,#7807,.F.);
#10655=ORIENTED_EDGE('',*,*,#7810,.F.);
#10656=ORIENTED_EDGE('',*,*,#7813,.F.);
#10657=ORIENTED_EDGE('',*,*,#7816,.F.);
#10658=ORIENTED_EDGE('',*,*,#7819,.F.);
#10659=ORIENTED_EDGE('',*,*,#7822,.F.);
#10660=ORIENTED_EDGE('',*,*,#7825,.F.);
#10661=ORIENTED_EDGE('',*,*,#7828,.F.);
#10662=ORIENTED_EDGE('',*,*,#7831,.F.);
#10663=ORIENTED_EDGE('',*,*,#7834,.F.);
#10664=ORIENTED_EDGE('',*,*,#7837,.F.);
#10665=ORIENTED_EDGE('',*,*,#7840,.F.);
#10666=ORIENTED_EDGE('',*,*,#7843,.F.);
#10667=ORIENTED_EDGE('',*,*,#7846,.F.);
#10668=ORIENTED_EDGE('',*,*,#7849,.F.);
#10669=ORIENTED_EDGE('',*,*,#7852,.F.);
#10670=ORIENTED_EDGE('',*,*,#7855,.F.);
#10671=ORIENTED_EDGE('',*,*,#7858,.F.);
#10672=ORIENTED_EDGE('',*,*,#7861,.F.);
#10673=ORIENTED_EDGE('',*,*,#7864,.F.);
#10674=ORIENTED_EDGE('',*,*,#7867,.F.);
#10675=ORIENTED_EDGE('',*,*,#7870,.F.);
#10676=ORIENTED_EDGE('',*,*,#7878,.F.);
#10677=ORIENTED_EDGE('',*,*,#7875,.F.);
#10678=ORIENTED_EDGE('',*,*,#7880,.F.);
#10679=ORIENTED_EDGE('',*,*,#7751,.F.);
#10680=ORIENTED_EDGE('',*,*,#7881,.F.);
#10681=ORIENTED_EDGE('',*,*,#7749,.F.);
#10682=ORIENTED_EDGE('',*,*,#7746,.F.);
#10683=ORIENTED_EDGE('',*,*,#7743,.F.);
#10684=ORIENTED_EDGE('',*,*,#7740,.F.);
#10685=ORIENTED_EDGE('',*,*,#7737,.F.);
#10686=ORIENTED_EDGE('',*,*,#7734,.F.);
#10687=ORIENTED_EDGE('',*,*,#7731,.F.);
#10688=ORIENTED_EDGE('',*,*,#7728,.F.);
#10689=ORIENTED_EDGE('',*,*,#7725,.F.);
#10690=ORIENTED_EDGE('',*,*,#7722,.F.);
#10691=ORIENTED_EDGE('',*,*,#7719,.F.);
#10692=ORIENTED_EDGE('',*,*,#7716,.F.);
#10693=ORIENTED_EDGE('',*,*,#7713,.F.);
#10694=ORIENTED_EDGE('',*,*,#7710,.F.);
#10695=ORIENTED_EDGE('',*,*,#7707,.F.);
#10696=ORIENTED_EDGE('',*,*,#7704,.F.);
#10697=ORIENTED_EDGE('',*,*,#7701,.F.);
#10698=ORIENTED_EDGE('',*,*,#7698,.F.);
#10699=ORIENTED_EDGE('',*,*,#7695,.F.);
#10700=ORIENTED_EDGE('',*,*,#7692,.F.);
#10701=ORIENTED_EDGE('',*,*,#7689,.F.);
#10702=ORIENTED_EDGE('',*,*,#7686,.F.);
#10703=ORIENTED_EDGE('',*,*,#7683,.F.);
#10704=ORIENTED_EDGE('',*,*,#7680,.F.);
#10705=ORIENTED_EDGE('',*,*,#7677,.F.);
#10706=ORIENTED_EDGE('',*,*,#7674,.F.);
#10707=ORIENTED_EDGE('',*,*,#7671,.F.);
#10708=ORIENTED_EDGE('',*,*,#7668,.F.);
#10709=ORIENTED_EDGE('',*,*,#7665,.F.);
#10710=ORIENTED_EDGE('',*,*,#7662,.F.);
#10711=ORIENTED_EDGE('',*,*,#7659,.F.);
#10712=ORIENTED_EDGE('',*,*,#7656,.F.);
#10713=ORIENTED_EDGE('',*,*,#7653,.F.);
#10714=ORIENTED_EDGE('',*,*,#7650,.F.);
#10715=ORIENTED_EDGE('',*,*,#7647,.F.);
#10716=ORIENTED_EDGE('',*,*,#7644,.F.);
#10717=ORIENTED_EDGE('',*,*,#7641,.F.);
#10718=ORIENTED_EDGE('',*,*,#7638,.F.);
#10719=ORIENTED_EDGE('',*,*,#7635,.F.);
#10720=ORIENTED_EDGE('',*,*,#7876,.F.);
#10721=ORIENTED_EDGE('',*,*,#7630,.F.);
#10722=ORIENTED_EDGE('',*,*,#7637,.F.);
#10723=ORIENTED_EDGE('',*,*,#7640,.F.);
#10724=ORIENTED_EDGE('',*,*,#7643,.F.);
#10725=ORIENTED_EDGE('',*,*,#7646,.F.);
#10726=ORIENTED_EDGE('',*,*,#7649,.F.);
#10727=ORIENTED_EDGE('',*,*,#7652,.F.);
#10728=ORIENTED_EDGE('',*,*,#7655,.F.);
#10729=ORIENTED_EDGE('',*,*,#7658,.F.);
#10730=ORIENTED_EDGE('',*,*,#7661,.F.);
#10731=ORIENTED_EDGE('',*,*,#7664,.F.);
#10732=ORIENTED_EDGE('',*,*,#7667,.F.);
#10733=ORIENTED_EDGE('',*,*,#7670,.F.);
#10734=ORIENTED_EDGE('',*,*,#7673,.F.);
#10735=ORIENTED_EDGE('',*,*,#7676,.F.);
#10736=ORIENTED_EDGE('',*,*,#7679,.F.);
#10737=ORIENTED_EDGE('',*,*,#7682,.F.);
#10738=ORIENTED_EDGE('',*,*,#7685,.F.);
#10739=ORIENTED_EDGE('',*,*,#7688,.F.);
#10740=ORIENTED_EDGE('',*,*,#7691,.F.);
#10741=ORIENTED_EDGE('',*,*,#7694,.F.);
#10742=ORIENTED_EDGE('',*,*,#7697,.F.);
#10743=ORIENTED_EDGE('',*,*,#7700,.F.);
#10744=ORIENTED_EDGE('',*,*,#7703,.F.);
#10745=ORIENTED_EDGE('',*,*,#7706,.F.);
#10746=ORIENTED_EDGE('',*,*,#7709,.F.);
#10747=ORIENTED_EDGE('',*,*,#7712,.F.);
#10748=ORIENTED_EDGE('',*,*,#7715,.F.);
#10749=ORIENTED_EDGE('',*,*,#7718,.F.);
#10750=ORIENTED_EDGE('',*,*,#7721,.F.);
#10751=ORIENTED_EDGE('',*,*,#7724,.F.);
#10752=ORIENTED_EDGE('',*,*,#7727,.F.);
#10753=ORIENTED_EDGE('',*,*,#7730,.F.);
#10754=ORIENTED_EDGE('',*,*,#7733,.F.);
#10755=ORIENTED_EDGE('',*,*,#7736,.F.);
#10756=ORIENTED_EDGE('',*,*,#7739,.F.);
#10757=ORIENTED_EDGE('',*,*,#7742,.F.);
#10758=ORIENTED_EDGE('',*,*,#7745,.F.);
#10759=ORIENTED_EDGE('',*,*,#7748,.F.);
#10760=ORIENTED_EDGE('',*,*,#7882,.F.);
#10761=ORIENTED_EDGE('',*,*,#7753,.F.);
#10762=ORIENTED_EDGE('',*,*,#7883,.F.);
#10763=ORIENTED_EDGE('',*,*,#7873,.T.);
#10764=ORIENTED_EDGE('',*,*,#7879,.T.);
#10765=ORIENTED_EDGE('',*,*,#7871,.T.);
#10766=ORIENTED_EDGE('',*,*,#7868,.T.);
#10767=ORIENTED_EDGE('',*,*,#7865,.T.);
#10768=ORIENTED_EDGE('',*,*,#7862,.T.);
#10769=ORIENTED_EDGE('',*,*,#7859,.T.);
#10770=ORIENTED_EDGE('',*,*,#7856,.T.);
#10771=ORIENTED_EDGE('',*,*,#7853,.T.);
#10772=ORIENTED_EDGE('',*,*,#7850,.T.);
#10773=ORIENTED_EDGE('',*,*,#7847,.T.);
#10774=ORIENTED_EDGE('',*,*,#7844,.T.);
#10775=ORIENTED_EDGE('',*,*,#7841,.T.);
#10776=ORIENTED_EDGE('',*,*,#7838,.T.);
#10777=ORIENTED_EDGE('',*,*,#7835,.T.);
#10778=ORIENTED_EDGE('',*,*,#7832,.T.);
#10779=ORIENTED_EDGE('',*,*,#7829,.T.);
#10780=ORIENTED_EDGE('',*,*,#7826,.T.);
#10781=ORIENTED_EDGE('',*,*,#7823,.T.);
#10782=ORIENTED_EDGE('',*,*,#7820,.T.);
#10783=ORIENTED_EDGE('',*,*,#7817,.T.);
#10784=ORIENTED_EDGE('',*,*,#7814,.T.);
#10785=ORIENTED_EDGE('',*,*,#7811,.T.);
#10786=ORIENTED_EDGE('',*,*,#7808,.T.);
#10787=ORIENTED_EDGE('',*,*,#7805,.T.);
#10788=ORIENTED_EDGE('',*,*,#7802,.T.);
#10789=ORIENTED_EDGE('',*,*,#7799,.T.);
#10790=ORIENTED_EDGE('',*,*,#7796,.T.);
#10791=ORIENTED_EDGE('',*,*,#7793,.T.);
#10792=ORIENTED_EDGE('',*,*,#7790,.T.);
#10793=ORIENTED_EDGE('',*,*,#7787,.T.);
#10794=ORIENTED_EDGE('',*,*,#7784,.T.);
#10795=ORIENTED_EDGE('',*,*,#7781,.T.);
#10796=ORIENTED_EDGE('',*,*,#7778,.T.);
#10797=ORIENTED_EDGE('',*,*,#7775,.T.);
#10798=ORIENTED_EDGE('',*,*,#7772,.T.);
#10799=ORIENTED_EDGE('',*,*,#7769,.T.);
#10800=ORIENTED_EDGE('',*,*,#7766,.T.);
#10801=ORIENTED_EDGE('',*,*,#7763,.T.);
#10802=ORIENTED_EDGE('',*,*,#7760,.T.);
#10803=ORIENTED_EDGE('',*,*,#7757,.T.);
#10804=ORIENTED_EDGE('',*,*,#7750,.T.);
#10805=ORIENTED_EDGE('',*,*,#7882,.T.);
#10806=ORIENTED_EDGE('',*,*,#7747,.F.);
#10807=ORIENTED_EDGE('',*,*,#7881,.T.);
#10808=ORIENTED_EDGE('',*,*,#7633,.F.);
#10809=ORIENTED_EDGE('',*,*,#7884,.F.);
#10810=ORIENTED_EDGE('',*,*,#7474,.F.);
#10811=ORIENTED_EDGE('',*,*,#7885,.T.);
#10812=ORIENTED_EDGE('',*,*,#7554,.T.);
#10813=ORIENTED_EDGE('',*,*,#7886,.T.);
#10814=ORIENTED_EDGE('',*,*,#7477,.F.);
#10815=ORIENTED_EDGE('',*,*,#7625,.T.);
#10816=ORIENTED_EDGE('',*,*,#7887,.T.);
#10817=ORIENTED_EDGE('',*,*,#7622,.F.);
#10818=ORIENTED_EDGE('',*,*,#7888,.F.);
#10819=ORIENTED_EDGE('',*,*,#7886,.F.);
#10820=ORIENTED_EDGE('',*,*,#7553,.F.);
#10821=ORIENTED_EDGE('',*,*,#7557,.F.);
#10822=ORIENTED_EDGE('',*,*,#7560,.F.);
#10823=ORIENTED_EDGE('',*,*,#7563,.F.);
#10824=ORIENTED_EDGE('',*,*,#7566,.F.);
#10825=ORIENTED_EDGE('',*,*,#7569,.F.);
#10826=ORIENTED_EDGE('',*,*,#7572,.F.);
#10827=ORIENTED_EDGE('',*,*,#7575,.F.);
#10828=ORIENTED_EDGE('',*,*,#7578,.F.);
#10829=ORIENTED_EDGE('',*,*,#7581,.F.);
#10830=ORIENTED_EDGE('',*,*,#7584,.F.);
#10831=ORIENTED_EDGE('',*,*,#7587,.F.);
#10832=ORIENTED_EDGE('',*,*,#7590,.F.);
#10833=ORIENTED_EDGE('',*,*,#7593,.F.);
#10834=ORIENTED_EDGE('',*,*,#7596,.F.);
#10835=ORIENTED_EDGE('',*,*,#7599,.F.);
#10836=ORIENTED_EDGE('',*,*,#7602,.F.);
#10837=ORIENTED_EDGE('',*,*,#7605,.F.);
#10838=ORIENTED_EDGE('',*,*,#7608,.F.);
#10839=ORIENTED_EDGE('',*,*,#7611,.F.);
#10840=ORIENTED_EDGE('',*,*,#7614,.F.);
#10841=ORIENTED_EDGE('',*,*,#7617,.F.);
#10842=ORIENTED_EDGE('',*,*,#7620,.F.);
#10843=ORIENTED_EDGE('',*,*,#7623,.F.);
#10844=ORIENTED_EDGE('',*,*,#7887,.F.);
#10845=ORIENTED_EDGE('',*,*,#7628,.F.);
#10846=ORIENTED_EDGE('',*,*,#7889,.F.);
#10847=ORIENTED_EDGE('',*,*,#7549,.F.);
#10848=ORIENTED_EDGE('',*,*,#7890,.F.);
#10849=ORIENTED_EDGE('',*,*,#7547,.F.);
#10850=ORIENTED_EDGE('',*,*,#7544,.F.);
#10851=ORIENTED_EDGE('',*,*,#7541,.F.);
#10852=ORIENTED_EDGE('',*,*,#7538,.F.);
#10853=ORIENTED_EDGE('',*,*,#7535,.F.);
#10854=ORIENTED_EDGE('',*,*,#7532,.F.);
#10855=ORIENTED_EDGE('',*,*,#7529,.F.);
#10856=ORIENTED_EDGE('',*,*,#7526,.F.);
#10857=ORIENTED_EDGE('',*,*,#7523,.F.);
#10858=ORIENTED_EDGE('',*,*,#7520,.F.);
#10859=ORIENTED_EDGE('',*,*,#7517,.F.);
#10860=ORIENTED_EDGE('',*,*,#7514,.F.);
#10861=ORIENTED_EDGE('',*,*,#7511,.F.);
#10862=ORIENTED_EDGE('',*,*,#7508,.F.);
#10863=ORIENTED_EDGE('',*,*,#7505,.F.);
#10864=ORIENTED_EDGE('',*,*,#7502,.F.);
#10865=ORIENTED_EDGE('',*,*,#7499,.F.);
#10866=ORIENTED_EDGE('',*,*,#7496,.F.);
#10867=ORIENTED_EDGE('',*,*,#7493,.F.);
#10868=ORIENTED_EDGE('',*,*,#7490,.F.);
#10869=ORIENTED_EDGE('',*,*,#7487,.F.);
#10870=ORIENTED_EDGE('',*,*,#7484,.F.);
#10871=ORIENTED_EDGE('',*,*,#7481,.F.);
#10872=ORIENTED_EDGE('',*,*,#7478,.F.);
#10873=ORIENTED_EDGE('',*,*,#7885,.F.);
#10874=ORIENTED_EDGE('',*,*,#7473,.F.);
#10875=ORIENTED_EDGE('',*,*,#7480,.F.);
#10876=ORIENTED_EDGE('',*,*,#7483,.F.);
#10877=ORIENTED_EDGE('',*,*,#7486,.F.);
#10878=ORIENTED_EDGE('',*,*,#7489,.F.);
#10879=ORIENTED_EDGE('',*,*,#7492,.F.);
#10880=ORIENTED_EDGE('',*,*,#7495,.F.);
#10881=ORIENTED_EDGE('',*,*,#7498,.F.);
#10882=ORIENTED_EDGE('',*,*,#7501,.F.);
#10883=ORIENTED_EDGE('',*,*,#7504,.F.);
#10884=ORIENTED_EDGE('',*,*,#7507,.F.);
#10885=ORIENTED_EDGE('',*,*,#7510,.F.);
#10886=ORIENTED_EDGE('',*,*,#7513,.F.);
#10887=ORIENTED_EDGE('',*,*,#7516,.F.);
#10888=ORIENTED_EDGE('',*,*,#7519,.F.);
#10889=ORIENTED_EDGE('',*,*,#7522,.F.);
#10890=ORIENTED_EDGE('',*,*,#7525,.F.);
#10891=ORIENTED_EDGE('',*,*,#7528,.F.);
#10892=ORIENTED_EDGE('',*,*,#7531,.F.);
#10893=ORIENTED_EDGE('',*,*,#7534,.F.);
#10894=ORIENTED_EDGE('',*,*,#7537,.F.);
#10895=ORIENTED_EDGE('',*,*,#7540,.F.);
#10896=ORIENTED_EDGE('',*,*,#7543,.F.);
#10897=ORIENTED_EDGE('',*,*,#7546,.F.);
#10898=ORIENTED_EDGE('',*,*,#7891,.F.);
#10899=ORIENTED_EDGE('',*,*,#7551,.F.);
#10900=ORIENTED_EDGE('',*,*,#7892,.F.);
#10901=ORIENTED_EDGE('',*,*,#7626,.T.);
#10902=ORIENTED_EDGE('',*,*,#7888,.T.);
#10903=ORIENTED_EDGE('',*,*,#7624,.T.);
#10904=ORIENTED_EDGE('',*,*,#7621,.T.);
#10905=ORIENTED_EDGE('',*,*,#7618,.T.);
#10906=ORIENTED_EDGE('',*,*,#7615,.T.);
#10907=ORIENTED_EDGE('',*,*,#7612,.T.);
#10908=ORIENTED_EDGE('',*,*,#7609,.T.);
#10909=ORIENTED_EDGE('',*,*,#7606,.T.);
#10910=ORIENTED_EDGE('',*,*,#7603,.T.);
#10911=ORIENTED_EDGE('',*,*,#7600,.T.);
#10912=ORIENTED_EDGE('',*,*,#7597,.T.);
#10913=ORIENTED_EDGE('',*,*,#7594,.T.);
#10914=ORIENTED_EDGE('',*,*,#7591,.T.);
#10915=ORIENTED_EDGE('',*,*,#7588,.T.);
#10916=ORIENTED_EDGE('',*,*,#7585,.T.);
#10917=ORIENTED_EDGE('',*,*,#7582,.T.);
#10918=ORIENTED_EDGE('',*,*,#7579,.T.);
#10919=ORIENTED_EDGE('',*,*,#7576,.T.);
#10920=ORIENTED_EDGE('',*,*,#7573,.T.);
#10921=ORIENTED_EDGE('',*,*,#7570,.T.);
#10922=ORIENTED_EDGE('',*,*,#7567,.T.);
#10923=ORIENTED_EDGE('',*,*,#7564,.T.);
#10924=ORIENTED_EDGE('',*,*,#7561,.T.);
#10925=ORIENTED_EDGE('',*,*,#7558,.T.);
#10926=ORIENTED_EDGE('',*,*,#7555,.T.);
#10927=ORIENTED_EDGE('',*,*,#7548,.T.);
#10928=ORIENTED_EDGE('',*,*,#7891,.T.);
#10929=ORIENTED_EDGE('',*,*,#7545,.F.);
#10930=ORIENTED_EDGE('',*,*,#7890,.T.);
#10931=ORIENTED_EDGE('',*,*,#7476,.F.);
#10932=ORIENTED_EDGE('',*,*,#7893,.F.);
#10933=ORIENTED_EDGE('',*,*,#7894,.T.);
#10934=ORIENTED_EDGE('',*,*,#7895,.T.);
#10935=ORIENTED_EDGE('',*,*,#7896,.T.);
#10936=ORIENTED_EDGE('',*,*,#7897,.T.);
#10937=ORIENTED_EDGE('',*,*,#7895,.F.);
#10938=ORIENTED_EDGE('',*,*,#7898,.F.);
#10939=ORIENTED_EDGE('',*,*,#7899,.F.);
#10940=ORIENTED_EDGE('',*,*,#7900,.F.);
#10941=ORIENTED_EDGE('',*,*,#7894,.F.);
#10942=ORIENTED_EDGE('',*,*,#7901,.T.);
#10943=ORIENTED_EDGE('',*,*,#7902,.F.);
#10944=ORIENTED_EDGE('',*,*,#7903,.T.);
#10945=ORIENTED_EDGE('',*,*,#7904,.F.);
#10946=ORIENTED_EDGE('',*,*,#7905,.T.);
#10947=ORIENTED_EDGE('',*,*,#7906,.F.);
#10948=ORIENTED_EDGE('',*,*,#7907,.T.);
#10949=ORIENTED_EDGE('',*,*,#7908,.F.);
#10950=ORIENTED_EDGE('',*,*,#7909,.T.);
#10951=ORIENTED_EDGE('',*,*,#7910,.F.);
#10952=ORIENTED_EDGE('',*,*,#7911,.T.);
#10953=ORIENTED_EDGE('',*,*,#7912,.F.);
#10954=ORIENTED_EDGE('',*,*,#7913,.T.);
#10955=ORIENTED_EDGE('',*,*,#7914,.F.);
#10956=ORIENTED_EDGE('',*,*,#7915,.T.);
#10957=ORIENTED_EDGE('',*,*,#7916,.F.);
#10958=ORIENTED_EDGE('',*,*,#7917,.T.);
#10959=ORIENTED_EDGE('',*,*,#7918,.F.);
#10960=ORIENTED_EDGE('',*,*,#7919,.T.);
#10961=ORIENTED_EDGE('',*,*,#7920,.F.);
#10962=ORIENTED_EDGE('',*,*,#7921,.T.);
#10963=ORIENTED_EDGE('',*,*,#7922,.F.);
#10964=ORIENTED_EDGE('',*,*,#7923,.T.);
#10965=ORIENTED_EDGE('',*,*,#7924,.F.);
#10966=ORIENTED_EDGE('',*,*,#7925,.T.);
#10967=ORIENTED_EDGE('',*,*,#7926,.F.);
#10968=ORIENTED_EDGE('',*,*,#7927,.T.);
#10969=ORIENTED_EDGE('',*,*,#7928,.F.);
#10970=ORIENTED_EDGE('',*,*,#7929,.T.);
#10971=ORIENTED_EDGE('',*,*,#7930,.F.);
#10972=ORIENTED_EDGE('',*,*,#7931,.T.);
#10973=ORIENTED_EDGE('',*,*,#7932,.F.);
#10974=ORIENTED_EDGE('',*,*,#7933,.T.);
#10975=ORIENTED_EDGE('',*,*,#7934,.F.);
#10976=ORIENTED_EDGE('',*,*,#7935,.T.);
#10977=ORIENTED_EDGE('',*,*,#7936,.F.);
#10978=ORIENTED_EDGE('',*,*,#7937,.T.);
#10979=ORIENTED_EDGE('',*,*,#7938,.F.);
#10980=ORIENTED_EDGE('',*,*,#7939,.T.);
#10981=ORIENTED_EDGE('',*,*,#7940,.F.);
#10982=ORIENTED_EDGE('',*,*,#7941,.T.);
#10983=ORIENTED_EDGE('',*,*,#7942,.F.);
#10984=ORIENTED_EDGE('',*,*,#7943,.T.);
#10985=ORIENTED_EDGE('',*,*,#7944,.F.);
#10986=ORIENTED_EDGE('',*,*,#7945,.T.);
#10987=ORIENTED_EDGE('',*,*,#7946,.F.);
#10988=ORIENTED_EDGE('',*,*,#7947,.T.);
#10989=ORIENTED_EDGE('',*,*,#7948,.F.);
#10990=ORIENTED_EDGE('',*,*,#7949,.T.);
#10991=ORIENTED_EDGE('',*,*,#7950,.F.);
#10992=ORIENTED_EDGE('',*,*,#7951,.T.);
#10993=ORIENTED_EDGE('',*,*,#7952,.F.);
#10994=ORIENTED_EDGE('',*,*,#7953,.T.);
#10995=ORIENTED_EDGE('',*,*,#7954,.F.);
#10996=ORIENTED_EDGE('',*,*,#7955,.T.);
#10997=ORIENTED_EDGE('',*,*,#7956,.F.);
#10998=ORIENTED_EDGE('',*,*,#7957,.T.);
#10999=ORIENTED_EDGE('',*,*,#7958,.F.);
#11000=ORIENTED_EDGE('',*,*,#7959,.T.);
#11001=ORIENTED_EDGE('',*,*,#7960,.F.);
#11002=ORIENTED_EDGE('',*,*,#7961,.T.);
#11003=ORIENTED_EDGE('',*,*,#7962,.F.);
#11004=ORIENTED_EDGE('',*,*,#7963,.T.);
#11005=ORIENTED_EDGE('',*,*,#7964,.F.);
#11006=ORIENTED_EDGE('',*,*,#7965,.T.);
#11007=ORIENTED_EDGE('',*,*,#7966,.F.);
#11008=ORIENTED_EDGE('',*,*,#7967,.T.);
#11009=ORIENTED_EDGE('',*,*,#7968,.F.);
#11010=ORIENTED_EDGE('',*,*,#7969,.T.);
#11011=ORIENTED_EDGE('',*,*,#7970,.F.);
#11012=ORIENTED_EDGE('',*,*,#7898,.T.);
#11013=ORIENTED_EDGE('',*,*,#7892,.T.);
#11014=ORIENTED_EDGE('',*,*,#7550,.T.);
#11015=ORIENTED_EDGE('',*,*,#7889,.T.);
#11016=ORIENTED_EDGE('',*,*,#7627,.T.);
#11017=ORIENTED_EDGE('',*,*,#7971,.T.);
#11018=ORIENTED_EDGE('',*,*,#7972,.T.);
#11019=ORIENTED_EDGE('',*,*,#7973,.T.);
#11020=ORIENTED_EDGE('',*,*,#7974,.T.);
#11021=ORIENTED_EDGE('',*,*,#7975,.T.);
#11022=ORIENTED_EDGE('',*,*,#7976,.T.);
#11023=ORIENTED_EDGE('',*,*,#7902,.T.);
#11024=ORIENTED_EDGE('',*,*,#7977,.T.);
#11025=ORIENTED_EDGE('',*,*,#7976,.F.);
#11026=ORIENTED_EDGE('',*,*,#7978,.F.);
#11027=ORIENTED_EDGE('',*,*,#7979,.F.);
#11028=ORIENTED_EDGE('',*,*,#7903,.F.);
#11029=ORIENTED_EDGE('',*,*,#7980,.T.);
#11030=ORIENTED_EDGE('',*,*,#7981,.T.);
#11031=ORIENTED_EDGE('',*,*,#7904,.T.);
#11032=ORIENTED_EDGE('',*,*,#7979,.T.);
#11033=ORIENTED_EDGE('',*,*,#7981,.F.);
#11034=ORIENTED_EDGE('',*,*,#7982,.F.);
#11035=ORIENTED_EDGE('',*,*,#7983,.F.);
#11036=ORIENTED_EDGE('',*,*,#7905,.F.);
#11037=ORIENTED_EDGE('',*,*,#7984,.T.);
#11038=ORIENTED_EDGE('',*,*,#7985,.T.);
#11039=ORIENTED_EDGE('',*,*,#7906,.T.);
#11040=ORIENTED_EDGE('',*,*,#7983,.T.);
#11041=ORIENTED_EDGE('',*,*,#7985,.F.);
#11042=ORIENTED_EDGE('',*,*,#7986,.F.);
#11043=ORIENTED_EDGE('',*,*,#7987,.F.);
#11044=ORIENTED_EDGE('',*,*,#7907,.F.);
#11045=ORIENTED_EDGE('',*,*,#7988,.T.);
#11046=ORIENTED_EDGE('',*,*,#7989,.T.);
#11047=ORIENTED_EDGE('',*,*,#7908,.T.);
#11048=ORIENTED_EDGE('',*,*,#7987,.T.);
#11049=ORIENTED_EDGE('',*,*,#7989,.F.);
#11050=ORIENTED_EDGE('',*,*,#7990,.F.);
#11051=ORIENTED_EDGE('',*,*,#7991,.F.);
#11052=ORIENTED_EDGE('',*,*,#7909,.F.);
#11053=ORIENTED_EDGE('',*,*,#7910,.T.);
#11054=ORIENTED_EDGE('',*,*,#7991,.T.);
#11055=ORIENTED_EDGE('',*,*,#7992,.T.);
#11056=ORIENTED_EDGE('',*,*,#7993,.T.);
#11057=ORIENTED_EDGE('',*,*,#7912,.T.);
#11058=ORIENTED_EDGE('',*,*,#7994,.T.);
#11059=ORIENTED_EDGE('',*,*,#7995,.T.);
#11060=ORIENTED_EDGE('',*,*,#7996,.T.);
#11061=ORIENTED_EDGE('',*,*,#7996,.F.);
#11062=ORIENTED_EDGE('',*,*,#7997,.F.);
#11063=ORIENTED_EDGE('',*,*,#7998,.F.);
#11064=ORIENTED_EDGE('',*,*,#7913,.F.);
#11065=ORIENTED_EDGE('',*,*,#7914,.T.);
#11066=ORIENTED_EDGE('',*,*,#7998,.T.);
#11067=ORIENTED_EDGE('',*,*,#7999,.T.);
#11068=ORIENTED_EDGE('',*,*,#8000,.T.);
#11069=ORIENTED_EDGE('',*,*,#7916,.T.);
#11070=ORIENTED_EDGE('',*,*,#8001,.T.);
#11071=ORIENTED_EDGE('',*,*,#8002,.T.);
#11072=ORIENTED_EDGE('',*,*,#8003,.T.);
#11073=ORIENTED_EDGE('',*,*,#8003,.F.);
#11074=ORIENTED_EDGE('',*,*,#8004,.F.);
#11075=ORIENTED_EDGE('',*,*,#8005,.F.);
#11076=ORIENTED_EDGE('',*,*,#7917,.F.);
#11077=ORIENTED_EDGE('',*,*,#7918,.T.);
#11078=ORIENTED_EDGE('',*,*,#8005,.T.);
#11079=ORIENTED_EDGE('',*,*,#8006,.T.);
#11080=ORIENTED_EDGE('',*,*,#8007,.T.);
#11081=ORIENTED_EDGE('',*,*,#8008,.T.);
#11082=ORIENTED_EDGE('',*,*,#8009,.T.);
#11083=ORIENTED_EDGE('',*,*,#7920,.T.);
#11084=ORIENTED_EDGE('',*,*,#8010,.T.);
#11085=ORIENTED_EDGE('',*,*,#8009,.F.);
#11086=ORIENTED_EDGE('',*,*,#8011,.F.);
#11087=ORIENTED_EDGE('',*,*,#8012,.F.);
#11088=ORIENTED_EDGE('',*,*,#7921,.F.);
#11089=ORIENTED_EDGE('',*,*,#8013,.T.);
#11090=ORIENTED_EDGE('',*,*,#8014,.T.);
#11091=ORIENTED_EDGE('',*,*,#7922,.T.);
#11092=ORIENTED_EDGE('',*,*,#8012,.T.);
#11093=ORIENTED_EDGE('',*,*,#8014,.F.);
#11094=ORIENTED_EDGE('',*,*,#8015,.F.);
#11095=ORIENTED_EDGE('',*,*,#8016,.F.);
#11096=ORIENTED_EDGE('',*,*,#7923,.F.);
#11097=ORIENTED_EDGE('',*,*,#8017,.T.);
#11098=ORIENTED_EDGE('',*,*,#8018,.T.);
#11099=ORIENTED_EDGE('',*,*,#7924,.T.);
#11100=ORIENTED_EDGE('',*,*,#8016,.T.);
#11101=ORIENTED_EDGE('',*,*,#8018,.F.);
#11102=ORIENTED_EDGE('',*,*,#8019,.F.);
#11103=ORIENTED_EDGE('',*,*,#8020,.F.);
#11104=ORIENTED_EDGE('',*,*,#7925,.F.);
#11105=ORIENTED_EDGE('',*,*,#8021,.T.);
#11106=ORIENTED_EDGE('',*,*,#8022,.T.);
#11107=ORIENTED_EDGE('',*,*,#7926,.T.);
#11108=ORIENTED_EDGE('',*,*,#8020,.T.);
#11109=ORIENTED_EDGE('',*,*,#8022,.F.);
#11110=ORIENTED_EDGE('',*,*,#8023,.F.);
#11111=ORIENTED_EDGE('',*,*,#8024,.F.);
#11112=ORIENTED_EDGE('',*,*,#7927,.F.);
#11113=ORIENTED_EDGE('',*,*,#7928,.T.);
#11114=ORIENTED_EDGE('',*,*,#8024,.T.);
#11115=ORIENTED_EDGE('',*,*,#8025,.T.);
#11116=ORIENTED_EDGE('',*,*,#8026,.T.);
#11117=ORIENTED_EDGE('',*,*,#7930,.T.);
#11118=ORIENTED_EDGE('',*,*,#8027,.T.);
#11119=ORIENTED_EDGE('',*,*,#8028,.T.);
#11120=ORIENTED_EDGE('',*,*,#8029,.T.);
#11121=ORIENTED_EDGE('',*,*,#8029,.F.);
#11122=ORIENTED_EDGE('',*,*,#8030,.F.);
#11123=ORIENTED_EDGE('',*,*,#8031,.F.);
#11124=ORIENTED_EDGE('',*,*,#7931,.F.);
#11125=ORIENTED_EDGE('',*,*,#7932,.T.);
#11126=ORIENTED_EDGE('',*,*,#8031,.T.);
#11127=ORIENTED_EDGE('',*,*,#8032,.T.);
#11128=ORIENTED_EDGE('',*,*,#8033,.T.);
#11129=ORIENTED_EDGE('',*,*,#7934,.T.);
#11130=ORIENTED_EDGE('',*,*,#8034,.T.);
#11131=ORIENTED_EDGE('',*,*,#8035,.T.);
#11132=ORIENTED_EDGE('',*,*,#8036,.T.);
#11133=ORIENTED_EDGE('',*,*,#8036,.F.);
#11134=ORIENTED_EDGE('',*,*,#8037,.F.);
#11135=ORIENTED_EDGE('',*,*,#8038,.F.);
#11136=ORIENTED_EDGE('',*,*,#7935,.F.);
#11137=ORIENTED_EDGE('',*,*,#7936,.T.);
#11138=ORIENTED_EDGE('',*,*,#8038,.T.);
#11139=ORIENTED_EDGE('',*,*,#8039,.T.);
#11140=ORIENTED_EDGE('',*,*,#8040,.T.);
#11141=ORIENTED_EDGE('',*,*,#8041,.T.);
#11142=ORIENTED_EDGE('',*,*,#8042,.T.);
#11143=ORIENTED_EDGE('',*,*,#7938,.T.);
#11144=ORIENTED_EDGE('',*,*,#8043,.T.);
#11145=ORIENTED_EDGE('',*,*,#8042,.F.);
#11146=ORIENTED_EDGE('',*,*,#8044,.F.);
#11147=ORIENTED_EDGE('',*,*,#8045,.F.);
#11148=ORIENTED_EDGE('',*,*,#7939,.F.);
#11149=ORIENTED_EDGE('',*,*,#8046,.T.);
#11150=ORIENTED_EDGE('',*,*,#8047,.T.);
#11151=ORIENTED_EDGE('',*,*,#7940,.T.);
#11152=ORIENTED_EDGE('',*,*,#8045,.T.);
#11153=ORIENTED_EDGE('',*,*,#8047,.F.);
#11154=ORIENTED_EDGE('',*,*,#8048,.F.);
#11155=ORIENTED_EDGE('',*,*,#8049,.F.);
#11156=ORIENTED_EDGE('',*,*,#7941,.F.);
#11157=ORIENTED_EDGE('',*,*,#8050,.T.);
#11158=ORIENTED_EDGE('',*,*,#8051,.T.);
#11159=ORIENTED_EDGE('',*,*,#7942,.T.);
#11160=ORIENTED_EDGE('',*,*,#8049,.T.);
#11161=ORIENTED_EDGE('',*,*,#8051,.F.);
#11162=ORIENTED_EDGE('',*,*,#8052,.F.);
#11163=ORIENTED_EDGE('',*,*,#8053,.F.);
#11164=ORIENTED_EDGE('',*,*,#7943,.F.);
#11165=ORIENTED_EDGE('',*,*,#8054,.T.);
#11166=ORIENTED_EDGE('',*,*,#8055,.T.);
#11167=ORIENTED_EDGE('',*,*,#7944,.T.);
#11168=ORIENTED_EDGE('',*,*,#8053,.T.);
#11169=ORIENTED_EDGE('',*,*,#8055,.F.);
#11170=ORIENTED_EDGE('',*,*,#8056,.F.);
#11171=ORIENTED_EDGE('',*,*,#8057,.F.);
#11172=ORIENTED_EDGE('',*,*,#7945,.F.);
#11173=ORIENTED_EDGE('',*,*,#7946,.T.);
#11174=ORIENTED_EDGE('',*,*,#8057,.T.);
#11175=ORIENTED_EDGE('',*,*,#8058,.T.);
#11176=ORIENTED_EDGE('',*,*,#8059,.T.);
#11177=ORIENTED_EDGE('',*,*,#7948,.T.);
#11178=ORIENTED_EDGE('',*,*,#8060,.T.);
#11179=ORIENTED_EDGE('',*,*,#8061,.T.);
#11180=ORIENTED_EDGE('',*,*,#8062,.T.);
#11181=ORIENTED_EDGE('',*,*,#8062,.F.);
#11182=ORIENTED_EDGE('',*,*,#8063,.F.);
#11183=ORIENTED_EDGE('',*,*,#8064,.F.);
#11184=ORIENTED_EDGE('',*,*,#7949,.F.);
#11185=ORIENTED_EDGE('',*,*,#7950,.T.);
#11186=ORIENTED_EDGE('',*,*,#8064,.T.);
#11187=ORIENTED_EDGE('',*,*,#8065,.T.);
#11188=ORIENTED_EDGE('',*,*,#8066,.T.);
#11189=ORIENTED_EDGE('',*,*,#7952,.T.);
#11190=ORIENTED_EDGE('',*,*,#8067,.T.);
#11191=ORIENTED_EDGE('',*,*,#8068,.T.);
#11192=ORIENTED_EDGE('',*,*,#8069,.T.);
#11193=ORIENTED_EDGE('',*,*,#8069,.F.);
#11194=ORIENTED_EDGE('',*,*,#8070,.F.);
#11195=ORIENTED_EDGE('',*,*,#8071,.F.);
#11196=ORIENTED_EDGE('',*,*,#7953,.F.);
#11197=ORIENTED_EDGE('',*,*,#7954,.T.);
#11198=ORIENTED_EDGE('',*,*,#8071,.T.);
#11199=ORIENTED_EDGE('',*,*,#8072,.T.);
#11200=ORIENTED_EDGE('',*,*,#8073,.T.);
#11201=ORIENTED_EDGE('',*,*,#8074,.T.);
#11202=ORIENTED_EDGE('',*,*,#8075,.T.);
#11203=ORIENTED_EDGE('',*,*,#7956,.T.);
#11204=ORIENTED_EDGE('',*,*,#8076,.T.);
#11205=ORIENTED_EDGE('',*,*,#8075,.F.);
#11206=ORIENTED_EDGE('',*,*,#8077,.F.);
#11207=ORIENTED_EDGE('',*,*,#8078,.F.);
#11208=ORIENTED_EDGE('',*,*,#7957,.F.);
#11209=ORIENTED_EDGE('',*,*,#8079,.T.);
#11210=ORIENTED_EDGE('',*,*,#8080,.T.);
#11211=ORIENTED_EDGE('',*,*,#7958,.T.);
#11212=ORIENTED_EDGE('',*,*,#8078,.T.);
#11213=ORIENTED_EDGE('',*,*,#8080,.F.);
#11214=ORIENTED_EDGE('',*,*,#8081,.F.);
#11215=ORIENTED_EDGE('',*,*,#8082,.F.);
#11216=ORIENTED_EDGE('',*,*,#7959,.F.);
#11217=ORIENTED_EDGE('',*,*,#8083,.T.);
#11218=ORIENTED_EDGE('',*,*,#8084,.T.);
#11219=ORIENTED_EDGE('',*,*,#7960,.T.);
#11220=ORIENTED_EDGE('',*,*,#8082,.T.);
#11221=ORIENTED_EDGE('',*,*,#8084,.F.);
#11222=ORIENTED_EDGE('',*,*,#8085,.F.);
#11223=ORIENTED_EDGE('',*,*,#8086,.F.);
#11224=ORIENTED_EDGE('',*,*,#7961,.F.);
#11225=ORIENTED_EDGE('',*,*,#8087,.T.);
#11226=ORIENTED_EDGE('',*,*,#8088,.T.);
#11227=ORIENTED_EDGE('',*,*,#7962,.T.);
#11228=ORIENTED_EDGE('',*,*,#8086,.T.);
#11229=ORIENTED_EDGE('',*,*,#8088,.F.);
#11230=ORIENTED_EDGE('',*,*,#8089,.F.);
#11231=ORIENTED_EDGE('',*,*,#8090,.F.);
#11232=ORIENTED_EDGE('',*,*,#7963,.F.);
#11233=ORIENTED_EDGE('',*,*,#7964,.T.);
#11234=ORIENTED_EDGE('',*,*,#8090,.T.);
#11235=ORIENTED_EDGE('',*,*,#8091,.T.);
#11236=ORIENTED_EDGE('',*,*,#8092,.T.);
#11237=ORIENTED_EDGE('',*,*,#7966,.T.);
#11238=ORIENTED_EDGE('',*,*,#8093,.T.);
#11239=ORIENTED_EDGE('',*,*,#8094,.T.);
#11240=ORIENTED_EDGE('',*,*,#8095,.T.);
#11241=ORIENTED_EDGE('',*,*,#8095,.F.);
#11242=ORIENTED_EDGE('',*,*,#8096,.F.);
#11243=ORIENTED_EDGE('',*,*,#8097,.F.);
#11244=ORIENTED_EDGE('',*,*,#7967,.F.);
#11245=ORIENTED_EDGE('',*,*,#7968,.T.);
#11246=ORIENTED_EDGE('',*,*,#8097,.T.);
#11247=ORIENTED_EDGE('',*,*,#8098,.T.);
#11248=ORIENTED_EDGE('',*,*,#8099,.T.);
#11249=ORIENTED_EDGE('',*,*,#7970,.T.);
#11250=ORIENTED_EDGE('',*,*,#8100,.T.);
#11251=ORIENTED_EDGE('',*,*,#8101,.T.);
#11252=ORIENTED_EDGE('',*,*,#7899,.T.);
#11253=ORIENTED_EDGE('',*,*,#7974,.F.);
#11254=ORIENTED_EDGE('',*,*,#8102,.T.);
#11255=ORIENTED_EDGE('',*,*,#8103,.T.);
#11256=ORIENTED_EDGE('',*,*,#8102,.F.);
#11257=ORIENTED_EDGE('',*,*,#7973,.F.);
#11258=ORIENTED_EDGE('',*,*,#8104,.T.);
#11259=ORIENTED_EDGE('',*,*,#8105,.T.);
#11260=ORIENTED_EDGE('',*,*,#8104,.F.);
#11261=ORIENTED_EDGE('',*,*,#7893,.T.);
#11262=ORIENTED_EDGE('',*,*,#8106,.T.);
#11263=ORIENTED_EDGE('',*,*,#7884,.T.);
#11264=ORIENTED_EDGE('',*,*,#8106,.F.);
#11265=ORIENTED_EDGE('',*,*,#7972,.F.);
#11266=ORIENTED_EDGE('',*,*,#8107,.T.);
#11267=ORIENTED_EDGE('',*,*,#8108,.T.);
#11268=ORIENTED_EDGE('',*,*,#8107,.F.);
#11269=ORIENTED_EDGE('',*,*,#7971,.F.);
#11270=ORIENTED_EDGE('',*,*,#8109,.T.);
#11271=ORIENTED_EDGE('',*,*,#8110,.T.);
#11272=ORIENTED_EDGE('',*,*,#8109,.F.);
#11273=ORIENTED_EDGE('',*,*,#8099,.F.);
#11274=ORIENTED_EDGE('',*,*,#8111,.F.);
#11275=ORIENTED_EDGE('',*,*,#8100,.F.);
#11276=ORIENTED_EDGE('',*,*,#7969,.F.);
#11277=ORIENTED_EDGE('',*,*,#8092,.F.);
#11278=ORIENTED_EDGE('',*,*,#8112,.F.);
#11279=ORIENTED_EDGE('',*,*,#8093,.F.);
#11280=ORIENTED_EDGE('',*,*,#7965,.F.);
#11281=ORIENTED_EDGE('',*,*,#8073,.F.);
#11282=ORIENTED_EDGE('',*,*,#8113,.F.);
#11283=ORIENTED_EDGE('',*,*,#8076,.F.);
#11284=ORIENTED_EDGE('',*,*,#7955,.F.);
#11285=ORIENTED_EDGE('',*,*,#8066,.F.);
#11286=ORIENTED_EDGE('',*,*,#8114,.F.);
#11287=ORIENTED_EDGE('',*,*,#8067,.F.);
#11288=ORIENTED_EDGE('',*,*,#7951,.F.);
#11289=ORIENTED_EDGE('',*,*,#8059,.F.);
#11290=ORIENTED_EDGE('',*,*,#8115,.F.);
#11291=ORIENTED_EDGE('',*,*,#8060,.F.);
#11292=ORIENTED_EDGE('',*,*,#7947,.F.);
#11293=ORIENTED_EDGE('',*,*,#8040,.F.);
#11294=ORIENTED_EDGE('',*,*,#8116,.F.);
#11295=ORIENTED_EDGE('',*,*,#8043,.F.);
#11296=ORIENTED_EDGE('',*,*,#7937,.F.);
#11297=ORIENTED_EDGE('',*,*,#8033,.F.);
#11298=ORIENTED_EDGE('',*,*,#8117,.F.);
#11299=ORIENTED_EDGE('',*,*,#8034,.F.);
#11300=ORIENTED_EDGE('',*,*,#7933,.F.);
#11301=ORIENTED_EDGE('',*,*,#8026,.F.);
#11302=ORIENTED_EDGE('',*,*,#8118,.F.);
#11303=ORIENTED_EDGE('',*,*,#8027,.F.);
#11304=ORIENTED_EDGE('',*,*,#7929,.F.);
#11305=ORIENTED_EDGE('',*,*,#8007,.F.);
#11306=ORIENTED_EDGE('',*,*,#8119,.F.);
#11307=ORIENTED_EDGE('',*,*,#8010,.F.);
#11308=ORIENTED_EDGE('',*,*,#7919,.F.);
#11309=ORIENTED_EDGE('',*,*,#8000,.F.);
#11310=ORIENTED_EDGE('',*,*,#8120,.F.);
#11311=ORIENTED_EDGE('',*,*,#8001,.F.);
#11312=ORIENTED_EDGE('',*,*,#7915,.F.);
#11313=ORIENTED_EDGE('',*,*,#7993,.F.);
#11314=ORIENTED_EDGE('',*,*,#8121,.F.);
#11315=ORIENTED_EDGE('',*,*,#7994,.F.);
#11316=ORIENTED_EDGE('',*,*,#7911,.F.);
#11317=ORIENTED_EDGE('',*,*,#7897,.F.);
#11318=ORIENTED_EDGE('',*,*,#8122,.F.);
#11319=ORIENTED_EDGE('',*,*,#7977,.F.);
#11320=ORIENTED_EDGE('',*,*,#7901,.F.);
#11321=ORIENTED_EDGE('',*,*,#7896,.F.);
#11322=ORIENTED_EDGE('',*,*,#7900,.T.);
#11323=ORIENTED_EDGE('',*,*,#8101,.F.);
#11324=ORIENTED_EDGE('',*,*,#8111,.T.);
#11325=ORIENTED_EDGE('',*,*,#8098,.F.);
#11326=ORIENTED_EDGE('',*,*,#8096,.T.);
#11327=ORIENTED_EDGE('',*,*,#8094,.F.);
#11328=ORIENTED_EDGE('',*,*,#8112,.T.);
#11329=ORIENTED_EDGE('',*,*,#8091,.F.);
#11330=ORIENTED_EDGE('',*,*,#8089,.T.);
#11331=ORIENTED_EDGE('',*,*,#8087,.F.);
#11332=ORIENTED_EDGE('',*,*,#8085,.T.);
#11333=ORIENTED_EDGE('',*,*,#8083,.F.);
#11334=ORIENTED_EDGE('',*,*,#8081,.T.);
#11335=ORIENTED_EDGE('',*,*,#8079,.F.);
#11336=ORIENTED_EDGE('',*,*,#8077,.T.);
#11337=ORIENTED_EDGE('',*,*,#8074,.F.);
#11338=ORIENTED_EDGE('',*,*,#8113,.T.);
#11339=ORIENTED_EDGE('',*,*,#8072,.F.);
#11340=ORIENTED_EDGE('',*,*,#8070,.T.);
#11341=ORIENTED_EDGE('',*,*,#8068,.F.);
#11342=ORIENTED_EDGE('',*,*,#8114,.T.);
#11343=ORIENTED_EDGE('',*,*,#8065,.F.);
#11344=ORIENTED_EDGE('',*,*,#8063,.T.);
#11345=ORIENTED_EDGE('',*,*,#8061,.F.);
#11346=ORIENTED_EDGE('',*,*,#8115,.T.);
#11347=ORIENTED_EDGE('',*,*,#8058,.F.);
#11348=ORIENTED_EDGE('',*,*,#8056,.T.);
#11349=ORIENTED_EDGE('',*,*,#8054,.F.);
#11350=ORIENTED_EDGE('',*,*,#8052,.T.);
#11351=ORIENTED_EDGE('',*,*,#8050,.F.);
#11352=ORIENTED_EDGE('',*,*,#8048,.T.);
#11353=ORIENTED_EDGE('',*,*,#8046,.F.);
#11354=ORIENTED_EDGE('',*,*,#8044,.T.);
#11355=ORIENTED_EDGE('',*,*,#8041,.F.);
#11356=ORIENTED_EDGE('',*,*,#8116,.T.);
#11357=ORIENTED_EDGE('',*,*,#8039,.F.);
#11358=ORIENTED_EDGE('',*,*,#8037,.T.);
#11359=ORIENTED_EDGE('',*,*,#8035,.F.);
#11360=ORIENTED_EDGE('',*,*,#8117,.T.);
#11361=ORIENTED_EDGE('',*,*,#8032,.F.);
#11362=ORIENTED_EDGE('',*,*,#8030,.T.);
#11363=ORIENTED_EDGE('',*,*,#8028,.F.);
#11364=ORIENTED_EDGE('',*,*,#8118,.T.);
#11365=ORIENTED_EDGE('',*,*,#8025,.F.);
#11366=ORIENTED_EDGE('',*,*,#8023,.T.);
#11367=ORIENTED_EDGE('',*,*,#8021,.F.);
#11368=ORIENTED_EDGE('',*,*,#8019,.T.);
#11369=ORIENTED_EDGE('',*,*,#8017,.F.);
#11370=ORIENTED_EDGE('',*,*,#8015,.T.);
#11371=ORIENTED_EDGE('',*,*,#8013,.F.);
#11372=ORIENTED_EDGE('',*,*,#8011,.T.);
#11373=ORIENTED_EDGE('',*,*,#8008,.F.);
#11374=ORIENTED_EDGE('',*,*,#8119,.T.);
#11375=ORIENTED_EDGE('',*,*,#8006,.F.);
#11376=ORIENTED_EDGE('',*,*,#8004,.T.);
#11377=ORIENTED_EDGE('',*,*,#8002,.F.);
#11378=ORIENTED_EDGE('',*,*,#8120,.T.);
#11379=ORIENTED_EDGE('',*,*,#7999,.F.);
#11380=ORIENTED_EDGE('',*,*,#7997,.T.);
#11381=ORIENTED_EDGE('',*,*,#7995,.F.);
#11382=ORIENTED_EDGE('',*,*,#8121,.T.);
#11383=ORIENTED_EDGE('',*,*,#7992,.F.);
#11384=ORIENTED_EDGE('',*,*,#7990,.T.);
#11385=ORIENTED_EDGE('',*,*,#7988,.F.);
#11386=ORIENTED_EDGE('',*,*,#7986,.T.);
#11387=ORIENTED_EDGE('',*,*,#7984,.F.);
#11388=ORIENTED_EDGE('',*,*,#7982,.T.);
#11389=ORIENTED_EDGE('',*,*,#7980,.F.);
#11390=ORIENTED_EDGE('',*,*,#7978,.T.);
#11391=ORIENTED_EDGE('',*,*,#7975,.F.);
#11392=ORIENTED_EDGE('',*,*,#8122,.T.);
#11393=ORIENTED_EDGE('',*,*,#7883,.T.);
#11394=ORIENTED_EDGE('',*,*,#7752,.T.);
#11395=ORIENTED_EDGE('',*,*,#7880,.T.);
#11396=ORIENTED_EDGE('',*,*,#7874,.T.);
#11397=ORIENTED_EDGE('',*,*,#8110,.F.);
#11398=ORIENTED_EDGE('',*,*,#8108,.F.);
#11399=ORIENTED_EDGE('',*,*,#8105,.F.);
#11400=ORIENTED_EDGE('',*,*,#8103,.F.);
#11401=ORIENTED_EDGE('',*,*,#8123,.F.);
#11402=ORIENTED_EDGE('',*,*,#8124,.T.);
#11403=ORIENTED_EDGE('',*,*,#8125,.F.);
#11404=ORIENTED_EDGE('',*,*,#8126,.T.);
#11405=ORIENTED_EDGE('',*,*,#8123,.T.);
#11406=ORIENTED_EDGE('',*,*,#8126,.F.);
#11407=ORIENTED_EDGE('',*,*,#8124,.F.);
#11408=ORIENTED_EDGE('',*,*,#8127,.T.);
#11409=ORIENTED_EDGE('',*,*,#8128,.F.);
#11410=ORIENTED_EDGE('',*,*,#8127,.F.);
#11411=ORIENTED_EDGE('',*,*,#8129,.F.);
#11412=ORIENTED_EDGE('',*,*,#8130,.T.);
#11413=ORIENTED_EDGE('',*,*,#8131,.F.);
#11414=ORIENTED_EDGE('',*,*,#8130,.F.);
#11415=ORIENTED_EDGE('',*,*,#8132,.F.);
#11416=ORIENTED_EDGE('',*,*,#8133,.T.);
#11417=ORIENTED_EDGE('',*,*,#8134,.F.);
#11418=ORIENTED_EDGE('',*,*,#8133,.F.);
#11419=ORIENTED_EDGE('',*,*,#8135,.F.);
#11420=ORIENTED_EDGE('',*,*,#8136,.T.);
#11421=ORIENTED_EDGE('',*,*,#8137,.F.);
#11422=ORIENTED_EDGE('',*,*,#8136,.F.);
#11423=ORIENTED_EDGE('',*,*,#8138,.F.);
#11424=ORIENTED_EDGE('',*,*,#8139,.T.);
#11425=ORIENTED_EDGE('',*,*,#8140,.F.);
#11426=ORIENTED_EDGE('',*,*,#8139,.F.);
#11427=ORIENTED_EDGE('',*,*,#8141,.T.);
#11428=ORIENTED_EDGE('',*,*,#8142,.T.);
#11429=ORIENTED_EDGE('',*,*,#8143,.F.);
#11430=ORIENTED_EDGE('',*,*,#8144,.F.);
#11431=ORIENTED_EDGE('',*,*,#8145,.T.);
#11432=ORIENTED_EDGE('',*,*,#8144,.T.);
#11433=ORIENTED_EDGE('',*,*,#8146,.F.);
#11434=ORIENTED_EDGE('',*,*,#8147,.F.);
#11435=ORIENTED_EDGE('',*,*,#8148,.T.);
#11436=ORIENTED_EDGE('',*,*,#8147,.T.);
#11437=ORIENTED_EDGE('',*,*,#8149,.F.);
#11438=ORIENTED_EDGE('',*,*,#8150,.F.);
#11439=ORIENTED_EDGE('',*,*,#8151,.T.);
#11440=ORIENTED_EDGE('',*,*,#8150,.T.);
#11441=ORIENTED_EDGE('',*,*,#8152,.F.);
#11442=ORIENTED_EDGE('',*,*,#8142,.F.);
#11443=ORIENTED_EDGE('',*,*,#8152,.T.);
#11444=ORIENTED_EDGE('',*,*,#8149,.T.);
#11445=ORIENTED_EDGE('',*,*,#8146,.T.);
#11446=ORIENTED_EDGE('',*,*,#8143,.T.);
#11447=ORIENTED_EDGE('',*,*,#8125,.T.);
#11448=ORIENTED_EDGE('',*,*,#8129,.T.);
#11449=ORIENTED_EDGE('',*,*,#8132,.T.);
#11450=ORIENTED_EDGE('',*,*,#8135,.T.);
#11451=ORIENTED_EDGE('',*,*,#8138,.T.);
#11452=ORIENTED_EDGE('',*,*,#8151,.F.);
#11453=ORIENTED_EDGE('',*,*,#8141,.F.);
#11454=ORIENTED_EDGE('',*,*,#8145,.F.);
#11455=ORIENTED_EDGE('',*,*,#8148,.F.);
#11456=ORIENTED_EDGE('',*,*,#8128,.T.);
#11457=ORIENTED_EDGE('',*,*,#8131,.T.);
#11458=ORIENTED_EDGE('',*,*,#8134,.T.);
#11459=ORIENTED_EDGE('',*,*,#8137,.T.);
#11460=ORIENTED_EDGE('',*,*,#8140,.T.);
#11461=ORIENTED_EDGE('',*,*,#8153,.F.);
#11462=ORIENTED_EDGE('',*,*,#8154,.T.);
#11463=ORIENTED_EDGE('',*,*,#8155,.T.);
#11464=ORIENTED_EDGE('',*,*,#8156,.T.);
#11465=ORIENTED_EDGE('',*,*,#8157,.F.);
#11466=ORIENTED_EDGE('',*,*,#8158,.T.);
#11467=ORIENTED_EDGE('',*,*,#8153,.T.);
#11468=ORIENTED_EDGE('',*,*,#8159,.T.);
#11469=ORIENTED_EDGE('',*,*,#8160,.F.);
#11470=ORIENTED_EDGE('',*,*,#8161,.T.);
#11471=ORIENTED_EDGE('',*,*,#8157,.T.);
#11472=ORIENTED_EDGE('',*,*,#8162,.T.);
#11473=ORIENTED_EDGE('',*,*,#8163,.F.);
#11474=ORIENTED_EDGE('',*,*,#8164,.T.);
#11475=ORIENTED_EDGE('',*,*,#8160,.T.);
#11476=ORIENTED_EDGE('',*,*,#8165,.T.);
#11477=ORIENTED_EDGE('',*,*,#8166,.F.);
#11478=ORIENTED_EDGE('',*,*,#8167,.T.);
#11479=ORIENTED_EDGE('',*,*,#8163,.T.);
#11480=ORIENTED_EDGE('',*,*,#8168,.T.);
#11481=ORIENTED_EDGE('',*,*,#8169,.F.);
#11482=ORIENTED_EDGE('',*,*,#8170,.T.);
#11483=ORIENTED_EDGE('',*,*,#8166,.T.);
#11484=ORIENTED_EDGE('',*,*,#8171,.T.);
#11485=ORIENTED_EDGE('',*,*,#8172,.F.);
#11486=ORIENTED_EDGE('',*,*,#8173,.T.);
#11487=ORIENTED_EDGE('',*,*,#8169,.T.);
#11488=ORIENTED_EDGE('',*,*,#8174,.T.);
#11489=ORIENTED_EDGE('',*,*,#8175,.F.);
#11490=ORIENTED_EDGE('',*,*,#8176,.T.);
#11491=ORIENTED_EDGE('',*,*,#8172,.T.);
#11492=ORIENTED_EDGE('',*,*,#8177,.T.);
#11493=ORIENTED_EDGE('',*,*,#8178,.F.);
#11494=ORIENTED_EDGE('',*,*,#8179,.T.);
#11495=ORIENTED_EDGE('',*,*,#8175,.T.);
#11496=ORIENTED_EDGE('',*,*,#8180,.T.);
#11497=ORIENTED_EDGE('',*,*,#8181,.F.);
#11498=ORIENTED_EDGE('',*,*,#8182,.T.);
#11499=ORIENTED_EDGE('',*,*,#8178,.T.);
#11500=ORIENTED_EDGE('',*,*,#8183,.T.);
#11501=ORIENTED_EDGE('',*,*,#8184,.F.);
#11502=ORIENTED_EDGE('',*,*,#8185,.T.);
#11503=ORIENTED_EDGE('',*,*,#8181,.T.);
#11504=ORIENTED_EDGE('',*,*,#8186,.T.);
#11505=ORIENTED_EDGE('',*,*,#8187,.F.);
#11506=ORIENTED_EDGE('',*,*,#8188,.T.);
#11507=ORIENTED_EDGE('',*,*,#8184,.T.);
#11508=ORIENTED_EDGE('',*,*,#8189,.T.);
#11509=ORIENTED_EDGE('',*,*,#8190,.F.);
#11510=ORIENTED_EDGE('',*,*,#8191,.T.);
#11511=ORIENTED_EDGE('',*,*,#8187,.T.);
#11512=ORIENTED_EDGE('',*,*,#8192,.T.);
#11513=ORIENTED_EDGE('',*,*,#8193,.F.);
#11514=ORIENTED_EDGE('',*,*,#8194,.T.);
#11515=ORIENTED_EDGE('',*,*,#8190,.T.);
#11516=ORIENTED_EDGE('',*,*,#8195,.T.);
#11517=ORIENTED_EDGE('',*,*,#8196,.F.);
#11518=ORIENTED_EDGE('',*,*,#8197,.T.);
#11519=ORIENTED_EDGE('',*,*,#8193,.T.);
#11520=ORIENTED_EDGE('',*,*,#8198,.T.);
#11521=ORIENTED_EDGE('',*,*,#8199,.F.);
#11522=ORIENTED_EDGE('',*,*,#8200,.T.);
#11523=ORIENTED_EDGE('',*,*,#8196,.T.);
#11524=ORIENTED_EDGE('',*,*,#8201,.T.);
#11525=ORIENTED_EDGE('',*,*,#8202,.F.);
#11526=ORIENTED_EDGE('',*,*,#8203,.T.);
#11527=ORIENTED_EDGE('',*,*,#8199,.T.);
#11528=ORIENTED_EDGE('',*,*,#8204,.T.);
#11529=ORIENTED_EDGE('',*,*,#8205,.F.);
#11530=ORIENTED_EDGE('',*,*,#8206,.T.);
#11531=ORIENTED_EDGE('',*,*,#8202,.T.);
#11532=ORIENTED_EDGE('',*,*,#8207,.T.);
#11533=ORIENTED_EDGE('',*,*,#8208,.F.);
#11534=ORIENTED_EDGE('',*,*,#8209,.T.);
#11535=ORIENTED_EDGE('',*,*,#8205,.T.);
#11536=ORIENTED_EDGE('',*,*,#8210,.T.);
#11537=ORIENTED_EDGE('',*,*,#8211,.F.);
#11538=ORIENTED_EDGE('',*,*,#8212,.T.);
#11539=ORIENTED_EDGE('',*,*,#8213,.T.);
#11540=ORIENTED_EDGE('',*,*,#8214,.F.);
#11541=ORIENTED_EDGE('',*,*,#8215,.F.);
#11542=ORIENTED_EDGE('',*,*,#8216,.T.);
#11543=ORIENTED_EDGE('',*,*,#8211,.T.);
#11544=ORIENTED_EDGE('',*,*,#8217,.F.);
#11545=ORIENTED_EDGE('',*,*,#8218,.F.);
#11546=ORIENTED_EDGE('',*,*,#8219,.T.);
#11547=ORIENTED_EDGE('',*,*,#8215,.T.);
#11548=ORIENTED_EDGE('',*,*,#8220,.F.);
#11549=ORIENTED_EDGE('',*,*,#8221,.F.);
#11550=ORIENTED_EDGE('',*,*,#8222,.T.);
#11551=ORIENTED_EDGE('',*,*,#8218,.T.);
#11552=ORIENTED_EDGE('',*,*,#8223,.F.);
#11553=ORIENTED_EDGE('',*,*,#8224,.F.);
#11554=ORIENTED_EDGE('',*,*,#8225,.T.);
#11555=ORIENTED_EDGE('',*,*,#8221,.T.);
#11556=ORIENTED_EDGE('',*,*,#8226,.F.);
#11557=ORIENTED_EDGE('',*,*,#8227,.F.);
#11558=ORIENTED_EDGE('',*,*,#8228,.T.);
#11559=ORIENTED_EDGE('',*,*,#8224,.T.);
#11560=ORIENTED_EDGE('',*,*,#8229,.F.);
#11561=ORIENTED_EDGE('',*,*,#8230,.F.);
#11562=ORIENTED_EDGE('',*,*,#8231,.T.);
#11563=ORIENTED_EDGE('',*,*,#8227,.T.);
#11564=ORIENTED_EDGE('',*,*,#8232,.F.);
#11565=ORIENTED_EDGE('',*,*,#8233,.F.);
#11566=ORIENTED_EDGE('',*,*,#8234,.T.);
#11567=ORIENTED_EDGE('',*,*,#8230,.T.);
#11568=ORIENTED_EDGE('',*,*,#8235,.F.);
#11569=ORIENTED_EDGE('',*,*,#8236,.F.);
#11570=ORIENTED_EDGE('',*,*,#8237,.T.);
#11571=ORIENTED_EDGE('',*,*,#8233,.T.);
#11572=ORIENTED_EDGE('',*,*,#8238,.F.);
#11573=ORIENTED_EDGE('',*,*,#8239,.F.);
#11574=ORIENTED_EDGE('',*,*,#8240,.T.);
#11575=ORIENTED_EDGE('',*,*,#8236,.T.);
#11576=ORIENTED_EDGE('',*,*,#8241,.F.);
#11577=ORIENTED_EDGE('',*,*,#8242,.F.);
#11578=ORIENTED_EDGE('',*,*,#8243,.T.);
#11579=ORIENTED_EDGE('',*,*,#8239,.T.);
#11580=ORIENTED_EDGE('',*,*,#8244,.F.);
#11581=ORIENTED_EDGE('',*,*,#8245,.F.);
#11582=ORIENTED_EDGE('',*,*,#8246,.T.);
#11583=ORIENTED_EDGE('',*,*,#8242,.T.);
#11584=ORIENTED_EDGE('',*,*,#8247,.F.);
#11585=ORIENTED_EDGE('',*,*,#8248,.F.);
#11586=ORIENTED_EDGE('',*,*,#8249,.T.);
#11587=ORIENTED_EDGE('',*,*,#8245,.T.);
#11588=ORIENTED_EDGE('',*,*,#8250,.F.);
#11589=ORIENTED_EDGE('',*,*,#8251,.F.);
#11590=ORIENTED_EDGE('',*,*,#8252,.T.);
#11591=ORIENTED_EDGE('',*,*,#8248,.T.);
#11592=ORIENTED_EDGE('',*,*,#8253,.F.);
#11593=ORIENTED_EDGE('',*,*,#8254,.F.);
#11594=ORIENTED_EDGE('',*,*,#8255,.T.);
#11595=ORIENTED_EDGE('',*,*,#8251,.T.);
#11596=ORIENTED_EDGE('',*,*,#8256,.F.);
#11597=ORIENTED_EDGE('',*,*,#8257,.F.);
#11598=ORIENTED_EDGE('',*,*,#8258,.T.);
#11599=ORIENTED_EDGE('',*,*,#8254,.T.);
#11600=ORIENTED_EDGE('',*,*,#8259,.F.);
#11601=ORIENTED_EDGE('',*,*,#8260,.F.);
#11602=ORIENTED_EDGE('',*,*,#8261,.T.);
#11603=ORIENTED_EDGE('',*,*,#8257,.T.);
#11604=ORIENTED_EDGE('',*,*,#8262,.F.);
#11605=ORIENTED_EDGE('',*,*,#8263,.F.);
#11606=ORIENTED_EDGE('',*,*,#8264,.T.);
#11607=ORIENTED_EDGE('',*,*,#8260,.T.);
#11608=ORIENTED_EDGE('',*,*,#8265,.F.);
#11609=ORIENTED_EDGE('',*,*,#8266,.F.);
#11610=ORIENTED_EDGE('',*,*,#8267,.T.);
#11611=ORIENTED_EDGE('',*,*,#8263,.T.);
#11612=ORIENTED_EDGE('',*,*,#8268,.F.);
#11613=ORIENTED_EDGE('',*,*,#8269,.F.);
#11614=ORIENTED_EDGE('',*,*,#8213,.F.);
#11615=ORIENTED_EDGE('',*,*,#8270,.F.);
#11616=ORIENTED_EDGE('',*,*,#8271,.F.);
#11617=ORIENTED_EDGE('',*,*,#8272,.F.);
#11618=ORIENTED_EDGE('',*,*,#8273,.T.);
#11619=ORIENTED_EDGE('',*,*,#8274,.F.);
#11620=ORIENTED_EDGE('',*,*,#8273,.F.);
#11621=ORIENTED_EDGE('',*,*,#8270,.T.);
#11622=ORIENTED_EDGE('',*,*,#8212,.F.);
#11623=ORIENTED_EDGE('',*,*,#8216,.F.);
#11624=ORIENTED_EDGE('',*,*,#8219,.F.);
#11625=ORIENTED_EDGE('',*,*,#8222,.F.);
#11626=ORIENTED_EDGE('',*,*,#8225,.F.);
#11627=ORIENTED_EDGE('',*,*,#8228,.F.);
#11628=ORIENTED_EDGE('',*,*,#8231,.F.);
#11629=ORIENTED_EDGE('',*,*,#8234,.F.);
#11630=ORIENTED_EDGE('',*,*,#8237,.F.);
#11631=ORIENTED_EDGE('',*,*,#8240,.F.);
#11632=ORIENTED_EDGE('',*,*,#8243,.F.);
#11633=ORIENTED_EDGE('',*,*,#8246,.F.);
#11634=ORIENTED_EDGE('',*,*,#8249,.F.);
#11635=ORIENTED_EDGE('',*,*,#8252,.F.);
#11636=ORIENTED_EDGE('',*,*,#8255,.F.);
#11637=ORIENTED_EDGE('',*,*,#8258,.F.);
#11638=ORIENTED_EDGE('',*,*,#8261,.F.);
#11639=ORIENTED_EDGE('',*,*,#8264,.F.);
#11640=ORIENTED_EDGE('',*,*,#8267,.F.);
#11641=ORIENTED_EDGE('',*,*,#8275,.F.);
#11642=ORIENTED_EDGE('',*,*,#8276,.F.);
#11643=ORIENTED_EDGE('',*,*,#8154,.F.);
#11644=ORIENTED_EDGE('',*,*,#8158,.F.);
#11645=ORIENTED_EDGE('',*,*,#8161,.F.);
#11646=ORIENTED_EDGE('',*,*,#8164,.F.);
#11647=ORIENTED_EDGE('',*,*,#8167,.F.);
#11648=ORIENTED_EDGE('',*,*,#8170,.F.);
#11649=ORIENTED_EDGE('',*,*,#8173,.F.);
#11650=ORIENTED_EDGE('',*,*,#8176,.F.);
#11651=ORIENTED_EDGE('',*,*,#8179,.F.);
#11652=ORIENTED_EDGE('',*,*,#8182,.F.);
#11653=ORIENTED_EDGE('',*,*,#8185,.F.);
#11654=ORIENTED_EDGE('',*,*,#8188,.F.);
#11655=ORIENTED_EDGE('',*,*,#8191,.F.);
#11656=ORIENTED_EDGE('',*,*,#8194,.F.);
#11657=ORIENTED_EDGE('',*,*,#8197,.F.);
#11658=ORIENTED_EDGE('',*,*,#8200,.F.);
#11659=ORIENTED_EDGE('',*,*,#8203,.F.);
#11660=ORIENTED_EDGE('',*,*,#8206,.F.);
#11661=ORIENTED_EDGE('',*,*,#8209,.F.);
#11662=ORIENTED_EDGE('',*,*,#8277,.F.);
#11663=ORIENTED_EDGE('',*,*,#8266,.T.);
#11664=ORIENTED_EDGE('',*,*,#8278,.F.);
#11665=ORIENTED_EDGE('',*,*,#8279,.F.);
#11666=ORIENTED_EDGE('',*,*,#8275,.T.);
#11667=ORIENTED_EDGE('',*,*,#8269,.T.);
#11668=ORIENTED_EDGE('',*,*,#8272,.T.);
#11669=ORIENTED_EDGE('',*,*,#8280,.F.);
#11670=ORIENTED_EDGE('',*,*,#8210,.F.);
#11671=ORIENTED_EDGE('',*,*,#8207,.F.);
#11672=ORIENTED_EDGE('',*,*,#8204,.F.);
#11673=ORIENTED_EDGE('',*,*,#8201,.F.);
#11674=ORIENTED_EDGE('',*,*,#8198,.F.);
#11675=ORIENTED_EDGE('',*,*,#8195,.F.);
#11676=ORIENTED_EDGE('',*,*,#8192,.F.);
#11677=ORIENTED_EDGE('',*,*,#8189,.F.);
#11678=ORIENTED_EDGE('',*,*,#8186,.F.);
#11679=ORIENTED_EDGE('',*,*,#8183,.F.);
#11680=ORIENTED_EDGE('',*,*,#8180,.F.);
#11681=ORIENTED_EDGE('',*,*,#8177,.F.);
#11682=ORIENTED_EDGE('',*,*,#8174,.F.);
#11683=ORIENTED_EDGE('',*,*,#8171,.F.);
#11684=ORIENTED_EDGE('',*,*,#8168,.F.);
#11685=ORIENTED_EDGE('',*,*,#8165,.F.);
#11686=ORIENTED_EDGE('',*,*,#8162,.F.);
#11687=ORIENTED_EDGE('',*,*,#8159,.F.);
#11688=ORIENTED_EDGE('',*,*,#8156,.F.);
#11689=ORIENTED_EDGE('',*,*,#8281,.F.);
#11690=ORIENTED_EDGE('',*,*,#8278,.T.);
#11691=ORIENTED_EDGE('',*,*,#8268,.T.);
#11692=ORIENTED_EDGE('',*,*,#8265,.T.);
#11693=ORIENTED_EDGE('',*,*,#8262,.T.);
#11694=ORIENTED_EDGE('',*,*,#8259,.T.);
#11695=ORIENTED_EDGE('',*,*,#8256,.T.);
#11696=ORIENTED_EDGE('',*,*,#8253,.T.);
#11697=ORIENTED_EDGE('',*,*,#8250,.T.);
#11698=ORIENTED_EDGE('',*,*,#8247,.T.);
#11699=ORIENTED_EDGE('',*,*,#8244,.T.);
#11700=ORIENTED_EDGE('',*,*,#8241,.T.);
#11701=ORIENTED_EDGE('',*,*,#8238,.T.);
#11702=ORIENTED_EDGE('',*,*,#8235,.T.);
#11703=ORIENTED_EDGE('',*,*,#8232,.T.);
#11704=ORIENTED_EDGE('',*,*,#8229,.T.);
#11705=ORIENTED_EDGE('',*,*,#8226,.T.);
#11706=ORIENTED_EDGE('',*,*,#8223,.T.);
#11707=ORIENTED_EDGE('',*,*,#8220,.T.);
#11708=ORIENTED_EDGE('',*,*,#8217,.T.);
#11709=ORIENTED_EDGE('',*,*,#8214,.T.);
#11710=ORIENTED_EDGE('',*,*,#8208,.T.);
#11711=ORIENTED_EDGE('',*,*,#8280,.T.);
#11712=ORIENTED_EDGE('',*,*,#8271,.T.);
#11713=ORIENTED_EDGE('',*,*,#8277,.T.);
#11714=ORIENTED_EDGE('',*,*,#8282,.F.);
#11715=ORIENTED_EDGE('',*,*,#8283,.T.);
#11716=ORIENTED_EDGE('',*,*,#8284,.T.);
#11717=ORIENTED_EDGE('',*,*,#8285,.F.);
#11718=ORIENTED_EDGE('',*,*,#8286,.F.);
#11719=ORIENTED_EDGE('',*,*,#8287,.T.);
#11720=ORIENTED_EDGE('',*,*,#8288,.T.);
#11721=ORIENTED_EDGE('',*,*,#8283,.F.);
#11722=ORIENTED_EDGE('',*,*,#8289,.F.);
#11723=ORIENTED_EDGE('',*,*,#8290,.T.);
#11724=ORIENTED_EDGE('',*,*,#8291,.T.);
#11725=ORIENTED_EDGE('',*,*,#8287,.F.);
#11726=ORIENTED_EDGE('',*,*,#8292,.F.);
#11727=ORIENTED_EDGE('',*,*,#8293,.T.);
#11728=ORIENTED_EDGE('',*,*,#8294,.T.);
#11729=ORIENTED_EDGE('',*,*,#8290,.F.);
#11730=ORIENTED_EDGE('',*,*,#8295,.F.);
#11731=ORIENTED_EDGE('',*,*,#8296,.T.);
#11732=ORIENTED_EDGE('',*,*,#8297,.T.);
#11733=ORIENTED_EDGE('',*,*,#8293,.F.);
#11734=ORIENTED_EDGE('',*,*,#8298,.F.);
#11735=ORIENTED_EDGE('',*,*,#8285,.T.);
#11736=ORIENTED_EDGE('',*,*,#8299,.T.);
#11737=ORIENTED_EDGE('',*,*,#8296,.F.);
#11738=ORIENTED_EDGE('',*,*,#8299,.F.);
#11739=ORIENTED_EDGE('',*,*,#8284,.F.);
#11740=ORIENTED_EDGE('',*,*,#8288,.F.);
#11741=ORIENTED_EDGE('',*,*,#8291,.F.);
#11742=ORIENTED_EDGE('',*,*,#8294,.F.);
#11743=ORIENTED_EDGE('',*,*,#8297,.F.);
#11744=ORIENTED_EDGE('',*,*,#8300,.T.);
#11745=ORIENTED_EDGE('',*,*,#8276,.T.);
#11746=ORIENTED_EDGE('',*,*,#8279,.T.);
#11747=ORIENTED_EDGE('',*,*,#8281,.T.);
#11748=ORIENTED_EDGE('',*,*,#8155,.F.);
#11749=ORIENTED_EDGE('',*,*,#8300,.F.);
#11750=ORIENTED_EDGE('',*,*,#8301,.T.);
#11751=ORIENTED_EDGE('',*,*,#8302,.T.);
#11752=ORIENTED_EDGE('',*,*,#8301,.F.);
#11753=ORIENTED_EDGE('',*,*,#8302,.F.);
#11754=ORIENTED_EDGE('',*,*,#8282,.T.);
#11755=ORIENTED_EDGE('',*,*,#8298,.T.);
#11756=ORIENTED_EDGE('',*,*,#8295,.T.);
#11757=ORIENTED_EDGE('',*,*,#8292,.T.);
#11758=ORIENTED_EDGE('',*,*,#8289,.T.);
#11759=ORIENTED_EDGE('',*,*,#8286,.T.);
#11760=ORIENTED_EDGE('',*,*,#8274,.T.);
#11761=ORIENTED_EDGE('',*,*,#8303,.F.);
#11762=ORIENTED_EDGE('',*,*,#8304,.T.);
#11763=ORIENTED_EDGE('',*,*,#8305,.T.);
#11764=ORIENTED_EDGE('',*,*,#8304,.F.);
#11765=ORIENTED_EDGE('',*,*,#8303,.T.);
#11766=ORIENTED_EDGE('',*,*,#8305,.F.);
#11767=ORIENTED_EDGE('',*,*,#8306,.T.);
#11768=ORIENTED_EDGE('',*,*,#8307,.T.);
#11769=ORIENTED_EDGE('',*,*,#8308,.T.);
#11770=ORIENTED_EDGE('',*,*,#8309,.T.);
#11771=ORIENTED_EDGE('',*,*,#8310,.T.);
#11772=ORIENTED_EDGE('',*,*,#8309,.F.);
#11773=ORIENTED_EDGE('',*,*,#8311,.T.);
#11774=ORIENTED_EDGE('',*,*,#8312,.T.);
#11775=ORIENTED_EDGE('',*,*,#8313,.T.);
#11776=ORIENTED_EDGE('',*,*,#8314,.T.);
#11777=ORIENTED_EDGE('',*,*,#8306,.F.);
#11778=ORIENTED_EDGE('',*,*,#8315,.T.);
#11779=ORIENTED_EDGE('',*,*,#8316,.T.);
#11780=ORIENTED_EDGE('',*,*,#8317,.T.);
#11781=ORIENTED_EDGE('',*,*,#8313,.F.);
#11782=ORIENTED_EDGE('',*,*,#8318,.T.);
#11783=ORIENTED_EDGE('',*,*,#8319,.T.);
#11784=ORIENTED_EDGE('',*,*,#8320,.T.);
#11785=ORIENTED_EDGE('',*,*,#8316,.F.);
#11786=ORIENTED_EDGE('',*,*,#8321,.T.);
#11787=ORIENTED_EDGE('',*,*,#8322,.T.);
#11788=ORIENTED_EDGE('',*,*,#8323,.T.);
#11789=ORIENTED_EDGE('',*,*,#8319,.F.);
#11790=ORIENTED_EDGE('',*,*,#8324,.T.);
#11791=ORIENTED_EDGE('',*,*,#8325,.T.);
#11792=ORIENTED_EDGE('',*,*,#8326,.T.);
#11793=ORIENTED_EDGE('',*,*,#8322,.F.);
#11794=ORIENTED_EDGE('',*,*,#8327,.T.);
#11795=ORIENTED_EDGE('',*,*,#8328,.T.);
#11796=ORIENTED_EDGE('',*,*,#8329,.T.);
#11797=ORIENTED_EDGE('',*,*,#8325,.F.);
#11798=ORIENTED_EDGE('',*,*,#8330,.T.);
#11799=ORIENTED_EDGE('',*,*,#8331,.F.);
#11800=ORIENTED_EDGE('',*,*,#8332,.T.);
#11801=ORIENTED_EDGE('',*,*,#8333,.F.);
#11802=ORIENTED_EDGE('',*,*,#8334,.T.);
#11803=ORIENTED_EDGE('',*,*,#8335,.T.);
#11804=ORIENTED_EDGE('',*,*,#8336,.T.);
#11805=ORIENTED_EDGE('',*,*,#8337,.F.);
#11806=ORIENTED_EDGE('',*,*,#8338,.F.);
#11807=ORIENTED_EDGE('',*,*,#8339,.T.);
#11808=ORIENTED_EDGE('',*,*,#8340,.T.);
#11809=ORIENTED_EDGE('',*,*,#8335,.F.);
#11810=ORIENTED_EDGE('',*,*,#8341,.F.);
#11811=ORIENTED_EDGE('',*,*,#8342,.T.);
#11812=ORIENTED_EDGE('',*,*,#8343,.T.);
#11813=ORIENTED_EDGE('',*,*,#8339,.F.);
#11814=ORIENTED_EDGE('',*,*,#8344,.F.);
#11815=ORIENTED_EDGE('',*,*,#8345,.T.);
#11816=ORIENTED_EDGE('',*,*,#8346,.T.);
#11817=ORIENTED_EDGE('',*,*,#8342,.F.);
#11818=ORIENTED_EDGE('',*,*,#8347,.F.);
#11819=ORIENTED_EDGE('',*,*,#8348,.T.);
#11820=ORIENTED_EDGE('',*,*,#8349,.T.);
#11821=ORIENTED_EDGE('',*,*,#8345,.F.);
#11822=ORIENTED_EDGE('',*,*,#8350,.F.);
#11823=ORIENTED_EDGE('',*,*,#8351,.T.);
#11824=ORIENTED_EDGE('',*,*,#8352,.T.);
#11825=ORIENTED_EDGE('',*,*,#8348,.F.);
#11826=ORIENTED_EDGE('',*,*,#8353,.F.);
#11827=ORIENTED_EDGE('',*,*,#8354,.T.);
#11828=ORIENTED_EDGE('',*,*,#8355,.T.);
#11829=ORIENTED_EDGE('',*,*,#8351,.F.);
#11830=ORIENTED_EDGE('',*,*,#8356,.F.);
#11831=ORIENTED_EDGE('',*,*,#8357,.F.);
#11832=ORIENTED_EDGE('',*,*,#8358,.F.);
#11833=ORIENTED_EDGE('',*,*,#8359,.F.);
#11834=ORIENTED_EDGE('',*,*,#8360,.T.);
#11835=ORIENTED_EDGE('',*,*,#8361,.T.);
#11836=ORIENTED_EDGE('',*,*,#8362,.T.);
#11837=ORIENTED_EDGE('',*,*,#8363,.T.);
#11838=ORIENTED_EDGE('',*,*,#8364,.T.);
#11839=ORIENTED_EDGE('',*,*,#8365,.T.);
#11840=ORIENTED_EDGE('',*,*,#8364,.F.);
#11841=ORIENTED_EDGE('',*,*,#8366,.T.);
#11842=ORIENTED_EDGE('',*,*,#8367,.T.);
#11843=ORIENTED_EDGE('',*,*,#8368,.T.);
#11844=ORIENTED_EDGE('',*,*,#8369,.T.);
#11845=ORIENTED_EDGE('',*,*,#8361,.F.);
#11846=ORIENTED_EDGE('',*,*,#8370,.T.);
#11847=ORIENTED_EDGE('',*,*,#8371,.T.);
#11848=ORIENTED_EDGE('',*,*,#8372,.T.);
#11849=ORIENTED_EDGE('',*,*,#8368,.F.);
#11850=ORIENTED_EDGE('',*,*,#8373,.T.);
#11851=ORIENTED_EDGE('',*,*,#8374,.T.);
#11852=ORIENTED_EDGE('',*,*,#8375,.T.);
#11853=ORIENTED_EDGE('',*,*,#8371,.F.);
#11854=ORIENTED_EDGE('',*,*,#8376,.T.);
#11855=ORIENTED_EDGE('',*,*,#8377,.T.);
#11856=ORIENTED_EDGE('',*,*,#8378,.T.);
#11857=ORIENTED_EDGE('',*,*,#8374,.F.);
#11858=ORIENTED_EDGE('',*,*,#8379,.T.);
#11859=ORIENTED_EDGE('',*,*,#8380,.T.);
#11860=ORIENTED_EDGE('',*,*,#8381,.T.);
#11861=ORIENTED_EDGE('',*,*,#8377,.F.);
#11862=ORIENTED_EDGE('',*,*,#8382,.T.);
#11863=ORIENTED_EDGE('',*,*,#8383,.T.);
#11864=ORIENTED_EDGE('',*,*,#8384,.T.);
#11865=ORIENTED_EDGE('',*,*,#8380,.F.);
#11866=ORIENTED_EDGE('',*,*,#8385,.T.);
#11867=ORIENTED_EDGE('',*,*,#8386,.F.);
#11868=ORIENTED_EDGE('',*,*,#8387,.T.);
#11869=ORIENTED_EDGE('',*,*,#8388,.F.);
#11870=ORIENTED_EDGE('',*,*,#8389,.T.);
#11871=ORIENTED_EDGE('',*,*,#8390,.T.);
#11872=ORIENTED_EDGE('',*,*,#8391,.T.);
#11873=ORIENTED_EDGE('',*,*,#8392,.F.);
#11874=ORIENTED_EDGE('',*,*,#8393,.F.);
#11875=ORIENTED_EDGE('',*,*,#8394,.T.);
#11876=ORIENTED_EDGE('',*,*,#8395,.T.);
#11877=ORIENTED_EDGE('',*,*,#8390,.F.);
#11878=ORIENTED_EDGE('',*,*,#8396,.F.);
#11879=ORIENTED_EDGE('',*,*,#8397,.T.);
#11880=ORIENTED_EDGE('',*,*,#8398,.T.);
#11881=ORIENTED_EDGE('',*,*,#8394,.F.);
#11882=ORIENTED_EDGE('',*,*,#8399,.F.);
#11883=ORIENTED_EDGE('',*,*,#8400,.T.);
#11884=ORIENTED_EDGE('',*,*,#8401,.T.);
#11885=ORIENTED_EDGE('',*,*,#8397,.F.);
#11886=ORIENTED_EDGE('',*,*,#8402,.F.);
#11887=ORIENTED_EDGE('',*,*,#8403,.T.);
#11888=ORIENTED_EDGE('',*,*,#8404,.T.);
#11889=ORIENTED_EDGE('',*,*,#8400,.F.);
#11890=ORIENTED_EDGE('',*,*,#8405,.F.);
#11891=ORIENTED_EDGE('',*,*,#8406,.T.);
#11892=ORIENTED_EDGE('',*,*,#8407,.T.);
#11893=ORIENTED_EDGE('',*,*,#8403,.F.);
#11894=ORIENTED_EDGE('',*,*,#8408,.F.);
#11895=ORIENTED_EDGE('',*,*,#8409,.T.);
#11896=ORIENTED_EDGE('',*,*,#8410,.T.);
#11897=ORIENTED_EDGE('',*,*,#8406,.F.);
#11898=ORIENTED_EDGE('',*,*,#8411,.F.);
#11899=ORIENTED_EDGE('',*,*,#8412,.F.);
#11900=ORIENTED_EDGE('',*,*,#8413,.F.);
#11901=ORIENTED_EDGE('',*,*,#8414,.F.);
#11902=ORIENTED_EDGE('',*,*,#8415,.T.);
#11903=ORIENTED_EDGE('',*,*,#8416,.T.);
#11904=ORIENTED_EDGE('',*,*,#8417,.T.);
#11905=ORIENTED_EDGE('',*,*,#8418,.T.);
#11906=ORIENTED_EDGE('',*,*,#8419,.T.);
#11907=ORIENTED_EDGE('',*,*,#8420,.T.);
#11908=ORIENTED_EDGE('',*,*,#8419,.F.);
#11909=ORIENTED_EDGE('',*,*,#8421,.T.);
#11910=ORIENTED_EDGE('',*,*,#8422,.T.);
#11911=ORIENTED_EDGE('',*,*,#8423,.T.);
#11912=ORIENTED_EDGE('',*,*,#8424,.T.);
#11913=ORIENTED_EDGE('',*,*,#8416,.F.);
#11914=ORIENTED_EDGE('',*,*,#8425,.T.);
#11915=ORIENTED_EDGE('',*,*,#8426,.T.);
#11916=ORIENTED_EDGE('',*,*,#8427,.T.);
#11917=ORIENTED_EDGE('',*,*,#8423,.F.);
#11918=ORIENTED_EDGE('',*,*,#8428,.T.);
#11919=ORIENTED_EDGE('',*,*,#8429,.T.);
#11920=ORIENTED_EDGE('',*,*,#8430,.T.);
#11921=ORIENTED_EDGE('',*,*,#8426,.F.);
#11922=ORIENTED_EDGE('',*,*,#8431,.T.);
#11923=ORIENTED_EDGE('',*,*,#8432,.T.);
#11924=ORIENTED_EDGE('',*,*,#8433,.T.);
#11925=ORIENTED_EDGE('',*,*,#8429,.F.);
#11926=ORIENTED_EDGE('',*,*,#8434,.T.);
#11927=ORIENTED_EDGE('',*,*,#8435,.T.);
#11928=ORIENTED_EDGE('',*,*,#8436,.T.);
#11929=ORIENTED_EDGE('',*,*,#8432,.F.);
#11930=ORIENTED_EDGE('',*,*,#8437,.T.);
#11931=ORIENTED_EDGE('',*,*,#8438,.T.);
#11932=ORIENTED_EDGE('',*,*,#8439,.T.);
#11933=ORIENTED_EDGE('',*,*,#8435,.F.);
#11934=ORIENTED_EDGE('',*,*,#8440,.T.);
#11935=ORIENTED_EDGE('',*,*,#8441,.F.);
#11936=ORIENTED_EDGE('',*,*,#8442,.T.);
#11937=ORIENTED_EDGE('',*,*,#8443,.F.);
#11938=ORIENTED_EDGE('',*,*,#8444,.T.);
#11939=ORIENTED_EDGE('',*,*,#8445,.T.);
#11940=ORIENTED_EDGE('',*,*,#8446,.T.);
#11941=ORIENTED_EDGE('',*,*,#8447,.F.);
#11942=ORIENTED_EDGE('',*,*,#8448,.F.);
#11943=ORIENTED_EDGE('',*,*,#8449,.T.);
#11944=ORIENTED_EDGE('',*,*,#8450,.T.);
#11945=ORIENTED_EDGE('',*,*,#8445,.F.);
#11946=ORIENTED_EDGE('',*,*,#8451,.F.);
#11947=ORIENTED_EDGE('',*,*,#8452,.T.);
#11948=ORIENTED_EDGE('',*,*,#8453,.T.);
#11949=ORIENTED_EDGE('',*,*,#8449,.F.);
#11950=ORIENTED_EDGE('',*,*,#8454,.F.);
#11951=ORIENTED_EDGE('',*,*,#8455,.T.);
#11952=ORIENTED_EDGE('',*,*,#8456,.T.);
#11953=ORIENTED_EDGE('',*,*,#8452,.F.);
#11954=ORIENTED_EDGE('',*,*,#8457,.F.);
#11955=ORIENTED_EDGE('',*,*,#8458,.T.);
#11956=ORIENTED_EDGE('',*,*,#8459,.T.);
#11957=ORIENTED_EDGE('',*,*,#8455,.F.);
#11958=ORIENTED_EDGE('',*,*,#8460,.F.);
#11959=ORIENTED_EDGE('',*,*,#8461,.T.);
#11960=ORIENTED_EDGE('',*,*,#8462,.T.);
#11961=ORIENTED_EDGE('',*,*,#8458,.F.);
#11962=ORIENTED_EDGE('',*,*,#8463,.F.);
#11963=ORIENTED_EDGE('',*,*,#8464,.T.);
#11964=ORIENTED_EDGE('',*,*,#8465,.T.);
#11965=ORIENTED_EDGE('',*,*,#8461,.F.);
#11966=ORIENTED_EDGE('',*,*,#8466,.F.);
#11967=ORIENTED_EDGE('',*,*,#8467,.F.);
#11968=ORIENTED_EDGE('',*,*,#8468,.F.);
#11969=ORIENTED_EDGE('',*,*,#8469,.F.);
#11970=ORIENTED_EDGE('',*,*,#8470,.T.);
#11971=ORIENTED_EDGE('',*,*,#8418,.F.);
#11972=ORIENTED_EDGE('',*,*,#8471,.T.);
#11973=ORIENTED_EDGE('',*,*,#8447,.T.);
#11974=ORIENTED_EDGE('',*,*,#8472,.T.);
#11975=ORIENTED_EDGE('',*,*,#8421,.F.);
#11976=ORIENTED_EDGE('',*,*,#8467,.T.);
#11977=ORIENTED_EDGE('',*,*,#8473,.T.);
#11978=ORIENTED_EDGE('',*,*,#8464,.F.);
#11979=ORIENTED_EDGE('',*,*,#8474,.F.);
#11980=ORIENTED_EDGE('',*,*,#8472,.F.);
#11981=ORIENTED_EDGE('',*,*,#8446,.F.);
#11982=ORIENTED_EDGE('',*,*,#8450,.F.);
#11983=ORIENTED_EDGE('',*,*,#8453,.F.);
#11984=ORIENTED_EDGE('',*,*,#8456,.F.);
#11985=ORIENTED_EDGE('',*,*,#8459,.F.);
#11986=ORIENTED_EDGE('',*,*,#8462,.F.);
#11987=ORIENTED_EDGE('',*,*,#8465,.F.);
#11988=ORIENTED_EDGE('',*,*,#8473,.F.);
#11989=ORIENTED_EDGE('',*,*,#8470,.F.);
#11990=ORIENTED_EDGE('',*,*,#8475,.F.);
#11991=ORIENTED_EDGE('',*,*,#8442,.F.);
#11992=ORIENTED_EDGE('',*,*,#8476,.F.);
#11993=ORIENTED_EDGE('',*,*,#8440,.F.);
#11994=ORIENTED_EDGE('',*,*,#8437,.F.);
#11995=ORIENTED_EDGE('',*,*,#8434,.F.);
#11996=ORIENTED_EDGE('',*,*,#8431,.F.);
#11997=ORIENTED_EDGE('',*,*,#8428,.F.);
#11998=ORIENTED_EDGE('',*,*,#8425,.F.);
#11999=ORIENTED_EDGE('',*,*,#8422,.F.);
#12000=ORIENTED_EDGE('',*,*,#8471,.F.);
#12001=ORIENTED_EDGE('',*,*,#8417,.F.);
#12002=ORIENTED_EDGE('',*,*,#8424,.F.);
#12003=ORIENTED_EDGE('',*,*,#8427,.F.);
#12004=ORIENTED_EDGE('',*,*,#8430,.F.);
#12005=ORIENTED_EDGE('',*,*,#8433,.F.);
#12006=ORIENTED_EDGE('',*,*,#8436,.F.);
#12007=ORIENTED_EDGE('',*,*,#8439,.F.);
#12008=ORIENTED_EDGE('',*,*,#8477,.F.);
#12009=ORIENTED_EDGE('',*,*,#8444,.F.);
#12010=ORIENTED_EDGE('',*,*,#8478,.F.);
#12011=ORIENTED_EDGE('',*,*,#8468,.T.);
#12012=ORIENTED_EDGE('',*,*,#8474,.T.);
#12013=ORIENTED_EDGE('',*,*,#8466,.T.);
#12014=ORIENTED_EDGE('',*,*,#8463,.T.);
#12015=ORIENTED_EDGE('',*,*,#8460,.T.);
#12016=ORIENTED_EDGE('',*,*,#8457,.T.);
#12017=ORIENTED_EDGE('',*,*,#8454,.T.);
#12018=ORIENTED_EDGE('',*,*,#8451,.T.);
#12019=ORIENTED_EDGE('',*,*,#8448,.T.);
#12020=ORIENTED_EDGE('',*,*,#8441,.T.);
#12021=ORIENTED_EDGE('',*,*,#8477,.T.);
#12022=ORIENTED_EDGE('',*,*,#8438,.F.);
#12023=ORIENTED_EDGE('',*,*,#8476,.T.);
#12024=ORIENTED_EDGE('',*,*,#8363,.F.);
#12025=ORIENTED_EDGE('',*,*,#8479,.T.);
#12026=ORIENTED_EDGE('',*,*,#8392,.T.);
#12027=ORIENTED_EDGE('',*,*,#8480,.T.);
#12028=ORIENTED_EDGE('',*,*,#8366,.F.);
#12029=ORIENTED_EDGE('',*,*,#8412,.T.);
#12030=ORIENTED_EDGE('',*,*,#8481,.T.);
#12031=ORIENTED_EDGE('',*,*,#8409,.F.);
#12032=ORIENTED_EDGE('',*,*,#8482,.F.);
#12033=ORIENTED_EDGE('',*,*,#8480,.F.);
#12034=ORIENTED_EDGE('',*,*,#8391,.F.);
#12035=ORIENTED_EDGE('',*,*,#8395,.F.);
#12036=ORIENTED_EDGE('',*,*,#8398,.F.);
#12037=ORIENTED_EDGE('',*,*,#8401,.F.);
#12038=ORIENTED_EDGE('',*,*,#8404,.F.);
#12039=ORIENTED_EDGE('',*,*,#8407,.F.);
#12040=ORIENTED_EDGE('',*,*,#8410,.F.);
#12041=ORIENTED_EDGE('',*,*,#8481,.F.);
#12042=ORIENTED_EDGE('',*,*,#8415,.F.);
#12043=ORIENTED_EDGE('',*,*,#8483,.F.);
#12044=ORIENTED_EDGE('',*,*,#8387,.F.);
#12045=ORIENTED_EDGE('',*,*,#8484,.F.);
#12046=ORIENTED_EDGE('',*,*,#8385,.F.);
#12047=ORIENTED_EDGE('',*,*,#8382,.F.);
#12048=ORIENTED_EDGE('',*,*,#8379,.F.);
#12049=ORIENTED_EDGE('',*,*,#8376,.F.);
#12050=ORIENTED_EDGE('',*,*,#8373,.F.);
#12051=ORIENTED_EDGE('',*,*,#8370,.F.);
#12052=ORIENTED_EDGE('',*,*,#8367,.F.);
#12053=ORIENTED_EDGE('',*,*,#8479,.F.);
#12054=ORIENTED_EDGE('',*,*,#8362,.F.);
#12055=ORIENTED_EDGE('',*,*,#8369,.F.);
#12056=ORIENTED_EDGE('',*,*,#8372,.F.);
#12057=ORIENTED_EDGE('',*,*,#8375,.F.);
#12058=ORIENTED_EDGE('',*,*,#8378,.F.);
#12059=ORIENTED_EDGE('',*,*,#8381,.F.);
#12060=ORIENTED_EDGE('',*,*,#8384,.F.);
#12061=ORIENTED_EDGE('',*,*,#8485,.F.);
#12062=ORIENTED_EDGE('',*,*,#8389,.F.);
#12063=ORIENTED_EDGE('',*,*,#8486,.F.);
#12064=ORIENTED_EDGE('',*,*,#8413,.T.);
#12065=ORIENTED_EDGE('',*,*,#8482,.T.);
#12066=ORIENTED_EDGE('',*,*,#8411,.T.);
#12067=ORIENTED_EDGE('',*,*,#8408,.T.);
#12068=ORIENTED_EDGE('',*,*,#8405,.T.);
#12069=ORIENTED_EDGE('',*,*,#8402,.T.);
#12070=ORIENTED_EDGE('',*,*,#8399,.T.);
#12071=ORIENTED_EDGE('',*,*,#8396,.T.);
#12072=ORIENTED_EDGE('',*,*,#8393,.T.);
#12073=ORIENTED_EDGE('',*,*,#8386,.T.);
#12074=ORIENTED_EDGE('',*,*,#8485,.T.);
#12075=ORIENTED_EDGE('',*,*,#8383,.F.);
#12076=ORIENTED_EDGE('',*,*,#8484,.T.);
#12077=ORIENTED_EDGE('',*,*,#8308,.F.);
#12078=ORIENTED_EDGE('',*,*,#8487,.T.);
#12079=ORIENTED_EDGE('',*,*,#8337,.T.);
#12080=ORIENTED_EDGE('',*,*,#8488,.T.);
#12081=ORIENTED_EDGE('',*,*,#8311,.F.);
#12082=ORIENTED_EDGE('',*,*,#8357,.T.);
#12083=ORIENTED_EDGE('',*,*,#8489,.T.);
#12084=ORIENTED_EDGE('',*,*,#8354,.F.);
#12085=ORIENTED_EDGE('',*,*,#8490,.F.);
#12086=ORIENTED_EDGE('',*,*,#8488,.F.);
#12087=ORIENTED_EDGE('',*,*,#8336,.F.);
#12088=ORIENTED_EDGE('',*,*,#8340,.F.);
#12089=ORIENTED_EDGE('',*,*,#8343,.F.);
#12090=ORIENTED_EDGE('',*,*,#8346,.F.);
#12091=ORIENTED_EDGE('',*,*,#8349,.F.);
#12092=ORIENTED_EDGE('',*,*,#8352,.F.);
#12093=ORIENTED_EDGE('',*,*,#8355,.F.);
#12094=ORIENTED_EDGE('',*,*,#8489,.F.);
#12095=ORIENTED_EDGE('',*,*,#8360,.F.);
#12096=ORIENTED_EDGE('',*,*,#8491,.F.);
#12097=ORIENTED_EDGE('',*,*,#8332,.F.);
#12098=ORIENTED_EDGE('',*,*,#8492,.F.);
#12099=ORIENTED_EDGE('',*,*,#8330,.F.);
#12100=ORIENTED_EDGE('',*,*,#8327,.F.);
#12101=ORIENTED_EDGE('',*,*,#8324,.F.);
#12102=ORIENTED_EDGE('',*,*,#8321,.F.);
#12103=ORIENTED_EDGE('',*,*,#8318,.F.);
#12104=ORIENTED_EDGE('',*,*,#8315,.F.);
#12105=ORIENTED_EDGE('',*,*,#8312,.F.);
#12106=ORIENTED_EDGE('',*,*,#8487,.F.);
#12107=ORIENTED_EDGE('',*,*,#8307,.F.);
#12108=ORIENTED_EDGE('',*,*,#8314,.F.);
#12109=ORIENTED_EDGE('',*,*,#8317,.F.);
#12110=ORIENTED_EDGE('',*,*,#8320,.F.);
#12111=ORIENTED_EDGE('',*,*,#8323,.F.);
#12112=ORIENTED_EDGE('',*,*,#8326,.F.);
#12113=ORIENTED_EDGE('',*,*,#8329,.F.);
#12114=ORIENTED_EDGE('',*,*,#8493,.F.);
#12115=ORIENTED_EDGE('',*,*,#8334,.F.);
#12116=ORIENTED_EDGE('',*,*,#8494,.F.);
#12117=ORIENTED_EDGE('',*,*,#8358,.T.);
#12118=ORIENTED_EDGE('',*,*,#8490,.T.);
#12119=ORIENTED_EDGE('',*,*,#8356,.T.);
#12120=ORIENTED_EDGE('',*,*,#8353,.T.);
#12121=ORIENTED_EDGE('',*,*,#8350,.T.);
#12122=ORIENTED_EDGE('',*,*,#8347,.T.);
#12123=ORIENTED_EDGE('',*,*,#8344,.T.);
#12124=ORIENTED_EDGE('',*,*,#8341,.T.);
#12125=ORIENTED_EDGE('',*,*,#8338,.T.);
#12126=ORIENTED_EDGE('',*,*,#8331,.T.);
#12127=ORIENTED_EDGE('',*,*,#8493,.T.);
#12128=ORIENTED_EDGE('',*,*,#8328,.F.);
#12129=ORIENTED_EDGE('',*,*,#8492,.T.);
#12130=ORIENTED_EDGE('',*,*,#8365,.F.);
#12131=ORIENTED_EDGE('',*,*,#8420,.F.);
#12132=ORIENTED_EDGE('',*,*,#8310,.F.);
#12133=ORIENTED_EDGE('',*,*,#8495,.F.);
#12134=ORIENTED_EDGE('',*,*,#8496,.F.);
#12135=ORIENTED_EDGE('',*,*,#8496,.T.);
#12136=ORIENTED_EDGE('',*,*,#8497,.F.);
#12137=ORIENTED_EDGE('',*,*,#8498,.T.);
#12138=ORIENTED_EDGE('',*,*,#8499,.T.);
#12139=ORIENTED_EDGE('',*,*,#8498,.F.);
#12140=ORIENTED_EDGE('',*,*,#8497,.T.);
#12141=ORIENTED_EDGE('',*,*,#8478,.T.);
#12142=ORIENTED_EDGE('',*,*,#8443,.T.);
#12143=ORIENTED_EDGE('',*,*,#8475,.T.);
#12144=ORIENTED_EDGE('',*,*,#8469,.T.);
#12145=ORIENTED_EDGE('',*,*,#8486,.T.);
#12146=ORIENTED_EDGE('',*,*,#8388,.T.);
#12147=ORIENTED_EDGE('',*,*,#8483,.T.);
#12148=ORIENTED_EDGE('',*,*,#8414,.T.);
#12149=ORIENTED_EDGE('',*,*,#8494,.T.);
#12150=ORIENTED_EDGE('',*,*,#8333,.T.);
#12151=ORIENTED_EDGE('',*,*,#8491,.T.);
#12152=ORIENTED_EDGE('',*,*,#8359,.T.);
#12153=ORIENTED_EDGE('',*,*,#8495,.T.);
#12154=ORIENTED_EDGE('',*,*,#8499,.F.);
#12155=ORIENTED_EDGE('',*,*,#8500,.F.);
#12156=ORIENTED_EDGE('',*,*,#8501,.T.);
#12157=ORIENTED_EDGE('',*,*,#8502,.F.);
#12158=ORIENTED_EDGE('',*,*,#8501,.F.);
#12159=ORIENTED_EDGE('',*,*,#8503,.F.);
#12160=ORIENTED_EDGE('',*,*,#8504,.T.);
#12161=ORIENTED_EDGE('',*,*,#8505,.F.);
#12162=ORIENTED_EDGE('',*,*,#8504,.F.);
#12163=ORIENTED_EDGE('',*,*,#8506,.F.);
#12164=ORIENTED_EDGE('',*,*,#8507,.T.);
#12165=ORIENTED_EDGE('',*,*,#8508,.F.);
#12166=ORIENTED_EDGE('',*,*,#8507,.F.);
#12167=ORIENTED_EDGE('',*,*,#8509,.F.);
#12168=ORIENTED_EDGE('',*,*,#8510,.T.);
#12169=ORIENTED_EDGE('',*,*,#8511,.F.);
#12170=ORIENTED_EDGE('',*,*,#8510,.F.);
#12171=ORIENTED_EDGE('',*,*,#8512,.F.);
#12172=ORIENTED_EDGE('',*,*,#8513,.T.);
#12173=ORIENTED_EDGE('',*,*,#8511,.T.);
#12174=ORIENTED_EDGE('',*,*,#8513,.F.);
#12175=ORIENTED_EDGE('',*,*,#8514,.F.);
#12176=ORIENTED_EDGE('',*,*,#8515,.T.);
#12177=ORIENTED_EDGE('',*,*,#8516,.T.);
#12178=ORIENTED_EDGE('',*,*,#8515,.F.);
#12179=ORIENTED_EDGE('',*,*,#8514,.T.);
#12180=ORIENTED_EDGE('',*,*,#8500,.T.);
#12181=ORIENTED_EDGE('',*,*,#8503,.T.);
#12182=ORIENTED_EDGE('',*,*,#8506,.T.);
#12183=ORIENTED_EDGE('',*,*,#8512,.T.);
#12184=ORIENTED_EDGE('',*,*,#8516,.F.);
#12185=ORIENTED_EDGE('',*,*,#8502,.T.);
#12186=ORIENTED_EDGE('',*,*,#8505,.T.);
#12187=ORIENTED_EDGE('',*,*,#8508,.T.);
#12188=ORIENTED_EDGE('',*,*,#8509,.T.);
#12189=ORIENTED_EDGE('',*,*,#8517,.F.);
#12190=ORIENTED_EDGE('',*,*,#8518,.T.);
#12191=ORIENTED_EDGE('',*,*,#8519,.T.);
#12192=ORIENTED_EDGE('',*,*,#8520,.T.);
#12193=ORIENTED_EDGE('',*,*,#8521,.F.);
#12194=ORIENTED_EDGE('',*,*,#8522,.T.);
#12195=ORIENTED_EDGE('',*,*,#8517,.T.);
#12196=ORIENTED_EDGE('',*,*,#8523,.T.);
#12197=ORIENTED_EDGE('',*,*,#8524,.F.);
#12198=ORIENTED_EDGE('',*,*,#8525,.T.);
#12199=ORIENTED_EDGE('',*,*,#8521,.T.);
#12200=ORIENTED_EDGE('',*,*,#8526,.T.);
#12201=ORIENTED_EDGE('',*,*,#8527,.F.);
#12202=ORIENTED_EDGE('',*,*,#8528,.T.);
#12203=ORIENTED_EDGE('',*,*,#8524,.T.);
#12204=ORIENTED_EDGE('',*,*,#8529,.T.);
#12205=ORIENTED_EDGE('',*,*,#8530,.F.);
#12206=ORIENTED_EDGE('',*,*,#8531,.T.);
#12207=ORIENTED_EDGE('',*,*,#8527,.T.);
#12208=ORIENTED_EDGE('',*,*,#8532,.T.);
#12209=ORIENTED_EDGE('',*,*,#8533,.F.);
#12210=ORIENTED_EDGE('',*,*,#8534,.T.);
#12211=ORIENTED_EDGE('',*,*,#8530,.T.);
#12212=ORIENTED_EDGE('',*,*,#8535,.T.);
#12213=ORIENTED_EDGE('',*,*,#8536,.F.);
#12214=ORIENTED_EDGE('',*,*,#8537,.T.);
#12215=ORIENTED_EDGE('',*,*,#8533,.T.);
#12216=ORIENTED_EDGE('',*,*,#8538,.T.);
#12217=ORIENTED_EDGE('',*,*,#8539,.F.);
#12218=ORIENTED_EDGE('',*,*,#8540,.T.);
#12219=ORIENTED_EDGE('',*,*,#8536,.T.);
#12220=ORIENTED_EDGE('',*,*,#8541,.T.);
#12221=ORIENTED_EDGE('',*,*,#8542,.F.);
#12222=ORIENTED_EDGE('',*,*,#8543,.T.);
#12223=ORIENTED_EDGE('',*,*,#8539,.T.);
#12224=ORIENTED_EDGE('',*,*,#8544,.T.);
#12225=ORIENTED_EDGE('',*,*,#8545,.F.);
#12226=ORIENTED_EDGE('',*,*,#8546,.T.);
#12227=ORIENTED_EDGE('',*,*,#8542,.T.);
#12228=ORIENTED_EDGE('',*,*,#8547,.T.);
#12229=ORIENTED_EDGE('',*,*,#8548,.F.);
#12230=ORIENTED_EDGE('',*,*,#8549,.T.);
#12231=ORIENTED_EDGE('',*,*,#8545,.T.);
#12232=ORIENTED_EDGE('',*,*,#8550,.T.);
#12233=ORIENTED_EDGE('',*,*,#8551,.F.);
#12234=ORIENTED_EDGE('',*,*,#8552,.T.);
#12235=ORIENTED_EDGE('',*,*,#8548,.T.);
#12236=ORIENTED_EDGE('',*,*,#8553,.T.);
#12237=ORIENTED_EDGE('',*,*,#8554,.F.);
#12238=ORIENTED_EDGE('',*,*,#8555,.T.);
#12239=ORIENTED_EDGE('',*,*,#8551,.T.);
#12240=ORIENTED_EDGE('',*,*,#8556,.T.);
#12241=ORIENTED_EDGE('',*,*,#8557,.F.);
#12242=ORIENTED_EDGE('',*,*,#8558,.T.);
#12243=ORIENTED_EDGE('',*,*,#8554,.T.);
#12244=ORIENTED_EDGE('',*,*,#8559,.T.);
#12245=ORIENTED_EDGE('',*,*,#8560,.F.);
#12246=ORIENTED_EDGE('',*,*,#8561,.T.);
#12247=ORIENTED_EDGE('',*,*,#8557,.T.);
#12248=ORIENTED_EDGE('',*,*,#8562,.T.);
#12249=ORIENTED_EDGE('',*,*,#8563,.F.);
#12250=ORIENTED_EDGE('',*,*,#8564,.T.);
#12251=ORIENTED_EDGE('',*,*,#8560,.T.);
#12252=ORIENTED_EDGE('',*,*,#8565,.T.);
#12253=ORIENTED_EDGE('',*,*,#8566,.F.);
#12254=ORIENTED_EDGE('',*,*,#8567,.T.);
#12255=ORIENTED_EDGE('',*,*,#8563,.T.);
#12256=ORIENTED_EDGE('',*,*,#8568,.T.);
#12257=ORIENTED_EDGE('',*,*,#8569,.F.);
#12258=ORIENTED_EDGE('',*,*,#8570,.T.);
#12259=ORIENTED_EDGE('',*,*,#8566,.T.);
#12260=ORIENTED_EDGE('',*,*,#8571,.T.);
#12261=ORIENTED_EDGE('',*,*,#8572,.F.);
#12262=ORIENTED_EDGE('',*,*,#8573,.T.);
#12263=ORIENTED_EDGE('',*,*,#8569,.T.);
#12264=ORIENTED_EDGE('',*,*,#8574,.T.);
#12265=ORIENTED_EDGE('',*,*,#8575,.F.);
#12266=ORIENTED_EDGE('',*,*,#8576,.T.);
#12267=ORIENTED_EDGE('',*,*,#8572,.T.);
#12268=ORIENTED_EDGE('',*,*,#8577,.T.);
#12269=ORIENTED_EDGE('',*,*,#8578,.F.);
#12270=ORIENTED_EDGE('',*,*,#8579,.T.);
#12271=ORIENTED_EDGE('',*,*,#8575,.T.);
#12272=ORIENTED_EDGE('',*,*,#8580,.T.);
#12273=ORIENTED_EDGE('',*,*,#8581,.F.);
#12274=ORIENTED_EDGE('',*,*,#8582,.T.);
#12275=ORIENTED_EDGE('',*,*,#8578,.T.);
#12276=ORIENTED_EDGE('',*,*,#8583,.T.);
#12277=ORIENTED_EDGE('',*,*,#8584,.F.);
#12278=ORIENTED_EDGE('',*,*,#8585,.T.);
#12279=ORIENTED_EDGE('',*,*,#8581,.T.);
#12280=ORIENTED_EDGE('',*,*,#8586,.T.);
#12281=ORIENTED_EDGE('',*,*,#8587,.F.);
#12282=ORIENTED_EDGE('',*,*,#8588,.T.);
#12283=ORIENTED_EDGE('',*,*,#8584,.T.);
#12284=ORIENTED_EDGE('',*,*,#8589,.T.);
#12285=ORIENTED_EDGE('',*,*,#8590,.F.);
#12286=ORIENTED_EDGE('',*,*,#8591,.T.);
#12287=ORIENTED_EDGE('',*,*,#8587,.T.);
#12288=ORIENTED_EDGE('',*,*,#8592,.T.);
#12289=ORIENTED_EDGE('',*,*,#8593,.F.);
#12290=ORIENTED_EDGE('',*,*,#8594,.T.);
#12291=ORIENTED_EDGE('',*,*,#8590,.T.);
#12292=ORIENTED_EDGE('',*,*,#8595,.T.);
#12293=ORIENTED_EDGE('',*,*,#8596,.F.);
#12294=ORIENTED_EDGE('',*,*,#8597,.T.);
#12295=ORIENTED_EDGE('',*,*,#8593,.T.);
#12296=ORIENTED_EDGE('',*,*,#8598,.T.);
#12297=ORIENTED_EDGE('',*,*,#8599,.F.);
#12298=ORIENTED_EDGE('',*,*,#8600,.T.);
#12299=ORIENTED_EDGE('',*,*,#8596,.T.);
#12300=ORIENTED_EDGE('',*,*,#8601,.T.);
#12301=ORIENTED_EDGE('',*,*,#8602,.F.);
#12302=ORIENTED_EDGE('',*,*,#8603,.T.);
#12303=ORIENTED_EDGE('',*,*,#8599,.T.);
#12304=ORIENTED_EDGE('',*,*,#8604,.T.);
#12305=ORIENTED_EDGE('',*,*,#8605,.F.);
#12306=ORIENTED_EDGE('',*,*,#8606,.T.);
#12307=ORIENTED_EDGE('',*,*,#8602,.T.);
#12308=ORIENTED_EDGE('',*,*,#8607,.T.);
#12309=ORIENTED_EDGE('',*,*,#8608,.F.);
#12310=ORIENTED_EDGE('',*,*,#8609,.T.);
#12311=ORIENTED_EDGE('',*,*,#8605,.T.);
#12312=ORIENTED_EDGE('',*,*,#8610,.T.);
#12313=ORIENTED_EDGE('',*,*,#8611,.F.);
#12314=ORIENTED_EDGE('',*,*,#8612,.T.);
#12315=ORIENTED_EDGE('',*,*,#8608,.T.);
#12316=ORIENTED_EDGE('',*,*,#8613,.T.);
#12317=ORIENTED_EDGE('',*,*,#8614,.F.);
#12318=ORIENTED_EDGE('',*,*,#8615,.T.);
#12319=ORIENTED_EDGE('',*,*,#8611,.T.);
#12320=ORIENTED_EDGE('',*,*,#8616,.T.);
#12321=ORIENTED_EDGE('',*,*,#8617,.F.);
#12322=ORIENTED_EDGE('',*,*,#8618,.T.);
#12323=ORIENTED_EDGE('',*,*,#8614,.T.);
#12324=ORIENTED_EDGE('',*,*,#8619,.T.);
#12325=ORIENTED_EDGE('',*,*,#8620,.F.);
#12326=ORIENTED_EDGE('',*,*,#8621,.T.);
#12327=ORIENTED_EDGE('',*,*,#8617,.T.);
#12328=ORIENTED_EDGE('',*,*,#8622,.T.);
#12329=ORIENTED_EDGE('',*,*,#8623,.F.);
#12330=ORIENTED_EDGE('',*,*,#8624,.T.);
#12331=ORIENTED_EDGE('',*,*,#8620,.T.);
#12332=ORIENTED_EDGE('',*,*,#8625,.T.);
#12333=ORIENTED_EDGE('',*,*,#8626,.F.);
#12334=ORIENTED_EDGE('',*,*,#8627,.T.);
#12335=ORIENTED_EDGE('',*,*,#8623,.T.);
#12336=ORIENTED_EDGE('',*,*,#8628,.T.);
#12337=ORIENTED_EDGE('',*,*,#8629,.F.);
#12338=ORIENTED_EDGE('',*,*,#8630,.T.);
#12339=ORIENTED_EDGE('',*,*,#8626,.T.);
#12340=ORIENTED_EDGE('',*,*,#8631,.T.);
#12341=ORIENTED_EDGE('',*,*,#8632,.F.);
#12342=ORIENTED_EDGE('',*,*,#8633,.T.);
#12343=ORIENTED_EDGE('',*,*,#8629,.T.);
#12344=ORIENTED_EDGE('',*,*,#8634,.T.);
#12345=ORIENTED_EDGE('',*,*,#8635,.F.);
#12346=ORIENTED_EDGE('',*,*,#8636,.T.);
#12347=ORIENTED_EDGE('',*,*,#8632,.T.);
#12348=ORIENTED_EDGE('',*,*,#8637,.T.);
#12349=ORIENTED_EDGE('',*,*,#8638,.F.);
#12350=ORIENTED_EDGE('',*,*,#8639,.T.);
#12351=ORIENTED_EDGE('',*,*,#8635,.T.);
#12352=ORIENTED_EDGE('',*,*,#8640,.T.);
#12353=ORIENTED_EDGE('',*,*,#8641,.F.);
#12354=ORIENTED_EDGE('',*,*,#8642,.T.);
#12355=ORIENTED_EDGE('',*,*,#8638,.T.);
#12356=ORIENTED_EDGE('',*,*,#8643,.T.);
#12357=ORIENTED_EDGE('',*,*,#8644,.F.);
#12358=ORIENTED_EDGE('',*,*,#8645,.T.);
#12359=ORIENTED_EDGE('',*,*,#8641,.T.);
#12360=ORIENTED_EDGE('',*,*,#8646,.T.);
#12361=ORIENTED_EDGE('',*,*,#8647,.F.);
#12362=ORIENTED_EDGE('',*,*,#8648,.T.);
#12363=ORIENTED_EDGE('',*,*,#8644,.T.);
#12364=ORIENTED_EDGE('',*,*,#8649,.T.);
#12365=ORIENTED_EDGE('',*,*,#8650,.F.);
#12366=ORIENTED_EDGE('',*,*,#8651,.T.);
#12367=ORIENTED_EDGE('',*,*,#8647,.T.);
#12368=ORIENTED_EDGE('',*,*,#8652,.T.);
#12369=ORIENTED_EDGE('',*,*,#8653,.F.);
#12370=ORIENTED_EDGE('',*,*,#8654,.T.);
#12371=ORIENTED_EDGE('',*,*,#8650,.T.);
#12372=ORIENTED_EDGE('',*,*,#8655,.T.);
#12373=ORIENTED_EDGE('',*,*,#8656,.F.);
#12374=ORIENTED_EDGE('',*,*,#8657,.T.);
#12375=ORIENTED_EDGE('',*,*,#8653,.T.);
#12376=ORIENTED_EDGE('',*,*,#8658,.T.);
#12377=ORIENTED_EDGE('',*,*,#8659,.F.);
#12378=ORIENTED_EDGE('',*,*,#8660,.T.);
#12379=ORIENTED_EDGE('',*,*,#8656,.T.);
#12380=ORIENTED_EDGE('',*,*,#8661,.T.);
#12381=ORIENTED_EDGE('',*,*,#8662,.F.);
#12382=ORIENTED_EDGE('',*,*,#8663,.T.);
#12383=ORIENTED_EDGE('',*,*,#8659,.T.);
#12384=ORIENTED_EDGE('',*,*,#8664,.T.);
#12385=ORIENTED_EDGE('',*,*,#8665,.F.);
#12386=ORIENTED_EDGE('',*,*,#8666,.T.);
#12387=ORIENTED_EDGE('',*,*,#8662,.T.);
#12388=ORIENTED_EDGE('',*,*,#8667,.T.);
#12389=ORIENTED_EDGE('',*,*,#8668,.F.);
#12390=ORIENTED_EDGE('',*,*,#8669,.T.);
#12391=ORIENTED_EDGE('',*,*,#8665,.T.);
#12392=ORIENTED_EDGE('',*,*,#8670,.T.);
#12393=ORIENTED_EDGE('',*,*,#8671,.F.);
#12394=ORIENTED_EDGE('',*,*,#8672,.T.);
#12395=ORIENTED_EDGE('',*,*,#8668,.T.);
#12396=ORIENTED_EDGE('',*,*,#8673,.T.);
#12397=ORIENTED_EDGE('',*,*,#8674,.F.);
#12398=ORIENTED_EDGE('',*,*,#8675,.T.);
#12399=ORIENTED_EDGE('',*,*,#8671,.T.);
#12400=ORIENTED_EDGE('',*,*,#8676,.T.);
#12401=ORIENTED_EDGE('',*,*,#8677,.F.);
#12402=ORIENTED_EDGE('',*,*,#8678,.T.);
#12403=ORIENTED_EDGE('',*,*,#8674,.T.);
#12404=ORIENTED_EDGE('',*,*,#8679,.T.);
#12405=ORIENTED_EDGE('',*,*,#8680,.F.);
#12406=ORIENTED_EDGE('',*,*,#8681,.T.);
#12407=ORIENTED_EDGE('',*,*,#8677,.T.);
#12408=ORIENTED_EDGE('',*,*,#8682,.T.);
#12409=ORIENTED_EDGE('',*,*,#8683,.F.);
#12410=ORIENTED_EDGE('',*,*,#8684,.T.);
#12411=ORIENTED_EDGE('',*,*,#8680,.T.);
#12412=ORIENTED_EDGE('',*,*,#8685,.T.);
#12413=ORIENTED_EDGE('',*,*,#8686,.F.);
#12414=ORIENTED_EDGE('',*,*,#8687,.T.);
#12415=ORIENTED_EDGE('',*,*,#8683,.T.);
#12416=ORIENTED_EDGE('',*,*,#8688,.T.);
#12417=ORIENTED_EDGE('',*,*,#8689,.F.);
#12418=ORIENTED_EDGE('',*,*,#8690,.T.);
#12419=ORIENTED_EDGE('',*,*,#8686,.T.);
#12420=ORIENTED_EDGE('',*,*,#8691,.T.);
#12421=ORIENTED_EDGE('',*,*,#8692,.F.);
#12422=ORIENTED_EDGE('',*,*,#8693,.T.);
#12423=ORIENTED_EDGE('',*,*,#8689,.T.);
#12424=ORIENTED_EDGE('',*,*,#8694,.T.);
#12425=ORIENTED_EDGE('',*,*,#8695,.F.);
#12426=ORIENTED_EDGE('',*,*,#8696,.T.);
#12427=ORIENTED_EDGE('',*,*,#8692,.T.);
#12428=ORIENTED_EDGE('',*,*,#8697,.T.);
#12429=ORIENTED_EDGE('',*,*,#8698,.F.);
#12430=ORIENTED_EDGE('',*,*,#8699,.T.);
#12431=ORIENTED_EDGE('',*,*,#8700,.F.);
#12432=ORIENTED_EDGE('',*,*,#8701,.F.);
#12433=ORIENTED_EDGE('',*,*,#8702,.F.);
#12434=ORIENTED_EDGE('',*,*,#8703,.T.);
#12435=ORIENTED_EDGE('',*,*,#8698,.T.);
#12436=ORIENTED_EDGE('',*,*,#8704,.F.);
#12437=ORIENTED_EDGE('',*,*,#8705,.F.);
#12438=ORIENTED_EDGE('',*,*,#8706,.T.);
#12439=ORIENTED_EDGE('',*,*,#8702,.T.);
#12440=ORIENTED_EDGE('',*,*,#8707,.F.);
#12441=ORIENTED_EDGE('',*,*,#8708,.F.);
#12442=ORIENTED_EDGE('',*,*,#8709,.T.);
#12443=ORIENTED_EDGE('',*,*,#8705,.T.);
#12444=ORIENTED_EDGE('',*,*,#8710,.F.);
#12445=ORIENTED_EDGE('',*,*,#8711,.F.);
#12446=ORIENTED_EDGE('',*,*,#8712,.T.);
#12447=ORIENTED_EDGE('',*,*,#8708,.T.);
#12448=ORIENTED_EDGE('',*,*,#8713,.F.);
#12449=ORIENTED_EDGE('',*,*,#8714,.F.);
#12450=ORIENTED_EDGE('',*,*,#8715,.T.);
#12451=ORIENTED_EDGE('',*,*,#8711,.T.);
#12452=ORIENTED_EDGE('',*,*,#8716,.F.);
#12453=ORIENTED_EDGE('',*,*,#8717,.F.);
#12454=ORIENTED_EDGE('',*,*,#8718,.T.);
#12455=ORIENTED_EDGE('',*,*,#8714,.T.);
#12456=ORIENTED_EDGE('',*,*,#8719,.F.);
#12457=ORIENTED_EDGE('',*,*,#8720,.F.);
#12458=ORIENTED_EDGE('',*,*,#8721,.T.);
#12459=ORIENTED_EDGE('',*,*,#8717,.T.);
#12460=ORIENTED_EDGE('',*,*,#8722,.F.);
#12461=ORIENTED_EDGE('',*,*,#8723,.F.);
#12462=ORIENTED_EDGE('',*,*,#8724,.T.);
#12463=ORIENTED_EDGE('',*,*,#8720,.T.);
#12464=ORIENTED_EDGE('',*,*,#8725,.F.);
#12465=ORIENTED_EDGE('',*,*,#8726,.F.);
#12466=ORIENTED_EDGE('',*,*,#8727,.T.);
#12467=ORIENTED_EDGE('',*,*,#8723,.T.);
#12468=ORIENTED_EDGE('',*,*,#8728,.F.);
#12469=ORIENTED_EDGE('',*,*,#8729,.F.);
#12470=ORIENTED_EDGE('',*,*,#8730,.T.);
#12471=ORIENTED_EDGE('',*,*,#8726,.T.);
#12472=ORIENTED_EDGE('',*,*,#8731,.F.);
#12473=ORIENTED_EDGE('',*,*,#8732,.F.);
#12474=ORIENTED_EDGE('',*,*,#8733,.T.);
#12475=ORIENTED_EDGE('',*,*,#8729,.T.);
#12476=ORIENTED_EDGE('',*,*,#8734,.F.);
#12477=ORIENTED_EDGE('',*,*,#8735,.F.);
#12478=ORIENTED_EDGE('',*,*,#8736,.T.);
#12479=ORIENTED_EDGE('',*,*,#8732,.T.);
#12480=ORIENTED_EDGE('',*,*,#8737,.F.);
#12481=ORIENTED_EDGE('',*,*,#8738,.F.);
#12482=ORIENTED_EDGE('',*,*,#8739,.T.);
#12483=ORIENTED_EDGE('',*,*,#8735,.T.);
#12484=ORIENTED_EDGE('',*,*,#8740,.F.);
#12485=ORIENTED_EDGE('',*,*,#8741,.F.);
#12486=ORIENTED_EDGE('',*,*,#8742,.T.);
#12487=ORIENTED_EDGE('',*,*,#8738,.T.);
#12488=ORIENTED_EDGE('',*,*,#8743,.F.);
#12489=ORIENTED_EDGE('',*,*,#8744,.F.);
#12490=ORIENTED_EDGE('',*,*,#8745,.T.);
#12491=ORIENTED_EDGE('',*,*,#8741,.T.);
#12492=ORIENTED_EDGE('',*,*,#8746,.F.);
#12493=ORIENTED_EDGE('',*,*,#8747,.F.);
#12494=ORIENTED_EDGE('',*,*,#8748,.T.);
#12495=ORIENTED_EDGE('',*,*,#8744,.T.);
#12496=ORIENTED_EDGE('',*,*,#8749,.F.);
#12497=ORIENTED_EDGE('',*,*,#8750,.F.);
#12498=ORIENTED_EDGE('',*,*,#8751,.T.);
#12499=ORIENTED_EDGE('',*,*,#8747,.T.);
#12500=ORIENTED_EDGE('',*,*,#8752,.F.);
#12501=ORIENTED_EDGE('',*,*,#8753,.F.);
#12502=ORIENTED_EDGE('',*,*,#8754,.T.);
#12503=ORIENTED_EDGE('',*,*,#8750,.T.);
#12504=ORIENTED_EDGE('',*,*,#8755,.F.);
#12505=ORIENTED_EDGE('',*,*,#8756,.F.);
#12506=ORIENTED_EDGE('',*,*,#8757,.T.);
#12507=ORIENTED_EDGE('',*,*,#8753,.T.);
#12508=ORIENTED_EDGE('',*,*,#8758,.F.);
#12509=ORIENTED_EDGE('',*,*,#8759,.F.);
#12510=ORIENTED_EDGE('',*,*,#8760,.T.);
#12511=ORIENTED_EDGE('',*,*,#8756,.T.);
#12512=ORIENTED_EDGE('',*,*,#8761,.F.);
#12513=ORIENTED_EDGE('',*,*,#8762,.F.);
#12514=ORIENTED_EDGE('',*,*,#8763,.T.);
#12515=ORIENTED_EDGE('',*,*,#8759,.T.);
#12516=ORIENTED_EDGE('',*,*,#8764,.F.);
#12517=ORIENTED_EDGE('',*,*,#8765,.F.);
#12518=ORIENTED_EDGE('',*,*,#8766,.T.);
#12519=ORIENTED_EDGE('',*,*,#8762,.T.);
#12520=ORIENTED_EDGE('',*,*,#8767,.F.);
#12521=ORIENTED_EDGE('',*,*,#8768,.F.);
#12522=ORIENTED_EDGE('',*,*,#8769,.T.);
#12523=ORIENTED_EDGE('',*,*,#8765,.T.);
#12524=ORIENTED_EDGE('',*,*,#8770,.F.);
#12525=ORIENTED_EDGE('',*,*,#8771,.F.);
#12526=ORIENTED_EDGE('',*,*,#8772,.T.);
#12527=ORIENTED_EDGE('',*,*,#8768,.T.);
#12528=ORIENTED_EDGE('',*,*,#8773,.F.);
#12529=ORIENTED_EDGE('',*,*,#8774,.F.);
#12530=ORIENTED_EDGE('',*,*,#8775,.T.);
#12531=ORIENTED_EDGE('',*,*,#8771,.T.);
#12532=ORIENTED_EDGE('',*,*,#8776,.F.);
#12533=ORIENTED_EDGE('',*,*,#8777,.F.);
#12534=ORIENTED_EDGE('',*,*,#8778,.T.);
#12535=ORIENTED_EDGE('',*,*,#8774,.T.);
#12536=ORIENTED_EDGE('',*,*,#8779,.F.);
#12537=ORIENTED_EDGE('',*,*,#8780,.F.);
#12538=ORIENTED_EDGE('',*,*,#8781,.T.);
#12539=ORIENTED_EDGE('',*,*,#8777,.T.);
#12540=ORIENTED_EDGE('',*,*,#8782,.F.);
#12541=ORIENTED_EDGE('',*,*,#8783,.F.);
#12542=ORIENTED_EDGE('',*,*,#8784,.T.);
#12543=ORIENTED_EDGE('',*,*,#8780,.T.);
#12544=ORIENTED_EDGE('',*,*,#8785,.F.);
#12545=ORIENTED_EDGE('',*,*,#8786,.F.);
#12546=ORIENTED_EDGE('',*,*,#8787,.T.);
#12547=ORIENTED_EDGE('',*,*,#8783,.T.);
#12548=ORIENTED_EDGE('',*,*,#8788,.F.);
#12549=ORIENTED_EDGE('',*,*,#8789,.F.);
#12550=ORIENTED_EDGE('',*,*,#8790,.T.);
#12551=ORIENTED_EDGE('',*,*,#8786,.T.);
#12552=ORIENTED_EDGE('',*,*,#8791,.F.);
#12553=ORIENTED_EDGE('',*,*,#8792,.F.);
#12554=ORIENTED_EDGE('',*,*,#8793,.T.);
#12555=ORIENTED_EDGE('',*,*,#8789,.T.);
#12556=ORIENTED_EDGE('',*,*,#8794,.F.);
#12557=ORIENTED_EDGE('',*,*,#8795,.F.);
#12558=ORIENTED_EDGE('',*,*,#8796,.T.);
#12559=ORIENTED_EDGE('',*,*,#8792,.T.);
#12560=ORIENTED_EDGE('',*,*,#8797,.F.);
#12561=ORIENTED_EDGE('',*,*,#8798,.F.);
#12562=ORIENTED_EDGE('',*,*,#8799,.T.);
#12563=ORIENTED_EDGE('',*,*,#8795,.T.);
#12564=ORIENTED_EDGE('',*,*,#8800,.F.);
#12565=ORIENTED_EDGE('',*,*,#8801,.F.);
#12566=ORIENTED_EDGE('',*,*,#8802,.T.);
#12567=ORIENTED_EDGE('',*,*,#8798,.T.);
#12568=ORIENTED_EDGE('',*,*,#8803,.F.);
#12569=ORIENTED_EDGE('',*,*,#8804,.F.);
#12570=ORIENTED_EDGE('',*,*,#8805,.T.);
#12571=ORIENTED_EDGE('',*,*,#8801,.T.);
#12572=ORIENTED_EDGE('',*,*,#8806,.F.);
#12573=ORIENTED_EDGE('',*,*,#8807,.F.);
#12574=ORIENTED_EDGE('',*,*,#8808,.T.);
#12575=ORIENTED_EDGE('',*,*,#8804,.T.);
#12576=ORIENTED_EDGE('',*,*,#8809,.F.);
#12577=ORIENTED_EDGE('',*,*,#8810,.F.);
#12578=ORIENTED_EDGE('',*,*,#8811,.T.);
#12579=ORIENTED_EDGE('',*,*,#8807,.T.);
#12580=ORIENTED_EDGE('',*,*,#8812,.F.);
#12581=ORIENTED_EDGE('',*,*,#8813,.F.);
#12582=ORIENTED_EDGE('',*,*,#8814,.T.);
#12583=ORIENTED_EDGE('',*,*,#8810,.T.);
#12584=ORIENTED_EDGE('',*,*,#8815,.F.);
#12585=ORIENTED_EDGE('',*,*,#8816,.F.);
#12586=ORIENTED_EDGE('',*,*,#8817,.T.);
#12587=ORIENTED_EDGE('',*,*,#8813,.T.);
#12588=ORIENTED_EDGE('',*,*,#8818,.F.);
#12589=ORIENTED_EDGE('',*,*,#8819,.F.);
#12590=ORIENTED_EDGE('',*,*,#8820,.T.);
#12591=ORIENTED_EDGE('',*,*,#8816,.T.);
#12592=ORIENTED_EDGE('',*,*,#8821,.F.);
#12593=ORIENTED_EDGE('',*,*,#8822,.F.);
#12594=ORIENTED_EDGE('',*,*,#8823,.T.);
#12595=ORIENTED_EDGE('',*,*,#8819,.T.);
#12596=ORIENTED_EDGE('',*,*,#8824,.F.);
#12597=ORIENTED_EDGE('',*,*,#8825,.F.);
#12598=ORIENTED_EDGE('',*,*,#8826,.T.);
#12599=ORIENTED_EDGE('',*,*,#8822,.T.);
#12600=ORIENTED_EDGE('',*,*,#8827,.F.);
#12601=ORIENTED_EDGE('',*,*,#8828,.F.);
#12602=ORIENTED_EDGE('',*,*,#8829,.T.);
#12603=ORIENTED_EDGE('',*,*,#8825,.T.);
#12604=ORIENTED_EDGE('',*,*,#8830,.F.);
#12605=ORIENTED_EDGE('',*,*,#8831,.F.);
#12606=ORIENTED_EDGE('',*,*,#8832,.T.);
#12607=ORIENTED_EDGE('',*,*,#8828,.T.);
#12608=ORIENTED_EDGE('',*,*,#8833,.F.);
#12609=ORIENTED_EDGE('',*,*,#8834,.F.);
#12610=ORIENTED_EDGE('',*,*,#8835,.T.);
#12611=ORIENTED_EDGE('',*,*,#8831,.T.);
#12612=ORIENTED_EDGE('',*,*,#8836,.F.);
#12613=ORIENTED_EDGE('',*,*,#8837,.F.);
#12614=ORIENTED_EDGE('',*,*,#8838,.T.);
#12615=ORIENTED_EDGE('',*,*,#8834,.T.);
#12616=ORIENTED_EDGE('',*,*,#8839,.F.);
#12617=ORIENTED_EDGE('',*,*,#8840,.F.);
#12618=ORIENTED_EDGE('',*,*,#8841,.T.);
#12619=ORIENTED_EDGE('',*,*,#8837,.T.);
#12620=ORIENTED_EDGE('',*,*,#8842,.F.);
#12621=ORIENTED_EDGE('',*,*,#8843,.F.);
#12622=ORIENTED_EDGE('',*,*,#8844,.T.);
#12623=ORIENTED_EDGE('',*,*,#8840,.T.);
#12624=ORIENTED_EDGE('',*,*,#8845,.F.);
#12625=ORIENTED_EDGE('',*,*,#8846,.F.);
#12626=ORIENTED_EDGE('',*,*,#8847,.T.);
#12627=ORIENTED_EDGE('',*,*,#8843,.T.);
#12628=ORIENTED_EDGE('',*,*,#8848,.F.);
#12629=ORIENTED_EDGE('',*,*,#8849,.F.);
#12630=ORIENTED_EDGE('',*,*,#8850,.T.);
#12631=ORIENTED_EDGE('',*,*,#8846,.T.);
#12632=ORIENTED_EDGE('',*,*,#8851,.F.);
#12633=ORIENTED_EDGE('',*,*,#8852,.F.);
#12634=ORIENTED_EDGE('',*,*,#8853,.T.);
#12635=ORIENTED_EDGE('',*,*,#8849,.T.);
#12636=ORIENTED_EDGE('',*,*,#8854,.F.);
#12637=ORIENTED_EDGE('',*,*,#8855,.F.);
#12638=ORIENTED_EDGE('',*,*,#8856,.T.);
#12639=ORIENTED_EDGE('',*,*,#8852,.T.);
#12640=ORIENTED_EDGE('',*,*,#8857,.F.);
#12641=ORIENTED_EDGE('',*,*,#8858,.F.);
#12642=ORIENTED_EDGE('',*,*,#8859,.T.);
#12643=ORIENTED_EDGE('',*,*,#8855,.T.);
#12644=ORIENTED_EDGE('',*,*,#8860,.F.);
#12645=ORIENTED_EDGE('',*,*,#8861,.F.);
#12646=ORIENTED_EDGE('',*,*,#8862,.T.);
#12647=ORIENTED_EDGE('',*,*,#8858,.T.);
#12648=ORIENTED_EDGE('',*,*,#8863,.F.);
#12649=ORIENTED_EDGE('',*,*,#8864,.F.);
#12650=ORIENTED_EDGE('',*,*,#8865,.T.);
#12651=ORIENTED_EDGE('',*,*,#8861,.T.);
#12652=ORIENTED_EDGE('',*,*,#8866,.F.);
#12653=ORIENTED_EDGE('',*,*,#8867,.F.);
#12654=ORIENTED_EDGE('',*,*,#8868,.T.);
#12655=ORIENTED_EDGE('',*,*,#8864,.T.);
#12656=ORIENTED_EDGE('',*,*,#8869,.F.);
#12657=ORIENTED_EDGE('',*,*,#8870,.F.);
#12658=ORIENTED_EDGE('',*,*,#8871,.T.);
#12659=ORIENTED_EDGE('',*,*,#8867,.T.);
#12660=ORIENTED_EDGE('',*,*,#8872,.F.);
#12661=ORIENTED_EDGE('',*,*,#8873,.F.);
#12662=ORIENTED_EDGE('',*,*,#8874,.T.);
#12663=ORIENTED_EDGE('',*,*,#8870,.T.);
#12664=ORIENTED_EDGE('',*,*,#8875,.F.);
#12665=ORIENTED_EDGE('',*,*,#8876,.F.);
#12666=ORIENTED_EDGE('',*,*,#8877,.T.);
#12667=ORIENTED_EDGE('',*,*,#8873,.T.);
#12668=ORIENTED_EDGE('',*,*,#8878,.F.);
#12669=ORIENTED_EDGE('',*,*,#8879,.F.);
#12670=ORIENTED_EDGE('',*,*,#8880,.F.);
#12671=ORIENTED_EDGE('',*,*,#8697,.F.);
#12672=ORIENTED_EDGE('',*,*,#8694,.F.);
#12673=ORIENTED_EDGE('',*,*,#8691,.F.);
#12674=ORIENTED_EDGE('',*,*,#8688,.F.);
#12675=ORIENTED_EDGE('',*,*,#8685,.F.);
#12676=ORIENTED_EDGE('',*,*,#8682,.F.);
#12677=ORIENTED_EDGE('',*,*,#8679,.F.);
#12678=ORIENTED_EDGE('',*,*,#8676,.F.);
#12679=ORIENTED_EDGE('',*,*,#8673,.F.);
#12680=ORIENTED_EDGE('',*,*,#8670,.F.);
#12681=ORIENTED_EDGE('',*,*,#8667,.F.);
#12682=ORIENTED_EDGE('',*,*,#8664,.F.);
#12683=ORIENTED_EDGE('',*,*,#8661,.F.);
#12684=ORIENTED_EDGE('',*,*,#8658,.F.);
#12685=ORIENTED_EDGE('',*,*,#8655,.F.);
#12686=ORIENTED_EDGE('',*,*,#8652,.F.);
#12687=ORIENTED_EDGE('',*,*,#8649,.F.);
#12688=ORIENTED_EDGE('',*,*,#8646,.F.);
#12689=ORIENTED_EDGE('',*,*,#8643,.F.);
#12690=ORIENTED_EDGE('',*,*,#8640,.F.);
#12691=ORIENTED_EDGE('',*,*,#8637,.F.);
#12692=ORIENTED_EDGE('',*,*,#8634,.F.);
#12693=ORIENTED_EDGE('',*,*,#8631,.F.);
#12694=ORIENTED_EDGE('',*,*,#8628,.F.);
#12695=ORIENTED_EDGE('',*,*,#8625,.F.);
#12696=ORIENTED_EDGE('',*,*,#8622,.F.);
#12697=ORIENTED_EDGE('',*,*,#8619,.F.);
#12698=ORIENTED_EDGE('',*,*,#8616,.F.);
#12699=ORIENTED_EDGE('',*,*,#8613,.F.);
#12700=ORIENTED_EDGE('',*,*,#8610,.F.);
#12701=ORIENTED_EDGE('',*,*,#8607,.F.);
#12702=ORIENTED_EDGE('',*,*,#8604,.F.);
#12703=ORIENTED_EDGE('',*,*,#8601,.F.);
#12704=ORIENTED_EDGE('',*,*,#8598,.F.);
#12705=ORIENTED_EDGE('',*,*,#8595,.F.);
#12706=ORIENTED_EDGE('',*,*,#8592,.F.);
#12707=ORIENTED_EDGE('',*,*,#8589,.F.);
#12708=ORIENTED_EDGE('',*,*,#8586,.F.);
#12709=ORIENTED_EDGE('',*,*,#8583,.F.);
#12710=ORIENTED_EDGE('',*,*,#8580,.F.);
#12711=ORIENTED_EDGE('',*,*,#8577,.F.);
#12712=ORIENTED_EDGE('',*,*,#8574,.F.);
#12713=ORIENTED_EDGE('',*,*,#8571,.F.);
#12714=ORIENTED_EDGE('',*,*,#8568,.F.);
#12715=ORIENTED_EDGE('',*,*,#8565,.F.);
#12716=ORIENTED_EDGE('',*,*,#8562,.F.);
#12717=ORIENTED_EDGE('',*,*,#8559,.F.);
#12718=ORIENTED_EDGE('',*,*,#8556,.F.);
#12719=ORIENTED_EDGE('',*,*,#8553,.F.);
#12720=ORIENTED_EDGE('',*,*,#8550,.F.);
#12721=ORIENTED_EDGE('',*,*,#8547,.F.);
#12722=ORIENTED_EDGE('',*,*,#8544,.F.);
#12723=ORIENTED_EDGE('',*,*,#8541,.F.);
#12724=ORIENTED_EDGE('',*,*,#8538,.F.);
#12725=ORIENTED_EDGE('',*,*,#8535,.F.);
#12726=ORIENTED_EDGE('',*,*,#8532,.F.);
#12727=ORIENTED_EDGE('',*,*,#8529,.F.);
#12728=ORIENTED_EDGE('',*,*,#8526,.F.);
#12729=ORIENTED_EDGE('',*,*,#8523,.F.);
#12730=ORIENTED_EDGE('',*,*,#8520,.F.);
#12731=ORIENTED_EDGE('',*,*,#8881,.F.);
#12732=ORIENTED_EDGE('',*,*,#8882,.T.);
#12733=ORIENTED_EDGE('',*,*,#8878,.T.);
#12734=ORIENTED_EDGE('',*,*,#8875,.T.);
#12735=ORIENTED_EDGE('',*,*,#8872,.T.);
#12736=ORIENTED_EDGE('',*,*,#8869,.T.);
#12737=ORIENTED_EDGE('',*,*,#8866,.T.);
#12738=ORIENTED_EDGE('',*,*,#8863,.T.);
#12739=ORIENTED_EDGE('',*,*,#8860,.T.);
#12740=ORIENTED_EDGE('',*,*,#8857,.T.);
#12741=ORIENTED_EDGE('',*,*,#8854,.T.);
#12742=ORIENTED_EDGE('',*,*,#8851,.T.);
#12743=ORIENTED_EDGE('',*,*,#8848,.T.);
#12744=ORIENTED_EDGE('',*,*,#8845,.T.);
#12745=ORIENTED_EDGE('',*,*,#8842,.T.);
#12746=ORIENTED_EDGE('',*,*,#8839,.T.);
#12747=ORIENTED_EDGE('',*,*,#8836,.T.);
#12748=ORIENTED_EDGE('',*,*,#8833,.T.);
#12749=ORIENTED_EDGE('',*,*,#8830,.T.);
#12750=ORIENTED_EDGE('',*,*,#8827,.T.);
#12751=ORIENTED_EDGE('',*,*,#8824,.T.);
#12752=ORIENTED_EDGE('',*,*,#8821,.T.);
#12753=ORIENTED_EDGE('',*,*,#8818,.T.);
#12754=ORIENTED_EDGE('',*,*,#8815,.T.);
#12755=ORIENTED_EDGE('',*,*,#8812,.T.);
#12756=ORIENTED_EDGE('',*,*,#8809,.T.);
#12757=ORIENTED_EDGE('',*,*,#8806,.T.);
#12758=ORIENTED_EDGE('',*,*,#8803,.T.);
#12759=ORIENTED_EDGE('',*,*,#8800,.T.);
#12760=ORIENTED_EDGE('',*,*,#8797,.T.);
#12761=ORIENTED_EDGE('',*,*,#8794,.T.);
#12762=ORIENTED_EDGE('',*,*,#8791,.T.);
#12763=ORIENTED_EDGE('',*,*,#8788,.T.);
#12764=ORIENTED_EDGE('',*,*,#8785,.T.);
#12765=ORIENTED_EDGE('',*,*,#8782,.T.);
#12766=ORIENTED_EDGE('',*,*,#8779,.T.);
#12767=ORIENTED_EDGE('',*,*,#8776,.T.);
#12768=ORIENTED_EDGE('',*,*,#8773,.T.);
#12769=ORIENTED_EDGE('',*,*,#8770,.T.);
#12770=ORIENTED_EDGE('',*,*,#8767,.T.);
#12771=ORIENTED_EDGE('',*,*,#8764,.T.);
#12772=ORIENTED_EDGE('',*,*,#8761,.T.);
#12773=ORIENTED_EDGE('',*,*,#8758,.T.);
#12774=ORIENTED_EDGE('',*,*,#8755,.T.);
#12775=ORIENTED_EDGE('',*,*,#8752,.T.);
#12776=ORIENTED_EDGE('',*,*,#8749,.T.);
#12777=ORIENTED_EDGE('',*,*,#8746,.T.);
#12778=ORIENTED_EDGE('',*,*,#8743,.T.);
#12779=ORIENTED_EDGE('',*,*,#8740,.T.);
#12780=ORIENTED_EDGE('',*,*,#8737,.T.);
#12781=ORIENTED_EDGE('',*,*,#8734,.T.);
#12782=ORIENTED_EDGE('',*,*,#8731,.T.);
#12783=ORIENTED_EDGE('',*,*,#8728,.T.);
#12784=ORIENTED_EDGE('',*,*,#8725,.T.);
#12785=ORIENTED_EDGE('',*,*,#8722,.T.);
#12786=ORIENTED_EDGE('',*,*,#8719,.T.);
#12787=ORIENTED_EDGE('',*,*,#8716,.T.);
#12788=ORIENTED_EDGE('',*,*,#8713,.T.);
#12789=ORIENTED_EDGE('',*,*,#8710,.T.);
#12790=ORIENTED_EDGE('',*,*,#8707,.T.);
#12791=ORIENTED_EDGE('',*,*,#8704,.T.);
#12792=ORIENTED_EDGE('',*,*,#8701,.T.);
#12793=ORIENTED_EDGE('',*,*,#8876,.T.);
#12794=ORIENTED_EDGE('',*,*,#8882,.F.);
#12795=ORIENTED_EDGE('',*,*,#8883,.F.);
#12796=ORIENTED_EDGE('',*,*,#8884,.T.);
#12797=ORIENTED_EDGE('',*,*,#8885,.F.);
#12798=ORIENTED_EDGE('',*,*,#8699,.F.);
#12799=ORIENTED_EDGE('',*,*,#8703,.F.);
#12800=ORIENTED_EDGE('',*,*,#8706,.F.);
#12801=ORIENTED_EDGE('',*,*,#8709,.F.);
#12802=ORIENTED_EDGE('',*,*,#8712,.F.);
#12803=ORIENTED_EDGE('',*,*,#8715,.F.);
#12804=ORIENTED_EDGE('',*,*,#8718,.F.);
#12805=ORIENTED_EDGE('',*,*,#8721,.F.);
#12806=ORIENTED_EDGE('',*,*,#8724,.F.);
#12807=ORIENTED_EDGE('',*,*,#8727,.F.);
#12808=ORIENTED_EDGE('',*,*,#8730,.F.);
#12809=ORIENTED_EDGE('',*,*,#8733,.F.);
#12810=ORIENTED_EDGE('',*,*,#8736,.F.);
#12811=ORIENTED_EDGE('',*,*,#8739,.F.);
#12812=ORIENTED_EDGE('',*,*,#8742,.F.);
#12813=ORIENTED_EDGE('',*,*,#8745,.F.);
#12814=ORIENTED_EDGE('',*,*,#8748,.F.);
#12815=ORIENTED_EDGE('',*,*,#8751,.F.);
#12816=ORIENTED_EDGE('',*,*,#8754,.F.);
#12817=ORIENTED_EDGE('',*,*,#8757,.F.);
#12818=ORIENTED_EDGE('',*,*,#8760,.F.);
#12819=ORIENTED_EDGE('',*,*,#8763,.F.);
#12820=ORIENTED_EDGE('',*,*,#8766,.F.);
#12821=ORIENTED_EDGE('',*,*,#8769,.F.);
#12822=ORIENTED_EDGE('',*,*,#8772,.F.);
#12823=ORIENTED_EDGE('',*,*,#8775,.F.);
#12824=ORIENTED_EDGE('',*,*,#8778,.F.);
#12825=ORIENTED_EDGE('',*,*,#8781,.F.);
#12826=ORIENTED_EDGE('',*,*,#8784,.F.);
#12827=ORIENTED_EDGE('',*,*,#8787,.F.);
#12828=ORIENTED_EDGE('',*,*,#8790,.F.);
#12829=ORIENTED_EDGE('',*,*,#8793,.F.);
#12830=ORIENTED_EDGE('',*,*,#8796,.F.);
#12831=ORIENTED_EDGE('',*,*,#8799,.F.);
#12832=ORIENTED_EDGE('',*,*,#8802,.F.);
#12833=ORIENTED_EDGE('',*,*,#8805,.F.);
#12834=ORIENTED_EDGE('',*,*,#8808,.F.);
#12835=ORIENTED_EDGE('',*,*,#8811,.F.);
#12836=ORIENTED_EDGE('',*,*,#8814,.F.);
#12837=ORIENTED_EDGE('',*,*,#8817,.F.);
#12838=ORIENTED_EDGE('',*,*,#8820,.F.);
#12839=ORIENTED_EDGE('',*,*,#8823,.F.);
#12840=ORIENTED_EDGE('',*,*,#8826,.F.);
#12841=ORIENTED_EDGE('',*,*,#8829,.F.);
#12842=ORIENTED_EDGE('',*,*,#8832,.F.);
#12843=ORIENTED_EDGE('',*,*,#8835,.F.);
#12844=ORIENTED_EDGE('',*,*,#8838,.F.);
#12845=ORIENTED_EDGE('',*,*,#8841,.F.);
#12846=ORIENTED_EDGE('',*,*,#8844,.F.);
#12847=ORIENTED_EDGE('',*,*,#8847,.F.);
#12848=ORIENTED_EDGE('',*,*,#8850,.F.);
#12849=ORIENTED_EDGE('',*,*,#8853,.F.);
#12850=ORIENTED_EDGE('',*,*,#8856,.F.);
#12851=ORIENTED_EDGE('',*,*,#8859,.F.);
#12852=ORIENTED_EDGE('',*,*,#8862,.F.);
#12853=ORIENTED_EDGE('',*,*,#8865,.F.);
#12854=ORIENTED_EDGE('',*,*,#8868,.F.);
#12855=ORIENTED_EDGE('',*,*,#8871,.F.);
#12856=ORIENTED_EDGE('',*,*,#8874,.F.);
#12857=ORIENTED_EDGE('',*,*,#8877,.F.);
#12858=ORIENTED_EDGE('',*,*,#8884,.F.);
#12859=ORIENTED_EDGE('',*,*,#8886,.F.);
#12860=ORIENTED_EDGE('',*,*,#8518,.F.);
#12861=ORIENTED_EDGE('',*,*,#8522,.F.);
#12862=ORIENTED_EDGE('',*,*,#8525,.F.);
#12863=ORIENTED_EDGE('',*,*,#8528,.F.);
#12864=ORIENTED_EDGE('',*,*,#8531,.F.);
#12865=ORIENTED_EDGE('',*,*,#8534,.F.);
#12866=ORIENTED_EDGE('',*,*,#8537,.F.);
#12867=ORIENTED_EDGE('',*,*,#8540,.F.);
#12868=ORIENTED_EDGE('',*,*,#8543,.F.);
#12869=ORIENTED_EDGE('',*,*,#8546,.F.);
#12870=ORIENTED_EDGE('',*,*,#8549,.F.);
#12871=ORIENTED_EDGE('',*,*,#8552,.F.);
#12872=ORIENTED_EDGE('',*,*,#8555,.F.);
#12873=ORIENTED_EDGE('',*,*,#8558,.F.);
#12874=ORIENTED_EDGE('',*,*,#8561,.F.);
#12875=ORIENTED_EDGE('',*,*,#8564,.F.);
#12876=ORIENTED_EDGE('',*,*,#8567,.F.);
#12877=ORIENTED_EDGE('',*,*,#8570,.F.);
#12878=ORIENTED_EDGE('',*,*,#8573,.F.);
#12879=ORIENTED_EDGE('',*,*,#8576,.F.);
#12880=ORIENTED_EDGE('',*,*,#8579,.F.);
#12881=ORIENTED_EDGE('',*,*,#8582,.F.);
#12882=ORIENTED_EDGE('',*,*,#8585,.F.);
#12883=ORIENTED_EDGE('',*,*,#8588,.F.);
#12884=ORIENTED_EDGE('',*,*,#8591,.F.);
#12885=ORIENTED_EDGE('',*,*,#8594,.F.);
#12886=ORIENTED_EDGE('',*,*,#8597,.F.);
#12887=ORIENTED_EDGE('',*,*,#8600,.F.);
#12888=ORIENTED_EDGE('',*,*,#8603,.F.);
#12889=ORIENTED_EDGE('',*,*,#8606,.F.);
#12890=ORIENTED_EDGE('',*,*,#8609,.F.);
#12891=ORIENTED_EDGE('',*,*,#8612,.F.);
#12892=ORIENTED_EDGE('',*,*,#8615,.F.);
#12893=ORIENTED_EDGE('',*,*,#8618,.F.);
#12894=ORIENTED_EDGE('',*,*,#8621,.F.);
#12895=ORIENTED_EDGE('',*,*,#8624,.F.);
#12896=ORIENTED_EDGE('',*,*,#8627,.F.);
#12897=ORIENTED_EDGE('',*,*,#8630,.F.);
#12898=ORIENTED_EDGE('',*,*,#8633,.F.);
#12899=ORIENTED_EDGE('',*,*,#8636,.F.);
#12900=ORIENTED_EDGE('',*,*,#8639,.F.);
#12901=ORIENTED_EDGE('',*,*,#8642,.F.);
#12902=ORIENTED_EDGE('',*,*,#8645,.F.);
#12903=ORIENTED_EDGE('',*,*,#8648,.F.);
#12904=ORIENTED_EDGE('',*,*,#8651,.F.);
#12905=ORIENTED_EDGE('',*,*,#8654,.F.);
#12906=ORIENTED_EDGE('',*,*,#8657,.F.);
#12907=ORIENTED_EDGE('',*,*,#8660,.F.);
#12908=ORIENTED_EDGE('',*,*,#8663,.F.);
#12909=ORIENTED_EDGE('',*,*,#8666,.F.);
#12910=ORIENTED_EDGE('',*,*,#8669,.F.);
#12911=ORIENTED_EDGE('',*,*,#8672,.F.);
#12912=ORIENTED_EDGE('',*,*,#8675,.F.);
#12913=ORIENTED_EDGE('',*,*,#8678,.F.);
#12914=ORIENTED_EDGE('',*,*,#8681,.F.);
#12915=ORIENTED_EDGE('',*,*,#8684,.F.);
#12916=ORIENTED_EDGE('',*,*,#8687,.F.);
#12917=ORIENTED_EDGE('',*,*,#8690,.F.);
#12918=ORIENTED_EDGE('',*,*,#8693,.F.);
#12919=ORIENTED_EDGE('',*,*,#8696,.F.);
#12920=ORIENTED_EDGE('',*,*,#8887,.F.);
#12921=ORIENTED_EDGE('',*,*,#8695,.T.);
#12922=ORIENTED_EDGE('',*,*,#8880,.T.);
#12923=ORIENTED_EDGE('',*,*,#8888,.F.);
#12924=ORIENTED_EDGE('',*,*,#8887,.T.);
#12925=ORIENTED_EDGE('',*,*,#8889,.T.);
#12926=ORIENTED_EDGE('',*,*,#8890,.T.);
#12927=ORIENTED_EDGE('',*,*,#8891,.T.);
#12928=ORIENTED_EDGE('',*,*,#8892,.T.);
#12929=ORIENTED_EDGE('',*,*,#8893,.T.);
#12930=ORIENTED_EDGE('',*,*,#8894,.T.);
#12931=ORIENTED_EDGE('',*,*,#8886,.T.);
#12932=ORIENTED_EDGE('',*,*,#8883,.T.);
#12933=ORIENTED_EDGE('',*,*,#8881,.T.);
#12934=ORIENTED_EDGE('',*,*,#8519,.F.);
#12935=ORIENTED_EDGE('',*,*,#8895,.F.);
#12936=ORIENTED_EDGE('',*,*,#8896,.F.);
#12937=ORIENTED_EDGE('',*,*,#8897,.F.);
#12938=ORIENTED_EDGE('',*,*,#8898,.F.);
#12939=ORIENTED_EDGE('',*,*,#8899,.F.);
#12940=ORIENTED_EDGE('',*,*,#8900,.F.);
#12941=ORIENTED_EDGE('',*,*,#8901,.F.);
#12942=ORIENTED_EDGE('',*,*,#8896,.T.);
#12943=ORIENTED_EDGE('',*,*,#8902,.T.);
#12944=ORIENTED_EDGE('',*,*,#8894,.F.);
#12945=ORIENTED_EDGE('',*,*,#8903,.F.);
#12946=ORIENTED_EDGE('',*,*,#8897,.T.);
#12947=ORIENTED_EDGE('',*,*,#8903,.T.);
#12948=ORIENTED_EDGE('',*,*,#8893,.F.);
#12949=ORIENTED_EDGE('',*,*,#8904,.F.);
#12950=ORIENTED_EDGE('',*,*,#8898,.T.);
#12951=ORIENTED_EDGE('',*,*,#8904,.T.);
#12952=ORIENTED_EDGE('',*,*,#8892,.F.);
#12953=ORIENTED_EDGE('',*,*,#8905,.F.);
#12954=ORIENTED_EDGE('',*,*,#8899,.T.);
#12955=ORIENTED_EDGE('',*,*,#8905,.T.);
#12956=ORIENTED_EDGE('',*,*,#8891,.F.);
#12957=ORIENTED_EDGE('',*,*,#8906,.F.);
#12958=ORIENTED_EDGE('',*,*,#8900,.T.);
#12959=ORIENTED_EDGE('',*,*,#8906,.T.);
#12960=ORIENTED_EDGE('',*,*,#8890,.F.);
#12961=ORIENTED_EDGE('',*,*,#8907,.F.);
#12962=ORIENTED_EDGE('',*,*,#8895,.T.);
#12963=ORIENTED_EDGE('',*,*,#8907,.T.);
#12964=ORIENTED_EDGE('',*,*,#8889,.F.);
#12965=ORIENTED_EDGE('',*,*,#8902,.F.);
#12966=ORIENTED_EDGE('',*,*,#8901,.T.);
#12967=ORIENTED_EDGE('',*,*,#8908,.T.);
#12968=ORIENTED_EDGE('',*,*,#8909,.F.);
#12969=ORIENTED_EDGE('',*,*,#8908,.F.);
#12970=ORIENTED_EDGE('',*,*,#8885,.T.);
#12971=ORIENTED_EDGE('',*,*,#8888,.T.);
#12972=ORIENTED_EDGE('',*,*,#8879,.T.);
#12973=ORIENTED_EDGE('',*,*,#8700,.T.);
#12974=ORIENTED_EDGE('',*,*,#8909,.T.);
#12975=ORIENTED_EDGE('',*,*,#8910,.T.);
#12976=ORIENTED_EDGE('',*,*,#8910,.F.);
#12977=ORIENTED_EDGE('',*,*,#8911,.T.);
#12978=ORIENTED_EDGE('',*,*,#8912,.T.);
#12979=ORIENTED_EDGE('',*,*,#8913,.F.);
#12980=ORIENTED_EDGE('',*,*,#8914,.T.);
#12981=ORIENTED_EDGE('',*,*,#8915,.T.);
#12982=ORIENTED_EDGE('',*,*,#8916,.T.);
#12983=ORIENTED_EDGE('',*,*,#8911,.F.);
#12984=ORIENTED_EDGE('',*,*,#8917,.T.);
#12985=ORIENTED_EDGE('',*,*,#8918,.T.);
#12986=ORIENTED_EDGE('',*,*,#8919,.T.);
#12987=ORIENTED_EDGE('',*,*,#8915,.F.);
#12988=ORIENTED_EDGE('',*,*,#8920,.T.);
#12989=ORIENTED_EDGE('',*,*,#8921,.T.);
#12990=ORIENTED_EDGE('',*,*,#8922,.T.);
#12991=ORIENTED_EDGE('',*,*,#8918,.F.);
#12992=ORIENTED_EDGE('',*,*,#8923,.T.);
#12993=ORIENTED_EDGE('',*,*,#8924,.T.);
#12994=ORIENTED_EDGE('',*,*,#8925,.T.);
#12995=ORIENTED_EDGE('',*,*,#8921,.F.);
#12996=ORIENTED_EDGE('',*,*,#8926,.T.);
#12997=ORIENTED_EDGE('',*,*,#8927,.T.);
#12998=ORIENTED_EDGE('',*,*,#8928,.T.);
#12999=ORIENTED_EDGE('',*,*,#8924,.F.);
#13000=ORIENTED_EDGE('',*,*,#8929,.T.);
#13001=ORIENTED_EDGE('',*,*,#8930,.T.);
#13002=ORIENTED_EDGE('',*,*,#8931,.T.);
#13003=ORIENTED_EDGE('',*,*,#8927,.F.);
#13004=ORIENTED_EDGE('',*,*,#8932,.T.);
#13005=ORIENTED_EDGE('',*,*,#8933,.F.);
#13006=ORIENTED_EDGE('',*,*,#8934,.T.);
#13007=ORIENTED_EDGE('',*,*,#8935,.F.);
#13008=ORIENTED_EDGE('',*,*,#8936,.T.);
#13009=ORIENTED_EDGE('',*,*,#8937,.T.);
#13010=ORIENTED_EDGE('',*,*,#8938,.T.);
#13011=ORIENTED_EDGE('',*,*,#8939,.F.);
#13012=ORIENTED_EDGE('',*,*,#8940,.F.);
#13013=ORIENTED_EDGE('',*,*,#8941,.T.);
#13014=ORIENTED_EDGE('',*,*,#8942,.T.);
#13015=ORIENTED_EDGE('',*,*,#8937,.F.);
#13016=ORIENTED_EDGE('',*,*,#8943,.F.);
#13017=ORIENTED_EDGE('',*,*,#8944,.T.);
#13018=ORIENTED_EDGE('',*,*,#8945,.T.);
#13019=ORIENTED_EDGE('',*,*,#8941,.F.);
#13020=ORIENTED_EDGE('',*,*,#8946,.F.);
#13021=ORIENTED_EDGE('',*,*,#8947,.T.);
#13022=ORIENTED_EDGE('',*,*,#8948,.T.);
#13023=ORIENTED_EDGE('',*,*,#8944,.F.);
#13024=ORIENTED_EDGE('',*,*,#8949,.F.);
#13025=ORIENTED_EDGE('',*,*,#8950,.T.);
#13026=ORIENTED_EDGE('',*,*,#8951,.T.);
#13027=ORIENTED_EDGE('',*,*,#8947,.F.);
#13028=ORIENTED_EDGE('',*,*,#8952,.F.);
#13029=ORIENTED_EDGE('',*,*,#8953,.T.);
#13030=ORIENTED_EDGE('',*,*,#8954,.T.);
#13031=ORIENTED_EDGE('',*,*,#8950,.F.);
#13032=ORIENTED_EDGE('',*,*,#8955,.F.);
#13033=ORIENTED_EDGE('',*,*,#8956,.T.);
#13034=ORIENTED_EDGE('',*,*,#8957,.T.);
#13035=ORIENTED_EDGE('',*,*,#8953,.F.);
#13036=ORIENTED_EDGE('',*,*,#8958,.F.);
#13037=ORIENTED_EDGE('',*,*,#8959,.F.);
#13038=ORIENTED_EDGE('',*,*,#8960,.F.);
#13039=ORIENTED_EDGE('',*,*,#8961,.F.);
#13040=ORIENTED_EDGE('',*,*,#8962,.T.);
#13041=ORIENTED_EDGE('',*,*,#8959,.T.);
#13042=ORIENTED_EDGE('',*,*,#8963,.T.);
#13043=ORIENTED_EDGE('',*,*,#8956,.F.);
#13044=ORIENTED_EDGE('',*,*,#8964,.F.);
#13045=ORIENTED_EDGE('',*,*,#8965,.F.);
#13046=ORIENTED_EDGE('',*,*,#8938,.F.);
#13047=ORIENTED_EDGE('',*,*,#8942,.F.);
#13048=ORIENTED_EDGE('',*,*,#8945,.F.);
#13049=ORIENTED_EDGE('',*,*,#8948,.F.);
#13050=ORIENTED_EDGE('',*,*,#8951,.F.);
#13051=ORIENTED_EDGE('',*,*,#8954,.F.);
#13052=ORIENTED_EDGE('',*,*,#8957,.F.);
#13053=ORIENTED_EDGE('',*,*,#8963,.F.);
#13054=ORIENTED_EDGE('',*,*,#8962,.F.);
#13055=ORIENTED_EDGE('',*,*,#8966,.F.);
#13056=ORIENTED_EDGE('',*,*,#8934,.F.);
#13057=ORIENTED_EDGE('',*,*,#8967,.F.);
#13058=ORIENTED_EDGE('',*,*,#8932,.F.);
#13059=ORIENTED_EDGE('',*,*,#8929,.F.);
#13060=ORIENTED_EDGE('',*,*,#8926,.F.);
#13061=ORIENTED_EDGE('',*,*,#8923,.F.);
#13062=ORIENTED_EDGE('',*,*,#8920,.F.);
#13063=ORIENTED_EDGE('',*,*,#8917,.F.);
#13064=ORIENTED_EDGE('',*,*,#8914,.F.);
#13065=ORIENTED_EDGE('',*,*,#8968,.F.);
#13066=ORIENTED_EDGE('',*,*,#8912,.F.);
#13067=ORIENTED_EDGE('',*,*,#8916,.F.);
#13068=ORIENTED_EDGE('',*,*,#8919,.F.);
#13069=ORIENTED_EDGE('',*,*,#8922,.F.);
#13070=ORIENTED_EDGE('',*,*,#8925,.F.);
#13071=ORIENTED_EDGE('',*,*,#8928,.F.);
#13072=ORIENTED_EDGE('',*,*,#8931,.F.);
#13073=ORIENTED_EDGE('',*,*,#8969,.F.);
#13074=ORIENTED_EDGE('',*,*,#8936,.F.);
#13075=ORIENTED_EDGE('',*,*,#8970,.F.);
#13076=ORIENTED_EDGE('',*,*,#8960,.T.);
#13077=ORIENTED_EDGE('',*,*,#8964,.T.);
#13078=ORIENTED_EDGE('',*,*,#8958,.T.);
#13079=ORIENTED_EDGE('',*,*,#8955,.T.);
#13080=ORIENTED_EDGE('',*,*,#8952,.T.);
#13081=ORIENTED_EDGE('',*,*,#8949,.T.);
#13082=ORIENTED_EDGE('',*,*,#8946,.T.);
#13083=ORIENTED_EDGE('',*,*,#8943,.T.);
#13084=ORIENTED_EDGE('',*,*,#8940,.T.);
#13085=ORIENTED_EDGE('',*,*,#8971,.T.);
#13086=ORIENTED_EDGE('',*,*,#8972,.T.);
#13087=ORIENTED_EDGE('',*,*,#8973,.T.);
#13088=ORIENTED_EDGE('',*,*,#8974,.T.);
#13089=ORIENTED_EDGE('',*,*,#8975,.T.);
#13090=ORIENTED_EDGE('',*,*,#8976,.T.);
#13091=ORIENTED_EDGE('',*,*,#8966,.T.);
#13092=ORIENTED_EDGE('',*,*,#8961,.T.);
#13093=ORIENTED_EDGE('',*,*,#8970,.T.);
#13094=ORIENTED_EDGE('',*,*,#8935,.T.);
#13095=ORIENTED_EDGE('',*,*,#8933,.T.);
#13096=ORIENTED_EDGE('',*,*,#8969,.T.);
#13097=ORIENTED_EDGE('',*,*,#8930,.F.);
#13098=ORIENTED_EDGE('',*,*,#8967,.T.);
#13099=ORIENTED_EDGE('',*,*,#8977,.T.);
#13100=ORIENTED_EDGE('',*,*,#8978,.T.);
#13101=ORIENTED_EDGE('',*,*,#8976,.F.);
#13102=ORIENTED_EDGE('',*,*,#8979,.F.);
#13103=ORIENTED_EDGE('',*,*,#8980,.T.);
#13104=ORIENTED_EDGE('',*,*,#8979,.T.);
#13105=ORIENTED_EDGE('',*,*,#8975,.F.);
#13106=ORIENTED_EDGE('',*,*,#8981,.F.);
#13107=ORIENTED_EDGE('',*,*,#8982,.T.);
#13108=ORIENTED_EDGE('',*,*,#8981,.T.);
#13109=ORIENTED_EDGE('',*,*,#8974,.F.);
#13110=ORIENTED_EDGE('',*,*,#8983,.F.);
#13111=ORIENTED_EDGE('',*,*,#8984,.T.);
#13112=ORIENTED_EDGE('',*,*,#8983,.T.);
#13113=ORIENTED_EDGE('',*,*,#8973,.F.);
#13114=ORIENTED_EDGE('',*,*,#8985,.F.);
#13115=ORIENTED_EDGE('',*,*,#8986,.T.);
#13116=ORIENTED_EDGE('',*,*,#8985,.T.);
#13117=ORIENTED_EDGE('',*,*,#8972,.F.);
#13118=ORIENTED_EDGE('',*,*,#8987,.F.);
#13119=ORIENTED_EDGE('',*,*,#8988,.T.);
#13120=ORIENTED_EDGE('',*,*,#8987,.T.);
#13121=ORIENTED_EDGE('',*,*,#8971,.F.);
#13122=ORIENTED_EDGE('',*,*,#8978,.F.);
#13123=ORIENTED_EDGE('',*,*,#8988,.F.);
#13124=ORIENTED_EDGE('',*,*,#8977,.F.);
#13125=ORIENTED_EDGE('',*,*,#8980,.F.);
#13126=ORIENTED_EDGE('',*,*,#8982,.F.);
#13127=ORIENTED_EDGE('',*,*,#8984,.F.);
#13128=ORIENTED_EDGE('',*,*,#8986,.F.);
#13129=ORIENTED_EDGE('',*,*,#8965,.T.);
#13130=ORIENTED_EDGE('',*,*,#8913,.T.);
#13131=ORIENTED_EDGE('',*,*,#8968,.T.);
#13132=ORIENTED_EDGE('',*,*,#8939,.T.);
#13133=ORIENTED_EDGE('',*,*,#8989,.F.);
#13134=ORIENTED_EDGE('',*,*,#8990,.T.);
#13135=ORIENTED_EDGE('',*,*,#8991,.T.);
#13136=ORIENTED_EDGE('',*,*,#8990,.F.);
#13137=ORIENTED_EDGE('',*,*,#8992,.F.);
#13138=ORIENTED_EDGE('',*,*,#8993,.T.);
#13139=ORIENTED_EDGE('',*,*,#8994,.T.);
#13140=ORIENTED_EDGE('',*,*,#8993,.F.);
#13141=ORIENTED_EDGE('',*,*,#8992,.T.);
#13142=ORIENTED_EDGE('',*,*,#8989,.T.);
#13143=ORIENTED_EDGE('',*,*,#8994,.F.);
#13144=ORIENTED_EDGE('',*,*,#8991,.F.);
#13145=ORIENTED_EDGE('',*,*,#8995,.F.);
#13146=ORIENTED_EDGE('',*,*,#8996,.T.);
#13147=ORIENTED_EDGE('',*,*,#8997,.T.);
#13148=ORIENTED_EDGE('',*,*,#8998,.T.);
#13149=ORIENTED_EDGE('',*,*,#8999,.F.);
#13150=ORIENTED_EDGE('',*,*,#9000,.T.);
#13151=ORIENTED_EDGE('',*,*,#8995,.T.);
#13152=ORIENTED_EDGE('',*,*,#9001,.T.);
#13153=ORIENTED_EDGE('',*,*,#9002,.F.);
#13154=ORIENTED_EDGE('',*,*,#9003,.T.);
#13155=ORIENTED_EDGE('',*,*,#8999,.T.);
#13156=ORIENTED_EDGE('',*,*,#9004,.T.);
#13157=ORIENTED_EDGE('',*,*,#9005,.F.);
#13158=ORIENTED_EDGE('',*,*,#9006,.T.);
#13159=ORIENTED_EDGE('',*,*,#9002,.T.);
#13160=ORIENTED_EDGE('',*,*,#9007,.T.);
#13161=ORIENTED_EDGE('',*,*,#9008,.F.);
#13162=ORIENTED_EDGE('',*,*,#9009,.T.);
#13163=ORIENTED_EDGE('',*,*,#9005,.T.);
#13164=ORIENTED_EDGE('',*,*,#9010,.T.);
#13165=ORIENTED_EDGE('',*,*,#9011,.F.);
#13166=ORIENTED_EDGE('',*,*,#9012,.T.);
#13167=ORIENTED_EDGE('',*,*,#9008,.T.);
#13168=ORIENTED_EDGE('',*,*,#9013,.T.);
#13169=ORIENTED_EDGE('',*,*,#9014,.F.);
#13170=ORIENTED_EDGE('',*,*,#9015,.T.);
#13171=ORIENTED_EDGE('',*,*,#9011,.T.);
#13172=ORIENTED_EDGE('',*,*,#9016,.T.);
#13173=ORIENTED_EDGE('',*,*,#9017,.F.);
#13174=ORIENTED_EDGE('',*,*,#9018,.T.);
#13175=ORIENTED_EDGE('',*,*,#9014,.T.);
#13176=ORIENTED_EDGE('',*,*,#9019,.T.);
#13177=ORIENTED_EDGE('',*,*,#9020,.F.);
#13178=ORIENTED_EDGE('',*,*,#9021,.T.);
#13179=ORIENTED_EDGE('',*,*,#9017,.T.);
#13180=ORIENTED_EDGE('',*,*,#9022,.T.);
#13181=ORIENTED_EDGE('',*,*,#9023,.F.);
#13182=ORIENTED_EDGE('',*,*,#9024,.T.);
#13183=ORIENTED_EDGE('',*,*,#9020,.T.);
#13184=ORIENTED_EDGE('',*,*,#9025,.T.);
#13185=ORIENTED_EDGE('',*,*,#9026,.F.);
#13186=ORIENTED_EDGE('',*,*,#9027,.T.);
#13187=ORIENTED_EDGE('',*,*,#9023,.T.);
#13188=ORIENTED_EDGE('',*,*,#9028,.T.);
#13189=ORIENTED_EDGE('',*,*,#9029,.F.);
#13190=ORIENTED_EDGE('',*,*,#9030,.T.);
#13191=ORIENTED_EDGE('',*,*,#9026,.T.);
#13192=ORIENTED_EDGE('',*,*,#9031,.T.);
#13193=ORIENTED_EDGE('',*,*,#9032,.F.);
#13194=ORIENTED_EDGE('',*,*,#9033,.T.);
#13195=ORIENTED_EDGE('',*,*,#9029,.T.);
#13196=ORIENTED_EDGE('',*,*,#9034,.T.);
#13197=ORIENTED_EDGE('',*,*,#9035,.F.);
#13198=ORIENTED_EDGE('',*,*,#9036,.T.);
#13199=ORIENTED_EDGE('',*,*,#9032,.T.);
#13200=ORIENTED_EDGE('',*,*,#9037,.T.);
#13201=ORIENTED_EDGE('',*,*,#9038,.F.);
#13202=ORIENTED_EDGE('',*,*,#9039,.T.);
#13203=ORIENTED_EDGE('',*,*,#9035,.T.);
#13204=ORIENTED_EDGE('',*,*,#9040,.T.);
#13205=ORIENTED_EDGE('',*,*,#9041,.F.);
#13206=ORIENTED_EDGE('',*,*,#9042,.T.);
#13207=ORIENTED_EDGE('',*,*,#9043,.T.);
#13208=ORIENTED_EDGE('',*,*,#9044,.F.);
#13209=ORIENTED_EDGE('',*,*,#9045,.F.);
#13210=ORIENTED_EDGE('',*,*,#9046,.T.);
#13211=ORIENTED_EDGE('',*,*,#9041,.T.);
#13212=ORIENTED_EDGE('',*,*,#9047,.F.);
#13213=ORIENTED_EDGE('',*,*,#9048,.F.);
#13214=ORIENTED_EDGE('',*,*,#9049,.T.);
#13215=ORIENTED_EDGE('',*,*,#9045,.T.);
#13216=ORIENTED_EDGE('',*,*,#9050,.F.);
#13217=ORIENTED_EDGE('',*,*,#9051,.F.);
#13218=ORIENTED_EDGE('',*,*,#9052,.T.);
#13219=ORIENTED_EDGE('',*,*,#9048,.T.);
#13220=ORIENTED_EDGE('',*,*,#9053,.F.);
#13221=ORIENTED_EDGE('',*,*,#9054,.F.);
#13222=ORIENTED_EDGE('',*,*,#9055,.T.);
#13223=ORIENTED_EDGE('',*,*,#9051,.T.);
#13224=ORIENTED_EDGE('',*,*,#9056,.F.);
#13225=ORIENTED_EDGE('',*,*,#9057,.F.);
#13226=ORIENTED_EDGE('',*,*,#9058,.T.);
#13227=ORIENTED_EDGE('',*,*,#9054,.T.);
#13228=ORIENTED_EDGE('',*,*,#9059,.F.);
#13229=ORIENTED_EDGE('',*,*,#9060,.F.);
#13230=ORIENTED_EDGE('',*,*,#9061,.T.);
#13231=ORIENTED_EDGE('',*,*,#9057,.T.);
#13232=ORIENTED_EDGE('',*,*,#9062,.F.);
#13233=ORIENTED_EDGE('',*,*,#9063,.F.);
#13234=ORIENTED_EDGE('',*,*,#9064,.T.);
#13235=ORIENTED_EDGE('',*,*,#9060,.T.);
#13236=ORIENTED_EDGE('',*,*,#9065,.F.);
#13237=ORIENTED_EDGE('',*,*,#9066,.F.);
#13238=ORIENTED_EDGE('',*,*,#9067,.T.);
#13239=ORIENTED_EDGE('',*,*,#9063,.T.);
#13240=ORIENTED_EDGE('',*,*,#9068,.F.);
#13241=ORIENTED_EDGE('',*,*,#9069,.F.);
#13242=ORIENTED_EDGE('',*,*,#9070,.T.);
#13243=ORIENTED_EDGE('',*,*,#9066,.T.);
#13244=ORIENTED_EDGE('',*,*,#9071,.F.);
#13245=ORIENTED_EDGE('',*,*,#9072,.F.);
#13246=ORIENTED_EDGE('',*,*,#9073,.T.);
#13247=ORIENTED_EDGE('',*,*,#9069,.T.);
#13248=ORIENTED_EDGE('',*,*,#9074,.F.);
#13249=ORIENTED_EDGE('',*,*,#9075,.F.);
#13250=ORIENTED_EDGE('',*,*,#9076,.T.);
#13251=ORIENTED_EDGE('',*,*,#9072,.T.);
#13252=ORIENTED_EDGE('',*,*,#9077,.F.);
#13253=ORIENTED_EDGE('',*,*,#9078,.F.);
#13254=ORIENTED_EDGE('',*,*,#9079,.T.);
#13255=ORIENTED_EDGE('',*,*,#9075,.T.);
#13256=ORIENTED_EDGE('',*,*,#9080,.F.);
#13257=ORIENTED_EDGE('',*,*,#9081,.F.);
#13258=ORIENTED_EDGE('',*,*,#9082,.T.);
#13259=ORIENTED_EDGE('',*,*,#9078,.T.);
#13260=ORIENTED_EDGE('',*,*,#9083,.F.);
#13261=ORIENTED_EDGE('',*,*,#9084,.F.);
#13262=ORIENTED_EDGE('',*,*,#9085,.T.);
#13263=ORIENTED_EDGE('',*,*,#9081,.T.);
#13264=ORIENTED_EDGE('',*,*,#9086,.F.);
#13265=ORIENTED_EDGE('',*,*,#9087,.F.);
#13266=ORIENTED_EDGE('',*,*,#9043,.F.);
#13267=ORIENTED_EDGE('',*,*,#9088,.F.);
#13268=ORIENTED_EDGE('',*,*,#9089,.F.);
#13269=ORIENTED_EDGE('',*,*,#9090,.F.);
#13270=ORIENTED_EDGE('',*,*,#9091,.T.);
#13271=ORIENTED_EDGE('',*,*,#9092,.F.);
#13272=ORIENTED_EDGE('',*,*,#9091,.F.);
#13273=ORIENTED_EDGE('',*,*,#9088,.T.);
#13274=ORIENTED_EDGE('',*,*,#9042,.F.);
#13275=ORIENTED_EDGE('',*,*,#9046,.F.);
#13276=ORIENTED_EDGE('',*,*,#9049,.F.);
#13277=ORIENTED_EDGE('',*,*,#9052,.F.);
#13278=ORIENTED_EDGE('',*,*,#9055,.F.);
#13279=ORIENTED_EDGE('',*,*,#9058,.F.);
#13280=ORIENTED_EDGE('',*,*,#9061,.F.);
#13281=ORIENTED_EDGE('',*,*,#9064,.F.);
#13282=ORIENTED_EDGE('',*,*,#9067,.F.);
#13283=ORIENTED_EDGE('',*,*,#9070,.F.);
#13284=ORIENTED_EDGE('',*,*,#9073,.F.);
#13285=ORIENTED_EDGE('',*,*,#9076,.F.);
#13286=ORIENTED_EDGE('',*,*,#9079,.F.);
#13287=ORIENTED_EDGE('',*,*,#9082,.F.);
#13288=ORIENTED_EDGE('',*,*,#9085,.F.);
#13289=ORIENTED_EDGE('',*,*,#9093,.F.);
#13290=ORIENTED_EDGE('',*,*,#9094,.F.);
#13291=ORIENTED_EDGE('',*,*,#8996,.F.);
#13292=ORIENTED_EDGE('',*,*,#9000,.F.);
#13293=ORIENTED_EDGE('',*,*,#9003,.F.);
#13294=ORIENTED_EDGE('',*,*,#9006,.F.);
#13295=ORIENTED_EDGE('',*,*,#9009,.F.);
#13296=ORIENTED_EDGE('',*,*,#9012,.F.);
#13297=ORIENTED_EDGE('',*,*,#9015,.F.);
#13298=ORIENTED_EDGE('',*,*,#9018,.F.);
#13299=ORIENTED_EDGE('',*,*,#9021,.F.);
#13300=ORIENTED_EDGE('',*,*,#9024,.F.);
#13301=ORIENTED_EDGE('',*,*,#9027,.F.);
#13302=ORIENTED_EDGE('',*,*,#9030,.F.);
#13303=ORIENTED_EDGE('',*,*,#9033,.F.);
#13304=ORIENTED_EDGE('',*,*,#9036,.F.);
#13305=ORIENTED_EDGE('',*,*,#9039,.F.);
#13306=ORIENTED_EDGE('',*,*,#9095,.F.);
#13307=ORIENTED_EDGE('',*,*,#9084,.T.);
#13308=ORIENTED_EDGE('',*,*,#9096,.F.);
#13309=ORIENTED_EDGE('',*,*,#9097,.F.);
#13310=ORIENTED_EDGE('',*,*,#9093,.T.);
#13311=ORIENTED_EDGE('',*,*,#9087,.T.);
#13312=ORIENTED_EDGE('',*,*,#9090,.T.);
#13313=ORIENTED_EDGE('',*,*,#9098,.F.);
#13314=ORIENTED_EDGE('',*,*,#9040,.F.);
#13315=ORIENTED_EDGE('',*,*,#9037,.F.);
#13316=ORIENTED_EDGE('',*,*,#9034,.F.);
#13317=ORIENTED_EDGE('',*,*,#9031,.F.);
#13318=ORIENTED_EDGE('',*,*,#9028,.F.);
#13319=ORIENTED_EDGE('',*,*,#9025,.F.);
#13320=ORIENTED_EDGE('',*,*,#9022,.F.);
#13321=ORIENTED_EDGE('',*,*,#9019,.F.);
#13322=ORIENTED_EDGE('',*,*,#9016,.F.);
#13323=ORIENTED_EDGE('',*,*,#9013,.F.);
#13324=ORIENTED_EDGE('',*,*,#9010,.F.);
#13325=ORIENTED_EDGE('',*,*,#9007,.F.);
#13326=ORIENTED_EDGE('',*,*,#9004,.F.);
#13327=ORIENTED_EDGE('',*,*,#9001,.F.);
#13328=ORIENTED_EDGE('',*,*,#8998,.F.);
#13329=ORIENTED_EDGE('',*,*,#9099,.F.);
#13330=ORIENTED_EDGE('',*,*,#9096,.T.);
#13331=ORIENTED_EDGE('',*,*,#9086,.T.);
#13332=ORIENTED_EDGE('',*,*,#9083,.T.);
#13333=ORIENTED_EDGE('',*,*,#9080,.T.);
#13334=ORIENTED_EDGE('',*,*,#9077,.T.);
#13335=ORIENTED_EDGE('',*,*,#9074,.T.);
#13336=ORIENTED_EDGE('',*,*,#9071,.T.);
#13337=ORIENTED_EDGE('',*,*,#9068,.T.);
#13338=ORIENTED_EDGE('',*,*,#9065,.T.);
#13339=ORIENTED_EDGE('',*,*,#9062,.T.);
#13340=ORIENTED_EDGE('',*,*,#9059,.T.);
#13341=ORIENTED_EDGE('',*,*,#9056,.T.);
#13342=ORIENTED_EDGE('',*,*,#9053,.T.);
#13343=ORIENTED_EDGE('',*,*,#9050,.T.);
#13344=ORIENTED_EDGE('',*,*,#9047,.T.);
#13345=ORIENTED_EDGE('',*,*,#9044,.T.);
#13346=ORIENTED_EDGE('',*,*,#9038,.T.);
#13347=ORIENTED_EDGE('',*,*,#9098,.T.);
#13348=ORIENTED_EDGE('',*,*,#9089,.T.);
#13349=ORIENTED_EDGE('',*,*,#9095,.T.);
#13350=ORIENTED_EDGE('',*,*,#9100,.F.);
#13351=ORIENTED_EDGE('',*,*,#9101,.T.);
#13352=ORIENTED_EDGE('',*,*,#9102,.T.);
#13353=ORIENTED_EDGE('',*,*,#9103,.F.);
#13354=ORIENTED_EDGE('',*,*,#9104,.F.);
#13355=ORIENTED_EDGE('',*,*,#9105,.T.);
#13356=ORIENTED_EDGE('',*,*,#9106,.T.);
#13357=ORIENTED_EDGE('',*,*,#9101,.F.);
#13358=ORIENTED_EDGE('',*,*,#9107,.F.);
#13359=ORIENTED_EDGE('',*,*,#9108,.T.);
#13360=ORIENTED_EDGE('',*,*,#9109,.T.);
#13361=ORIENTED_EDGE('',*,*,#9105,.F.);
#13362=ORIENTED_EDGE('',*,*,#9110,.F.);
#13363=ORIENTED_EDGE('',*,*,#9111,.T.);
#13364=ORIENTED_EDGE('',*,*,#9112,.T.);
#13365=ORIENTED_EDGE('',*,*,#9108,.F.);
#13366=ORIENTED_EDGE('',*,*,#9113,.F.);
#13367=ORIENTED_EDGE('',*,*,#9114,.T.);
#13368=ORIENTED_EDGE('',*,*,#9115,.T.);
#13369=ORIENTED_EDGE('',*,*,#9111,.F.);
#13370=ORIENTED_EDGE('',*,*,#9116,.F.);
#13371=ORIENTED_EDGE('',*,*,#9103,.T.);
#13372=ORIENTED_EDGE('',*,*,#9117,.T.);
#13373=ORIENTED_EDGE('',*,*,#9114,.F.);
#13374=ORIENTED_EDGE('',*,*,#9117,.F.);
#13375=ORIENTED_EDGE('',*,*,#9102,.F.);
#13376=ORIENTED_EDGE('',*,*,#9106,.F.);
#13377=ORIENTED_EDGE('',*,*,#9109,.F.);
#13378=ORIENTED_EDGE('',*,*,#9112,.F.);
#13379=ORIENTED_EDGE('',*,*,#9115,.F.);
#13380=ORIENTED_EDGE('',*,*,#9118,.T.);
#13381=ORIENTED_EDGE('',*,*,#9094,.T.);
#13382=ORIENTED_EDGE('',*,*,#9097,.T.);
#13383=ORIENTED_EDGE('',*,*,#9099,.T.);
#13384=ORIENTED_EDGE('',*,*,#8997,.F.);
#13385=ORIENTED_EDGE('',*,*,#9118,.F.);
#13386=ORIENTED_EDGE('',*,*,#9119,.T.);
#13387=ORIENTED_EDGE('',*,*,#9120,.T.);
#13388=ORIENTED_EDGE('',*,*,#9119,.F.);
#13389=ORIENTED_EDGE('',*,*,#9120,.F.);
#13390=ORIENTED_EDGE('',*,*,#9100,.T.);
#13391=ORIENTED_EDGE('',*,*,#9116,.T.);
#13392=ORIENTED_EDGE('',*,*,#9113,.T.);
#13393=ORIENTED_EDGE('',*,*,#9110,.T.);
#13394=ORIENTED_EDGE('',*,*,#9107,.T.);
#13395=ORIENTED_EDGE('',*,*,#9104,.T.);
#13396=ORIENTED_EDGE('',*,*,#9092,.T.);
#13397=ORIENTED_EDGE('',*,*,#9121,.F.);
#13398=ORIENTED_EDGE('',*,*,#9122,.T.);
#13399=ORIENTED_EDGE('',*,*,#9123,.T.);
#13400=ORIENTED_EDGE('',*,*,#9122,.F.);
#13401=ORIENTED_EDGE('',*,*,#9124,.F.);
#13402=ORIENTED_EDGE('',*,*,#9125,.T.);
#13403=ORIENTED_EDGE('',*,*,#9126,.T.);
#13404=ORIENTED_EDGE('',*,*,#9125,.F.);
#13405=ORIENTED_EDGE('',*,*,#9124,.T.);
#13406=ORIENTED_EDGE('',*,*,#9121,.T.);
#13407=ORIENTED_EDGE('',*,*,#9126,.F.);
#13408=ORIENTED_EDGE('',*,*,#9123,.F.);
#13409=PLANE('',#14505);
#13410=PLANE('',#14506);
#13411=PLANE('',#14507);
#13412=PLANE('',#14508);
#13413=PLANE('',#14509);
#13414=PLANE('',#14510);
#13415=PLANE('',#14511);
#13416=PLANE('',#14512);
#13417=PLANE('',#14513);
#13418=PLANE('',#14514);
#13419=PLANE('',#14516);
#13420=PLANE('',#14517);
#13421=PLANE('',#14518);
#13422=PLANE('',#14519);
#13423=PLANE('',#14520);
#13424=PLANE('',#14521);
#13425=PLANE('',#14522);
#13426=PLANE('',#14523);
#13427=PLANE('',#14524);
#13428=PLANE('',#14525);
#13429=PLANE('',#14608);
#13430=PLANE('',#14616);
#13431=PLANE('',#14617);
#13432=PLANE('',#14618);
#13433=PLANE('',#14619);
#13434=PLANE('',#14620);
#13435=PLANE('',#14678);
#13436=PLANE('',#14679);
#13437=PLANE('',#14680);
#13438=PLANE('',#14681);
#13439=PLANE('',#14682);
#13440=PLANE('',#14683);
#13441=PLANE('',#14684);
#13442=PLANE('',#14685);
#13443=PLANE('',#14689);
#13444=PLANE('',#14690);
#13445=PLANE('',#14698);
#13446=PLANE('',#14699);
#13447=PLANE('',#14884);
#13448=PLANE('',#14887);
#13449=PLANE('',#14889);
#13450=PLANE('',#14892);
#13451=PLANE('',#14897);
#13452=PLANE('',#14898);
#13453=PLANE('',#14940);
#13454=PLANE('',#14943);
#13455=PLANE('',#14946);
#13456=PLANE('',#14949);
#13457=PLANE('',#14954);
#13458=PLANE('',#14959);
#13459=PLANE('',#14964);
#13460=PLANE('',#14967);
#13461=PLANE('',#14970);
#13462=PLANE('',#14973);
#13463=PLANE('',#14978);
#13464=PLANE('',#14983);
#13465=PLANE('',#14988);
#13466=PLANE('',#14991);
#13467=PLANE('',#14994);
#13468=PLANE('',#14997);
#13469=PLANE('',#15002);
#13470=PLANE('',#15007);
#13471=PLANE('',#15012);
#13472=PLANE('',#15015);
#13473=PLANE('',#15018);
#13474=PLANE('',#15021);
#13475=PLANE('',#15026);
#13476=PLANE('',#15040);
#13477=PLANE('',#15041);
#13478=PLANE('',#15042);
#13479=PLANE('',#15043);
#13480=PLANE('',#15044);
#13481=PLANE('',#15045);
#13482=PLANE('',#15046);
#13483=PLANE('',#15047);
#13484=PLANE('',#15048);
#13485=PLANE('',#15049);
#13486=PLANE('',#15050);
#13487=PLANE('',#15051);
#13488=PLANE('',#15052);
#13489=PLANE('',#15054);
#13490=PLANE('',#15073);
#13491=PLANE('',#15074);
#13492=PLANE('',#15075);
#13493=PLANE('',#15076);
#13494=PLANE('',#15077);
#13495=PLANE('',#15078);
#13496=PLANE('',#15126);
#13497=PLANE('',#15127);
#13498=PLANE('',#15128);
#13499=PLANE('',#15129);
#13500=PLANE('',#15130);
#13501=PLANE('',#15131);
#13502=PLANE('',#15132);
#13503=PLANE('',#15133);
#13504=PLANE('',#15137);
#13505=PLANE('',#15138);
#13506=PLANE('',#15143);
#13507=PLANE('',#15144);
#13508=PLANE('',#15212);
#13509=PLANE('',#15215);
#13510=PLANE('',#15218);
#13511=PLANE('',#15221);
#13512=PLANE('',#15222);
#13513=PLANE('',#15223);
#13514=PLANE('',#15230);
#13515=PLANE('',#15231);
#13516=PLANE('',#15251);
#13517=PLANE('',#15252);
#13518=PLANE('',#15380);
#13519=PLANE('',#15381);
#13520=PLANE('',#15383);
#13521=PLANE('',#15384);
#13522=PLANE('',#15385);
#13523=PLANE('',#15386);
#13524=PLANE('',#15387);
#13525=PLANE('',#15388);
#13526=PLANE('',#15391);
#13527=PLANE('',#15416);
#13528=PLANE('',#15418);
#13529=PLANE('',#15419);
#13530=PLANE('',#15420);
#13531=PLANE('',#15421);
#13532=PLANE('',#15422);
#13533=PLANE('',#15423);
#13534=PLANE('',#15424);
#13535=PLANE('',#15432);
#13536=PLANE('',#15433);
#13537=PLANE('',#15473);
#13538=PLANE('',#15474);
#13539=PLANE('',#15475);
#13540=PLANE('',#15476);
#13541=PLANE('',#15477);
#13542=PLANE('',#15478);
#13543=PLANE('',#15479);
#13544=PLANE('',#15480);
#13545=PLANE('',#15484);
#13546=PLANE('',#15485);
#13547=PLANE('',#15493);
#13548=PLANE('',#15494);
#13549=ADVANCED_FACE('',(#2303),#13409,.T.);
#13550=ADVANCED_FACE('',(#2304),#13410,.T.);
#13551=ADVANCED_FACE('',(#2305),#13411,.T.);
#13552=ADVANCED_FACE('',(#2306),#13412,.T.);
#13553=ADVANCED_FACE('',(#2307),#13413,.T.);
#13554=ADVANCED_FACE('',(#2308),#13414,.T.);
#13555=ADVANCED_FACE('',(#2309),#13415,.T.);
#13556=ADVANCED_FACE('',(#2310),#13416,.T.);
#13557=ADVANCED_FACE('',(#2311,#2240),#13417,.T.);
#13558=ADVANCED_FACE('',(#2312,#2241),#13418,.F.);
#13559=ADVANCED_FACE('',(#2313),#13419,.T.);
#13560=ADVANCED_FACE('',(#2314),#13420,.T.);
#13561=ADVANCED_FACE('',(#2315),#13421,.T.);
#13562=ADVANCED_FACE('',(#2316),#13422,.T.);
#13563=ADVANCED_FACE('',(#2317),#13423,.T.);
#13564=ADVANCED_FACE('',(#2318),#13424,.T.);
#13565=ADVANCED_FACE('',(#2319),#13425,.T.);
#13566=ADVANCED_FACE('',(#2320),#13426,.T.);
#13567=ADVANCED_FACE('',(#2321,#2242),#13427,.T.);
#13568=ADVANCED_FACE('',(#2322,#2243),#13428,.F.);
#13569=ADVANCED_FACE('',(#2323),#1590,.F.);
#13570=ADVANCED_FACE('',(#2324),#1591,.F.);
#13571=ADVANCED_FACE('',(#2325),#1592,.F.);
#13572=ADVANCED_FACE('',(#2326),#1593,.F.);
#13573=ADVANCED_FACE('',(#2327),#1594,.F.);
#13574=ADVANCED_FACE('',(#2328),#1595,.F.);
#13575=ADVANCED_FACE('',(#2329),#1596,.F.);
#13576=ADVANCED_FACE('',(#2330),#1597,.F.);
#13577=ADVANCED_FACE('',(#2331),#1598,.F.);
#13578=ADVANCED_FACE('',(#2332),#1599,.F.);
#13579=ADVANCED_FACE('',(#2333),#1600,.F.);
#13580=ADVANCED_FACE('',(#2334),#1601,.F.);
#13581=ADVANCED_FACE('',(#2335),#1602,.F.);
#13582=ADVANCED_FACE('',(#2336),#1603,.F.);
#13583=ADVANCED_FACE('',(#2337),#1604,.F.);
#13584=ADVANCED_FACE('',(#2338),#1605,.F.);
#13585=ADVANCED_FACE('',(#2339),#1606,.F.);
#13586=ADVANCED_FACE('',(#2340),#1607,.F.);
#13587=ADVANCED_FACE('',(#2341),#1608,.F.);
#13588=ADVANCED_FACE('',(#2342),#1609,.F.);
#13589=ADVANCED_FACE('',(#2343),#1610,.F.);
#13590=ADVANCED_FACE('',(#2344),#1611,.F.);
#13591=ADVANCED_FACE('',(#2345),#1612,.F.);
#13592=ADVANCED_FACE('',(#2346),#1613,.F.);
#13593=ADVANCED_FACE('',(#2347),#1614,.F.);
#13594=ADVANCED_FACE('',(#2348),#1615,.F.);
#13595=ADVANCED_FACE('',(#2349),#1616,.F.);
#13596=ADVANCED_FACE('',(#2350),#1617,.F.);
#13597=ADVANCED_FACE('',(#2351),#1618,.F.);
#13598=ADVANCED_FACE('',(#2352),#1619,.F.);
#13599=ADVANCED_FACE('',(#2353),#1620,.F.);
#13600=ADVANCED_FACE('',(#2354),#1621,.F.);
#13601=ADVANCED_FACE('',(#2355),#1622,.F.);
#13602=ADVANCED_FACE('',(#2356),#1623,.F.);
#13603=ADVANCED_FACE('',(#2357),#1624,.F.);
#13604=ADVANCED_FACE('',(#2358),#1625,.F.);
#13605=ADVANCED_FACE('',(#2359),#1626,.F.);
#13606=ADVANCED_FACE('',(#2360),#1627,.F.);
#13607=ADVANCED_FACE('',(#2361),#1628,.F.);
#13608=ADVANCED_FACE('',(#2362),#1629,.F.);
#13609=ADVANCED_FACE('',(#2363),#1630,.F.);
#13610=ADVANCED_FACE('',(#2364),#1631,.F.);
#13611=ADVANCED_FACE('',(#2365),#1632,.F.);
#13612=ADVANCED_FACE('',(#2366),#1633,.F.);
#13613=ADVANCED_FACE('',(#2367),#1634,.F.);
#13614=ADVANCED_FACE('',(#2368),#1635,.F.);
#13615=ADVANCED_FACE('',(#2369),#1636,.F.);
#13616=ADVANCED_FACE('',(#2370),#1637,.F.);
#13617=ADVANCED_FACE('',(#2371),#1638,.F.);
#13618=ADVANCED_FACE('',(#2372),#1639,.F.);
#13619=ADVANCED_FACE('',(#2373),#1640,.F.);
#13620=ADVANCED_FACE('',(#2374),#1641,.F.);
#13621=ADVANCED_FACE('',(#2375),#1642,.F.);
#13622=ADVANCED_FACE('',(#2376),#1643,.F.);
#13623=ADVANCED_FACE('',(#2377),#1644,.F.);
#13624=ADVANCED_FACE('',(#2378),#1645,.F.);
#13625=ADVANCED_FACE('',(#2379),#1646,.F.);
#13626=ADVANCED_FACE('',(#2380),#1647,.F.);
#13627=ADVANCED_FACE('',(#2381),#1648,.F.);
#13628=ADVANCED_FACE('',(#2382),#1649,.F.);
#13629=ADVANCED_FACE('',(#2383),#1650,.F.);
#13630=ADVANCED_FACE('',(#2384),#1651,.F.);
#13631=ADVANCED_FACE('',(#2385),#1652,.F.);
#13632=ADVANCED_FACE('',(#2386),#1653,.F.);
#13633=ADVANCED_FACE('',(#2387),#1654,.F.);
#13634=ADVANCED_FACE('',(#2388),#257,.F.);
#13635=ADVANCED_FACE('',(#2389),#258,.F.);
#13636=ADVANCED_FACE('',(#2390,#2244,#2245,#2246,#2247),#13429,.T.);
#13637=ADVANCED_FACE('',(#2391),#1655,.F.);
#13638=ADVANCED_FACE('',(#2392),#259,.F.);
#13639=ADVANCED_FACE('',(#2393),#260,.F.);
#13640=ADVANCED_FACE('',(#2394),#1656,.F.);
#13641=ADVANCED_FACE('',(#2395),#261,.F.);
#13642=ADVANCED_FACE('',(#2396),#262,.F.);
#13643=ADVANCED_FACE('',(#2397),#1657,.F.);
#13644=ADVANCED_FACE('',(#2398),#263,.F.);
#13645=ADVANCED_FACE('',(#2399),#264,.F.);
#13646=ADVANCED_FACE('',(#2400),#1658,.F.);
#13647=ADVANCED_FACE('',(#2401),#1659,.F.);
#13648=ADVANCED_FACE('',(#2402),#1660,.F.);
#13649=ADVANCED_FACE('',(#2403),#1661,.F.);
#13650=ADVANCED_FACE('',(#2404),#13430,.T.);
#13651=ADVANCED_FACE('',(#2405),#13431,.T.);
#13652=ADVANCED_FACE('',(#2406),#13432,.T.);
#13653=ADVANCED_FACE('',(#2407),#13433,.T.);
#13654=ADVANCED_FACE('',(#2408,#2248,#2249,#2250,#2251),#13434,.F.);
#13655=ADVANCED_FACE('',(#2409),#1662,.T.);
#13656=ADVANCED_FACE('',(#2410),#1663,.T.);
#13657=ADVANCED_FACE('',(#2411),#1664,.T.);
#13658=ADVANCED_FACE('',(#2412),#1665,.T.);
#13659=ADVANCED_FACE('',(#2413),#1666,.T.);
#13660=ADVANCED_FACE('',(#2414),#1667,.T.);
#13661=ADVANCED_FACE('',(#2415),#1668,.T.);
#13662=ADVANCED_FACE('',(#2416),#1669,.T.);
#13663=ADVANCED_FACE('',(#2417),#1670,.T.);
#13664=ADVANCED_FACE('',(#2418),#1671,.T.);
#13665=ADVANCED_FACE('',(#2419),#1672,.T.);
#13666=ADVANCED_FACE('',(#2420),#1673,.T.);
#13667=ADVANCED_FACE('',(#2421),#1674,.T.);
#13668=ADVANCED_FACE('',(#2422),#1675,.T.);
#13669=ADVANCED_FACE('',(#2423),#1676,.T.);
#13670=ADVANCED_FACE('',(#2424),#1677,.T.);
#13671=ADVANCED_FACE('',(#2425),#1678,.T.);
#13672=ADVANCED_FACE('',(#2426),#1679,.T.);
#13673=ADVANCED_FACE('',(#2427),#1680,.T.);
#13674=ADVANCED_FACE('',(#2428),#1681,.T.);
#13675=ADVANCED_FACE('',(#2429),#1682,.T.);
#13676=ADVANCED_FACE('',(#2430),#1683,.T.);
#13677=ADVANCED_FACE('',(#2431),#1684,.T.);
#13678=ADVANCED_FACE('',(#2432),#1685,.T.);
#13679=ADVANCED_FACE('',(#2433),#1686,.T.);
#13680=ADVANCED_FACE('',(#2434),#1687,.T.);
#13681=ADVANCED_FACE('',(#2435),#1688,.T.);
#13682=ADVANCED_FACE('',(#2436),#1689,.T.);
#13683=ADVANCED_FACE('',(#2437),#1690,.T.);
#13684=ADVANCED_FACE('',(#2438),#1691,.T.);
#13685=ADVANCED_FACE('',(#2439),#1692,.T.);
#13686=ADVANCED_FACE('',(#2440),#1693,.T.);
#13687=ADVANCED_FACE('',(#2441),#1694,.T.);
#13688=ADVANCED_FACE('',(#2442),#1695,.T.);
#13689=ADVANCED_FACE('',(#2443),#1696,.T.);
#13690=ADVANCED_FACE('',(#2444),#1697,.T.);
#13691=ADVANCED_FACE('',(#2445),#1698,.T.);
#13692=ADVANCED_FACE('',(#2446),#1699,.T.);
#13693=ADVANCED_FACE('',(#2447),#1700,.T.);
#13694=ADVANCED_FACE('',(#2448),#1701,.T.);
#13695=ADVANCED_FACE('',(#2449),#1702,.T.);
#13696=ADVANCED_FACE('',(#2450),#1703,.T.);
#13697=ADVANCED_FACE('',(#2451),#1704,.T.);
#13698=ADVANCED_FACE('',(#2452),#1705,.T.);
#13699=ADVANCED_FACE('',(#2453),#1706,.T.);
#13700=ADVANCED_FACE('',(#2454),#1707,.T.);
#13701=ADVANCED_FACE('',(#2455),#1708,.T.);
#13702=ADVANCED_FACE('',(#2456),#1709,.T.);
#13703=ADVANCED_FACE('',(#2457),#254,.T.);
#13704=ADVANCED_FACE('',(#2458),#265,.F.);
#13705=ADVANCED_FACE('',(#2459),#1710,.T.);
#13706=ADVANCED_FACE('',(#2460),#266,.F.);
#13707=ADVANCED_FACE('',(#2461),#1711,.T.);
#13708=ADVANCED_FACE('',(#2462),#13435,.F.);
#13709=ADVANCED_FACE('',(#2463),#13436,.F.);
#13710=ADVANCED_FACE('',(#2464),#13437,.F.);
#13711=ADVANCED_FACE('',(#2465),#13438,.F.);
#13712=ADVANCED_FACE('',(#2466),#13439,.F.);
#13713=ADVANCED_FACE('',(#2467),#13440,.F.);
#13714=ADVANCED_FACE('',(#2468),#13441,.F.);
#13715=ADVANCED_FACE('',(#2469,#2252),#13442,.T.);
#13716=ADVANCED_FACE('',(#2470),#1712,.T.);
#13717=ADVANCED_FACE('',(#2471,#2253),#13443,.F.);
#13718=ADVANCED_FACE('',(#2472),#13444,.T.);
#13719=ADVANCED_FACE('',(#2473),#1713,.F.);
#13720=ADVANCED_FACE('',(#2474),#1714,.T.);
#13721=ADVANCED_FACE('',(#2475,#2254),#13445,.T.);
#13722=ADVANCED_FACE('',(#2476,#2255),#13446,.F.);
#13723=ADVANCED_FACE('',(#2477),#1715,.F.);
#13724=ADVANCED_FACE('',(#2478),#1716,.F.);
#13725=ADVANCED_FACE('',(#2479),#1717,.F.);
#13726=ADVANCED_FACE('',(#2480),#1718,.F.);
#13727=ADVANCED_FACE('',(#2481),#1719,.F.);
#13728=ADVANCED_FACE('',(#2482),#1720,.F.);
#13729=ADVANCED_FACE('',(#2483),#1721,.F.);
#13730=ADVANCED_FACE('',(#2484),#1722,.F.);
#13731=ADVANCED_FACE('',(#2485),#1723,.F.);
#13732=ADVANCED_FACE('',(#2486),#1724,.F.);
#13733=ADVANCED_FACE('',(#2487),#1725,.F.);
#13734=ADVANCED_FACE('',(#2488),#1726,.F.);
#13735=ADVANCED_FACE('',(#2489),#1727,.F.);
#13736=ADVANCED_FACE('',(#2490),#1728,.F.);
#13737=ADVANCED_FACE('',(#2491),#1729,.F.);
#13738=ADVANCED_FACE('',(#2492),#1730,.F.);
#13739=ADVANCED_FACE('',(#2493),#1731,.F.);
#13740=ADVANCED_FACE('',(#2494),#1732,.F.);
#13741=ADVANCED_FACE('',(#2495),#1733,.F.);
#13742=ADVANCED_FACE('',(#2496),#1734,.F.);
#13743=ADVANCED_FACE('',(#2497),#1735,.F.);
#13744=ADVANCED_FACE('',(#2498),#1736,.F.);
#13745=ADVANCED_FACE('',(#2499),#1737,.F.);
#13746=ADVANCED_FACE('',(#2500),#1738,.F.);
#13747=ADVANCED_FACE('',(#2501),#1739,.F.);
#13748=ADVANCED_FACE('',(#2502),#1740,.F.);
#13749=ADVANCED_FACE('',(#2503),#1741,.F.);
#13750=ADVANCED_FACE('',(#2504),#1742,.F.);
#13751=ADVANCED_FACE('',(#2505),#1743,.F.);
#13752=ADVANCED_FACE('',(#2506),#1744,.F.);
#13753=ADVANCED_FACE('',(#2507),#1745,.F.);
#13754=ADVANCED_FACE('',(#2508),#1746,.F.);
#13755=ADVANCED_FACE('',(#2509),#1747,.F.);
#13756=ADVANCED_FACE('',(#2510),#1748,.F.);
#13757=ADVANCED_FACE('',(#2511),#1749,.F.);
#13758=ADVANCED_FACE('',(#2512),#1750,.F.);
#13759=ADVANCED_FACE('',(#2513),#1751,.F.);
#13760=ADVANCED_FACE('',(#2514),#1752,.F.);
#13761=ADVANCED_FACE('',(#2515),#1753,.F.);
#13762=ADVANCED_FACE('',(#2516),#1754,.F.);
#13763=ADVANCED_FACE('',(#2517),#1755,.F.);
#13764=ADVANCED_FACE('',(#2518),#1756,.F.);
#13765=ADVANCED_FACE('',(#2519),#1757,.F.);
#13766=ADVANCED_FACE('',(#2520),#1758,.F.);
#13767=ADVANCED_FACE('',(#2521),#1759,.F.);
#13768=ADVANCED_FACE('',(#2522),#1760,.F.);
#13769=ADVANCED_FACE('',(#2523),#1761,.F.);
#13770=ADVANCED_FACE('',(#2524),#1762,.F.);
#13771=ADVANCED_FACE('',(#2525),#1763,.F.);
#13772=ADVANCED_FACE('',(#2526),#1764,.F.);
#13773=ADVANCED_FACE('',(#2527),#1765,.F.);
#13774=ADVANCED_FACE('',(#2528),#1766,.F.);
#13775=ADVANCED_FACE('',(#2529),#1767,.F.);
#13776=ADVANCED_FACE('',(#2530),#1768,.F.);
#13777=ADVANCED_FACE('',(#2531),#1769,.F.);
#13778=ADVANCED_FACE('',(#2532),#1770,.F.);
#13779=ADVANCED_FACE('',(#2533),#1771,.F.);
#13780=ADVANCED_FACE('',(#2534),#1772,.F.);
#13781=ADVANCED_FACE('',(#2535),#1773,.F.);
#13782=ADVANCED_FACE('',(#2536),#1774,.F.);
#13783=ADVANCED_FACE('',(#2537),#1775,.F.);
#13784=ADVANCED_FACE('',(#2538),#1776,.F.);
#13785=ADVANCED_FACE('',(#2539),#1777,.F.);
#13786=ADVANCED_FACE('',(#2540),#1778,.F.);
#13787=ADVANCED_FACE('',(#2541),#1779,.F.);
#13788=ADVANCED_FACE('',(#2542),#1780,.F.);
#13789=ADVANCED_FACE('',(#2543),#1781,.F.);
#13790=ADVANCED_FACE('',(#2544),#1782,.F.);
#13791=ADVANCED_FACE('',(#2545),#1783,.F.);
#13792=ADVANCED_FACE('',(#2546),#1784,.F.);
#13793=ADVANCED_FACE('',(#2547),#1785,.F.);
#13794=ADVANCED_FACE('',(#2548),#1786,.F.);
#13795=ADVANCED_FACE('',(#2549),#1787,.F.);
#13796=ADVANCED_FACE('',(#2550),#1788,.F.);
#13797=ADVANCED_FACE('',(#2551),#1789,.F.);
#13798=ADVANCED_FACE('',(#2552),#1790,.F.);
#13799=ADVANCED_FACE('',(#2553),#1791,.F.);
#13800=ADVANCED_FACE('',(#2554),#1792,.F.);
#13801=ADVANCED_FACE('',(#2555),#1793,.F.);
#13802=ADVANCED_FACE('',(#2556),#1794,.F.);
#13803=ADVANCED_FACE('',(#2557),#1795,.F.);
#13804=ADVANCED_FACE('',(#2558),#1796,.F.);
#13805=ADVANCED_FACE('',(#2559),#1797,.F.);
#13806=ADVANCED_FACE('',(#2560),#1798,.F.);
#13807=ADVANCED_FACE('',(#2561),#1799,.F.);
#13808=ADVANCED_FACE('',(#2562),#1800,.F.);
#13809=ADVANCED_FACE('',(#2563),#1801,.F.);
#13810=ADVANCED_FACE('',(#2564),#1802,.F.);
#13811=ADVANCED_FACE('',(#2565),#1803,.F.);
#13812=ADVANCED_FACE('',(#2566),#1804,.F.);
#13813=ADVANCED_FACE('',(#2567),#1805,.F.);
#13814=ADVANCED_FACE('',(#2568),#1806,.F.);
#13815=ADVANCED_FACE('',(#2569),#1807,.F.);
#13816=ADVANCED_FACE('',(#2570),#1808,.F.);
#13817=ADVANCED_FACE('',(#2571),#1809,.F.);
#13818=ADVANCED_FACE('',(#2572),#1810,.F.);
#13819=ADVANCED_FACE('',(#2573),#1811,.F.);
#13820=ADVANCED_FACE('',(#2574),#1812,.F.);
#13821=ADVANCED_FACE('',(#2575),#1813,.F.);
#13822=ADVANCED_FACE('',(#2576),#1814,.F.);
#13823=ADVANCED_FACE('',(#2577),#1815,.F.);
#13824=ADVANCED_FACE('',(#2578),#1816,.F.);
#13825=ADVANCED_FACE('',(#2579),#1817,.F.);
#13826=ADVANCED_FACE('',(#2580),#1818,.F.);
#13827=ADVANCED_FACE('',(#2581),#1819,.F.);
#13828=ADVANCED_FACE('',(#2582),#1820,.F.);
#13829=ADVANCED_FACE('',(#2583),#1821,.F.);
#13830=ADVANCED_FACE('',(#2584),#1822,.F.);
#13831=ADVANCED_FACE('',(#2585),#1823,.F.);
#13832=ADVANCED_FACE('',(#2586),#1824,.F.);
#13833=ADVANCED_FACE('',(#2587),#1825,.F.);
#13834=ADVANCED_FACE('',(#2588),#1826,.F.);
#13835=ADVANCED_FACE('',(#2589),#1827,.F.);
#13836=ADVANCED_FACE('',(#2590),#1828,.F.);
#13837=ADVANCED_FACE('',(#2591),#1829,.F.);
#13838=ADVANCED_FACE('',(#2592),#1830,.F.);
#13839=ADVANCED_FACE('',(#2593),#1831,.F.);
#13840=ADVANCED_FACE('',(#2594),#1832,.F.);
#13841=ADVANCED_FACE('',(#2595),#1833,.F.);
#13842=ADVANCED_FACE('',(#2596),#1834,.F.);
#13843=ADVANCED_FACE('',(#2597),#1835,.F.);
#13844=ADVANCED_FACE('',(#2598),#1836,.F.);
#13845=ADVANCED_FACE('',(#2599),#1837,.F.);
#13846=ADVANCED_FACE('',(#2600),#1838,.F.);
#13847=ADVANCED_FACE('',(#2601),#1839,.F.);
#13848=ADVANCED_FACE('',(#2602),#1840,.F.);
#13849=ADVANCED_FACE('',(#2603),#1841,.F.);
#13850=ADVANCED_FACE('',(#2604),#1842,.F.);
#13851=ADVANCED_FACE('',(#2605),#1843,.F.);
#13852=ADVANCED_FACE('',(#2606),#1844,.F.);
#13853=ADVANCED_FACE('',(#2607),#13447,.F.);
#13854=ADVANCED_FACE('',(#2608),#1845,.F.);
#13855=ADVANCED_FACE('',(#2609),#267,.F.);
#13856=ADVANCED_FACE('',(#2610),#268,.F.);
#13857=ADVANCED_FACE('',(#2611),#1846,.F.);
#13858=ADVANCED_FACE('',(#2612,#2256),#13448,.F.);
#13859=ADVANCED_FACE('',(#2613),#13449,.T.);
#13860=ADVANCED_FACE('',(#2614),#1847,.F.);
#13861=ADVANCED_FACE('',(#2615),#269,.F.);
#13862=ADVANCED_FACE('',(#2616),#270,.F.);
#13863=ADVANCED_FACE('',(#2617),#1848,.F.);
#13864=ADVANCED_FACE('',(#2618,#2257),#13450,.F.);
#13865=ADVANCED_FACE('',(#2619),#1849,.T.);
#13866=ADVANCED_FACE('',(#2620),#13451,.T.);
#13867=ADVANCED_FACE('',(#2621,#2258,#2259,#2260,#2261,#2262),#13452,.T.);
#13868=ADVANCED_FACE('',(#2622),#1850,.F.);
#13869=ADVANCED_FACE('',(#2623),#13453,.T.);
#13870=ADVANCED_FACE('',(#2624),#1851,.F.);
#13871=ADVANCED_FACE('',(#2625),#13454,.T.);
#13872=ADVANCED_FACE('',(#2626),#1852,.F.);
#13873=ADVANCED_FACE('',(#2627),#13455,.T.);
#13874=ADVANCED_FACE('',(#2628),#1853,.F.);
#13875=ADVANCED_FACE('',(#2629),#13456,.T.);
#13876=ADVANCED_FACE('',(#2630),#1854,.T.);
#13877=ADVANCED_FACE('',(#2631),#1855,.T.);
#13878=ADVANCED_FACE('',(#2632),#13457,.T.);
#13879=ADVANCED_FACE('',(#2633),#1856,.T.);
#13880=ADVANCED_FACE('',(#2634),#1857,.T.);
#13881=ADVANCED_FACE('',(#2635),#13458,.T.);
#13882=ADVANCED_FACE('',(#2636),#1858,.T.);
#13883=ADVANCED_FACE('',(#2637),#1859,.F.);
#13884=ADVANCED_FACE('',(#2638),#13459,.T.);
#13885=ADVANCED_FACE('',(#2639),#1860,.F.);
#13886=ADVANCED_FACE('',(#2640),#13460,.T.);
#13887=ADVANCED_FACE('',(#2641),#1861,.F.);
#13888=ADVANCED_FACE('',(#2642),#13461,.T.);
#13889=ADVANCED_FACE('',(#2643),#1862,.F.);
#13890=ADVANCED_FACE('',(#2644),#13462,.T.);
#13891=ADVANCED_FACE('',(#2645),#1863,.T.);
#13892=ADVANCED_FACE('',(#2646),#1864,.T.);
#13893=ADVANCED_FACE('',(#2647),#13463,.T.);
#13894=ADVANCED_FACE('',(#2648),#1865,.T.);
#13895=ADVANCED_FACE('',(#2649),#1866,.T.);
#13896=ADVANCED_FACE('',(#2650),#13464,.T.);
#13897=ADVANCED_FACE('',(#2651),#1867,.T.);
#13898=ADVANCED_FACE('',(#2652),#1868,.F.);
#13899=ADVANCED_FACE('',(#2653),#13465,.T.);
#13900=ADVANCED_FACE('',(#2654),#1869,.F.);
#13901=ADVANCED_FACE('',(#2655),#13466,.T.);
#13902=ADVANCED_FACE('',(#2656),#1870,.F.);
#13903=ADVANCED_FACE('',(#2657),#13467,.T.);
#13904=ADVANCED_FACE('',(#2658),#1871,.F.);
#13905=ADVANCED_FACE('',(#2659),#13468,.T.);
#13906=ADVANCED_FACE('',(#2660),#1872,.T.);
#13907=ADVANCED_FACE('',(#2661),#1873,.T.);
#13908=ADVANCED_FACE('',(#2662),#13469,.T.);
#13909=ADVANCED_FACE('',(#2663),#1874,.T.);
#13910=ADVANCED_FACE('',(#2664),#1875,.T.);
#13911=ADVANCED_FACE('',(#2665),#13470,.T.);
#13912=ADVANCED_FACE('',(#2666),#1876,.T.);
#13913=ADVANCED_FACE('',(#2667),#1877,.F.);
#13914=ADVANCED_FACE('',(#2668),#13471,.T.);
#13915=ADVANCED_FACE('',(#2669),#1878,.F.);
#13916=ADVANCED_FACE('',(#2670),#13472,.T.);
#13917=ADVANCED_FACE('',(#2671),#1879,.F.);
#13918=ADVANCED_FACE('',(#2672),#13473,.T.);
#13919=ADVANCED_FACE('',(#2673),#1880,.F.);
#13920=ADVANCED_FACE('',(#2674),#13474,.T.);
#13921=ADVANCED_FACE('',(#2675),#1881,.T.);
#13922=ADVANCED_FACE('',(#2676),#1882,.T.);
#13923=ADVANCED_FACE('',(#2677),#13475,.T.);
#13924=ADVANCED_FACE('',(#2678),#1883,.T.);
#13925=ADVANCED_FACE('',(#2679),#1884,.T.);
#13926=ADVANCED_FACE('',(#2680),#1885,.F.);
#13927=ADVANCED_FACE('',(#2681),#1886,.F.);
#13928=ADVANCED_FACE('',(#2682),#1887,.F.);
#13929=ADVANCED_FACE('',(#2683),#1888,.F.);
#13930=ADVANCED_FACE('',(#2684),#1889,.F.);
#13931=ADVANCED_FACE('',(#2685),#13476,.T.);
#13932=ADVANCED_FACE('',(#2686),#13477,.T.);
#13933=ADVANCED_FACE('',(#2687),#13478,.T.);
#13934=ADVANCED_FACE('',(#2688),#13479,.T.);
#13935=ADVANCED_FACE('',(#2689),#13480,.T.);
#13936=ADVANCED_FACE('',(#2690),#13481,.T.);
#13937=ADVANCED_FACE('',(#2691),#13482,.T.);
#13938=ADVANCED_FACE('',(#2692),#13483,.T.);
#13939=ADVANCED_FACE('',(#2693),#13484,.T.);
#13940=ADVANCED_FACE('',(#2694),#13485,.T.);
#13941=ADVANCED_FACE('',(#2695),#13486,.T.);
#13942=ADVANCED_FACE('',(#2696),#13487,.T.);
#13943=ADVANCED_FACE('',(#2697,#2263,#2264,#2265,#2266,#2267),#13488,.F.);
#13944=ADVANCED_FACE('',(#2698,#2268),#13489,.F.);
#13945=ADVANCED_FACE('',(#2699),#1890,.F.);
#13946=ADVANCED_FACE('',(#2700),#1891,.F.);
#13947=ADVANCED_FACE('',(#2701),#1892,.F.);
#13948=ADVANCED_FACE('',(#2702),#1893,.F.);
#13949=ADVANCED_FACE('',(#2703),#1894,.F.);
#13950=ADVANCED_FACE('',(#2704),#1895,.F.);
#13951=ADVANCED_FACE('',(#2705),#13490,.T.);
#13952=ADVANCED_FACE('',(#2706),#13491,.T.);
#13953=ADVANCED_FACE('',(#2707),#13492,.T.);
#13954=ADVANCED_FACE('',(#2708),#13493,.T.);
#13955=ADVANCED_FACE('',(#2709,#2269,#2270,#2271,#2272,#2273),#13494,.T.);
#13956=ADVANCED_FACE('',(#2710,#2274,#2275,#2276,#2277,#2278),#13495,.F.);
#13957=ADVANCED_FACE('',(#2711),#1896,.T.);
#13958=ADVANCED_FACE('',(#2712),#1897,.T.);
#13959=ADVANCED_FACE('',(#2713),#1898,.T.);
#13960=ADVANCED_FACE('',(#2714),#1899,.T.);
#13961=ADVANCED_FACE('',(#2715),#1900,.T.);
#13962=ADVANCED_FACE('',(#2716),#1901,.T.);
#13963=ADVANCED_FACE('',(#2717),#1902,.T.);
#13964=ADVANCED_FACE('',(#2718),#1903,.T.);
#13965=ADVANCED_FACE('',(#2719),#1904,.T.);
#13966=ADVANCED_FACE('',(#2720),#1905,.T.);
#13967=ADVANCED_FACE('',(#2721),#1906,.T.);
#13968=ADVANCED_FACE('',(#2722),#1907,.T.);
#13969=ADVANCED_FACE('',(#2723),#1908,.T.);
#13970=ADVANCED_FACE('',(#2724),#1909,.T.);
#13971=ADVANCED_FACE('',(#2725),#1910,.T.);
#13972=ADVANCED_FACE('',(#2726),#1911,.T.);
#13973=ADVANCED_FACE('',(#2727),#1912,.T.);
#13974=ADVANCED_FACE('',(#2728),#1913,.T.);
#13975=ADVANCED_FACE('',(#2729),#1914,.T.);
#13976=ADVANCED_FACE('',(#2730),#1915,.T.);
#13977=ADVANCED_FACE('',(#2731),#1916,.T.);
#13978=ADVANCED_FACE('',(#2732),#1917,.T.);
#13979=ADVANCED_FACE('',(#2733),#1918,.T.);
#13980=ADVANCED_FACE('',(#2734),#1919,.T.);
#13981=ADVANCED_FACE('',(#2735),#1920,.T.);
#13982=ADVANCED_FACE('',(#2736),#1921,.T.);
#13983=ADVANCED_FACE('',(#2737),#1922,.T.);
#13984=ADVANCED_FACE('',(#2738),#1923,.T.);
#13985=ADVANCED_FACE('',(#2739),#1924,.T.);
#13986=ADVANCED_FACE('',(#2740),#1925,.T.);
#13987=ADVANCED_FACE('',(#2741),#1926,.T.);
#13988=ADVANCED_FACE('',(#2742),#1927,.T.);
#13989=ADVANCED_FACE('',(#2743),#1928,.T.);
#13990=ADVANCED_FACE('',(#2744),#1929,.T.);
#13991=ADVANCED_FACE('',(#2745),#1930,.T.);
#13992=ADVANCED_FACE('',(#2746),#1931,.T.);
#13993=ADVANCED_FACE('',(#2747),#1932,.T.);
#13994=ADVANCED_FACE('',(#2748),#1933,.T.);
#13995=ADVANCED_FACE('',(#2749),#255,.T.);
#13996=ADVANCED_FACE('',(#2750),#271,.F.);
#13997=ADVANCED_FACE('',(#2751),#1934,.T.);
#13998=ADVANCED_FACE('',(#2752),#272,.F.);
#13999=ADVANCED_FACE('',(#2753),#1935,.T.);
#14000=ADVANCED_FACE('',(#2754),#13496,.F.);
#14001=ADVANCED_FACE('',(#2755),#13497,.F.);
#14002=ADVANCED_FACE('',(#2756),#13498,.F.);
#14003=ADVANCED_FACE('',(#2757),#13499,.F.);
#14004=ADVANCED_FACE('',(#2758),#13500,.F.);
#14005=ADVANCED_FACE('',(#2759),#13501,.F.);
#14006=ADVANCED_FACE('',(#2760),#13502,.F.);
#14007=ADVANCED_FACE('',(#2761,#2279),#13503,.T.);
#14008=ADVANCED_FACE('',(#2762),#1936,.T.);
#14009=ADVANCED_FACE('',(#2763,#2280),#13504,.F.);
#14010=ADVANCED_FACE('',(#2764),#13505,.T.);
#14011=ADVANCED_FACE('',(#2765),#1937,.T.);
#14012=ADVANCED_FACE('',(#2766),#13506,.T.);
#14013=ADVANCED_FACE('',(#2767),#13507,.F.);
#14014=ADVANCED_FACE('',(#2768),#1938,.F.);
#14015=ADVANCED_FACE('',(#2769),#1939,.F.);
#14016=ADVANCED_FACE('',(#2770),#1940,.F.);
#14017=ADVANCED_FACE('',(#2771),#1941,.F.);
#14018=ADVANCED_FACE('',(#2772),#1942,.F.);
#14019=ADVANCED_FACE('',(#2773),#1943,.F.);
#14020=ADVANCED_FACE('',(#2774),#1944,.F.);
#14021=ADVANCED_FACE('',(#2775),#1945,.F.);
#14022=ADVANCED_FACE('',(#2776),#1946,.F.);
#14023=ADVANCED_FACE('',(#2777),#1947,.F.);
#14024=ADVANCED_FACE('',(#2778),#1948,.F.);
#14025=ADVANCED_FACE('',(#2779),#1949,.F.);
#14026=ADVANCED_FACE('',(#2780),#1950,.F.);
#14027=ADVANCED_FACE('',(#2781),#1951,.F.);
#14028=ADVANCED_FACE('',(#2782),#1952,.F.);
#14029=ADVANCED_FACE('',(#2783),#1953,.F.);
#14030=ADVANCED_FACE('',(#2784),#1954,.F.);
#14031=ADVANCED_FACE('',(#2785),#1955,.F.);
#14032=ADVANCED_FACE('',(#2786),#1956,.F.);
#14033=ADVANCED_FACE('',(#2787),#1957,.F.);
#14034=ADVANCED_FACE('',(#2788),#1958,.F.);
#14035=ADVANCED_FACE('',(#2789),#1959,.F.);
#14036=ADVANCED_FACE('',(#2790),#1960,.F.);
#14037=ADVANCED_FACE('',(#2791),#1961,.F.);
#14038=ADVANCED_FACE('',(#2792),#1962,.F.);
#14039=ADVANCED_FACE('',(#2793),#1963,.F.);
#14040=ADVANCED_FACE('',(#2794),#1964,.F.);
#14041=ADVANCED_FACE('',(#2795),#1965,.F.);
#14042=ADVANCED_FACE('',(#2796),#1966,.F.);
#14043=ADVANCED_FACE('',(#2797),#1967,.F.);
#14044=ADVANCED_FACE('',(#2798),#1968,.F.);
#14045=ADVANCED_FACE('',(#2799),#1969,.F.);
#14046=ADVANCED_FACE('',(#2800),#1970,.F.);
#14047=ADVANCED_FACE('',(#2801),#1971,.F.);
#14048=ADVANCED_FACE('',(#2802),#1972,.F.);
#14049=ADVANCED_FACE('',(#2803),#1973,.F.);
#14050=ADVANCED_FACE('',(#2804),#1974,.F.);
#14051=ADVANCED_FACE('',(#2805),#1975,.F.);
#14052=ADVANCED_FACE('',(#2806),#1976,.F.);
#14053=ADVANCED_FACE('',(#2807),#1977,.F.);
#14054=ADVANCED_FACE('',(#2808),#1978,.F.);
#14055=ADVANCED_FACE('',(#2809),#1979,.F.);
#14056=ADVANCED_FACE('',(#2810),#1980,.F.);
#14057=ADVANCED_FACE('',(#2811),#1981,.F.);
#14058=ADVANCED_FACE('',(#2812),#1982,.F.);
#14059=ADVANCED_FACE('',(#2813),#1983,.F.);
#14060=ADVANCED_FACE('',(#2814),#1984,.F.);
#14061=ADVANCED_FACE('',(#2815),#1985,.F.);
#14062=ADVANCED_FACE('',(#2816),#13508,.T.);
#14063=ADVANCED_FACE('',(#2817),#1986,.F.);
#14064=ADVANCED_FACE('',(#2818),#273,.F.);
#14065=ADVANCED_FACE('',(#2819),#274,.F.);
#14066=ADVANCED_FACE('',(#2820),#1987,.F.);
#14067=ADVANCED_FACE('',(#2821),#13509,.T.);
#14068=ADVANCED_FACE('',(#2822),#1988,.F.);
#14069=ADVANCED_FACE('',(#2823),#275,.F.);
#14070=ADVANCED_FACE('',(#2824),#276,.F.);
#14071=ADVANCED_FACE('',(#2825),#1989,.F.);
#14072=ADVANCED_FACE('',(#2826),#13510,.T.);
#14073=ADVANCED_FACE('',(#2827),#1990,.F.);
#14074=ADVANCED_FACE('',(#2828),#277,.F.);
#14075=ADVANCED_FACE('',(#2829),#278,.F.);
#14076=ADVANCED_FACE('',(#2830),#1991,.F.);
#14077=ADVANCED_FACE('',(#2831),#13511,.F.);
#14078=ADVANCED_FACE('',(#2832),#13512,.F.);
#14079=ADVANCED_FACE('',(#2833),#13513,.F.);
#14080=ADVANCED_FACE('',(#2834),#11,.F.);
#14081=ADVANCED_FACE('',(#2835),#1992,.T.);
#14082=ADVANCED_FACE('',(#2836,#2281,#2282,#2283,#2284),#13514,.T.);
#14083=ADVANCED_FACE('',(#2837),#13515,.F.);
#14084=ADVANCED_FACE('',(#2838),#1993,.F.);
#14085=ADVANCED_FACE('',(#2839),#1994,.F.);
#14086=ADVANCED_FACE('',(#2840),#1995,.F.);
#14087=ADVANCED_FACE('',(#2841),#12,.F.);
#14088=ADVANCED_FACE('',(#2842),#1996,.F.);
#14089=ADVANCED_FACE('',(#2843),#1997,.T.);
#14090=ADVANCED_FACE('',(#2844,#2285,#2286,#2287,#2288),#13516,.T.);
#14091=ADVANCED_FACE('',(#2845,#2289,#2290,#2291,#2292),#13517,.F.);
#14092=ADVANCED_FACE('',(#2846),#1998,.T.);
#14093=ADVANCED_FACE('',(#2847),#1999,.T.);
#14094=ADVANCED_FACE('',(#2848),#2000,.T.);
#14095=ADVANCED_FACE('',(#2849),#2001,.T.);
#14096=ADVANCED_FACE('',(#2850),#2002,.T.);
#14097=ADVANCED_FACE('',(#2851),#2003,.T.);
#14098=ADVANCED_FACE('',(#2852),#2004,.T.);
#14099=ADVANCED_FACE('',(#2853),#2005,.T.);
#14100=ADVANCED_FACE('',(#2854),#2006,.T.);
#14101=ADVANCED_FACE('',(#2855),#2007,.T.);
#14102=ADVANCED_FACE('',(#2856),#2008,.T.);
#14103=ADVANCED_FACE('',(#2857),#2009,.T.);
#14104=ADVANCED_FACE('',(#2858),#2010,.T.);
#14105=ADVANCED_FACE('',(#2859),#2011,.T.);
#14106=ADVANCED_FACE('',(#2860),#2012,.T.);
#14107=ADVANCED_FACE('',(#2861),#2013,.T.);
#14108=ADVANCED_FACE('',(#2862),#2014,.T.);
#14109=ADVANCED_FACE('',(#2863),#2015,.T.);
#14110=ADVANCED_FACE('',(#2864),#2016,.T.);
#14111=ADVANCED_FACE('',(#2865),#2017,.T.);
#14112=ADVANCED_FACE('',(#2866),#2018,.T.);
#14113=ADVANCED_FACE('',(#2867),#2019,.T.);
#14114=ADVANCED_FACE('',(#2868),#2020,.T.);
#14115=ADVANCED_FACE('',(#2869),#2021,.T.);
#14116=ADVANCED_FACE('',(#2870),#2022,.T.);
#14117=ADVANCED_FACE('',(#2871),#2023,.T.);
#14118=ADVANCED_FACE('',(#2872),#2024,.T.);
#14119=ADVANCED_FACE('',(#2873),#2025,.T.);
#14120=ADVANCED_FACE('',(#2874),#2026,.T.);
#14121=ADVANCED_FACE('',(#2875),#2027,.T.);
#14122=ADVANCED_FACE('',(#2876),#2028,.T.);
#14123=ADVANCED_FACE('',(#2877),#2029,.T.);
#14124=ADVANCED_FACE('',(#2878),#2030,.T.);
#14125=ADVANCED_FACE('',(#2879),#2031,.T.);
#14126=ADVANCED_FACE('',(#2880),#2032,.T.);
#14127=ADVANCED_FACE('',(#2881),#2033,.T.);
#14128=ADVANCED_FACE('',(#2882),#2034,.T.);
#14129=ADVANCED_FACE('',(#2883),#2035,.T.);
#14130=ADVANCED_FACE('',(#2884),#2036,.T.);
#14131=ADVANCED_FACE('',(#2885),#2037,.T.);
#14132=ADVANCED_FACE('',(#2886),#2038,.T.);
#14133=ADVANCED_FACE('',(#2887),#2039,.T.);
#14134=ADVANCED_FACE('',(#2888),#2040,.T.);
#14135=ADVANCED_FACE('',(#2889),#2041,.T.);
#14136=ADVANCED_FACE('',(#2890),#2042,.T.);
#14137=ADVANCED_FACE('',(#2891),#2043,.T.);
#14138=ADVANCED_FACE('',(#2892),#2044,.T.);
#14139=ADVANCED_FACE('',(#2893),#2045,.T.);
#14140=ADVANCED_FACE('',(#2894),#2046,.T.);
#14141=ADVANCED_FACE('',(#2895),#2047,.T.);
#14142=ADVANCED_FACE('',(#2896),#2048,.T.);
#14143=ADVANCED_FACE('',(#2897),#2049,.T.);
#14144=ADVANCED_FACE('',(#2898),#2050,.T.);
#14145=ADVANCED_FACE('',(#2899),#2051,.T.);
#14146=ADVANCED_FACE('',(#2900),#2052,.T.);
#14147=ADVANCED_FACE('',(#2901),#2053,.T.);
#14148=ADVANCED_FACE('',(#2902),#2054,.T.);
#14149=ADVANCED_FACE('',(#2903),#2055,.T.);
#14150=ADVANCED_FACE('',(#2904),#2056,.T.);
#14151=ADVANCED_FACE('',(#2905),#2057,.T.);
#14152=ADVANCED_FACE('',(#2906),#2058,.T.);
#14153=ADVANCED_FACE('',(#2907),#2059,.T.);
#14154=ADVANCED_FACE('',(#2908),#2060,.T.);
#14155=ADVANCED_FACE('',(#2909),#2061,.T.);
#14156=ADVANCED_FACE('',(#2910),#2062,.T.);
#14157=ADVANCED_FACE('',(#2911),#2063,.T.);
#14158=ADVANCED_FACE('',(#2912),#2064,.T.);
#14159=ADVANCED_FACE('',(#2913),#2065,.T.);
#14160=ADVANCED_FACE('',(#2914),#2066,.T.);
#14161=ADVANCED_FACE('',(#2915),#2067,.T.);
#14162=ADVANCED_FACE('',(#2916),#2068,.T.);
#14163=ADVANCED_FACE('',(#2917),#2069,.T.);
#14164=ADVANCED_FACE('',(#2918),#2070,.T.);
#14165=ADVANCED_FACE('',(#2919),#2071,.T.);
#14166=ADVANCED_FACE('',(#2920),#2072,.T.);
#14167=ADVANCED_FACE('',(#2921),#2073,.T.);
#14168=ADVANCED_FACE('',(#2922),#2074,.T.);
#14169=ADVANCED_FACE('',(#2923),#2075,.T.);
#14170=ADVANCED_FACE('',(#2924),#2076,.T.);
#14171=ADVANCED_FACE('',(#2925),#2077,.T.);
#14172=ADVANCED_FACE('',(#2926),#2078,.T.);
#14173=ADVANCED_FACE('',(#2927),#2079,.T.);
#14174=ADVANCED_FACE('',(#2928),#2080,.T.);
#14175=ADVANCED_FACE('',(#2929),#2081,.T.);
#14176=ADVANCED_FACE('',(#2930),#2082,.T.);
#14177=ADVANCED_FACE('',(#2931),#2083,.T.);
#14178=ADVANCED_FACE('',(#2932),#2084,.T.);
#14179=ADVANCED_FACE('',(#2933),#2085,.T.);
#14180=ADVANCED_FACE('',(#2934),#2086,.T.);
#14181=ADVANCED_FACE('',(#2935),#2087,.T.);
#14182=ADVANCED_FACE('',(#2936),#2088,.T.);
#14183=ADVANCED_FACE('',(#2937),#2089,.T.);
#14184=ADVANCED_FACE('',(#2938),#2090,.T.);
#14185=ADVANCED_FACE('',(#2939),#2091,.T.);
#14186=ADVANCED_FACE('',(#2940),#2092,.T.);
#14187=ADVANCED_FACE('',(#2941),#2093,.T.);
#14188=ADVANCED_FACE('',(#2942),#2094,.T.);
#14189=ADVANCED_FACE('',(#2943),#2095,.T.);
#14190=ADVANCED_FACE('',(#2944),#2096,.T.);
#14191=ADVANCED_FACE('',(#2945),#2097,.T.);
#14192=ADVANCED_FACE('',(#2946),#2098,.T.);
#14193=ADVANCED_FACE('',(#2947),#2099,.T.);
#14194=ADVANCED_FACE('',(#2948),#2100,.T.);
#14195=ADVANCED_FACE('',(#2949),#2101,.T.);
#14196=ADVANCED_FACE('',(#2950),#2102,.T.);
#14197=ADVANCED_FACE('',(#2951),#2103,.T.);
#14198=ADVANCED_FACE('',(#2952),#2104,.T.);
#14199=ADVANCED_FACE('',(#2953),#2105,.T.);
#14200=ADVANCED_FACE('',(#2954),#2106,.T.);
#14201=ADVANCED_FACE('',(#2955),#2107,.T.);
#14202=ADVANCED_FACE('',(#2956),#2108,.T.);
#14203=ADVANCED_FACE('',(#2957),#2109,.T.);
#14204=ADVANCED_FACE('',(#2958),#2110,.T.);
#14205=ADVANCED_FACE('',(#2959),#2111,.T.);
#14206=ADVANCED_FACE('',(#2960),#2112,.T.);
#14207=ADVANCED_FACE('',(#2961),#2113,.T.);
#14208=ADVANCED_FACE('',(#2962),#2114,.T.);
#14209=ADVANCED_FACE('',(#2963),#2115,.T.);
#14210=ADVANCED_FACE('',(#2964),#2116,.T.);
#14211=ADVANCED_FACE('',(#2965),#2117,.T.);
#14212=ADVANCED_FACE('',(#2966),#279,.F.);
#14213=ADVANCED_FACE('',(#2967),#2118,.T.);
#14214=ADVANCED_FACE('',(#2968),#280,.F.);
#14215=ADVANCED_FACE('',(#2969),#2119,.T.);
#14216=ADVANCED_FACE('',(#2970,#2293),#13518,.T.);
#14217=ADVANCED_FACE('',(#2971,#2294),#13519,.F.);
#14218=ADVANCED_FACE('',(#2972),#13520,.T.);
#14219=ADVANCED_FACE('',(#2973),#13521,.T.);
#14220=ADVANCED_FACE('',(#2974),#13522,.T.);
#14221=ADVANCED_FACE('',(#2975),#13523,.T.);
#14222=ADVANCED_FACE('',(#2976),#13524,.T.);
#14223=ADVANCED_FACE('',(#2977),#13525,.T.);
#14224=ADVANCED_FACE('',(#2978),#2120,.T.);
#14225=ADVANCED_FACE('',(#2979),#13526,.T.);
#14226=ADVANCED_FACE('',(#2980),#13,.T.);
#14227=ADVANCED_FACE('',(#2981),#2121,.F.);
#14228=ADVANCED_FACE('',(#2982),#2122,.F.);
#14229=ADVANCED_FACE('',(#2983),#2123,.F.);
#14230=ADVANCED_FACE('',(#2984),#2124,.F.);
#14231=ADVANCED_FACE('',(#2985),#2125,.F.);
#14232=ADVANCED_FACE('',(#2986),#2126,.F.);
#14233=ADVANCED_FACE('',(#2987),#2127,.F.);
#14234=ADVANCED_FACE('',(#2988),#2128,.F.);
#14235=ADVANCED_FACE('',(#2989),#2129,.F.);
#14236=ADVANCED_FACE('',(#2990),#2130,.F.);
#14237=ADVANCED_FACE('',(#2991),#2131,.F.);
#14238=ADVANCED_FACE('',(#2992),#2132,.F.);
#14239=ADVANCED_FACE('',(#2993),#2133,.F.);
#14240=ADVANCED_FACE('',(#2994),#2134,.F.);
#14241=ADVANCED_FACE('',(#2995),#2135,.F.);
#14242=ADVANCED_FACE('',(#2996),#2136,.F.);
#14243=ADVANCED_FACE('',(#2997),#2137,.F.);
#14244=ADVANCED_FACE('',(#2998),#281,.F.);
#14245=ADVANCED_FACE('',(#2999),#282,.F.);
#14246=ADVANCED_FACE('',(#3000,#2295),#13527,.T.);
#14247=ADVANCED_FACE('',(#3001),#2138,.F.);
#14248=ADVANCED_FACE('',(#3002),#13528,.T.);
#14249=ADVANCED_FACE('',(#3003),#13529,.T.);
#14250=ADVANCED_FACE('',(#3004),#13530,.T.);
#14251=ADVANCED_FACE('',(#3005),#13531,.T.);
#14252=ADVANCED_FACE('',(#3006),#13532,.T.);
#14253=ADVANCED_FACE('',(#3007),#13533,.T.);
#14254=ADVANCED_FACE('',(#3008,#2296),#13534,.F.);
#14255=ADVANCED_FACE('',(#3009),#2139,.F.);
#14256=ADVANCED_FACE('',(#3010),#2140,.T.);
#14257=ADVANCED_FACE('',(#3011,#2297),#13535,.T.);
#14258=ADVANCED_FACE('',(#3012,#2298),#13536,.F.);
#14259=ADVANCED_FACE('',(#3013),#2141,.T.);
#14260=ADVANCED_FACE('',(#3014),#2142,.T.);
#14261=ADVANCED_FACE('',(#3015),#2143,.T.);
#14262=ADVANCED_FACE('',(#3016),#2144,.T.);
#14263=ADVANCED_FACE('',(#3017),#2145,.T.);
#14264=ADVANCED_FACE('',(#3018),#2146,.T.);
#14265=ADVANCED_FACE('',(#3019),#2147,.T.);
#14266=ADVANCED_FACE('',(#3020),#2148,.T.);
#14267=ADVANCED_FACE('',(#3021),#2149,.T.);
#14268=ADVANCED_FACE('',(#3022),#2150,.T.);
#14269=ADVANCED_FACE('',(#3023),#2151,.T.);
#14270=ADVANCED_FACE('',(#3024),#2152,.T.);
#14271=ADVANCED_FACE('',(#3025),#2153,.T.);
#14272=ADVANCED_FACE('',(#3026),#2154,.T.);
#14273=ADVANCED_FACE('',(#3027),#2155,.T.);
#14274=ADVANCED_FACE('',(#3028),#2156,.T.);
#14275=ADVANCED_FACE('',(#3029),#2157,.T.);
#14276=ADVANCED_FACE('',(#3030),#2158,.T.);
#14277=ADVANCED_FACE('',(#3031),#2159,.T.);
#14278=ADVANCED_FACE('',(#3032),#2160,.T.);
#14279=ADVANCED_FACE('',(#3033),#2161,.T.);
#14280=ADVANCED_FACE('',(#3034),#2162,.T.);
#14281=ADVANCED_FACE('',(#3035),#2163,.T.);
#14282=ADVANCED_FACE('',(#3036),#2164,.T.);
#14283=ADVANCED_FACE('',(#3037),#2165,.T.);
#14284=ADVANCED_FACE('',(#3038),#2166,.T.);
#14285=ADVANCED_FACE('',(#3039),#2167,.T.);
#14286=ADVANCED_FACE('',(#3040),#2168,.T.);
#14287=ADVANCED_FACE('',(#3041),#2169,.T.);
#14288=ADVANCED_FACE('',(#3042),#2170,.T.);
#14289=ADVANCED_FACE('',(#3043),#256,.T.);
#14290=ADVANCED_FACE('',(#3044),#283,.F.);
#14291=ADVANCED_FACE('',(#3045),#2171,.T.);
#14292=ADVANCED_FACE('',(#3046),#284,.F.);
#14293=ADVANCED_FACE('',(#3047),#2172,.T.);
#14294=ADVANCED_FACE('',(#3048),#13537,.F.);
#14295=ADVANCED_FACE('',(#3049),#13538,.F.);
#14296=ADVANCED_FACE('',(#3050),#13539,.F.);
#14297=ADVANCED_FACE('',(#3051),#13540,.F.);
#14298=ADVANCED_FACE('',(#3052),#13541,.F.);
#14299=ADVANCED_FACE('',(#3053),#13542,.F.);
#14300=ADVANCED_FACE('',(#3054),#13543,.F.);
#14301=ADVANCED_FACE('',(#3055,#2299),#13544,.T.);
#14302=ADVANCED_FACE('',(#3056),#2173,.T.);
#14303=ADVANCED_FACE('',(#3057,#2300),#13545,.F.);
#14304=ADVANCED_FACE('',(#3058),#13546,.T.);
#14305=ADVANCED_FACE('',(#3059),#2174,.F.);
#14306=ADVANCED_FACE('',(#3060),#2175,.T.);
#14307=ADVANCED_FACE('',(#3061,#2301),#13547,.T.);
#14308=ADVANCED_FACE('',(#3062,#2302),#13548,.F.);
#14309=CLOSED_SHELL('',(#13549,#13550,#13551,#13552,#13553,#13554,#13555,
#13556,#13557,#13558));
#14310=CLOSED_SHELL('',(#13559,#13560,#13561,#13562,#13563,#13564,#13565,
#13566,#13567,#13568));
#14311=CLOSED_SHELL('',(#13569,#13570,#13571,#13572,#13573,#13574,#13575,
#13576,#13577,#13578,#13579,#13580,#13581,#13582,#13583,#13584,#13585,#13586,
#13587,#13588,#13589,#13590,#13591,#13592,#13593,#13594,#13595,#13596,#13597,
#13598,#13599,#13600,#13601,#13602,#13603,#13604,#13605,#13606,#13607,#13608,
#13609,#13610,#13611,#13612,#13613,#13614,#13615,#13616,#13617,#13618,#13619,
#13620,#13621,#13622,#13623,#13624,#13625,#13626,#13627,#13628,#13629,#13630,
#13631,#13632,#13633,#13634,#13635,#13636,#13637,#13638,#13639,#13640,#13641,
#13642,#13643,#13644,#13645,#13646,#13647,#13648,#13649,#13650,#13651,#13652,
#13653,#13654));
#14312=CLOSED_SHELL('',(#13655,#13656,#13657,#13658,#13659,#13660,#13661,
#13662,#13663,#13664,#13665,#13666,#13667,#13668,#13669,#13670,#13671,#13672,
#13673,#13674,#13675,#13676,#13677,#13678,#13679,#13680,#13681,#13682,#13683,
#13684,#13685,#13686,#13687,#13688,#13689,#13690,#13691,#13692,#13693,#13694,
#13695,#13696,#13697,#13698,#13699,#13700,#13701,#13702,#13703,#13704,#13705,
#13706,#13707,#13708,#13709,#13710,#13711,#13712,#13713,#13714,#13715,#13716,
#13717,#13718));
#14313=CLOSED_SHELL('',(#13719,#13720,#13721,#13722));
#14314=CLOSED_SHELL('',(#13723,#13724,#13725,#13726,#13727,#13728,#13729,
#13730,#13731,#13732,#13733,#13734,#13735,#13736,#13737,#13738,#13739,#13740,
#13741,#13742,#13743,#13744,#13745,#13746,#13747,#13748,#13749,#13750,#13751,
#13752,#13753,#13754,#13755,#13756,#13757,#13758,#13759,#13760,#13761,#13762,
#13763,#13764,#13765,#13766,#13767,#13768,#13769,#13770,#13771,#13772,#13773,
#13774,#13775,#13776,#13777,#13778,#13779,#13780,#13781,#13782,#13783,#13784,
#13785,#13786,#13787,#13788,#13789,#13790,#13791,#13792,#13793,#13794,#13795,
#13796,#13797,#13798,#13799,#13800,#13801,#13802,#13803,#13804,#13805,#13806,
#13807,#13808,#13809,#13810,#13811,#13812,#13813,#13814,#13815,#13816,#13817,
#13818,#13819,#13820,#13821,#13822,#13823,#13824,#13825,#13826,#13827,#13828,
#13829,#13830,#13831,#13832,#13833,#13834,#13835,#13836,#13837,#13838,#13839,
#13840,#13841,#13842,#13843,#13844,#13845,#13846,#13847,#13848,#13849,#13850,
#13851,#13852,#13853,#13854,#13855,#13856,#13857,#13858,#13859,#13860,#13861,
#13862,#13863,#13864,#13865,#13866,#13867,#13868,#13869,#13870,#13871,#13872,
#13873,#13874,#13875,#13876,#13877,#13878,#13879,#13880,#13881,#13882,#13883,
#13884,#13885,#13886,#13887,#13888,#13889,#13890,#13891,#13892,#13893,#13894,
#13895,#13896,#13897,#13898,#13899,#13900,#13901,#13902,#13903,#13904,#13905,
#13906,#13907,#13908,#13909,#13910,#13911,#13912,#13913,#13914,#13915,#13916,
#13917,#13918,#13919,#13920,#13921,#13922,#13923,#13924,#13925,#13926,#13927,
#13928,#13929,#13930,#13931,#13932,#13933,#13934,#13935,#13936,#13937,#13938,
#13939,#13940,#13941,#13942,#13943));
#14315=CLOSED_SHELL('',(#13944,#13945,#13946,#13947,#13948,#13949,#13950,
#13951,#13952,#13953,#13954,#13955,#13956));
#14316=CLOSED_SHELL('',(#13957,#13958,#13959,#13960,#13961,#13962,#13963,
#13964,#13965,#13966,#13967,#13968,#13969,#13970,#13971,#13972,#13973,#13974,
#13975,#13976,#13977,#13978,#13979,#13980,#13981,#13982,#13983,#13984,#13985,
#13986,#13987,#13988,#13989,#13990,#13991,#13992,#13993,#13994,#13995,#13996,
#13997,#13998,#13999,#14000,#14001,#14002,#14003,#14004,#14005,#14006,#14007,
#14008,#14009,#14010));
#14317=CLOSED_SHELL('',(#14011,#14012,#14013));
#14318=CLOSED_SHELL('',(#14014,#14015,#14016,#14017,#14018,#14019,#14020,
#14021,#14022,#14023,#14024,#14025,#14026,#14027,#14028,#14029,#14030,#14031,
#14032,#14033,#14034,#14035,#14036,#14037,#14038,#14039,#14040,#14041,#14042,
#14043,#14044,#14045,#14046,#14047,#14048,#14049,#14050,#14051,#14052,#14053,
#14054,#14055,#14056,#14057,#14058,#14059,#14060,#14061,#14062,#14063,#14064,
#14065,#14066,#14067,#14068,#14069,#14070,#14071,#14072,#14073,#14074,#14075,
#14076,#14077,#14078,#14079,#14080,#14081,#14082,#14083));
#14319=CLOSED_SHELL('',(#14084,#14085,#14086,#14087,#14088,#14089,#14090,
#14091));
#14320=CLOSED_SHELL('',(#14092,#14093,#14094,#14095,#14096,#14097,#14098,
#14099,#14100,#14101,#14102,#14103,#14104,#14105,#14106,#14107,#14108,#14109,
#14110,#14111,#14112,#14113,#14114,#14115,#14116,#14117,#14118,#14119,#14120,
#14121,#14122,#14123,#14124,#14125,#14126,#14127,#14128,#14129,#14130,#14131,
#14132,#14133,#14134,#14135,#14136,#14137,#14138,#14139,#14140,#14141,#14142,
#14143,#14144,#14145,#14146,#14147,#14148,#14149,#14150,#14151,#14152,#14153,
#14154,#14155,#14156,#14157,#14158,#14159,#14160,#14161,#14162,#14163,#14164,
#14165,#14166,#14167,#14168,#14169,#14170,#14171,#14172,#14173,#14174,#14175,
#14176,#14177,#14178,#14179,#14180,#14181,#14182,#14183,#14184,#14185,#14186,
#14187,#14188,#14189,#14190,#14191,#14192,#14193,#14194,#14195,#14196,#14197,
#14198,#14199,#14200,#14201,#14202,#14203,#14204,#14205,#14206,#14207,#14208,
#14209,#14210,#14211,#14212,#14213,#14214,#14215,#14216,#14217,#14218,#14219,
#14220,#14221,#14222,#14223,#14224,#14225,#14226));
#14321=CLOSED_SHELL('',(#14227,#14228,#14229,#14230,#14231,#14232,#14233,
#14234,#14235,#14236,#14237,#14238,#14239,#14240,#14241,#14242,#14243,#14244,
#14245,#14246,#14247,#14248,#14249,#14250,#14251,#14252,#14253,#14254));
#14322=CLOSED_SHELL('',(#14255,#14256,#14257,#14258));
#14323=CLOSED_SHELL('',(#14259,#14260,#14261,#14262,#14263,#14264,#14265,
#14266,#14267,#14268,#14269,#14270,#14271,#14272,#14273,#14274,#14275,#14276,
#14277,#14278,#14279,#14280,#14281,#14282,#14283,#14284,#14285,#14286,#14287,
#14288,#14289,#14290,#14291,#14292,#14293,#14294,#14295,#14296,#14297,#14298,
#14299,#14300,#14301,#14302,#14303,#14304));
#14324=CLOSED_SHELL('',(#14305,#14306,#14307,#14308));
#14325=DERIVED_UNIT_ELEMENT(#14357,1.);
#14326=DERIVED_UNIT_ELEMENT(#63757,-3.);
#14327=DERIVED_UNIT_ELEMENT(#14357,1.);
#14328=DERIVED_UNIT_ELEMENT(#63757,-3.);
#14329=DERIVED_UNIT_ELEMENT(#14357,1.);
#14330=DERIVED_UNIT_ELEMENT(#63757,-3.);
#14331=DERIVED_UNIT_ELEMENT(#14357,1.);
#14332=DERIVED_UNIT_ELEMENT(#63757,-3.);
#14333=DERIVED_UNIT_ELEMENT(#14357,1.);
#14334=DERIVED_UNIT_ELEMENT(#63757,-3.);
#14335=DERIVED_UNIT_ELEMENT(#14357,1.);
#14336=DERIVED_UNIT_ELEMENT(#63757,-3.);
#14337=DERIVED_UNIT_ELEMENT(#14357,1.);
#14338=DERIVED_UNIT_ELEMENT(#63757,-3.);
#14339=DERIVED_UNIT_ELEMENT(#14357,1.);
#14340=DERIVED_UNIT_ELEMENT(#63757,-3.);
#14341=DERIVED_UNIT_ELEMENT(#14357,1.);
#14342=DERIVED_UNIT_ELEMENT(#63757,-3.);
#14343=DERIVED_UNIT_ELEMENT(#14357,1.);
#14344=DERIVED_UNIT_ELEMENT(#63757,-3.);
#14345=DERIVED_UNIT_ELEMENT(#14357,1.);
#14346=DERIVED_UNIT_ELEMENT(#63757,-3.);
#14347=DERIVED_UNIT_ELEMENT(#14357,1.);
#14348=DERIVED_UNIT_ELEMENT(#63757,-3.);
#14349=DERIVED_UNIT_ELEMENT(#14357,1.);
#14350=DERIVED_UNIT_ELEMENT(#63757,-3.);
#14351=DERIVED_UNIT_ELEMENT(#14357,1.);
#14352=DERIVED_UNIT_ELEMENT(#63757,-3.);
#14353=DERIVED_UNIT_ELEMENT(#14357,1.);
#14354=DERIVED_UNIT_ELEMENT(#63757,-3.);
#14355=DERIVED_UNIT_ELEMENT(#14357,1.);
#14356=DERIVED_UNIT_ELEMENT(#63757,-3.);
#14357=(
MASS_UNIT()
NAMED_UNIT(*)
SI_UNIT(.KILO.,.GRAM.)
);
#14358=DERIVED_UNIT((#14325,#14326));
#14359=DERIVED_UNIT((#14327,#14328));
#14360=DERIVED_UNIT((#14329,#14330));
#14361=DERIVED_UNIT((#14331,#14332));
#14362=DERIVED_UNIT((#14333,#14334));
#14363=DERIVED_UNIT((#14335,#14336));
#14364=DERIVED_UNIT((#14337,#14338));
#14365=DERIVED_UNIT((#14339,#14340));
#14366=DERIVED_UNIT((#14341,#14342));
#14367=DERIVED_UNIT((#14343,#14344));
#14368=DERIVED_UNIT((#14345,#14346));
#14369=DERIVED_UNIT((#14347,#14348));
#14370=DERIVED_UNIT((#14349,#14350));
#14371=DERIVED_UNIT((#14351,#14352));
#14372=DERIVED_UNIT((#14353,#14354));
#14373=DERIVED_UNIT((#14355,#14356));
#14374=MEASURE_REPRESENTATION_ITEM('density measure',
POSITIVE_RATIO_MEASURE(7850.),#14358);
#14375=MEASURE_REPRESENTATION_ITEM('density measure',
POSITIVE_RATIO_MEASURE(7850.),#14359);
#14376=MEASURE_REPRESENTATION_ITEM('density measure',
POSITIVE_RATIO_MEASURE(7850.),#14360);
#14377=MEASURE_REPRESENTATION_ITEM('density measure',
POSITIVE_RATIO_MEASURE(7850.),#14361);
#14378=MEASURE_REPRESENTATION_ITEM('density measure',
POSITIVE_RATIO_MEASURE(7850.),#14362);
#14379=MEASURE_REPRESENTATION_ITEM('density measure',
POSITIVE_RATIO_MEASURE(2700.),#14363);
#14380=MEASURE_REPRESENTATION_ITEM('density measure',
POSITIVE_RATIO_MEASURE(7850.),#14364);
#14381=MEASURE_REPRESENTATION_ITEM('density measure',
POSITIVE_RATIO_MEASURE(7850.),#14365);
#14382=MEASURE_REPRESENTATION_ITEM('density measure',
POSITIVE_RATIO_MEASURE(7850.),#14366);
#14383=MEASURE_REPRESENTATION_ITEM('density measure',
POSITIVE_RATIO_MEASURE(7850.),#14367);
#14384=MEASURE_REPRESENTATION_ITEM('density measure',
POSITIVE_RATIO_MEASURE(7850.),#14368);
#14385=MEASURE_REPRESENTATION_ITEM('density measure',
POSITIVE_RATIO_MEASURE(7850.),#14369);
#14386=MEASURE_REPRESENTATION_ITEM('density measure',
POSITIVE_RATIO_MEASURE(7850.),#14370);
#14387=MEASURE_REPRESENTATION_ITEM('density measure',
POSITIVE_RATIO_MEASURE(7850.),#14371);
#14388=MEASURE_REPRESENTATION_ITEM('density measure',
POSITIVE_RATIO_MEASURE(7850.),#14372);
#14389=MEASURE_REPRESENTATION_ITEM('density measure',
POSITIVE_RATIO_MEASURE(7850.),#14373);
#14390=PROPERTY_DEFINITION_REPRESENTATION(#14470,#14422);
#14391=PROPERTY_DEFINITION_REPRESENTATION(#14471,#14423);
#14392=PROPERTY_DEFINITION_REPRESENTATION(#14472,#14424);
#14393=PROPERTY_DEFINITION_REPRESENTATION(#14473,#14425);
#14394=PROPERTY_DEFINITION_REPRESENTATION(#14474,#14426);
#14395=PROPERTY_DEFINITION_REPRESENTATION(#14475,#14427);
#14396=PROPERTY_DEFINITION_REPRESENTATION(#14476,#14428);
#14397=PROPERTY_DEFINITION_REPRESENTATION(#14477,#14429);
#14398=PROPERTY_DEFINITION_REPRESENTATION(#14478,#14430);
#14399=PROPERTY_DEFINITION_REPRESENTATION(#14479,#14431);
#14400=PROPERTY_DEFINITION_REPRESENTATION(#14480,#14432);
#14401=PROPERTY_DEFINITION_REPRESENTATION(#14481,#14433);
#14402=PROPERTY_DEFINITION_REPRESENTATION(#14482,#14434);
#14403=PROPERTY_DEFINITION_REPRESENTATION(#14483,#14435);
#14404=PROPERTY_DEFINITION_REPRESENTATION(#14484,#14436);
#14405=PROPERTY_DEFINITION_REPRESENTATION(#14485,#14437);
#14406=PROPERTY_DEFINITION_REPRESENTATION(#14486,#14438);
#14407=PROPERTY_DEFINITION_REPRESENTATION(#14487,#14439);
#14408=PROPERTY_DEFINITION_REPRESENTATION(#14488,#14440);
#14409=PROPERTY_DEFINITION_REPRESENTATION(#14489,#14441);
#14410=PROPERTY_DEFINITION_REPRESENTATION(#14490,#14442);
#14411=PROPERTY_DEFINITION_REPRESENTATION(#14491,#14443);
#14412=PROPERTY_DEFINITION_REPRESENTATION(#14492,#14444);
#14413=PROPERTY_DEFINITION_REPRESENTATION(#14493,#14445);
#14414=PROPERTY_DEFINITION_REPRESENTATION(#14494,#14446);
#14415=PROPERTY_DEFINITION_REPRESENTATION(#14495,#14447);
#14416=PROPERTY_DEFINITION_REPRESENTATION(#14496,#14448);
#14417=PROPERTY_DEFINITION_REPRESENTATION(#14497,#14449);
#14418=PROPERTY_DEFINITION_REPRESENTATION(#14498,#14450);
#14419=PROPERTY_DEFINITION_REPRESENTATION(#14499,#14451);
#14420=PROPERTY_DEFINITION_REPRESENTATION(#14500,#14452);
#14421=PROPERTY_DEFINITION_REPRESENTATION(#14501,#14453);
#14422=REPRESENTATION('material name',(#14454),#63738);
#14423=REPRESENTATION('density',(#14374),#63738);
#14424=REPRESENTATION('material name',(#14455),#63739);
#14425=REPRESENTATION('density',(#14375),#63739);
#14426=REPRESENTATION('material name',(#14456),#63740);
#14427=REPRESENTATION('density',(#14376),#63740);
#14428=REPRESENTATION('material name',(#14457),#63741);
#14429=REPRESENTATION('density',(#14377),#63741);
#14430=REPRESENTATION('material name',(#14458),#63742);
#14431=REPRESENTATION('density',(#14378),#63742);
#14432=REPRESENTATION('material name',(#14459),#63744);
#14433=REPRESENTATION('density',(#14379),#63744);
#14434=REPRESENTATION('material name',(#14460),#63745);
#14435=REPRESENTATION('density',(#14380),#63745);
#14436=REPRESENTATION('material name',(#14461),#63746);
#14437=REPRESENTATION('density',(#14381),#63746);
#14438=REPRESENTATION('material name',(#14462),#63747);
#14439=REPRESENTATION('density',(#14382),#63747);
#14440=REPRESENTATION('material name',(#14463),#63748);
#14441=REPRESENTATION('density',(#14383),#63748);
#14442=REPRESENTATION('material name',(#14464),#63749);
#14443=REPRESENTATION('density',(#14384),#63749);
#14444=REPRESENTATION('material name',(#14465),#63750);
#14445=REPRESENTATION('density',(#14385),#63750);
#14446=REPRESENTATION('material name',(#14466),#63751);
#14447=REPRESENTATION('density',(#14386),#63751);
#14448=REPRESENTATION('material name',(#14467),#63752);
#14449=REPRESENTATION('density',(#14387),#63752);
#14450=REPRESENTATION('material name',(#14468),#63753);
#14451=REPRESENTATION('density',(#14388),#63753);
#14452=REPRESENTATION('material name',(#14469),#63754);
#14453=REPRESENTATION('density',(#14389),#63754);
#14454=DESCRIPTIVE_REPRESENTATION_ITEM('Steel','Steel');
#14455=DESCRIPTIVE_REPRESENTATION_ITEM('Steel','Steel');
#14456=DESCRIPTIVE_REPRESENTATION_ITEM('Steel','Steel');
#14457=DESCRIPTIVE_REPRESENTATION_ITEM('Steel','Steel');
#14458=DESCRIPTIVE_REPRESENTATION_ITEM('Steel','Steel');
#14459=DESCRIPTIVE_REPRESENTATION_ITEM('Aluminum 6061','Aluminum 6061');
#14460=DESCRIPTIVE_REPRESENTATION_ITEM('Steel','Steel');
#14461=DESCRIPTIVE_REPRESENTATION_ITEM('Steel','Steel');
#14462=DESCRIPTIVE_REPRESENTATION_ITEM('Steel','Steel');
#14463=DESCRIPTIVE_REPRESENTATION_ITEM('Steel','Steel');
#14464=DESCRIPTIVE_REPRESENTATION_ITEM('Steel','Steel');
#14465=DESCRIPTIVE_REPRESENTATION_ITEM('Steel','Steel');
#14466=DESCRIPTIVE_REPRESENTATION_ITEM('Steel','Steel');
#14467=DESCRIPTIVE_REPRESENTATION_ITEM('Steel','Steel');
#14468=DESCRIPTIVE_REPRESENTATION_ITEM('Steel','Steel');
#14469=DESCRIPTIVE_REPRESENTATION_ITEM('Steel','Steel');
#14470=PROPERTY_DEFINITION('material property','material name',#63880);
#14471=PROPERTY_DEFINITION('material property','density of part',#63880);
#14472=PROPERTY_DEFINITION('material property','material name',#63881);
#14473=PROPERTY_DEFINITION('material property','density of part',#63881);
#14474=PROPERTY_DEFINITION('material property','material name',#63882);
#14475=PROPERTY_DEFINITION('material property','density of part',#63882);
#14476=PROPERTY_DEFINITION('material property','material name',#63883);
#14477=PROPERTY_DEFINITION('material property','density of part',#63883);
#14478=PROPERTY_DEFINITION('material property','material name',#63884);
#14479=PROPERTY_DEFINITION('material property','density of part',#63884);
#14480=PROPERTY_DEFINITION('material property','material name',#63886);
#14481=PROPERTY_DEFINITION('material property','density of part',#63886);
#14482=PROPERTY_DEFINITION('material property','material name',#63887);
#14483=PROPERTY_DEFINITION('material property','density of part',#63887);
#14484=PROPERTY_DEFINITION('material property','material name',#63888);
#14485=PROPERTY_DEFINITION('material property','density of part',#63888);
#14486=PROPERTY_DEFINITION('material property','material name',#63889);
#14487=PROPERTY_DEFINITION('material property','density of part',#63889);
#14488=PROPERTY_DEFINITION('material property','material name',#63890);
#14489=PROPERTY_DEFINITION('material property','density of part',#63890);
#14490=PROPERTY_DEFINITION('material property','material name',#63891);
#14491=PROPERTY_DEFINITION('material property','density of part',#63891);
#14492=PROPERTY_DEFINITION('material property','material name',#63892);
#14493=PROPERTY_DEFINITION('material property','density of part',#63892);
#14494=PROPERTY_DEFINITION('material property','material name',#63893);
#14495=PROPERTY_DEFINITION('material property','density of part',#63893);
#14496=PROPERTY_DEFINITION('material property','material name',#63894);
#14497=PROPERTY_DEFINITION('material property','density of part',#63894);
#14498=PROPERTY_DEFINITION('material property','material name',#63895);
#14499=PROPERTY_DEFINITION('material property','density of part',#63895);
#14500=PROPERTY_DEFINITION('material property','material name',#63896);
#14501=PROPERTY_DEFINITION('material property','density of part',#63896);
#14502=AXIS2_PLACEMENT_3D('',#18377,#15515,#15516);
#14503=AXIS2_PLACEMENT_3D('',#18378,#15517,#15518);
#14504=AXIS2_PLACEMENT_3D('',#18379,#15519,#15520);
#14505=AXIS2_PLACEMENT_3D('',#18380,#15521,#15522);
#14506=AXIS2_PLACEMENT_3D('',#18389,#15527,#15528);
#14507=AXIS2_PLACEMENT_3D('',#18395,#15532,#15533);
#14508=AXIS2_PLACEMENT_3D('',#18401,#15537,#15538);
#14509=AXIS2_PLACEMENT_3D('',#18404,#15541,#15542);
#14510=AXIS2_PLACEMENT_3D('',#18413,#15547,#15548);
#14511=AXIS2_PLACEMENT_3D('',#18419,#15552,#15553);
#14512=AXIS2_PLACEMENT_3D('',#18425,#15557,#15558);
#14513=AXIS2_PLACEMENT_3D('',#18428,#15561,#15562);
#14514=AXIS2_PLACEMENT_3D('',#18429,#15563,#15564);
#14515=AXIS2_PLACEMENT_3D('',#18430,#15565,#15566);
#14516=AXIS2_PLACEMENT_3D('',#18431,#15567,#15568);
#14517=AXIS2_PLACEMENT_3D('',#18440,#15573,#15574);
#14518=AXIS2_PLACEMENT_3D('',#18446,#15578,#15579);
#14519=AXIS2_PLACEMENT_3D('',#18452,#15583,#15584);
#14520=AXIS2_PLACEMENT_3D('',#18455,#15587,#15588);
#14521=AXIS2_PLACEMENT_3D('',#18464,#15593,#15594);
#14522=AXIS2_PLACEMENT_3D('',#18470,#15598,#15599);
#14523=AXIS2_PLACEMENT_3D('',#18476,#15603,#15604);
#14524=AXIS2_PLACEMENT_3D('',#18479,#15607,#15608);
#14525=AXIS2_PLACEMENT_3D('',#18480,#15609,#15610);
#14526=AXIS2_PLACEMENT_3D('',#18481,#15611,#15612);
#14527=AXIS2_PLACEMENT_3D('',#18482,#15613,#15614);
#14528=AXIS2_PLACEMENT_3D('',#18492,#15616,#15617);
#14529=AXIS2_PLACEMENT_3D('',#18503,#15618,#15619);
#14530=AXIS2_PLACEMENT_3D('',#18554,#15621,#15622);
#14531=AXIS2_PLACEMENT_3D('',#18605,#15624,#15625);
#14532=AXIS2_PLACEMENT_3D('',#18653,#15627,#15628);
#14533=AXIS2_PLACEMENT_3D('',#18704,#15630,#15631);
#14534=AXIS2_PLACEMENT_3D('',#18755,#15633,#15634);
#14535=AXIS2_PLACEMENT_3D('',#18803,#15636,#15637);
#14536=AXIS2_PLACEMENT_3D('',#18822,#15639,#15640);
#14537=AXIS2_PLACEMENT_3D('',#18842,#15641,#15642);
#14538=AXIS2_PLACEMENT_3D('',#18852,#15644,#15645);
#14539=AXIS2_PLACEMENT_3D('',#18863,#15646,#15647);
#14540=AXIS2_PLACEMENT_3D('',#18914,#15649,#15650);
#14541=AXIS2_PLACEMENT_3D('',#18965,#15652,#15653);
#14542=AXIS2_PLACEMENT_3D('',#19013,#15655,#15656);
#14543=AXIS2_PLACEMENT_3D('',#19064,#15658,#15659);
#14544=AXIS2_PLACEMENT_3D('',#19115,#15661,#15662);
#14545=AXIS2_PLACEMENT_3D('',#19163,#15664,#15665);
#14546=AXIS2_PLACEMENT_3D('',#19182,#15667,#15668);
#14547=AXIS2_PLACEMENT_3D('',#19202,#15669,#15670);
#14548=AXIS2_PLACEMENT_3D('',#19212,#15672,#15673);
#14549=AXIS2_PLACEMENT_3D('',#19223,#15674,#15675);
#14550=AXIS2_PLACEMENT_3D('',#19274,#15677,#15678);
#14551=AXIS2_PLACEMENT_3D('',#19325,#15680,#15681);
#14552=AXIS2_PLACEMENT_3D('',#19373,#15683,#15684);
#14553=AXIS2_PLACEMENT_3D('',#19424,#15686,#15687);
#14554=AXIS2_PLACEMENT_3D('',#19475,#15689,#15690);
#14555=AXIS2_PLACEMENT_3D('',#19523,#15692,#15693);
#14556=AXIS2_PLACEMENT_3D('',#19542,#15695,#15696);
#14557=AXIS2_PLACEMENT_3D('',#19562,#15697,#15698);
#14558=AXIS2_PLACEMENT_3D('',#19572,#15700,#15701);
#14559=AXIS2_PLACEMENT_3D('',#19583,#15702,#15703);
#14560=AXIS2_PLACEMENT_3D('',#19634,#15705,#15706);
#14561=AXIS2_PLACEMENT_3D('',#19685,#15708,#15709);
#14562=AXIS2_PLACEMENT_3D('',#19733,#15711,#15712);
#14563=AXIS2_PLACEMENT_3D('',#19784,#15714,#15715);
#14564=AXIS2_PLACEMENT_3D('',#19835,#15717,#15718);
#14565=AXIS2_PLACEMENT_3D('',#19883,#15720,#15721);
#14566=AXIS2_PLACEMENT_3D('',#19902,#15723,#15724);
#14567=AXIS2_PLACEMENT_3D('',#19922,#15725,#15726);
#14568=AXIS2_PLACEMENT_3D('',#19936,#15728,#15729);
#14569=AXIS2_PLACEMENT_3D('',#19946,#15730,#15731);
#14570=AXIS2_PLACEMENT_3D('',#19970,#15733,#15734);
#14571=AXIS2_PLACEMENT_3D('',#19995,#15736,#15737);
#14572=AXIS2_PLACEMENT_3D('',#20020,#15739,#15740);
#14573=AXIS2_PLACEMENT_3D('',#20044,#15742,#15743);
#14574=AXIS2_PLACEMENT_3D('',#20069,#15745,#15746);
#14575=AXIS2_PLACEMENT_3D('',#20094,#15748,#15749);
#14576=AXIS2_PLACEMENT_3D('',#20105,#15751,#15752);
#14577=AXIS2_PLACEMENT_3D('',#20111,#15753,#15754);
#14578=AXIS2_PLACEMENT_3D('',#20125,#15756,#15757);
#14579=AXIS2_PLACEMENT_3D('',#20135,#15758,#15759);
#14580=AXIS2_PLACEMENT_3D('',#20159,#15761,#15762);
#14581=AXIS2_PLACEMENT_3D('',#20184,#15764,#15765);
#14582=AXIS2_PLACEMENT_3D('',#20209,#15767,#15768);
#14583=AXIS2_PLACEMENT_3D('',#20233,#15770,#15771);
#14584=AXIS2_PLACEMENT_3D('',#20258,#15773,#15774);
#14585=AXIS2_PLACEMENT_3D('',#20283,#15776,#15777);
#14586=AXIS2_PLACEMENT_3D('',#20294,#15779,#15780);
#14587=AXIS2_PLACEMENT_3D('',#20300,#15781,#15782);
#14588=AXIS2_PLACEMENT_3D('',#20314,#15784,#15785);
#14589=AXIS2_PLACEMENT_3D('',#20324,#15786,#15787);
#14590=AXIS2_PLACEMENT_3D('',#20348,#15789,#15790);
#14591=AXIS2_PLACEMENT_3D('',#20373,#15792,#15793);
#14592=AXIS2_PLACEMENT_3D('',#20398,#15795,#15796);
#14593=AXIS2_PLACEMENT_3D('',#20422,#15798,#15799);
#14594=AXIS2_PLACEMENT_3D('',#20447,#15801,#15802);
#14595=AXIS2_PLACEMENT_3D('',#20472,#15804,#15805);
#14596=AXIS2_PLACEMENT_3D('',#20483,#15807,#15808);
#14597=AXIS2_PLACEMENT_3D('',#20489,#15809,#15810);
#14598=AXIS2_PLACEMENT_3D('',#20503,#15812,#15813);
#14599=AXIS2_PLACEMENT_3D('',#20513,#15814,#15815);
#14600=AXIS2_PLACEMENT_3D('',#20537,#15817,#15818);
#14601=AXIS2_PLACEMENT_3D('',#20562,#15820,#15821);
#14602=AXIS2_PLACEMENT_3D('',#20587,#15823,#15824);
#14603=AXIS2_PLACEMENT_3D('',#20611,#15826,#15827);
#14604=AXIS2_PLACEMENT_3D('',#20636,#15829,#15830);
#14605=AXIS2_PLACEMENT_3D('',#20661,#15832,#15833);
#14606=AXIS2_PLACEMENT_3D('',#20672,#15835,#15836);
#14607=AXIS2_PLACEMENT_3D('',#20678,#15837,#15838);
#14608=AXIS2_PLACEMENT_3D('',#21580,#15839,#15840);
#14609=AXIS2_PLACEMENT_3D('',#22162,#15845,#15846);
#14610=AXIS2_PLACEMENT_3D('',#22873,#15847,#15848);
#14611=AXIS2_PLACEMENT_3D('',#23584,#15849,#15850);
#14612=AXIS2_PLACEMENT_3D('',#24295,#15851,#15852);
#14613=AXIS2_PLACEMENT_3D('',#24296,#15853,#15854);
#14614=AXIS2_PLACEMENT_3D('',#24297,#15855,#15856);
#14615=AXIS2_PLACEMENT_3D('',#24298,#15857,#15858);
#14616=AXIS2_PLACEMENT_3D('',#24299,#15859,#15860);
#14617=AXIS2_PLACEMENT_3D('',#24305,#15864,#15865);
#14618=AXIS2_PLACEMENT_3D('',#24309,#15868,#15869);
#14619=AXIS2_PLACEMENT_3D('',#24313,#15872,#15873);
#14620=AXIS2_PLACEMENT_3D('',#24315,#15875,#15876);
#14621=AXIS2_PLACEMENT_3D('',#24316,#15877,#15878);
#14622=AXIS2_PLACEMENT_3D('',#24317,#15879,#15880);
#14623=AXIS2_PLACEMENT_3D('',#24333,#15882,#15883);
#14624=AXIS2_PLACEMENT_3D('',#24341,#15884,#15885);
#14625=AXIS2_PLACEMENT_3D('',#24389,#15887,#15888);
#14626=AXIS2_PLACEMENT_3D('',#24437,#15890,#15891);
#14627=AXIS2_PLACEMENT_3D('',#24485,#15893,#15894);
#14628=AXIS2_PLACEMENT_3D('',#24539,#15896,#15897);
#14629=AXIS2_PLACEMENT_3D('',#24587,#15899,#15900);
#14630=AXIS2_PLACEMENT_3D('',#24635,#15902,#15903);
#14631=AXIS2_PLACEMENT_3D('',#24689,#15905,#15906);
#14632=AXIS2_PLACEMENT_3D('',#24737,#15908,#15909);
#14633=AXIS2_PLACEMENT_3D('',#24785,#15911,#15912);
#14634=AXIS2_PLACEMENT_3D('',#24839,#15914,#15915);
#14635=AXIS2_PLACEMENT_3D('',#24887,#15917,#15918);
#14636=AXIS2_PLACEMENT_3D('',#24935,#15920,#15921);
#14637=AXIS2_PLACEMENT_3D('',#24983,#15923,#15924);
#14638=AXIS2_PLACEMENT_3D('',#25037,#15926,#15927);
#14639=AXIS2_PLACEMENT_3D('',#25085,#15929,#15930);
#14640=AXIS2_PLACEMENT_3D('',#25133,#15932,#15933);
#14641=AXIS2_PLACEMENT_3D('',#25187,#15935,#15936);
#14642=AXIS2_PLACEMENT_3D('',#25235,#15938,#15939);
#14643=AXIS2_PLACEMENT_3D('',#25283,#15941,#15942);
#14644=AXIS2_PLACEMENT_3D('',#25331,#15944,#15945);
#14645=AXIS2_PLACEMENT_3D('',#25385,#15947,#15948);
#14646=AXIS2_PLACEMENT_3D('',#25433,#15950,#15951);
#14647=AXIS2_PLACEMENT_3D('',#25481,#15953,#15954);
#14648=AXIS2_PLACEMENT_3D('',#25497,#15956,#15957);
#14649=AXIS2_PLACEMENT_3D('',#25506,#15958,#15959);
#14650=AXIS2_PLACEMENT_3D('',#25531,#15961,#15962);
#14651=AXIS2_PLACEMENT_3D('',#25555,#15964,#15965);
#14652=AXIS2_PLACEMENT_3D('',#25580,#15967,#15968);
#14653=AXIS2_PLACEMENT_3D('',#25605,#15970,#15971);
#14654=AXIS2_PLACEMENT_3D('',#25629,#15973,#15974);
#14655=AXIS2_PLACEMENT_3D('',#25653,#15976,#15977);
#14656=AXIS2_PLACEMENT_3D('',#25678,#15979,#15980);
#14657=AXIS2_PLACEMENT_3D('',#25703,#15982,#15983);
#14658=AXIS2_PLACEMENT_3D('',#25727,#15985,#15986);
#14659=AXIS2_PLACEMENT_3D('',#25752,#15988,#15989);
#14660=AXIS2_PLACEMENT_3D('',#25777,#15991,#15992);
#14661=AXIS2_PLACEMENT_3D('',#25801,#15994,#15995);
#14662=AXIS2_PLACEMENT_3D('',#25825,#15997,#15998);
#14663=AXIS2_PLACEMENT_3D('',#25850,#16000,#16001);
#14664=AXIS2_PLACEMENT_3D('',#25875,#16003,#16004);
#14665=AXIS2_PLACEMENT_3D('',#25899,#16006,#16007);
#14666=AXIS2_PLACEMENT_3D('',#25924,#16009,#16010);
#14667=AXIS2_PLACEMENT_3D('',#25949,#16012,#16013);
#14668=AXIS2_PLACEMENT_3D('',#25973,#16015,#16016);
#14669=AXIS2_PLACEMENT_3D('',#25998,#16018,#16019);
#14670=AXIS2_PLACEMENT_3D('',#26023,#16021,#16022);
#14671=AXIS2_PLACEMENT_3D('',#26047,#16024,#16025);
#14672=AXIS2_PLACEMENT_3D('',#26071,#16027,#16028);
#14673=AXIS2_PLACEMENT_3D('',#26374,#16029,#16030);
#14674=AXIS2_PLACEMENT_3D('',#26408,#16032,#16033);
#14675=AXIS2_PLACEMENT_3D('',#27166,#16034,#16035);
#14676=AXIS2_PLACEMENT_3D('',#27177,#16036,#16037);
#14677=AXIS2_PLACEMENT_3D('',#27937,#16038,#16039);
#14678=AXIS2_PLACEMENT_3D('',#27938,#16040,#16041);
#14679=AXIS2_PLACEMENT_3D('',#27947,#16046,#16047);
#14680=AXIS2_PLACEMENT_3D('',#27953,#16051,#16052);
#14681=AXIS2_PLACEMENT_3D('',#27959,#16056,#16057);
#14682=AXIS2_PLACEMENT_3D('',#27965,#16061,#16062);
#14683=AXIS2_PLACEMENT_3D('',#27971,#16066,#16067);
#14684=AXIS2_PLACEMENT_3D('',#27974,#16070,#16071);
#14685=AXIS2_PLACEMENT_3D('',#27975,#16072,#16073);
#14686=AXIS2_PLACEMENT_3D('',#27977,#16074,#16075);
#14687=AXIS2_PLACEMENT_3D('',#27978,#16076,#16077);
#14688=AXIS2_PLACEMENT_3D('',#27981,#16079,#16080);
#14689=AXIS2_PLACEMENT_3D('',#27982,#16081,#16082);
#14690=AXIS2_PLACEMENT_3D('',#27983,#16083,#16084);
#14691=AXIS2_PLACEMENT_3D('',#27984,#16085,#16086);
#14692=AXIS2_PLACEMENT_3D('',#27985,#16087,#16088);
#14693=AXIS2_PLACEMENT_3D('',#27987,#16089,#16090);
#14694=AXIS2_PLACEMENT_3D('',#27990,#16092,#16093);
#14695=AXIS2_PLACEMENT_3D('',#27991,#16094,#16095);
#14696=AXIS2_PLACEMENT_3D('',#27993,#16096,#16097);
#14697=AXIS2_PLACEMENT_3D('',#27996,#16099,#16100);
#14698=AXIS2_PLACEMENT_3D('',#27997,#16101,#16102);
#14699=AXIS2_PLACEMENT_3D('',#27998,#16103,#16104);
#14700=AXIS2_PLACEMENT_3D('',#27999,#16105,#16106);
#14701=AXIS2_PLACEMENT_3D('',#28000,#16107,#16108);
#14702=AXIS2_PLACEMENT_3D('',#28001,#16109,#16110);
#14703=AXIS2_PLACEMENT_3D('',#28002,#16111,#16112);
#14704=AXIS2_PLACEMENT_3D('',#28003,#16113,#16114);
#14705=AXIS2_PLACEMENT_3D('',#28004,#16115,#16116);
#14706=AXIS2_PLACEMENT_3D('',#28005,#16117,#16118);
#14707=AXIS2_PLACEMENT_3D('',#28006,#16119,#16120);
#14708=AXIS2_PLACEMENT_3D('',#28007,#16121,#16122);
#14709=AXIS2_PLACEMENT_3D('',#28008,#16123,#16124);
#14710=AXIS2_PLACEMENT_3D('',#28009,#16125,#16126);
#14711=AXIS2_PLACEMENT_3D('',#28010,#16127,#16128);
#14712=AXIS2_PLACEMENT_3D('',#28011,#16129,#16130);
#14713=AXIS2_PLACEMENT_3D('',#28012,#16131,#16132);
#14714=AXIS2_PLACEMENT_3D('',#28013,#16133,#16134);
#14715=AXIS2_PLACEMENT_3D('',#28014,#16135,#16136);
#14716=AXIS2_PLACEMENT_3D('',#28015,#16137,#16138);
#14717=AXIS2_PLACEMENT_3D('',#28016,#16139,#16140);
#14718=AXIS2_PLACEMENT_3D('',#28017,#16141,#16142);
#14719=AXIS2_PLACEMENT_3D('',#28018,#16143,#16144);
#14720=AXIS2_PLACEMENT_3D('',#28019,#16145,#16146);
#14721=AXIS2_PLACEMENT_3D('',#28020,#16147,#16148);
#14722=AXIS2_PLACEMENT_3D('',#28021,#16149,#16150);
#14723=AXIS2_PLACEMENT_3D('',#28022,#16151,#16152);
#14724=AXIS2_PLACEMENT_3D('',#28023,#16153,#16154);
#14725=AXIS2_PLACEMENT_3D('',#28024,#16155,#16156);
#14726=AXIS2_PLACEMENT_3D('',#28025,#16157,#16158);
#14727=AXIS2_PLACEMENT_3D('',#28026,#16159,#16160);
#14728=AXIS2_PLACEMENT_3D('',#28027,#16161,#16162);
#14729=AXIS2_PLACEMENT_3D('',#28028,#16163,#16164);
#14730=AXIS2_PLACEMENT_3D('',#28029,#16165,#16166);
#14731=AXIS2_PLACEMENT_3D('',#28030,#16167,#16168);
#14732=AXIS2_PLACEMENT_3D('',#28031,#16169,#16170);
#14733=AXIS2_PLACEMENT_3D('',#28032,#16171,#16172);
#14734=AXIS2_PLACEMENT_3D('',#28033,#16173,#16174);
#14735=AXIS2_PLACEMENT_3D('',#28034,#16175,#16176);
#14736=AXIS2_PLACEMENT_3D('',#28035,#16177,#16178);
#14737=AXIS2_PLACEMENT_3D('',#28036,#16179,#16180);
#14738=AXIS2_PLACEMENT_3D('',#28037,#16181,#16182);
#14739=AXIS2_PLACEMENT_3D('',#28038,#16183,#16184);
#14740=AXIS2_PLACEMENT_3D('',#28039,#16185,#16186);
#14741=AXIS2_PLACEMENT_3D('',#28040,#16187,#16188);
#14742=AXIS2_PLACEMENT_3D('',#28041,#16189,#16190);
#14743=AXIS2_PLACEMENT_3D('',#28054,#16192,#16193);
#14744=AXIS2_PLACEMENT_3D('',#28057,#16195,#16196);
#14745=AXIS2_PLACEMENT_3D('',#28059,#16197,#16198);
#14746=AXIS2_PLACEMENT_3D('',#28076,#16199,#16200);
#14747=AXIS2_PLACEMENT_3D('',#28166,#16202,#16203);
#14748=AXIS2_PLACEMENT_3D('',#28253,#16205,#16206);
#14749=AXIS2_PLACEMENT_3D('',#28340,#16208,#16209);
#14750=AXIS2_PLACEMENT_3D('',#28427,#16211,#16212);
#14751=AXIS2_PLACEMENT_3D('',#28517,#16214,#16215);
#14752=AXIS2_PLACEMENT_3D('',#28604,#16217,#16218);
#14753=AXIS2_PLACEMENT_3D('',#28691,#16220,#16221);
#14754=AXIS2_PLACEMENT_3D('',#28781,#16223,#16224);
#14755=AXIS2_PLACEMENT_3D('',#28868,#16226,#16227);
#14756=AXIS2_PLACEMENT_3D('',#28955,#16229,#16230);
#14757=AXIS2_PLACEMENT_3D('',#29042,#16232,#16233);
#14758=AXIS2_PLACEMENT_3D('',#29132,#16235,#16236);
#14759=AXIS2_PLACEMENT_3D('',#29219,#16238,#16239);
#14760=AXIS2_PLACEMENT_3D('',#29306,#16241,#16242);
#14761=AXIS2_PLACEMENT_3D('',#29393,#16244,#16245);
#14762=AXIS2_PLACEMENT_3D('',#29483,#16247,#16248);
#14763=AXIS2_PLACEMENT_3D('',#29570,#16250,#16251);
#14764=AXIS2_PLACEMENT_3D('',#29657,#16253,#16254);
#14765=AXIS2_PLACEMENT_3D('',#29747,#16256,#16257);
#14766=AXIS2_PLACEMENT_3D('',#29834,#16259,#16260);
#14767=AXIS2_PLACEMENT_3D('',#29921,#16262,#16263);
#14768=AXIS2_PLACEMENT_3D('',#30008,#16265,#16266);
#14769=AXIS2_PLACEMENT_3D('',#30098,#16268,#16269);
#14770=AXIS2_PLACEMENT_3D('',#30129,#16271,#16272);
#14771=AXIS2_PLACEMENT_3D('',#30167,#16273,#16274);
#14772=AXIS2_PLACEMENT_3D('',#30185,#16276,#16277);
#14773=AXIS2_PLACEMENT_3D('',#30200,#16278,#16279);
#14774=AXIS2_PLACEMENT_3D('',#30237,#16281,#16282);
#14775=AXIS2_PLACEMENT_3D('',#30275,#16284,#16285);
#14776=AXIS2_PLACEMENT_3D('',#30311,#16287,#16288);
#14777=AXIS2_PLACEMENT_3D('',#30349,#16290,#16291);
#14778=AXIS2_PLACEMENT_3D('',#30387,#16293,#16294);
#14779=AXIS2_PLACEMENT_3D('',#30423,#16296,#16297);
#14780=AXIS2_PLACEMENT_3D('',#30461,#16299,#16300);
#14781=AXIS2_PLACEMENT_3D('',#30499,#16302,#16303);
#14782=AXIS2_PLACEMENT_3D('',#30535,#16305,#16306);
#14783=AXIS2_PLACEMENT_3D('',#30573,#16308,#16309);
#14784=AXIS2_PLACEMENT_3D('',#30610,#16311,#16312);
#14785=AXIS2_PLACEMENT_3D('',#30647,#16314,#16315);
#14786=AXIS2_PLACEMENT_3D('',#30685,#16317,#16318);
#14787=AXIS2_PLACEMENT_3D('',#30721,#16320,#16321);
#14788=AXIS2_PLACEMENT_3D('',#30759,#16323,#16324);
#14789=AXIS2_PLACEMENT_3D('',#30797,#16326,#16327);
#14790=AXIS2_PLACEMENT_3D('',#30833,#16329,#16330);
#14791=AXIS2_PLACEMENT_3D('',#30871,#16332,#16333);
#14792=AXIS2_PLACEMENT_3D('',#30909,#16335,#16336);
#14793=AXIS2_PLACEMENT_3D('',#30945,#16338,#16339);
#14794=AXIS2_PLACEMENT_3D('',#30983,#16341,#16342);
#14795=AXIS2_PLACEMENT_3D('',#31020,#16344,#16345);
#14796=AXIS2_PLACEMENT_3D('',#31057,#16347,#16348);
#14797=AXIS2_PLACEMENT_3D('',#31069,#16350,#16351);
#14798=AXIS2_PLACEMENT_3D('',#31077,#16352,#16353);
#14799=AXIS2_PLACEMENT_3D('',#31090,#16355,#16356);
#14800=AXIS2_PLACEMENT_3D('',#31093,#16358,#16359);
#14801=AXIS2_PLACEMENT_3D('',#31095,#16360,#16361);
#14802=AXIS2_PLACEMENT_3D('',#31112,#16362,#16363);
#14803=AXIS2_PLACEMENT_3D('',#31202,#16365,#16366);
#14804=AXIS2_PLACEMENT_3D('',#31289,#16368,#16369);
#14805=AXIS2_PLACEMENT_3D('',#31376,#16371,#16372);
#14806=AXIS2_PLACEMENT_3D('',#31463,#16374,#16375);
#14807=AXIS2_PLACEMENT_3D('',#31550,#16377,#16378);
#14808=AXIS2_PLACEMENT_3D('',#31640,#16380,#16381);
#14809=AXIS2_PLACEMENT_3D('',#31727,#16383,#16384);
#14810=AXIS2_PLACEMENT_3D('',#31814,#16386,#16387);
#14811=AXIS2_PLACEMENT_3D('',#31901,#16389,#16390);
#14812=AXIS2_PLACEMENT_3D('',#31988,#16392,#16393);
#14813=AXIS2_PLACEMENT_3D('',#32078,#16395,#16396);
#14814=AXIS2_PLACEMENT_3D('',#32165,#16398,#16399);
#14815=AXIS2_PLACEMENT_3D('',#32252,#16401,#16402);
#14816=AXIS2_PLACEMENT_3D('',#32339,#16404,#16405);
#14817=AXIS2_PLACEMENT_3D('',#32426,#16407,#16408);
#14818=AXIS2_PLACEMENT_3D('',#32513,#16410,#16411);
#14819=AXIS2_PLACEMENT_3D('',#32600,#16413,#16414);
#14820=AXIS2_PLACEMENT_3D('',#32687,#16416,#16417);
#14821=AXIS2_PLACEMENT_3D('',#32762,#16419,#16420);
#14822=AXIS2_PLACEMENT_3D('',#32810,#16422,#16423);
#14823=AXIS2_PLACEMENT_3D('',#32867,#16425,#16426);
#14824=AXIS2_PLACEMENT_3D('',#32954,#16428,#16429);
#14825=AXIS2_PLACEMENT_3D('',#33041,#16431,#16432);
#14826=AXIS2_PLACEMENT_3D('',#33128,#16434,#16435);
#14827=AXIS2_PLACEMENT_3D('',#33215,#16437,#16438);
#14828=AXIS2_PLACEMENT_3D('',#33302,#16440,#16441);
#14829=AXIS2_PLACEMENT_3D('',#33392,#16443,#16444);
#14830=AXIS2_PLACEMENT_3D('',#33479,#16446,#16447);
#14831=AXIS2_PLACEMENT_3D('',#33566,#16449,#16450);
#14832=AXIS2_PLACEMENT_3D('',#33653,#16452,#16453);
#14833=AXIS2_PLACEMENT_3D('',#33740,#16455,#16456);
#14834=AXIS2_PLACEMENT_3D('',#33830,#16458,#16459);
#14835=AXIS2_PLACEMENT_3D('',#33917,#16461,#16462);
#14836=AXIS2_PLACEMENT_3D('',#34004,#16464,#16465);
#14837=AXIS2_PLACEMENT_3D('',#34091,#16467,#16468);
#14838=AXIS2_PLACEMENT_3D('',#34178,#16470,#16471);
#14839=AXIS2_PLACEMENT_3D('',#34268,#16473,#16474);
#14840=AXIS2_PLACEMENT_3D('',#34355,#16476,#16477);
#14841=AXIS2_PLACEMENT_3D('',#34386,#16479,#16480);
#14842=AXIS2_PLACEMENT_3D('',#34424,#16481,#16482);
#14843=AXIS2_PLACEMENT_3D('',#34442,#16484,#16485);
#14844=AXIS2_PLACEMENT_3D('',#34457,#16486,#16487);
#14845=AXIS2_PLACEMENT_3D('',#34494,#16489,#16490);
#14846=AXIS2_PLACEMENT_3D('',#34532,#16492,#16493);
#14847=AXIS2_PLACEMENT_3D('',#34568,#16495,#16496);
#14848=AXIS2_PLACEMENT_3D('',#34606,#16498,#16499);
#14849=AXIS2_PLACEMENT_3D('',#34643,#16501,#16502);
#14850=AXIS2_PLACEMENT_3D('',#34680,#16504,#16505);
#14851=AXIS2_PLACEMENT_3D('',#34718,#16507,#16508);
#14852=AXIS2_PLACEMENT_3D('',#34754,#16510,#16511);
#14853=AXIS2_PLACEMENT_3D('',#34792,#16513,#16514);
#14854=AXIS2_PLACEMENT_3D('',#34829,#16516,#16517);
#14855=AXIS2_PLACEMENT_3D('',#34866,#16519,#16520);
#14856=AXIS2_PLACEMENT_3D('',#34904,#16522,#16523);
#14857=AXIS2_PLACEMENT_3D('',#34940,#16525,#16526);
#14858=AXIS2_PLACEMENT_3D('',#34978,#16528,#16529);
#14859=AXIS2_PLACEMENT_3D('',#35015,#16531,#16532);
#14860=AXIS2_PLACEMENT_3D('',#35052,#16534,#16535);
#14861=AXIS2_PLACEMENT_3D('',#35090,#16537,#16538);
#14862=AXIS2_PLACEMENT_3D('',#35126,#16540,#16541);
#14863=AXIS2_PLACEMENT_3D('',#35153,#16543,#16544);
#14864=AXIS2_PLACEMENT_3D('',#35177,#16546,#16547);
#14865=AXIS2_PLACEMENT_3D('',#35210,#16549,#16550);
#14866=AXIS2_PLACEMENT_3D('',#35248,#16552,#16553);
#14867=AXIS2_PLACEMENT_3D('',#35284,#16555,#16556);
#14868=AXIS2_PLACEMENT_3D('',#35322,#16558,#16559);
#14869=AXIS2_PLACEMENT_3D('',#35358,#16561,#16562);
#14870=AXIS2_PLACEMENT_3D('',#35396,#16564,#16565);
#14871=AXIS2_PLACEMENT_3D('',#35434,#16567,#16568);
#14872=AXIS2_PLACEMENT_3D('',#35470,#16570,#16571);
#14873=AXIS2_PLACEMENT_3D('',#35508,#16573,#16574);
#14874=AXIS2_PLACEMENT_3D('',#35544,#16576,#16577);
#14875=AXIS2_PLACEMENT_3D('',#35582,#16579,#16580);
#14876=AXIS2_PLACEMENT_3D('',#35620,#16582,#16583);
#14877=AXIS2_PLACEMENT_3D('',#35656,#16585,#16586);
#14878=AXIS2_PLACEMENT_3D('',#35694,#16588,#16589);
#14879=AXIS2_PLACEMENT_3D('',#35730,#16591,#16592);
#14880=AXIS2_PLACEMENT_3D('',#35768,#16594,#16595);
#14881=AXIS2_PLACEMENT_3D('',#35806,#16597,#16598);
#14882=AXIS2_PLACEMENT_3D('',#35842,#16600,#16601);
#14883=AXIS2_PLACEMENT_3D('',#35854,#16603,#16604);
#14884=AXIS2_PLACEMENT_3D('',#35862,#16605,#16606);
#14885=AXIS2_PLACEMENT_3D('',#36072,#16607,#16608);
#14886=AXIS2_PLACEMENT_3D('',#40378,#16609,#16610);
#14887=AXIS2_PLACEMENT_3D('',#40379,#16611,#16612);
#14888=AXIS2_PLACEMENT_3D('',#40381,#16613,#16614);
#14889=AXIS2_PLACEMENT_3D('',#40382,#16615,#16616);
#14890=AXIS2_PLACEMENT_3D('',#40589,#16617,#16618);
#14891=AXIS2_PLACEMENT_3D('',#43503,#16619,#16620);
#14892=AXIS2_PLACEMENT_3D('',#43504,#16621,#16622);
#14893=AXIS2_PLACEMENT_3D('',#43506,#16623,#16624);
#14894=AXIS2_PLACEMENT_3D('',#43507,#16625,#16626);
#14895=AXIS2_PLACEMENT_3D('',#43510,#16627,#16628);
#14896=AXIS2_PLACEMENT_3D('',#43514,#16630,#16631);
#14897=AXIS2_PLACEMENT_3D('',#43516,#16633,#16634);
#14898=AXIS2_PLACEMENT_3D('',#43522,#16638,#16639);
#14899=AXIS2_PLACEMENT_3D('',#43526,#16641,#16642);
#14900=AXIS2_PLACEMENT_3D('',#43530,#16644,#16645);
#14901=AXIS2_PLACEMENT_3D('',#43534,#16647,#16648);
#14902=AXIS2_PLACEMENT_3D('',#43538,#16650,#16651);
#14903=AXIS2_PLACEMENT_3D('',#43542,#16653,#16654);
#14904=AXIS2_PLACEMENT_3D('',#43546,#16656,#16657);
#14905=AXIS2_PLACEMENT_3D('',#43550,#16659,#16660);
#14906=AXIS2_PLACEMENT_3D('',#43554,#16662,#16663);
#14907=AXIS2_PLACEMENT_3D('',#43558,#16665,#16666);
#14908=AXIS2_PLACEMENT_3D('',#43562,#16668,#16669);
#14909=AXIS2_PLACEMENT_3D('',#43566,#16671,#16672);
#14910=AXIS2_PLACEMENT_3D('',#43570,#16674,#16675);
#14911=AXIS2_PLACEMENT_3D('',#43574,#16677,#16678);
#14912=AXIS2_PLACEMENT_3D('',#43578,#16680,#16681);
#14913=AXIS2_PLACEMENT_3D('',#43582,#16683,#16684);
#14914=AXIS2_PLACEMENT_3D('',#43586,#16686,#16687);
#14915=AXIS2_PLACEMENT_3D('',#43590,#16689,#16690);
#14916=AXIS2_PLACEMENT_3D('',#43594,#16692,#16693);
#14917=AXIS2_PLACEMENT_3D('',#43598,#16695,#16696);
#14918=AXIS2_PLACEMENT_3D('',#43602,#16698,#16699);
#14919=AXIS2_PLACEMENT_3D('',#43606,#16701,#16702);
#14920=AXIS2_PLACEMENT_3D('',#43610,#16704,#16705);
#14921=AXIS2_PLACEMENT_3D('',#43614,#16707,#16708);
#14922=AXIS2_PLACEMENT_3D('',#43618,#16710,#16711);
#14923=AXIS2_PLACEMENT_3D('',#43622,#16713,#16714);
#14924=AXIS2_PLACEMENT_3D('',#43626,#16716,#16717);
#14925=AXIS2_PLACEMENT_3D('',#43630,#16719,#16720);
#14926=AXIS2_PLACEMENT_3D('',#43634,#16722,#16723);
#14927=AXIS2_PLACEMENT_3D('',#43638,#16725,#16726);
#14928=AXIS2_PLACEMENT_3D('',#43642,#16728,#16729);
#14929=AXIS2_PLACEMENT_3D('',#43646,#16731,#16732);
#14930=AXIS2_PLACEMENT_3D('',#43650,#16734,#16735);
#14931=AXIS2_PLACEMENT_3D('',#43654,#16737,#16738);
#14932=AXIS2_PLACEMENT_3D('',#43658,#16740,#16741);
#14933=AXIS2_PLACEMENT_3D('',#43661,#16743,#16744);
#14934=AXIS2_PLACEMENT_3D('',#43663,#16745,#16746);
#14935=AXIS2_PLACEMENT_3D('',#43665,#16747,#16748);
#14936=AXIS2_PLACEMENT_3D('',#43667,#16749,#16750);
#14937=AXIS2_PLACEMENT_3D('',#43669,#16751,#16752);
#14938=AXIS2_PLACEMENT_3D('',#43670,#16753,#16754);
#14939=AXIS2_PLACEMENT_3D('',#43673,#16755,#16756);
#14940=AXIS2_PLACEMENT_3D('',#43676,#16759,#16760);
#14941=AXIS2_PLACEMENT_3D('',#43680,#16763,#16764);
#14942=AXIS2_PLACEMENT_3D('',#43682,#16765,#16766);
#14943=AXIS2_PLACEMENT_3D('',#43684,#16768,#16769);
#14944=AXIS2_PLACEMENT_3D('',#43688,#16772,#16773);
#14945=AXIS2_PLACEMENT_3D('',#43690,#16774,#16775);
#14946=AXIS2_PLACEMENT_3D('',#43692,#16777,#16778);
#14947=AXIS2_PLACEMENT_3D('',#43696,#16781,#16782);
#14948=AXIS2_PLACEMENT_3D('',#43698,#16783,#16784);
#14949=AXIS2_PLACEMENT_3D('',#43700,#16786,#16787);
#14950=AXIS2_PLACEMENT_3D('',#43704,#16790,#16791);
#14951=AXIS2_PLACEMENT_3D('',#43706,#16792,#16793);
#14952=AXIS2_PLACEMENT_3D('',#43708,#16795,#16796);
#14953=AXIS2_PLACEMENT_3D('',#43712,#16798,#16799);
#14954=AXIS2_PLACEMENT_3D('',#43714,#16801,#16802);
#14955=AXIS2_PLACEMENT_3D('',#43718,#16805,#16806);
#14956=AXIS2_PLACEMENT_3D('',#43720,#16807,#16808);
#14957=AXIS2_PLACEMENT_3D('',#43722,#16810,#16811);
#14958=AXIS2_PLACEMENT_3D('',#43726,#16813,#16814);
#14959=AXIS2_PLACEMENT_3D('',#43728,#16816,#16817);
#14960=AXIS2_PLACEMENT_3D('',#43732,#16820,#16821);
#14961=AXIS2_PLACEMENT_3D('',#43734,#16822,#16823);
#14962=AXIS2_PLACEMENT_3D('',#43736,#16825,#16826);
#14963=AXIS2_PLACEMENT_3D('',#43739,#16827,#16828);
#14964=AXIS2_PLACEMENT_3D('',#43742,#16831,#16832);
#14965=AXIS2_PLACEMENT_3D('',#43746,#16835,#16836);
#14966=AXIS2_PLACEMENT_3D('',#43748,#16837,#16838);
#14967=AXIS2_PLACEMENT_3D('',#43750,#16840,#16841);
#14968=AXIS2_PLACEMENT_3D('',#43754,#16844,#16845);
#14969=AXIS2_PLACEMENT_3D('',#43756,#16846,#16847);
#14970=AXIS2_PLACEMENT_3D('',#43758,#16849,#16850);
#14971=AXIS2_PLACEMENT_3D('',#43762,#16853,#16854);
#14972=AXIS2_PLACEMENT_3D('',#43764,#16855,#16856);
#14973=AXIS2_PLACEMENT_3D('',#43766,#16858,#16859);
#14974=AXIS2_PLACEMENT_3D('',#43770,#16862,#16863);
#14975=AXIS2_PLACEMENT_3D('',#43772,#16864,#16865);
#14976=AXIS2_PLACEMENT_3D('',#43774,#16867,#16868);
#14977=AXIS2_PLACEMENT_3D('',#43778,#16870,#16871);
#14978=AXIS2_PLACEMENT_3D('',#43780,#16873,#16874);
#14979=AXIS2_PLACEMENT_3D('',#43784,#16877,#16878);
#14980=AXIS2_PLACEMENT_3D('',#43786,#16879,#16880);
#14981=AXIS2_PLACEMENT_3D('',#43788,#16882,#16883);
#14982=AXIS2_PLACEMENT_3D('',#43792,#16885,#16886);
#14983=AXIS2_PLACEMENT_3D('',#43794,#16888,#16889);
#14984=AXIS2_PLACEMENT_3D('',#43798,#16892,#16893);
#14985=AXIS2_PLACEMENT_3D('',#43800,#16894,#16895);
#14986=AXIS2_PLACEMENT_3D('',#43802,#16897,#16898);
#14987=AXIS2_PLACEMENT_3D('',#43805,#16899,#16900);
#14988=AXIS2_PLACEMENT_3D('',#43808,#16903,#16904);
#14989=AXIS2_PLACEMENT_3D('',#43812,#16907,#16908);
#14990=AXIS2_PLACEMENT_3D('',#43814,#16909,#16910);
#14991=AXIS2_PLACEMENT_3D('',#43816,#16912,#16913);
#14992=AXIS2_PLACEMENT_3D('',#43820,#16916,#16917);
#14993=AXIS2_PLACEMENT_3D('',#43822,#16918,#16919);
#14994=AXIS2_PLACEMENT_3D('',#43824,#16921,#16922);
#14995=AXIS2_PLACEMENT_3D('',#43828,#16925,#16926);
#14996=AXIS2_PLACEMENT_3D('',#43830,#16927,#16928);
#14997=AXIS2_PLACEMENT_3D('',#43832,#16930,#16931);
#14998=AXIS2_PLACEMENT_3D('',#43836,#16934,#16935);
#14999=AXIS2_PLACEMENT_3D('',#43838,#16936,#16937);
#15000=AXIS2_PLACEMENT_3D('',#43840,#16939,#16940);
#15001=AXIS2_PLACEMENT_3D('',#43844,#16942,#16943);
#15002=AXIS2_PLACEMENT_3D('',#43846,#16945,#16946);
#15003=AXIS2_PLACEMENT_3D('',#43850,#16949,#16950);
#15004=AXIS2_PLACEMENT_3D('',#43852,#16951,#16952);
#15005=AXIS2_PLACEMENT_3D('',#43854,#16954,#16955);
#15006=AXIS2_PLACEMENT_3D('',#43858,#16957,#16958);
#15007=AXIS2_PLACEMENT_3D('',#43860,#16960,#16961);
#15008=AXIS2_PLACEMENT_3D('',#43864,#16964,#16965);
#15009=AXIS2_PLACEMENT_3D('',#43866,#16966,#16967);
#15010=AXIS2_PLACEMENT_3D('',#43868,#16969,#16970);
#15011=AXIS2_PLACEMENT_3D('',#43871,#16971,#16972);
#15012=AXIS2_PLACEMENT_3D('',#43874,#16975,#16976);
#15013=AXIS2_PLACEMENT_3D('',#43878,#16979,#16980);
#15014=AXIS2_PLACEMENT_3D('',#43880,#16981,#16982);
#15015=AXIS2_PLACEMENT_3D('',#43882,#16984,#16985);
#15016=AXIS2_PLACEMENT_3D('',#43886,#16988,#16989);
#15017=AXIS2_PLACEMENT_3D('',#43888,#16990,#16991);
#15018=AXIS2_PLACEMENT_3D('',#43890,#16993,#16994);
#15019=AXIS2_PLACEMENT_3D('',#43894,#16997,#16998);
#15020=AXIS2_PLACEMENT_3D('',#43896,#16999,#17000);
#15021=AXIS2_PLACEMENT_3D('',#43898,#17002,#17003);
#15022=AXIS2_PLACEMENT_3D('',#43902,#17006,#17007);
#15023=AXIS2_PLACEMENT_3D('',#43904,#17008,#17009);
#15024=AXIS2_PLACEMENT_3D('',#43906,#17011,#17012);
#15025=AXIS2_PLACEMENT_3D('',#43910,#17014,#17015);
#15026=AXIS2_PLACEMENT_3D('',#43912,#17017,#17018);
#15027=AXIS2_PLACEMENT_3D('',#43916,#17021,#17022);
#15028=AXIS2_PLACEMENT_3D('',#43918,#17023,#17024);
#15029=AXIS2_PLACEMENT_3D('',#43920,#17026,#17027);
#15030=AXIS2_PLACEMENT_3D('',#43923,#17029,#17030);
#15031=AXIS2_PLACEMENT_3D('',#43924,#17031,#17032);
#15032=AXIS2_PLACEMENT_3D('',#43927,#17034,#17035);
#15033=AXIS2_PLACEMENT_3D('',#43928,#17036,#17037);
#15034=AXIS2_PLACEMENT_3D('',#43931,#17039,#17040);
#15035=AXIS2_PLACEMENT_3D('',#43932,#17041,#17042);
#15036=AXIS2_PLACEMENT_3D('',#43934,#17044,#17045);
#15037=AXIS2_PLACEMENT_3D('',#43937,#17047,#17048);
#15038=AXIS2_PLACEMENT_3D('',#43938,#17049,#17050);
#15039=AXIS2_PLACEMENT_3D('',#43941,#17052,#17053);
#15040=AXIS2_PLACEMENT_3D('',#43942,#17054,#17055);
#15041=AXIS2_PLACEMENT_3D('',#43944,#17057,#17058);
#15042=AXIS2_PLACEMENT_3D('',#43946,#17060,#17061);
#15043=AXIS2_PLACEMENT_3D('',#43948,#17063,#17064);
#15044=AXIS2_PLACEMENT_3D('',#43950,#17066,#17067);
#15045=AXIS2_PLACEMENT_3D('',#43952,#17069,#17070);
#15046=AXIS2_PLACEMENT_3D('',#43954,#17072,#17073);
#15047=AXIS2_PLACEMENT_3D('',#43956,#17075,#17076);
#15048=AXIS2_PLACEMENT_3D('',#43958,#17078,#17079);
#15049=AXIS2_PLACEMENT_3D('',#43960,#17081,#17082);
#15050=AXIS2_PLACEMENT_3D('',#43962,#17084,#17085);
#15051=AXIS2_PLACEMENT_3D('',#43964,#17087,#17088);
#15052=AXIS2_PLACEMENT_3D('',#43966,#17090,#17091);
#15053=AXIS2_PLACEMENT_3D('',#43967,#17092,#17093);
#15054=AXIS2_PLACEMENT_3D('',#43968,#17094,#17095);
#15055=AXIS2_PLACEMENT_3D('',#43970,#17096,#17097);
#15056=AXIS2_PLACEMENT_3D('',#43972,#17098,#17099);
#15057=AXIS2_PLACEMENT_3D('',#43973,#17100,#17101);
#15058=AXIS2_PLACEMENT_3D('',#43975,#17102,#17103);
#15059=AXIS2_PLACEMENT_3D('',#43977,#17105,#17106);
#15060=AXIS2_PLACEMENT_3D('',#43980,#17108,#17109);
#15061=AXIS2_PLACEMENT_3D('',#43981,#17110,#17111);
#15062=AXIS2_PLACEMENT_3D('',#43983,#17112,#17113);
#15063=AXIS2_PLACEMENT_3D('',#43986,#17115,#17116);
#15064=AXIS2_PLACEMENT_3D('',#43987,#17117,#17118);
#15065=AXIS2_PLACEMENT_3D('',#43989,#17119,#17120);
#15066=AXIS2_PLACEMENT_3D('',#43992,#17122,#17123);
#15067=AXIS2_PLACEMENT_3D('',#43993,#17124,#17125);
#15068=AXIS2_PLACEMENT_3D('',#43995,#17126,#17127);
#15069=AXIS2_PLACEMENT_3D('',#43998,#17129,#17130);
#15070=AXIS2_PLACEMENT_3D('',#43999,#17131,#17132);
#15071=AXIS2_PLACEMENT_3D('',#44001,#17133,#17134);
#15072=AXIS2_PLACEMENT_3D('',#44004,#17136,#17137);
#15073=AXIS2_PLACEMENT_3D('',#44005,#17138,#17139);
#15074=AXIS2_PLACEMENT_3D('',#44014,#17144,#17145);
#15075=AXIS2_PLACEMENT_3D('',#44020,#17149,#17150);
#15076=AXIS2_PLACEMENT_3D('',#44026,#17154,#17155);
#15077=AXIS2_PLACEMENT_3D('',#44029,#17158,#17159);
#15078=AXIS2_PLACEMENT_3D('',#44030,#17160,#17161);
#15079=AXIS2_PLACEMENT_3D('',#44031,#17162,#17163);
#15080=AXIS2_PLACEMENT_3D('',#44032,#17164,#17165);
#15081=AXIS2_PLACEMENT_3D('',#44048,#17167,#17168);
#15082=AXIS2_PLACEMENT_3D('',#44059,#17169,#17170);
#15083=AXIS2_PLACEMENT_3D('',#44107,#17172,#17173);
#15084=AXIS2_PLACEMENT_3D('',#44155,#17175,#17176);
#15085=AXIS2_PLACEMENT_3D('',#44209,#17178,#17179);
#15086=AXIS2_PLACEMENT_3D('',#44257,#17181,#17182);
#15087=AXIS2_PLACEMENT_3D('',#44305,#17184,#17185);
#15088=AXIS2_PLACEMENT_3D('',#44359,#17187,#17188);
#15089=AXIS2_PLACEMENT_3D('',#44407,#17190,#17191);
#15090=AXIS2_PLACEMENT_3D('',#44455,#17193,#17194);
#15091=AXIS2_PLACEMENT_3D('',#44503,#17196,#17197);
#15092=AXIS2_PLACEMENT_3D('',#44557,#17199,#17200);
#15093=AXIS2_PLACEMENT_3D('',#44605,#17202,#17203);
#15094=AXIS2_PLACEMENT_3D('',#44653,#17205,#17206);
#15095=AXIS2_PLACEMENT_3D('',#44707,#17208,#17209);
#15096=AXIS2_PLACEMENT_3D('',#44755,#17211,#17212);
#15097=AXIS2_PLACEMENT_3D('',#44803,#17214,#17215);
#15098=AXIS2_PLACEMENT_3D('',#44857,#17217,#17218);
#15099=AXIS2_PLACEMENT_3D('',#44905,#17220,#17221);
#15100=AXIS2_PLACEMENT_3D('',#44953,#17223,#17224);
#15101=AXIS2_PLACEMENT_3D('',#44970,#17226,#17227);
#15102=AXIS2_PLACEMENT_3D('',#44980,#17228,#17229);
#15103=AXIS2_PLACEMENT_3D('',#45005,#17231,#17232);
#15104=AXIS2_PLACEMENT_3D('',#45029,#17234,#17235);
#15105=AXIS2_PLACEMENT_3D('',#45054,#17237,#17238);
#15106=AXIS2_PLACEMENT_3D('',#45079,#17240,#17241);
#15107=AXIS2_PLACEMENT_3D('',#45103,#17243,#17244);
#15108=AXIS2_PLACEMENT_3D('',#45128,#17246,#17247);
#15109=AXIS2_PLACEMENT_3D('',#45153,#17249,#17250);
#15110=AXIS2_PLACEMENT_3D('',#45177,#17252,#17253);
#15111=AXIS2_PLACEMENT_3D('',#45202,#17255,#17256);
#15112=AXIS2_PLACEMENT_3D('',#45227,#17258,#17259);
#15113=AXIS2_PLACEMENT_3D('',#45251,#17261,#17262);
#15114=AXIS2_PLACEMENT_3D('',#45275,#17264,#17265);
#15115=AXIS2_PLACEMENT_3D('',#45300,#17267,#17268);
#15116=AXIS2_PLACEMENT_3D('',#45325,#17270,#17271);
#15117=AXIS2_PLACEMENT_3D('',#45349,#17273,#17274);
#15118=AXIS2_PLACEMENT_3D('',#45374,#17276,#17277);
#15119=AXIS2_PLACEMENT_3D('',#45399,#17279,#17280);
#15120=AXIS2_PLACEMENT_3D('',#45423,#17282,#17283);
#15121=AXIS2_PLACEMENT_3D('',#45744,#17284,#17285);
#15122=AXIS2_PLACEMENT_3D('',#45784,#17287,#17288);
#15123=AXIS2_PLACEMENT_3D('',#46433,#17289,#17290);
#15124=AXIS2_PLACEMENT_3D('',#46444,#17291,#17292);
#15125=AXIS2_PLACEMENT_3D('',#47097,#17293,#17294);
#15126=AXIS2_PLACEMENT_3D('',#47098,#17295,#17296);
#15127=AXIS2_PLACEMENT_3D('',#47107,#17301,#17302);
#15128=AXIS2_PLACEMENT_3D('',#47113,#17306,#17307);
#15129=AXIS2_PLACEMENT_3D('',#47119,#17311,#17312);
#15130=AXIS2_PLACEMENT_3D('',#47125,#17316,#17317);
#15131=AXIS2_PLACEMENT_3D('',#47131,#17321,#17322);
#15132=AXIS2_PLACEMENT_3D('',#47134,#17325,#17326);
#15133=AXIS2_PLACEMENT_3D('',#47135,#17327,#17328);
#15134=AXIS2_PLACEMENT_3D('',#47137,#17329,#17330);
#15135=AXIS2_PLACEMENT_3D('',#47138,#17331,#17332);
#15136=AXIS2_PLACEMENT_3D('',#47141,#17334,#17335);
#15137=AXIS2_PLACEMENT_3D('',#47142,#17336,#17337);
#15138=AXIS2_PLACEMENT_3D('',#47143,#17338,#17339);
#15139=AXIS2_PLACEMENT_3D('',#47144,#17340,#17341);
#15140=AXIS2_PLACEMENT_3D('',#47145,#17342,#17343);
#15141=AXIS2_PLACEMENT_3D('',#47147,#17344,#17345);
#15142=AXIS2_PLACEMENT_3D('',#47150,#17347,#17348);
#15143=AXIS2_PLACEMENT_3D('',#47151,#17349,#17350);
#15144=AXIS2_PLACEMENT_3D('',#47152,#17351,#17352);
#15145=AXIS2_PLACEMENT_3D('',#47153,#17353,#17354);
#15146=AXIS2_PLACEMENT_3D('',#47154,#17355,#17356);
#15147=AXIS2_PLACEMENT_3D('',#47164,#17358,#17359);
#15148=AXIS2_PLACEMENT_3D('',#47167,#17361,#17362);
#15149=AXIS2_PLACEMENT_3D('',#47169,#17363,#17364);
#15150=AXIS2_PLACEMENT_3D('',#47180,#17365,#17366);
#15151=AXIS2_PLACEMENT_3D('',#47231,#17368,#17369);
#15152=AXIS2_PLACEMENT_3D('',#47282,#17371,#17372);
#15153=AXIS2_PLACEMENT_3D('',#47330,#17374,#17375);
#15154=AXIS2_PLACEMENT_3D('',#47381,#17377,#17378);
#15155=AXIS2_PLACEMENT_3D('',#47432,#17380,#17381);
#15156=AXIS2_PLACEMENT_3D('',#47480,#17383,#17384);
#15157=AXIS2_PLACEMENT_3D('',#47499,#17386,#17387);
#15158=AXIS2_PLACEMENT_3D('',#47519,#17388,#17389);
#15159=AXIS2_PLACEMENT_3D('',#47533,#17391,#17392);
#15160=AXIS2_PLACEMENT_3D('',#47543,#17393,#17394);
#15161=AXIS2_PLACEMENT_3D('',#47567,#17396,#17397);
#15162=AXIS2_PLACEMENT_3D('',#47592,#17399,#17400);
#15163=AXIS2_PLACEMENT_3D('',#47617,#17402,#17403);
#15164=AXIS2_PLACEMENT_3D('',#47641,#17405,#17406);
#15165=AXIS2_PLACEMENT_3D('',#47666,#17408,#17409);
#15166=AXIS2_PLACEMENT_3D('',#47691,#17411,#17412);
#15167=AXIS2_PLACEMENT_3D('',#47702,#17414,#17415);
#15168=AXIS2_PLACEMENT_3D('',#47708,#17416,#17417);
#15169=AXIS2_PLACEMENT_3D('',#47718,#17419,#17420);
#15170=AXIS2_PLACEMENT_3D('',#47721,#17422,#17423);
#15171=AXIS2_PLACEMENT_3D('',#47723,#17424,#17425);
#15172=AXIS2_PLACEMENT_3D('',#47734,#17426,#17427);
#15173=AXIS2_PLACEMENT_3D('',#47785,#17429,#17430);
#15174=AXIS2_PLACEMENT_3D('',#47836,#17432,#17433);
#15175=AXIS2_PLACEMENT_3D('',#47884,#17435,#17436);
#15176=AXIS2_PLACEMENT_3D('',#47935,#17438,#17439);
#15177=AXIS2_PLACEMENT_3D('',#47986,#17441,#17442);
#15178=AXIS2_PLACEMENT_3D('',#48034,#17444,#17445);
#15179=AXIS2_PLACEMENT_3D('',#48053,#17447,#17448);
#15180=AXIS2_PLACEMENT_3D('',#48073,#17449,#17450);
#15181=AXIS2_PLACEMENT_3D('',#48087,#17452,#17453);
#15182=AXIS2_PLACEMENT_3D('',#48097,#17454,#17455);
#15183=AXIS2_PLACEMENT_3D('',#48121,#17457,#17458);
#15184=AXIS2_PLACEMENT_3D('',#48146,#17460,#17461);
#15185=AXIS2_PLACEMENT_3D('',#48171,#17463,#17464);
#15186=AXIS2_PLACEMENT_3D('',#48195,#17466,#17467);
#15187=AXIS2_PLACEMENT_3D('',#48220,#17469,#17470);
#15188=AXIS2_PLACEMENT_3D('',#48245,#17472,#17473);
#15189=AXIS2_PLACEMENT_3D('',#48256,#17475,#17476);
#15190=AXIS2_PLACEMENT_3D('',#48262,#17477,#17478);
#15191=AXIS2_PLACEMENT_3D('',#48272,#17480,#17481);
#15192=AXIS2_PLACEMENT_3D('',#48275,#17483,#17484);
#15193=AXIS2_PLACEMENT_3D('',#48277,#17485,#17486);
#15194=AXIS2_PLACEMENT_3D('',#48288,#17487,#17488);
#15195=AXIS2_PLACEMENT_3D('',#48339,#17490,#17491);
#15196=AXIS2_PLACEMENT_3D('',#48390,#17493,#17494);
#15197=AXIS2_PLACEMENT_3D('',#48438,#17496,#17497);
#15198=AXIS2_PLACEMENT_3D('',#48489,#17499,#17500);
#15199=AXIS2_PLACEMENT_3D('',#48540,#17502,#17503);
#15200=AXIS2_PLACEMENT_3D('',#48588,#17505,#17506);
#15201=AXIS2_PLACEMENT_3D('',#48607,#17508,#17509);
#15202=AXIS2_PLACEMENT_3D('',#48627,#17510,#17511);
#15203=AXIS2_PLACEMENT_3D('',#48641,#17513,#17514);
#15204=AXIS2_PLACEMENT_3D('',#48651,#17515,#17516);
#15205=AXIS2_PLACEMENT_3D('',#48675,#17518,#17519);
#15206=AXIS2_PLACEMENT_3D('',#48700,#17521,#17522);
#15207=AXIS2_PLACEMENT_3D('',#48725,#17524,#17525);
#15208=AXIS2_PLACEMENT_3D('',#48749,#17527,#17528);
#15209=AXIS2_PLACEMENT_3D('',#48774,#17530,#17531);
#15210=AXIS2_PLACEMENT_3D('',#48799,#17533,#17534);
#15211=AXIS2_PLACEMENT_3D('',#48810,#17536,#17537);
#15212=AXIS2_PLACEMENT_3D('',#48816,#17538,#17539);
#15213=AXIS2_PLACEMENT_3D('',#49008,#17540,#17541);
#15214=AXIS2_PLACEMENT_3D('',#49707,#17542,#17543);
#15215=AXIS2_PLACEMENT_3D('',#49708,#17544,#17545);
#15216=AXIS2_PLACEMENT_3D('',#49900,#17546,#17547);
#15217=AXIS2_PLACEMENT_3D('',#50599,#17548,#17549);
#15218=AXIS2_PLACEMENT_3D('',#50600,#17550,#17551);
#15219=AXIS2_PLACEMENT_3D('',#50792,#17552,#17553);
#15220=AXIS2_PLACEMENT_3D('',#51491,#17554,#17555);
#15221=AXIS2_PLACEMENT_3D('',#51492,#17556,#17557);
#15222=AXIS2_PLACEMENT_3D('',#51493,#17558,#17559);
#15223=AXIS2_PLACEMENT_3D('',#51494,#17560,#17561);
#15224=AXIS2_PLACEMENT_3D('',#51495,#17562,#17563);
#15225=AXIS2_PLACEMENT_3D('',#51497,#17564,#17565);
#15226=AXIS2_PLACEMENT_3D('',#51499,#17566,#17567);
#15227=AXIS2_PLACEMENT_3D('',#51500,#17568,#17569);
#15228=AXIS2_PLACEMENT_3D('',#51502,#17570,#17571);
#15229=AXIS2_PLACEMENT_3D('',#51505,#17573,#17574);
#15230=AXIS2_PLACEMENT_3D('',#51506,#17575,#17576);
#15231=AXIS2_PLACEMENT_3D('',#51507,#17577,#17578);
#15232=AXIS2_PLACEMENT_3D('',#51508,#17579,#17580);
#15233=AXIS2_PLACEMENT_3D('',#51509,#17581,#17582);
#15234=AXIS2_PLACEMENT_3D('',#51511,#17583,#17584);
#15235=AXIS2_PLACEMENT_3D('',#51514,#17586,#17587);
#15236=AXIS2_PLACEMENT_3D('',#51515,#17588,#17589);
#15237=AXIS2_PLACEMENT_3D('',#51517,#17590,#17591);
#15238=AXIS2_PLACEMENT_3D('',#51520,#17593,#17594);
#15239=AXIS2_PLACEMENT_3D('',#51521,#17595,#17596);
#15240=AXIS2_PLACEMENT_3D('',#51523,#17597,#17598);
#15241=AXIS2_PLACEMENT_3D('',#51526,#17600,#17601);
#15242=AXIS2_PLACEMENT_3D('',#51527,#17602,#17603);
#15243=AXIS2_PLACEMENT_3D('',#51529,#17604,#17605);
#15244=AXIS2_PLACEMENT_3D('',#51531,#17606,#17607);
#15245=AXIS2_PLACEMENT_3D('',#51532,#17608,#17609);
#15246=AXIS2_PLACEMENT_3D('',#51533,#17610,#17611);
#15247=AXIS2_PLACEMENT_3D('',#51535,#17612,#17613);
#15248=AXIS2_PLACEMENT_3D('',#51537,#17615,#17616);
#15249=AXIS2_PLACEMENT_3D('',#51539,#17617,#17618);
#15250=AXIS2_PLACEMENT_3D('',#51542,#17620,#17621);
#15251=AXIS2_PLACEMENT_3D('',#51543,#17622,#17623);
#15252=AXIS2_PLACEMENT_3D('',#51544,#17624,#17625);
#15253=AXIS2_PLACEMENT_3D('',#51545,#17626,#17627);
#15254=AXIS2_PLACEMENT_3D('',#51546,#17628,#17629);
#15255=AXIS2_PLACEMENT_3D('',#51562,#17631,#17632);
#15256=AXIS2_PLACEMENT_3D('',#51573,#17633,#17634);
#15257=AXIS2_PLACEMENT_3D('',#51621,#17636,#17637);
#15258=AXIS2_PLACEMENT_3D('',#51669,#17639,#17640);
#15259=AXIS2_PLACEMENT_3D('',#51720,#17642,#17643);
#15260=AXIS2_PLACEMENT_3D('',#51768,#17645,#17646);
#15261=AXIS2_PLACEMENT_3D('',#51816,#17648,#17649);
#15262=AXIS2_PLACEMENT_3D('',#51864,#17651,#17652);
#15263=AXIS2_PLACEMENT_3D('',#51918,#17654,#17655);
#15264=AXIS2_PLACEMENT_3D('',#51966,#17657,#17658);
#15265=AXIS2_PLACEMENT_3D('',#52014,#17660,#17661);
#15266=AXIS2_PLACEMENT_3D('',#52068,#17663,#17664);
#15267=AXIS2_PLACEMENT_3D('',#52116,#17666,#17667);
#15268=AXIS2_PLACEMENT_3D('',#52164,#17669,#17670);
#15269=AXIS2_PLACEMENT_3D('',#52215,#17672,#17673);
#15270=AXIS2_PLACEMENT_3D('',#52266,#17675,#17676);
#15271=AXIS2_PLACEMENT_3D('',#52314,#17678,#17679);
#15272=AXIS2_PLACEMENT_3D('',#52362,#17681,#17682);
#15273=AXIS2_PLACEMENT_3D('',#52416,#17684,#17685);
#15274=AXIS2_PLACEMENT_3D('',#52464,#17687,#17688);
#15275=AXIS2_PLACEMENT_3D('',#52512,#17690,#17691);
#15276=AXIS2_PLACEMENT_3D('',#52566,#17693,#17694);
#15277=AXIS2_PLACEMENT_3D('',#52614,#17696,#17697);
#15278=AXIS2_PLACEMENT_3D('',#52662,#17699,#17700);
#15279=AXIS2_PLACEMENT_3D('',#52710,#17702,#17703);
#15280=AXIS2_PLACEMENT_3D('',#52764,#17705,#17706);
#15281=AXIS2_PLACEMENT_3D('',#52812,#17708,#17709);
#15282=AXIS2_PLACEMENT_3D('',#52860,#17711,#17712);
#15283=AXIS2_PLACEMENT_3D('',#52914,#17714,#17715);
#15284=AXIS2_PLACEMENT_3D('',#52962,#17717,#17718);
#15285=AXIS2_PLACEMENT_3D('',#53010,#17720,#17721);
#15286=AXIS2_PLACEMENT_3D('',#53064,#17723,#17724);
#15287=AXIS2_PLACEMENT_3D('',#53112,#17726,#17727);
#15288=AXIS2_PLACEMENT_3D('',#53160,#17729,#17730);
#15289=AXIS2_PLACEMENT_3D('',#53208,#17732,#17733);
#15290=AXIS2_PLACEMENT_3D('',#53262,#17735,#17736);
#15291=AXIS2_PLACEMENT_3D('',#53310,#17738,#17739);
#15292=AXIS2_PLACEMENT_3D('',#53358,#17741,#17742);
#15293=AXIS2_PLACEMENT_3D('',#53412,#17744,#17745);
#15294=AXIS2_PLACEMENT_3D('',#53460,#17747,#17748);
#15295=AXIS2_PLACEMENT_3D('',#53508,#17750,#17751);
#15296=AXIS2_PLACEMENT_3D('',#53562,#17753,#17754);
#15297=AXIS2_PLACEMENT_3D('',#53610,#17756,#17757);
#15298=AXIS2_PLACEMENT_3D('',#53658,#17759,#17760);
#15299=AXIS2_PLACEMENT_3D('',#53706,#17762,#17763);
#15300=AXIS2_PLACEMENT_3D('',#53760,#17765,#17766);
#15301=AXIS2_PLACEMENT_3D('',#53808,#17768,#17769);
#15302=AXIS2_PLACEMENT_3D('',#53856,#17771,#17772);
#15303=AXIS2_PLACEMENT_3D('',#53910,#17774,#17775);
#15304=AXIS2_PLACEMENT_3D('',#53958,#17777,#17778);
#15305=AXIS2_PLACEMENT_3D('',#54006,#17780,#17781);
#15306=AXIS2_PLACEMENT_3D('',#54060,#17783,#17784);
#15307=AXIS2_PLACEMENT_3D('',#54108,#17786,#17787);
#15308=AXIS2_PLACEMENT_3D('',#54156,#17789,#17790);
#15309=AXIS2_PLACEMENT_3D('',#54204,#17792,#17793);
#15310=AXIS2_PLACEMENT_3D('',#54258,#17795,#17796);
#15311=AXIS2_PLACEMENT_3D('',#54306,#17798,#17799);
#15312=AXIS2_PLACEMENT_3D('',#54354,#17801,#17802);
#15313=AXIS2_PLACEMENT_3D('',#54408,#17804,#17805);
#15314=AXIS2_PLACEMENT_3D('',#54456,#17807,#17808);
#15315=AXIS2_PLACEMENT_3D('',#54504,#17810,#17811);
#15316=AXIS2_PLACEMENT_3D('',#54516,#17813,#17814);
#15317=AXIS2_PLACEMENT_3D('',#54522,#17815,#17816);
#15318=AXIS2_PLACEMENT_3D('',#54547,#17818,#17819);
#15319=AXIS2_PLACEMENT_3D('',#54571,#17821,#17822);
#15320=AXIS2_PLACEMENT_3D('',#54596,#17824,#17825);
#15321=AXIS2_PLACEMENT_3D('',#54621,#17827,#17828);
#15322=AXIS2_PLACEMENT_3D('',#54645,#17830,#17831);
#15323=AXIS2_PLACEMENT_3D('',#54670,#17833,#17834);
#15324=AXIS2_PLACEMENT_3D('',#54695,#17836,#17837);
#15325=AXIS2_PLACEMENT_3D('',#54719,#17839,#17840);
#15326=AXIS2_PLACEMENT_3D('',#54743,#17842,#17843);
#15327=AXIS2_PLACEMENT_3D('',#54768,#17845,#17846);
#15328=AXIS2_PLACEMENT_3D('',#54793,#17848,#17849);
#15329=AXIS2_PLACEMENT_3D('',#54817,#17851,#17852);
#15330=AXIS2_PLACEMENT_3D('',#54842,#17854,#17855);
#15331=AXIS2_PLACEMENT_3D('',#54867,#17857,#17858);
#15332=AXIS2_PLACEMENT_3D('',#54891,#17860,#17861);
#15333=AXIS2_PLACEMENT_3D('',#54916,#17863,#17864);
#15334=AXIS2_PLACEMENT_3D('',#54941,#17866,#17867);
#15335=AXIS2_PLACEMENT_3D('',#54965,#17869,#17870);
#15336=AXIS2_PLACEMENT_3D('',#54989,#17872,#17873);
#15337=AXIS2_PLACEMENT_3D('',#55014,#17875,#17876);
#15338=AXIS2_PLACEMENT_3D('',#55039,#17878,#17879);
#15339=AXIS2_PLACEMENT_3D('',#55063,#17881,#17882);
#15340=AXIS2_PLACEMENT_3D('',#55088,#17884,#17885);
#15341=AXIS2_PLACEMENT_3D('',#55113,#17887,#17888);
#15342=AXIS2_PLACEMENT_3D('',#55137,#17890,#17891);
#15343=AXIS2_PLACEMENT_3D('',#55162,#17893,#17894);
#15344=AXIS2_PLACEMENT_3D('',#55187,#17896,#17897);
#15345=AXIS2_PLACEMENT_3D('',#55211,#17899,#17900);
#15346=AXIS2_PLACEMENT_3D('',#55235,#17902,#17903);
#15347=AXIS2_PLACEMENT_3D('',#55260,#17905,#17906);
#15348=AXIS2_PLACEMENT_3D('',#55285,#17908,#17909);
#15349=AXIS2_PLACEMENT_3D('',#55309,#17911,#17912);
#15350=AXIS2_PLACEMENT_3D('',#55334,#17914,#17915);
#15351=AXIS2_PLACEMENT_3D('',#55359,#17917,#17918);
#15352=AXIS2_PLACEMENT_3D('',#55383,#17920,#17921);
#15353=AXIS2_PLACEMENT_3D('',#55408,#17923,#17924);
#15354=AXIS2_PLACEMENT_3D('',#55433,#17926,#17927);
#15355=AXIS2_PLACEMENT_3D('',#55457,#17929,#17930);
#15356=AXIS2_PLACEMENT_3D('',#55481,#17932,#17933);
#15357=AXIS2_PLACEMENT_3D('',#55506,#17935,#17936);
#15358=AXIS2_PLACEMENT_3D('',#55531,#17938,#17939);
#15359=AXIS2_PLACEMENT_3D('',#55555,#17941,#17942);
#15360=AXIS2_PLACEMENT_3D('',#55580,#17944,#17945);
#15361=AXIS2_PLACEMENT_3D('',#55605,#17947,#17948);
#15362=AXIS2_PLACEMENT_3D('',#55629,#17950,#17951);
#15363=AXIS2_PLACEMENT_3D('',#55654,#17953,#17954);
#15364=AXIS2_PLACEMENT_3D('',#55678,#17956,#17957);
#15365=AXIS2_PLACEMENT_3D('',#55703,#17959,#17960);
#15366=AXIS2_PLACEMENT_3D('',#55727,#17962,#17963);
#15367=AXIS2_PLACEMENT_3D('',#55752,#17965,#17966);
#15368=AXIS2_PLACEMENT_3D('',#55777,#17968,#17969);
#15369=AXIS2_PLACEMENT_3D('',#55801,#17971,#17972);
#15370=AXIS2_PLACEMENT_3D('',#55826,#17974,#17975);
#15371=AXIS2_PLACEMENT_3D('',#55851,#17977,#17978);
#15372=AXIS2_PLACEMENT_3D('',#55875,#17980,#17981);
#15373=AXIS2_PLACEMENT_3D('',#55900,#17983,#17984);
#15374=AXIS2_PLACEMENT_3D('',#55924,#17986,#17987);
#15375=AXIS2_PLACEMENT_3D('',#55949,#17989,#17990);
#15376=AXIS2_PLACEMENT_3D('',#57758,#17992,#17993);
#15377=AXIS2_PLACEMENT_3D('',#57760,#17994,#17995);
#15378=AXIS2_PLACEMENT_3D('',#59542,#17996,#17997);
#15379=AXIS2_PLACEMENT_3D('',#59543,#17998,#17999);
#15380=AXIS2_PLACEMENT_3D('',#59544,#18000,#18001);
#15381=AXIS2_PLACEMENT_3D('',#59557,#18008,#18009);
#15382=AXIS2_PLACEMENT_3D('',#59571,#18016,#18017);
#15383=AXIS2_PLACEMENT_3D('',#59572,#18018,#18019);
#15384=AXIS2_PLACEMENT_3D('',#59575,#18022,#18023);
#15385=AXIS2_PLACEMENT_3D('',#59577,#18025,#18026);
#15386=AXIS2_PLACEMENT_3D('',#59579,#18028,#18029);
#15387=AXIS2_PLACEMENT_3D('',#59581,#18031,#18032);
#15388=AXIS2_PLACEMENT_3D('',#59583,#18034,#18035);
#15389=AXIS2_PLACEMENT_3D('',#59584,#18036,#18037);
#15390=AXIS2_PLACEMENT_3D('',#59587,#18039,#18040);
#15391=AXIS2_PLACEMENT_3D('',#59588,#18041,#18042);
#15392=AXIS2_PLACEMENT_3D('',#59589,#18043,#18044);
#15393=AXIS2_PLACEMENT_3D('',#59591,#18045,#18046);
#15394=AXIS2_PLACEMENT_3D('',#59592,#18047,#18048);
#15395=AXIS2_PLACEMENT_3D('',#59593,#18049,#18050);
#15396=AXIS2_PLACEMENT_3D('',#59606,#18052,#18053);
#15397=AXIS2_PLACEMENT_3D('',#59617,#18054,#18055);
#15398=AXIS2_PLACEMENT_3D('',#59668,#18057,#18058);
#15399=AXIS2_PLACEMENT_3D('',#59719,#18060,#18061);
#15400=AXIS2_PLACEMENT_3D('',#59767,#18063,#18064);
#15401=AXIS2_PLACEMENT_3D('',#59818,#18066,#18067);
#15402=AXIS2_PLACEMENT_3D('',#59869,#18069,#18070);
#15403=AXIS2_PLACEMENT_3D('',#59917,#18072,#18073);
#15404=AXIS2_PLACEMENT_3D('',#59939,#18075,#18076);
#15405=AXIS2_PLACEMENT_3D('',#59959,#18077,#18078);
#15406=AXIS2_PLACEMENT_3D('',#59974,#18080,#18081);
#15407=AXIS2_PLACEMENT_3D('',#59984,#18082,#18083);
#15408=AXIS2_PLACEMENT_3D('',#60008,#18085,#18086);
#15409=AXIS2_PLACEMENT_3D('',#60033,#18088,#18089);
#15410=AXIS2_PLACEMENT_3D('',#60058,#18091,#18092);
#15411=AXIS2_PLACEMENT_3D('',#60082,#18094,#18095);
#15412=AXIS2_PLACEMENT_3D('',#60107,#18097,#18098);
#15413=AXIS2_PLACEMENT_3D('',#60132,#18100,#18101);
#15414=AXIS2_PLACEMENT_3D('',#60144,#18103,#18104);
#15415=AXIS2_PLACEMENT_3D('',#60150,#18105,#18106);
#15416=AXIS2_PLACEMENT_3D('',#61104,#18107,#18108);
#15417=AXIS2_PLACEMENT_3D('',#61117,#18115,#18116);
#15418=AXIS2_PLACEMENT_3D('',#61118,#18117,#18118);
#15419=AXIS2_PLACEMENT_3D('',#61124,#18122,#18123);
#15420=AXIS2_PLACEMENT_3D('',#61128,#18126,#18127);
#15421=AXIS2_PLACEMENT_3D('',#61132,#18130,#18131);
#15422=AXIS2_PLACEMENT_3D('',#61136,#18134,#18135);
#15423=AXIS2_PLACEMENT_3D('',#61140,#18138,#18139);
#15424=AXIS2_PLACEMENT_3D('',#61142,#18141,#18142);
#15425=AXIS2_PLACEMENT_3D('',#61143,#18143,#18144);
#15426=AXIS2_PLACEMENT_3D('',#61144,#18145,#18146);
#15427=AXIS2_PLACEMENT_3D('',#61146,#18147,#18148);
#15428=AXIS2_PLACEMENT_3D('',#61149,#18150,#18151);
#15429=AXIS2_PLACEMENT_3D('',#61150,#18152,#18153);
#15430=AXIS2_PLACEMENT_3D('',#61152,#18154,#18155);
#15431=AXIS2_PLACEMENT_3D('',#61155,#18157,#18158);
#15432=AXIS2_PLACEMENT_3D('',#61156,#18159,#18160);
#15433=AXIS2_PLACEMENT_3D('',#61157,#18161,#18162);
#15434=AXIS2_PLACEMENT_3D('',#61158,#18163,#18164);
#15435=AXIS2_PLACEMENT_3D('',#61159,#18165,#18166);
#15436=AXIS2_PLACEMENT_3D('',#61175,#18168,#18169);
#15437=AXIS2_PLACEMENT_3D('',#61183,#18170,#18171);
#15438=AXIS2_PLACEMENT_3D('',#61231,#18173,#18174);
#15439=AXIS2_PLACEMENT_3D('',#61279,#18176,#18177);
#15440=AXIS2_PLACEMENT_3D('',#61333,#18179,#18180);
#15441=AXIS2_PLACEMENT_3D('',#61381,#18182,#18183);
#15442=AXIS2_PLACEMENT_3D('',#61429,#18185,#18186);
#15443=AXIS2_PLACEMENT_3D('',#61483,#18188,#18189);
#15444=AXIS2_PLACEMENT_3D('',#61531,#18191,#18192);
#15445=AXIS2_PLACEMENT_3D('',#61579,#18194,#18195);
#15446=AXIS2_PLACEMENT_3D('',#61633,#18197,#18198);
#15447=AXIS2_PLACEMENT_3D('',#61681,#18200,#18201);
#15448=AXIS2_PLACEMENT_3D('',#61729,#18203,#18204);
#15449=AXIS2_PLACEMENT_3D('',#61783,#18206,#18207);
#15450=AXIS2_PLACEMENT_3D('',#61831,#18209,#18210);
#15451=AXIS2_PLACEMENT_3D('',#61879,#18212,#18213);
#15452=AXIS2_PLACEMENT_3D('',#61895,#18215,#18216);
#15453=AXIS2_PLACEMENT_3D('',#61904,#18217,#18218);
#15454=AXIS2_PLACEMENT_3D('',#61929,#18220,#18221);
#15455=AXIS2_PLACEMENT_3D('',#61953,#18223,#18224);
#15456=AXIS2_PLACEMENT_3D('',#61978,#18226,#18227);
#15457=AXIS2_PLACEMENT_3D('',#62003,#18229,#18230);
#15458=AXIS2_PLACEMENT_3D('',#62027,#18232,#18233);
#15459=AXIS2_PLACEMENT_3D('',#62052,#18235,#18236);
#15460=AXIS2_PLACEMENT_3D('',#62077,#18238,#18239);
#15461=AXIS2_PLACEMENT_3D('',#62101,#18241,#18242);
#15462=AXIS2_PLACEMENT_3D('',#62126,#18244,#18245);
#15463=AXIS2_PLACEMENT_3D('',#62151,#18247,#18248);
#15464=AXIS2_PLACEMENT_3D('',#62175,#18250,#18251);
#15465=AXIS2_PLACEMENT_3D('',#62200,#18253,#18254);
#15466=AXIS2_PLACEMENT_3D('',#62225,#18256,#18257);
#15467=AXIS2_PLACEMENT_3D('',#62249,#18259,#18260);
#15468=AXIS2_PLACEMENT_3D('',#62537,#18261,#18262);
#15469=AXIS2_PLACEMENT_3D('',#62571,#18264,#18265);
#15470=AXIS2_PLACEMENT_3D('',#63096,#18266,#18267);
#15471=AXIS2_PLACEMENT_3D('',#63107,#18268,#18269);
#15472=AXIS2_PLACEMENT_3D('',#63634,#18270,#18271);
#15473=AXIS2_PLACEMENT_3D('',#63635,#18272,#18273);
#15474=AXIS2_PLACEMENT_3D('',#63644,#18278,#18279);
#15475=AXIS2_PLACEMENT_3D('',#63650,#18283,#18284);
#15476=AXIS2_PLACEMENT_3D('',#63656,#18288,#18289);
#15477=AXIS2_PLACEMENT_3D('',#63662,#18293,#18294);
#15478=AXIS2_PLACEMENT_3D('',#63668,#18298,#18299);
#15479=AXIS2_PLACEMENT_3D('',#63671,#18302,#18303);
#15480=AXIS2_PLACEMENT_3D('',#63672,#18304,#18305);
#15481=AXIS2_PLACEMENT_3D('',#63674,#18306,#18307);
#15482=AXIS2_PLACEMENT_3D('',#63675,#18308,#18309);
#15483=AXIS2_PLACEMENT_3D('',#63678,#18311,#18312);
#15484=AXIS2_PLACEMENT_3D('',#63679,#18313,#18314);
#15485=AXIS2_PLACEMENT_3D('',#63680,#18315,#18316);
#15486=AXIS2_PLACEMENT_3D('',#63681,#18317,#18318);
#15487=AXIS2_PLACEMENT_3D('',#63682,#18319,#18320);
#15488=AXIS2_PLACEMENT_3D('',#63684,#18321,#18322);
#15489=AXIS2_PLACEMENT_3D('',#63687,#18324,#18325);
#15490=AXIS2_PLACEMENT_3D('',#63688,#18326,#18327);
#15491=AXIS2_PLACEMENT_3D('',#63690,#18328,#18329);
#15492=AXIS2_PLACEMENT_3D('',#63693,#18331,#18332);
#15493=AXIS2_PLACEMENT_3D('',#63694,#18333,#18334);
#15494=AXIS2_PLACEMENT_3D('',#63695,#18335,#18336);
#15495=AXIS2_PLACEMENT_3D('',#63696,#18337,#18338);
#15496=AXIS2_PLACEMENT_3D('',#63697,#18339,#18340);
#15497=AXIS2_PLACEMENT_3D('',#63698,#18341,#18342);
#15498=AXIS2_PLACEMENT_3D('',#63699,#18343,#18344);
#15499=AXIS2_PLACEMENT_3D('',#63700,#18345,#18346);
#15500=AXIS2_PLACEMENT_3D('',#63701,#18347,#18348);
#15501=AXIS2_PLACEMENT_3D('',#63702,#18349,#18350);
#15502=AXIS2_PLACEMENT_3D('',#63703,#18351,#18352);
#15503=AXIS2_PLACEMENT_3D('',#63704,#18353,#18354);
#15504=AXIS2_PLACEMENT_3D('',#63705,#18355,#18356);
#15505=AXIS2_PLACEMENT_3D('',#63706,#18357,#18358);
#15506=AXIS2_PLACEMENT_3D('',#63707,#18359,#18360);
#15507=AXIS2_PLACEMENT_3D('',#63708,#18361,#18362);
#15508=AXIS2_PLACEMENT_3D('',#63709,#18363,#18364);
#15509=AXIS2_PLACEMENT_3D('',#63710,#18365,#18366);
#15510=AXIS2_PLACEMENT_3D('',#63711,#18367,#18368);
#15511=AXIS2_PLACEMENT_3D('',#63712,#18369,#18370);
#15512=AXIS2_PLACEMENT_3D('',#63713,#18371,#18372);
#15513=AXIS2_PLACEMENT_3D('',#63714,#18373,#18374);
#15514=AXIS2_PLACEMENT_3D('',#63715,#18375,#18376);
#15515=DIRECTION('axis',(0.,0.,1.));
#15516=DIRECTION('refdir',(1.,0.,0.));
#15517=DIRECTION('axis',(0.,0.,1.));
#15518=DIRECTION('refdir',(1.,0.,0.));
#15519=DIRECTION('axis',(0.,0.,1.));
#15520=DIRECTION('refdir',(1.,0.,0.));
#15521=DIRECTION('center_axis',(0.,1.,0.));
#15522=DIRECTION('ref_axis',(-1.,0.,0.));
#15523=DIRECTION('',(-1.,0.,0.));
#15524=DIRECTION('',(0.,0.,1.));
#15525=DIRECTION('',(-1.,0.,0.));
#15526=DIRECTION('',(0.,0.,1.));
#15527=DIRECTION('center_axis',(-1.,0.,0.));
#15528=DIRECTION('ref_axis',(0.,-1.,0.));
#15529=DIRECTION('',(0.,-1.,0.));
#15530=DIRECTION('',(0.,-1.,0.));
#15531=DIRECTION('',(0.,0.,1.));
#15532=DIRECTION('center_axis',(0.,-1.,0.));
#15533=DIRECTION('ref_axis',(1.,0.,0.));
#15534=DIRECTION('',(1.,0.,0.));
#15535=DIRECTION('',(1.,0.,0.));
#15536=DIRECTION('',(0.,0.,1.));
#15537=DIRECTION('center_axis',(1.,0.,0.));
#15538=DIRECTION('ref_axis',(0.,1.,0.));
#15539=DIRECTION('',(0.,1.,0.));
#15540=DIRECTION('',(0.,1.,0.));
#15541=DIRECTION('center_axis',(0.,1.,0.));
#15542=DIRECTION('ref_axis',(-1.,0.,0.));
#15543=DIRECTION('',(-1.,0.,0.));
#15544=DIRECTION('',(0.,0.,1.));
#15545=DIRECTION('',(-1.,0.,0.));
#15546=DIRECTION('',(0.,0.,1.));
#15547=DIRECTION('center_axis',(1.,0.,0.));
#15548=DIRECTION('ref_axis',(0.,1.,0.));
#15549=DIRECTION('',(0.,1.,0.));
#15550=DIRECTION('',(0.,1.,0.));
#15551=DIRECTION('',(0.,0.,1.));
#15552=DIRECTION('center_axis',(0.,-1.,0.));
#15553=DIRECTION('ref_axis',(1.,0.,0.));
#15554=DIRECTION('',(1.,0.,0.));
#15555=DIRECTION('',(1.,0.,0.));
#15556=DIRECTION('',(0.,0.,1.));
#15557=DIRECTION('center_axis',(-1.,0.,0.));
#15558=DIRECTION('ref_axis',(0.,-1.,0.));
#15559=DIRECTION('',(0.,-1.,0.));
#15560=DIRECTION('',(0.,-1.,0.));
#15561=DIRECTION('center_axis',(0.,0.,1.));
#15562=DIRECTION('ref_axis',(1.,0.,0.));
#15563=DIRECTION('center_axis',(0.,0.,1.));
#15564=DIRECTION('ref_axis',(1.,0.,0.));
#15565=DIRECTION('axis',(0.,0.,1.));
#15566=DIRECTION('refdir',(1.,0.,0.));
#15567=DIRECTION('center_axis',(0.,1.,0.));
#15568=DIRECTION('ref_axis',(-1.,0.,0.));
#15569=DIRECTION('',(-1.,0.,0.));
#15570=DIRECTION('',(0.,0.,1.));
#15571=DIRECTION('',(-1.,0.,0.));
#15572=DIRECTION('',(0.,0.,1.));
#15573=DIRECTION('center_axis',(-1.,0.,0.));
#15574=DIRECTION('ref_axis',(0.,-1.,0.));
#15575=DIRECTION('',(0.,-1.,0.));
#15576=DIRECTION('',(0.,-1.,0.));
#15577=DIRECTION('',(0.,0.,1.));
#15578=DIRECTION('center_axis',(0.,-1.,0.));
#15579=DIRECTION('ref_axis',(1.,0.,0.));
#15580=DIRECTION('',(1.,0.,0.));
#15581=DIRECTION('',(1.,0.,0.));
#15582=DIRECTION('',(0.,0.,1.));
#15583=DIRECTION('center_axis',(1.,0.,0.));
#15584=DIRECTION('ref_axis',(0.,1.,0.));
#15585=DIRECTION('',(0.,1.,0.));
#15586=DIRECTION('',(0.,1.,0.));
#15587=DIRECTION('center_axis',(0.,1.,0.));
#15588=DIRECTION('ref_axis',(-1.,0.,0.));
#15589=DIRECTION('',(-1.,0.,0.));
#15590=DIRECTION('',(0.,0.,1.));
#15591=DIRECTION('',(-1.,0.,0.));
#15592=DIRECTION('',(0.,0.,1.));
#15593=DIRECTION('center_axis',(1.,0.,0.));
#15594=DIRECTION('ref_axis',(0.,1.,0.));
#15595=DIRECTION('',(0.,1.,0.));
#15596=DIRECTION('',(0.,1.,0.));
#15597=DIRECTION('',(0.,0.,1.));
#15598=DIRECTION('center_axis',(0.,-1.,0.));
#15599=DIRECTION('ref_axis',(1.,0.,0.));
#15600=DIRECTION('',(1.,0.,0.));
#15601=DIRECTION('',(1.,0.,0.));
#15602=DIRECTION('',(0.,0.,1.));
#15603=DIRECTION('center_axis',(-1.,0.,0.));
#15604=DIRECTION('ref_axis',(0.,-1.,0.));
#15605=DIRECTION('',(0.,-1.,0.));
#15606=DIRECTION('',(0.,-1.,0.));
#15607=DIRECTION('center_axis',(0.,0.,1.));
#15608=DIRECTION('ref_axis',(1.,0.,0.));
#15609=DIRECTION('center_axis',(0.,0.,1.));
#15610=DIRECTION('ref_axis',(1.,0.,0.));
#15611=DIRECTION('axis',(0.,0.,1.));
#15612=DIRECTION('refdir',(1.,0.,0.));
#15613=DIRECTION('center_axis',(0.,0.,-1.));
#15614=DIRECTION('ref_axis',(-0.34687556303371,0.9379111598494,0.));
#15615=DIRECTION('',(0.,0.,-1.));
#15616=DIRECTION('center_axis',(0.,0.,-1.));
#15617=DIRECTION('ref_axis',(1.,0.,0.));
#15618=DIRECTION('center_axis',(0.,0.,-1.));
#15619=DIRECTION('ref_axis',(1.,0.,0.));
#15620=DIRECTION('',(0.,0.,-1.));
#15621=DIRECTION('center_axis',(0.,0.,-1.));
#15622=DIRECTION('ref_axis',(1.,0.,0.));
#15623=DIRECTION('',(0.,0.,-1.));
#15624=DIRECTION('center_axis',(0.,0.,-1.));
#15625=DIRECTION('ref_axis',(1.,0.,0.));
#15626=DIRECTION('',(0.,0.,-1.));
#15627=DIRECTION('center_axis',(0.,0.,-1.));
#15628=DIRECTION('ref_axis',(1.,0.,0.));
#15629=DIRECTION('',(0.,0.,-1.));
#15630=DIRECTION('center_axis',(0.,0.,-1.));
#15631=DIRECTION('ref_axis',(1.,0.,0.));
#15632=DIRECTION('',(0.,0.,-1.));
#15633=DIRECTION('center_axis',(0.,0.,-1.));
#15634=DIRECTION('ref_axis',(1.,0.,0.));
#15635=DIRECTION('',(0.,0.,-1.));
#15636=DIRECTION('center_axis',(0.,0.,-1.));
#15637=DIRECTION('ref_axis',(0.938001830644068,-0.346630301197656,0.));
#15638=DIRECTION('',(0.,0.,-1.));
#15639=DIRECTION('center_axis',(0.,0.,-1.));
#15640=DIRECTION('ref_axis',(1.,0.,0.));
#15641=DIRECTION('center_axis',(0.,0.,-1.));
#15642=DIRECTION('ref_axis',(-0.346875820911814,0.937911064476134,0.));
#15643=DIRECTION('',(0.,0.,-1.));
#15644=DIRECTION('center_axis',(0.,0.,-1.));
#15645=DIRECTION('ref_axis',(1.,0.,0.));
#15646=DIRECTION('center_axis',(0.,0.,-1.));
#15647=DIRECTION('ref_axis',(1.,0.,0.));
#15648=DIRECTION('',(0.,0.,-1.));
#15649=DIRECTION('center_axis',(0.,0.,-1.));
#15650=DIRECTION('ref_axis',(1.,0.,0.));
#15651=DIRECTION('',(0.,0.,-1.));
#15652=DIRECTION('center_axis',(0.,0.,-1.));
#15653=DIRECTION('ref_axis',(1.,0.,0.));
#15654=DIRECTION('',(0.,0.,-1.));
#15655=DIRECTION('center_axis',(0.,0.,-1.));
#15656=DIRECTION('ref_axis',(1.,0.,0.));
#15657=DIRECTION('',(0.,0.,-1.));
#15658=DIRECTION('center_axis',(0.,0.,-1.));
#15659=DIRECTION('ref_axis',(1.,0.,0.));
#15660=DIRECTION('',(0.,0.,-1.));
#15661=DIRECTION('center_axis',(0.,0.,-1.));
#15662=DIRECTION('ref_axis',(1.,0.,0.));
#15663=DIRECTION('',(0.,0.,-1.));
#15664=DIRECTION('center_axis',(0.,0.,-1.));
#15665=DIRECTION('ref_axis',(0.938001844837498,-0.346630262789403,0.));
#15666=DIRECTION('',(0.,0.,-1.));
#15667=DIRECTION('center_axis',(0.,0.,-1.));
#15668=DIRECTION('ref_axis',(1.,0.,0.));
#15669=DIRECTION('center_axis',(0.,0.,-1.));
#15670=DIRECTION('ref_axis',(-0.346875921807931,0.937911027160838,0.));
#15671=DIRECTION('',(0.,0.,-1.));
#15672=DIRECTION('center_axis',(0.,0.,-1.));
#15673=DIRECTION('ref_axis',(1.,0.,0.));
#15674=DIRECTION('center_axis',(0.,0.,-1.));
#15675=DIRECTION('ref_axis',(1.,0.,0.));
#15676=DIRECTION('',(0.,0.,-1.));
#15677=DIRECTION('center_axis',(0.,0.,-1.));
#15678=DIRECTION('ref_axis',(1.,0.,0.));
#15679=DIRECTION('',(0.,0.,-1.));
#15680=DIRECTION('center_axis',(0.,0.,-1.));
#15681=DIRECTION('ref_axis',(1.,0.,0.));
#15682=DIRECTION('',(0.,0.,-1.));
#15683=DIRECTION('center_axis',(0.,0.,-1.));
#15684=DIRECTION('ref_axis',(1.,0.,0.));
#15685=DIRECTION('',(0.,0.,-1.));
#15686=DIRECTION('center_axis',(0.,0.,-1.));
#15687=DIRECTION('ref_axis',(1.,0.,0.));
#15688=DIRECTION('',(0.,0.,-1.));
#15689=DIRECTION('center_axis',(0.,0.,-1.));
#15690=DIRECTION('ref_axis',(1.,0.,0.));
#15691=DIRECTION('',(0.,0.,-1.));
#15692=DIRECTION('center_axis',(0.,0.,-1.));
#15693=DIRECTION('ref_axis',(0.93800185687022,-0.346630230228148,0.));
#15694=DIRECTION('',(0.,0.,-1.));
#15695=DIRECTION('center_axis',(0.,0.,-1.));
#15696=DIRECTION('ref_axis',(1.,0.,0.));
#15697=DIRECTION('center_axis',(0.,0.,-1.));
#15698=DIRECTION('ref_axis',(-0.346875444642522,0.937911203634999,0.));
#15699=DIRECTION('',(0.,0.,-1.));
#15700=DIRECTION('center_axis',(0.,0.,-1.));
#15701=DIRECTION('ref_axis',(1.,0.,0.));
#15702=DIRECTION('center_axis',(0.,0.,-1.));
#15703=DIRECTION('ref_axis',(1.,0.,0.));
#15704=DIRECTION('',(0.,0.,-1.));
#15705=DIRECTION('center_axis',(0.,0.,-1.));
#15706=DIRECTION('ref_axis',(1.,0.,0.));
#15707=DIRECTION('',(0.,0.,-1.));
#15708=DIRECTION('center_axis',(0.,0.,-1.));
#15709=DIRECTION('ref_axis',(1.,0.,0.));
#15710=DIRECTION('',(0.,0.,-1.));
#15711=DIRECTION('center_axis',(0.,0.,-1.));
#15712=DIRECTION('ref_axis',(1.,0.,0.));
#15713=DIRECTION('',(0.,0.,-1.));
#15714=DIRECTION('center_axis',(0.,0.,-1.));
#15715=DIRECTION('ref_axis',(1.,0.,0.));
#15716=DIRECTION('',(0.,0.,-1.));
#15717=DIRECTION('center_axis',(0.,0.,-1.));
#15718=DIRECTION('ref_axis',(1.,0.,0.));
#15719=DIRECTION('',(0.,0.,-1.));
#15720=DIRECTION('center_axis',(0.,0.,-1.));
#15721=DIRECTION('ref_axis',(0.938001817986921,-0.346630335448631,0.));
#15722=DIRECTION('',(0.,0.,-1.));
#15723=DIRECTION('center_axis',(0.,0.,-1.));
#15724=DIRECTION('ref_axis',(1.,0.,0.));
#15725=DIRECTION('center_axis',(0.,0.,-1.));
#15726=DIRECTION('ref_axis',(0.793238775227928,0.608910704023913,0.));
#15727=DIRECTION('',(1.22464679914735E-16,-2.81870473344804E-30,-1.));
#15728=DIRECTION('center_axis',(0.,0.,1.));
#15729=DIRECTION('ref_axis',(1.,-2.28940061540476E-14,0.));
#15730=DIRECTION('center_axis',(0.,0.,-1.));
#15731=DIRECTION('ref_axis',(1.,-2.28940061540476E-14,0.));
#15732=DIRECTION('',(1.22464679914735E-16,-2.81870473344804E-30,-1.));
#15733=DIRECTION('center_axis',(0.,0.,-1.));
#15734=DIRECTION('ref_axis',(1.,-2.28940061540476E-14,0.));
#15735=DIRECTION('',(1.22464679914735E-16,-2.81870473344804E-30,-1.));
#15736=DIRECTION('center_axis',(0.,0.,-1.));
#15737=DIRECTION('ref_axis',(1.,-2.28940061540476E-14,0.));
#15738=DIRECTION('',(1.22464679914735E-16,-2.81870473344804E-30,-1.));
#15739=DIRECTION('center_axis',(0.,0.,-1.));
#15740=DIRECTION('ref_axis',(1.,-2.28940061540476E-14,0.));
#15741=DIRECTION('',(1.22464679914735E-16,-2.81870473344804E-30,-1.));
#15742=DIRECTION('center_axis',(0.,0.,-1.));
#15743=DIRECTION('ref_axis',(1.,-2.28940061540476E-14,0.));
#15744=DIRECTION('',(1.22464679914735E-16,-2.81870473344804E-30,-1.));
#15745=DIRECTION('center_axis',(0.,0.,-1.));
#15746=DIRECTION('ref_axis',(1.,-2.28940061540476E-14,0.));
#15747=DIRECTION('',(1.22464679914735E-16,-2.81870473344804E-30,-1.));
#15748=DIRECTION('center_axis',(0.,0.,-1.));
#15749=DIRECTION('ref_axis',(-0.609093973761813,-0.793098058960582,0.));
#15750=DIRECTION('',(1.22464679914735E-16,-2.81870473344804E-30,-1.));
#15751=DIRECTION('center_axis',(0.,0.,-1.));
#15752=DIRECTION('ref_axis',(1.,-2.28940061540476E-14,0.));
#15753=DIRECTION('center_axis',(0.,0.,-1.));
#15754=DIRECTION('ref_axis',(0.793238729919907,0.608910763047471,0.));
#15755=DIRECTION('',(1.22464679914735E-16,-2.551685006246E-30,-1.));
#15756=DIRECTION('center_axis',(0.,0.,1.));
#15757=DIRECTION('ref_axis',(1.,-2.07136246155669E-14,0.));
#15758=DIRECTION('center_axis',(0.,0.,-1.));
#15759=DIRECTION('ref_axis',(1.,-2.07136246155669E-14,0.));
#15760=DIRECTION('',(1.22464679914735E-16,-2.551685006246E-30,-1.));
#15761=DIRECTION('center_axis',(0.,0.,-1.));
#15762=DIRECTION('ref_axis',(1.,-2.07136246155669E-14,0.));
#15763=DIRECTION('',(1.22464679914735E-16,-2.551685006246E-30,-1.));
#15764=DIRECTION('center_axis',(0.,0.,-1.));
#15765=DIRECTION('ref_axis',(1.,-2.07136246155669E-14,0.));
#15766=DIRECTION('',(1.22464679914735E-16,-2.551685006246E-30,-1.));
#15767=DIRECTION('center_axis',(0.,0.,-1.));
#15768=DIRECTION('ref_axis',(1.,-2.07136246155669E-14,0.));
#15769=DIRECTION('',(1.22464679914735E-16,-2.551685006246E-30,-1.));
#15770=DIRECTION('center_axis',(0.,0.,-1.));
#15771=DIRECTION('ref_axis',(1.,-2.07136246155669E-14,0.));
#15772=DIRECTION('',(1.22464679914735E-16,-2.551685006246E-30,-1.));
#15773=DIRECTION('center_axis',(0.,0.,-1.));
#15774=DIRECTION('ref_axis',(1.,-2.07136246155669E-14,0.));
#15775=DIRECTION('',(1.22464679914735E-16,-2.551685006246E-30,-1.));
#15776=DIRECTION('center_axis',(0.,0.,-1.));
#15777=DIRECTION('ref_axis',(-0.609093922666122,-0.793098098201727,0.));
#15778=DIRECTION('',(1.22464679914735E-16,-2.551685006246E-30,-1.));
#15779=DIRECTION('center_axis',(0.,0.,-1.));
#15780=DIRECTION('ref_axis',(1.,-2.07136246155669E-14,0.));
#15781=DIRECTION('center_axis',(0.,0.,-1.));
#15782=DIRECTION('ref_axis',(0.793238788726965,0.608910686438477,0.));
#15783=DIRECTION('',(1.22464679914735E-16,-2.55168500624601E-30,-1.));
#15784=DIRECTION('center_axis',(0.,0.,1.));
#15785=DIRECTION('ref_axis',(1.,-2.0713624615567E-14,0.));
#15786=DIRECTION('center_axis',(0.,0.,-1.));
#15787=DIRECTION('ref_axis',(1.,-2.0713624615567E-14,0.));
#15788=DIRECTION('',(1.22464679914735E-16,-2.55168500624601E-30,-1.));
#15789=DIRECTION('center_axis',(0.,0.,-1.));
#15790=DIRECTION('ref_axis',(1.,-2.0713624615567E-14,0.));
#15791=DIRECTION('',(1.22464679914735E-16,-2.55168500624601E-30,-1.));
#15792=DIRECTION('center_axis',(0.,0.,-1.));
#15793=DIRECTION('ref_axis',(1.,-2.0713624615567E-14,0.));
#15794=DIRECTION('',(1.22464679914735E-16,-2.55168500624601E-30,-1.));
#15795=DIRECTION('center_axis',(0.,0.,-1.));
#15796=DIRECTION('ref_axis',(1.,-2.0713624615567E-14,0.));
#15797=DIRECTION('',(1.22464679914735E-16,-2.55168500624601E-30,-1.));
#15798=DIRECTION('center_axis',(0.,0.,-1.));
#15799=DIRECTION('ref_axis',(1.,-2.0713624615567E-14,0.));
#15800=DIRECTION('',(1.22464679914735E-16,-2.55168500624601E-30,-1.));
#15801=DIRECTION('center_axis',(0.,0.,-1.));
#15802=DIRECTION('ref_axis',(1.,-2.0713624615567E-14,0.));
#15803=DIRECTION('',(1.22464679914735E-16,-2.55168500624601E-30,-1.));
#15804=DIRECTION('center_axis',(0.,0.,-1.));
#15805=DIRECTION('ref_axis',(-0.609093953553475,-0.79309807448045,0.));
#15806=DIRECTION('',(1.22464679914735E-16,-2.55168500624601E-30,-1.));
#15807=DIRECTION('center_axis',(0.,0.,-1.));
#15808=DIRECTION('ref_axis',(1.,-2.0713624615567E-14,0.));
#15809=DIRECTION('center_axis',(0.,0.,-1.));
#15810=DIRECTION('ref_axis',(0.79323871288191,0.608910785243167,0.));
#15811=DIRECTION('',(1.22464679914735E-16,-2.55168500624601E-30,-1.));
#15812=DIRECTION('center_axis',(0.,0.,1.));
#15813=DIRECTION('ref_axis',(1.,-2.0713624615567E-14,0.));
#15814=DIRECTION('center_axis',(0.,0.,-1.));
#15815=DIRECTION('ref_axis',(1.,-2.0713624615567E-14,0.));
#15816=DIRECTION('',(1.22464679914735E-16,-2.55168500624601E-30,-1.));
#15817=DIRECTION('center_axis',(0.,0.,-1.));
#15818=DIRECTION('ref_axis',(1.,-2.0713624615567E-14,0.));
#15819=DIRECTION('',(1.22464679914735E-16,-2.55168500624601E-30,-1.));
#15820=DIRECTION('center_axis',(0.,0.,-1.));
#15821=DIRECTION('ref_axis',(1.,-2.0713624615567E-14,0.));
#15822=DIRECTION('',(1.22464679914735E-16,-2.55168500624601E-30,-1.));
#15823=DIRECTION('center_axis',(0.,0.,-1.));
#15824=DIRECTION('ref_axis',(1.,-2.0713624615567E-14,0.));
#15825=DIRECTION('',(1.22464679914735E-16,-2.55168500624601E-30,-1.));
#15826=DIRECTION('center_axis',(0.,0.,-1.));
#15827=DIRECTION('ref_axis',(1.,-2.0713624615567E-14,0.));
#15828=DIRECTION('',(1.22464679914735E-16,-2.55168500624601E-30,-1.));
#15829=DIRECTION('center_axis',(0.,0.,-1.));
#15830=DIRECTION('ref_axis',(1.,-2.0713624615567E-14,0.));
#15831=DIRECTION('',(1.22464679914735E-16,-2.55168500624601E-30,-1.));
#15832=DIRECTION('center_axis',(0.,0.,-1.));
#15833=DIRECTION('ref_axis',(-0.609093936537935,-0.793098087548269,0.));
#15834=DIRECTION('',(1.22464679914735E-16,-2.55168500624601E-30,-1.));
#15835=DIRECTION('center_axis',(0.,0.,-1.));
#15836=DIRECTION('ref_axis',(1.,-2.0713624615567E-14,0.));
#15837=DIRECTION('center_axis',(0.,0.,-1.));
#15838=DIRECTION('ref_axis',(1.,-2.0713624615567E-14,0.));
#15839=DIRECTION('center_axis',(0.,0.,1.));
#15840=DIRECTION('ref_axis',(1.,0.,0.));
#15841=DIRECTION('',(0.,-1.,0.));
#15842=DIRECTION('',(1.,0.,0.));
#15843=DIRECTION('',(0.,1.,0.));
#15844=DIRECTION('',(-1.,0.,0.));
#15845=DIRECTION('center_axis',(0.,0.,-1.));
#15846=DIRECTION('ref_axis',(1.,-2.0713624615567E-14,0.));
#15847=DIRECTION('center_axis',(0.,0.,-1.));
#15848=DIRECTION('ref_axis',(1.,-2.07136246155669E-14,0.));
#15849=DIRECTION('center_axis',(0.,0.,-1.));
#15850=DIRECTION('ref_axis',(1.,-2.28940061540476E-14,0.));
#15851=DIRECTION('center_axis',(0.,0.,-1.));
#15852=DIRECTION('ref_axis',(1.,0.,0.));
#15853=DIRECTION('center_axis',(0.,0.,-1.));
#15854=DIRECTION('ref_axis',(1.,0.,0.));
#15855=DIRECTION('center_axis',(0.,0.,-1.));
#15856=DIRECTION('ref_axis',(1.,0.,0.));
#15857=DIRECTION('center_axis',(0.,0.,-1.));
#15858=DIRECTION('ref_axis',(1.,0.,0.));
#15859=DIRECTION('center_axis',(0.,1.,0.));
#15860=DIRECTION('ref_axis',(-1.,0.,0.));
#15861=DIRECTION('',(-1.,0.,0.));
#15862=DIRECTION('',(0.,0.,1.));
#15863=DIRECTION('',(0.,0.,1.));
#15864=DIRECTION('center_axis',(1.,0.,0.));
#15865=DIRECTION('ref_axis',(0.,1.,0.));
#15866=DIRECTION('',(0.,1.,0.));
#15867=DIRECTION('',(0.,0.,1.));
#15868=DIRECTION('center_axis',(0.,-1.,0.));
#15869=DIRECTION('ref_axis',(1.,0.,0.));
#15870=DIRECTION('',(1.,0.,0.));
#15871=DIRECTION('',(0.,0.,1.));
#15872=DIRECTION('center_axis',(-1.,0.,0.));
#15873=DIRECTION('ref_axis',(0.,-1.,0.));
#15874=DIRECTION('',(0.,-1.,0.));
#15875=DIRECTION('center_axis',(0.,0.,1.));
#15876=DIRECTION('ref_axis',(1.,0.,0.));
#15877=DIRECTION('axis',(0.,0.,1.));
#15878=DIRECTION('refdir',(1.,0.,0.));
#15879=DIRECTION('center_axis',(0.,0.,1.));
#15880=DIRECTION('ref_axis',(1.,0.,0.));
#15881=DIRECTION('',(0.,0.,-1.));
#15882=DIRECTION('center_axis',(0.,0.,-1.));
#15883=DIRECTION('ref_axis',(1.,0.,0.));
#15884=DIRECTION('center_axis',(0.,0.,1.));
#15885=DIRECTION('ref_axis',(1.,0.,0.));
#15886=DIRECTION('',(0.,0.,-1.));
#15887=DIRECTION('center_axis',(0.,0.,1.));
#15888=DIRECTION('ref_axis',(1.,0.,0.));
#15889=DIRECTION('',(0.,0.,-1.));
#15890=DIRECTION('center_axis',(0.,0.,1.));
#15891=DIRECTION('ref_axis',(1.,0.,0.));
#15892=DIRECTION('',(0.,0.,-1.));
#15893=DIRECTION('center_axis',(0.,0.,1.));
#15894=DIRECTION('ref_axis',(1.,0.,0.));
#15895=DIRECTION('',(0.,0.,-1.));
#15896=DIRECTION('center_axis',(0.,0.,1.));
#15897=DIRECTION('ref_axis',(1.,0.,0.));
#15898=DIRECTION('',(0.,0.,-1.));
#15899=DIRECTION('center_axis',(0.,0.,1.));
#15900=DIRECTION('ref_axis',(1.,0.,0.));
#15901=DIRECTION('',(0.,0.,-1.));
#15902=DIRECTION('center_axis',(0.,0.,1.));
#15903=DIRECTION('ref_axis',(1.,0.,0.));
#15904=DIRECTION('',(0.,0.,-1.));
#15905=DIRECTION('center_axis',(0.,0.,1.));
#15906=DIRECTION('ref_axis',(1.,0.,0.));
#15907=DIRECTION('',(0.,0.,-1.));
#15908=DIRECTION('center_axis',(0.,0.,1.));
#15909=DIRECTION('ref_axis',(1.,0.,0.));
#15910=DIRECTION('',(0.,0.,-1.));
#15911=DIRECTION('center_axis',(0.,0.,1.));
#15912=DIRECTION('ref_axis',(1.,0.,0.));
#15913=DIRECTION('',(0.,0.,-1.));
#15914=DIRECTION('center_axis',(0.,0.,1.));
#15915=DIRECTION('ref_axis',(1.,0.,0.));
#15916=DIRECTION('',(0.,0.,-1.));
#15917=DIRECTION('center_axis',(0.,0.,1.));
#15918=DIRECTION('ref_axis',(1.,0.,0.));
#15919=DIRECTION('',(0.,0.,-1.));
#15920=DIRECTION('center_axis',(0.,0.,1.));
#15921=DIRECTION('ref_axis',(1.,0.,0.));
#15922=DIRECTION('',(0.,0.,-1.));
#15923=DIRECTION('center_axis',(0.,0.,1.));
#15924=DIRECTION('ref_axis',(1.,0.,0.));
#15925=DIRECTION('',(0.,0.,-1.));
#15926=DIRECTION('center_axis',(0.,0.,1.));
#15927=DIRECTION('ref_axis',(1.,0.,0.));
#15928=DIRECTION('',(0.,0.,-1.));
#15929=DIRECTION('center_axis',(0.,0.,1.));
#15930=DIRECTION('ref_axis',(1.,0.,0.));
#15931=DIRECTION('',(0.,0.,-1.));
#15932=DIRECTION('center_axis',(0.,0.,1.));
#15933=DIRECTION('ref_axis',(1.,0.,0.));
#15934=DIRECTION('',(0.,0.,-1.));
#15935=DIRECTION('center_axis',(0.,0.,1.));
#15936=DIRECTION('ref_axis',(1.,0.,0.));
#15937=DIRECTION('',(0.,0.,-1.));
#15938=DIRECTION('center_axis',(0.,0.,1.));
#15939=DIRECTION('ref_axis',(1.,0.,0.));
#15940=DIRECTION('',(0.,0.,-1.));
#15941=DIRECTION('center_axis',(0.,0.,1.));
#15942=DIRECTION('ref_axis',(1.,0.,0.));
#15943=DIRECTION('',(0.,0.,-1.));
#15944=DIRECTION('center_axis',(0.,0.,1.));
#15945=DIRECTION('ref_axis',(1.,0.,0.));
#15946=DIRECTION('',(0.,0.,-1.));
#15947=DIRECTION('center_axis',(0.,0.,1.));
#15948=DIRECTION('ref_axis',(1.,0.,0.));
#15949=DIRECTION('',(0.,0.,-1.));
#15950=DIRECTION('center_axis',(0.,0.,1.));
#15951=DIRECTION('ref_axis',(1.,0.,0.));
#15952=DIRECTION('',(0.,0.,-1.));
#15953=DIRECTION('center_axis',(0.,0.,1.));
#15954=DIRECTION('ref_axis',(0.997333825498281,-0.0729742455731076,0.));
#15955=DIRECTION('',(0.,0.,1.));
#15956=DIRECTION('center_axis',(0.,0.,-1.));
#15957=DIRECTION('ref_axis',(1.,-6.20171864138877E-14,0.));
#15958=DIRECTION('center_axis',(0.,0.,1.));
#15959=DIRECTION('ref_axis',(1.,-6.20171864138877E-14,0.));
#15960=DIRECTION('',(0.,0.,1.));
#15961=DIRECTION('center_axis',(0.,0.,1.));
#15962=DIRECTION('ref_axis',(1.,-6.20171864138877E-14,0.));
#15963=DIRECTION('',(0.,0.,1.));
#15964=DIRECTION('center_axis',(0.,0.,1.));
#15965=DIRECTION('ref_axis',(1.,-6.20171864138877E-14,0.));
#15966=DIRECTION('',(0.,0.,1.));
#15967=DIRECTION('center_axis',(0.,0.,1.));
#15968=DIRECTION('ref_axis',(1.,-6.20171864138877E-14,0.));
#15969=DIRECTION('',(0.,0.,1.));
#15970=DIRECTION('center_axis',(0.,0.,1.));
#15971=DIRECTION('ref_axis',(1.,-6.20171864138877E-14,0.));
#15972=DIRECTION('',(0.,0.,1.));
#15973=DIRECTION('center_axis',(0.,0.,1.));
#15974=DIRECTION('ref_axis',(1.,-6.20171864138877E-14,0.));
#15975=DIRECTION('',(0.,0.,1.));
#15976=DIRECTION('center_axis',(0.,0.,1.));
#15977=DIRECTION('ref_axis',(1.,-6.20171864138877E-14,0.));
#15978=DIRECTION('',(0.,0.,1.));
#15979=DIRECTION('center_axis',(0.,0.,1.));
#15980=DIRECTION('ref_axis',(1.,-6.20171864138877E-14,0.));
#15981=DIRECTION('',(0.,0.,1.));
#15982=DIRECTION('center_axis',(0.,0.,1.));
#15983=DIRECTION('ref_axis',(1.,-6.20171864138877E-14,0.));
#15984=DIRECTION('',(0.,0.,1.));
#15985=DIRECTION('center_axis',(0.,0.,1.));
#15986=DIRECTION('ref_axis',(1.,-6.20171864138877E-14,0.));
#15987=DIRECTION('',(0.,0.,1.));
#15988=DIRECTION('center_axis',(0.,0.,1.));
#15989=DIRECTION('ref_axis',(1.,-6.20171864138877E-14,0.));
#15990=DIRECTION('',(0.,0.,1.));
#15991=DIRECTION('center_axis',(0.,0.,1.));
#15992=DIRECTION('ref_axis',(1.,-6.20171864138877E-14,0.));
#15993=DIRECTION('',(0.,0.,1.));
#15994=DIRECTION('center_axis',(0.,0.,1.));
#15995=DIRECTION('ref_axis',(1.,-6.20171864138877E-14,0.));
#15996=DIRECTION('',(0.,0.,1.));
#15997=DIRECTION('center_axis',(0.,0.,1.));
#15998=DIRECTION('ref_axis',(1.,-6.20171864138877E-14,0.));
#15999=DIRECTION('',(0.,0.,1.));
#16000=DIRECTION('center_axis',(0.,0.,1.));
#16001=DIRECTION('ref_axis',(1.,-6.20171864138877E-14,0.));
#16002=DIRECTION('',(0.,0.,1.));
#16003=DIRECTION('center_axis',(0.,0.,1.));
#16004=DIRECTION('ref_axis',(1.,-6.20171864138877E-14,0.));
#16005=DIRECTION('',(0.,0.,1.));
#16006=DIRECTION('center_axis',(0.,0.,1.));
#16007=DIRECTION('ref_axis',(1.,-6.20171864138877E-14,0.));
#16008=DIRECTION('',(0.,0.,1.));
#16009=DIRECTION('center_axis',(0.,0.,1.));
#16010=DIRECTION('ref_axis',(1.,-6.20171864138877E-14,0.));
#16011=DIRECTION('',(0.,0.,1.));
#16012=DIRECTION('center_axis',(0.,0.,1.));
#16013=DIRECTION('ref_axis',(1.,-6.20171864138877E-14,0.));
#16014=DIRECTION('',(0.,0.,1.));
#16015=DIRECTION('center_axis',(0.,0.,1.));
#16016=DIRECTION('ref_axis',(1.,-6.20171864138877E-14,0.));
#16017=DIRECTION('',(0.,0.,1.));
#16018=DIRECTION('center_axis',(0.,0.,1.));
#16019=DIRECTION('ref_axis',(1.,-6.20171864138877E-14,0.));
#16020=DIRECTION('',(0.,0.,1.));
#16021=DIRECTION('center_axis',(0.,0.,1.));
#16022=DIRECTION('ref_axis',(1.,-6.20171864138877E-14,0.));
#16023=DIRECTION('',(0.,0.,1.));
#16024=DIRECTION('center_axis',(0.,0.,1.));
#16025=DIRECTION('ref_axis',(1.,-6.20171864138877E-14,0.));
#16026=DIRECTION('',(0.,0.,1.));
#16027=DIRECTION('center_axis',(0.,0.,-1.));
#16028=DIRECTION('ref_axis',(1.,0.,0.));
#16029=DIRECTION('center_axis',(0.,0.,-1.));
#16030=DIRECTION('ref_axis',(1.,0.,0.));
#16031=DIRECTION('',(0.707106781186547,8.65956056235493E-17,0.707106781186548));
#16032=DIRECTION('center_axis',(0.,0.,1.));
#16033=DIRECTION('ref_axis',(1.,0.,0.));
#16034=DIRECTION('center_axis',(0.,0.,1.));
#16035=DIRECTION('ref_axis',(1.,-6.20171864138877E-14,0.));
#16036=DIRECTION('center_axis',(0.,0.,-1.));
#16037=DIRECTION('ref_axis',(1.,-6.20171864138877E-14,0.));
#16038=DIRECTION('center_axis',(0.,0.,1.));
#16039=DIRECTION('ref_axis',(1.,0.,0.));
#16040=DIRECTION('center_axis',(-1.60246890531964E-16,-1.,0.));
#16041=DIRECTION('ref_axis',(1.,-1.60246890531964E-16,0.));
#16042=DIRECTION('',(1.,-1.60246890531964E-16,0.));
#16043=DIRECTION('',(0.,0.,1.));
#16044=DIRECTION('',(1.,-1.60246890531964E-16,0.));
#16045=DIRECTION('',(0.,0.,1.));
#16046=DIRECTION('center_axis',(-0.866025403784439,-0.5,0.));
#16047=DIRECTION('ref_axis',(0.5,-0.866025403784439,0.));
#16048=DIRECTION('',(0.5,-0.866025403784439,0.));
#16049=DIRECTION('',(0.,0.,1.));
#16050=DIRECTION('',(0.5,-0.866025403784439,0.));
#16051=DIRECTION('center_axis',(-0.866025403784439,0.5,0.));
#16052=DIRECTION('ref_axis',(-0.5,-0.866025403784439,0.));
#16053=DIRECTION('',(-0.5,-0.866025403784439,0.));
#16054=DIRECTION('',(0.,0.,1.));
#16055=DIRECTION('',(-0.5,-0.866025403784439,0.));
#16056=DIRECTION('center_axis',(1.60246890531964E-16,1.,0.));
#16057=DIRECTION('ref_axis',(-1.,1.60246890531964E-16,0.));
#16058=DIRECTION('',(-1.,1.60246890531964E-16,0.));
#16059=DIRECTION('',(0.,0.,1.));
#16060=DIRECTION('',(-1.,1.60246890531964E-16,0.));
#16061=DIRECTION('center_axis',(0.866025403784439,0.5,0.));
#16062=DIRECTION('ref_axis',(-0.5,0.866025403784439,0.));
#16063=DIRECTION('',(-0.5,0.866025403784439,0.));
#16064=DIRECTION('',(0.,0.,1.));
#16065=DIRECTION('',(-0.5,0.866025403784439,0.));
#16066=DIRECTION('center_axis',(0.866025403784439,-0.5,0.));
#16067=DIRECTION('ref_axis',(0.5,0.866025403784439,0.));
#16068=DIRECTION('',(0.5,0.866025403784439,0.));
#16069=DIRECTION('',(0.5,0.866025403784439,0.));
#16070=DIRECTION('center_axis',(0.,0.,1.));
#16071=DIRECTION('ref_axis',(1.,0.,0.));
#16072=DIRECTION('center_axis',(0.,0.,1.));
#16073=DIRECTION('ref_axis',(1.,0.,0.));
#16074=DIRECTION('center_axis',(0.,0.,1.));
#16075=DIRECTION('ref_axis',(1.,0.,0.));
#16076=DIRECTION('center_axis',(0.,0.,1.));
#16077=DIRECTION('ref_axis',(1.,0.,0.));
#16078=DIRECTION('',(0.,0.,-1.));
#16079=DIRECTION('center_axis',(0.,0.,1.));
#16080=DIRECTION('ref_axis',(1.,0.,0.));
#16081=DIRECTION('center_axis',(0.,0.,1.));
#16082=DIRECTION('ref_axis',(1.,0.,0.));
#16083=DIRECTION('center_axis',(0.,0.,1.));
#16084=DIRECTION('ref_axis',(1.,0.,0.));
#16085=DIRECTION('axis',(0.,0.,1.));
#16086=DIRECTION('refdir',(1.,0.,0.));
#16087=DIRECTION('center_axis',(0.,0.,1.));
#16088=DIRECTION('ref_axis',(1.,0.,0.));
#16089=DIRECTION('center_axis',(0.,0.,-1.));
#16090=DIRECTION('ref_axis',(1.,0.,0.));
#16091=DIRECTION('',(0.,0.,-1.));
#16092=DIRECTION('center_axis',(0.,0.,-1.));
#16093=DIRECTION('ref_axis',(1.,0.,0.));
#16094=DIRECTION('center_axis',(0.,0.,1.));
#16095=DIRECTION('ref_axis',(1.,0.,0.));
#16096=DIRECTION('center_axis',(0.,0.,1.));
#16097=DIRECTION('ref_axis',(1.,0.,0.));
#16098=DIRECTION('',(0.,0.,-1.));
#16099=DIRECTION('center_axis',(0.,0.,1.));
#16100=DIRECTION('ref_axis',(1.,0.,0.));
#16101=DIRECTION('center_axis',(0.,0.,1.));
#16102=DIRECTION('ref_axis',(1.,0.,0.));
#16103=DIRECTION('center_axis',(0.,0.,1.));
#16104=DIRECTION('ref_axis',(1.,0.,0.));
#16105=DIRECTION('',(1.,0.,2.22044604925031E-16));
#16106=DIRECTION('',(2.22044604925031E-16,0.,-1.));
#16107=DIRECTION('',(0.,1.,0.));
#16108=DIRECTION('',(0.,0.,1.));
#16109=DIRECTION('',(0.,0.,1.));
#16110=DIRECTION('',(1.,0.,0.));
#16111=DIRECTION('',(0.,0.,1.));
#16112=DIRECTION('',(-1.,1.22464679914735E-16,0.));
#16113=DIRECTION('',(0.,0.,1.));
#16114=DIRECTION('',(1.,0.,0.));
#16115=DIRECTION('',(1.,0.,2.22044604925031E-16));
#16116=DIRECTION('',(2.22044604925031E-16,0.,-1.));
#16117=DIRECTION('',(0.,1.,0.));
#16118=DIRECTION('',(0.,0.,1.));
#16119=DIRECTION('',(0.,0.,1.));
#16120=DIRECTION('',(1.,0.,0.));
#16121=DIRECTION('',(0.,0.,1.));
#16122=DIRECTION('',(1.,0.,0.));
#16123=DIRECTION('',(0.,0.,1.));
#16124=DIRECTION('',(1.,0.,0.));
#16125=DIRECTION('',(0.,0.,1.));
#16126=DIRECTION('',(-1.,1.22464679914735E-16,0.));
#16127=DIRECTION('',(0.,0.,1.));
#16128=DIRECTION('',(1.,0.,0.));
#16129=DIRECTION('',(0.,0.,1.));
#16130=DIRECTION('',(-1.,1.22464679914735E-16,0.));
#16131=DIRECTION('',(0.,0.,1.));
#16132=DIRECTION('',(1.,0.,0.));
#16133=DIRECTION('',(0.,0.,1.));
#16134=DIRECTION('',(-1.,1.22464679914735E-16,0.));
#16135=DIRECTION('',(0.,0.,1.));
#16136=DIRECTION('',(1.,0.,0.));
#16137=DIRECTION('',(0.,0.,1.));
#16138=DIRECTION('',(-1.,1.22464679914735E-16,0.));
#16139=DIRECTION('',(0.,0.,1.));
#16140=DIRECTION('',(1.,0.,0.));
#16141=DIRECTION('',(0.,0.,1.));
#16142=DIRECTION('',(-1.,1.22464679914735E-16,0.));
#16143=DIRECTION('',(0.,0.,1.));
#16144=DIRECTION('',(1.,0.,0.));
#16145=DIRECTION('',(0.,0.,1.));
#16146=DIRECTION('',(-1.,1.22464679914735E-16,0.));
#16147=DIRECTION('',(0.,0.,1.));
#16148=DIRECTION('',(1.,0.,0.));
#16149=DIRECTION('',(0.,0.,1.));
#16150=DIRECTION('',(-1.,1.22464679914735E-16,0.));
#16151=DIRECTION('',(0.,0.,1.));
#16152=DIRECTION('',(1.,0.,0.));
#16153=DIRECTION('',(0.,0.,1.));
#16154=DIRECTION('',(-1.,1.22464679914735E-16,0.));
#16155=DIRECTION('',(0.,0.,1.));
#16156=DIRECTION('',(1.,0.,0.));
#16157=DIRECTION('',(0.,0.,1.));
#16158=DIRECTION('',(-1.,1.22464679914735E-16,0.));
#16159=DIRECTION('',(0.,0.,1.));
#16160=DIRECTION('',(1.,0.,0.));
#16161=DIRECTION('',(0.,0.,1.));
#16162=DIRECTION('',(-1.,1.22464679914735E-16,0.));
#16163=DIRECTION('',(0.,0.,1.));
#16164=DIRECTION('',(1.,0.,0.));
#16165=DIRECTION('',(0.,0.,1.));
#16166=DIRECTION('',(-1.,1.22464679914735E-16,0.));
#16167=DIRECTION('',(0.,0.,1.));
#16168=DIRECTION('',(1.,0.,0.));
#16169=DIRECTION('',(0.,0.,1.));
#16170=DIRECTION('',(-1.,1.22464679914735E-16,0.));
#16171=DIRECTION('',(0.,0.,1.));
#16172=DIRECTION('',(1.,0.,0.));
#16173=DIRECTION('',(0.,0.,1.));
#16174=DIRECTION('',(-1.,1.22464679914735E-16,0.));
#16175=DIRECTION('',(0.,0.,1.));
#16176=DIRECTION('',(1.,0.,0.));
#16177=DIRECTION('',(0.,0.,1.));
#16178=DIRECTION('',(-1.,1.22464679914735E-16,0.));
#16179=DIRECTION('',(0.,0.,1.));
#16180=DIRECTION('',(1.,0.,0.));
#16181=DIRECTION('',(0.,0.,1.));
#16182=DIRECTION('',(-1.,1.22464679914735E-16,0.));
#16183=DIRECTION('',(0.,0.,1.));
#16184=DIRECTION('',(1.,0.,0.));
#16185=DIRECTION('axis',(0.,0.,1.));
#16186=DIRECTION('refdir',(1.,0.,0.));
#16187=DIRECTION('axis',(0.,0.,1.));
#16188=DIRECTION('refdir',(1.,0.,0.));
#16189=DIRECTION('center_axis',(0.,0.,-1.));
#16190=DIRECTION('ref_axis',(1.,0.,0.));
#16191=DIRECTION('',(0.,0.,-1.));
#16192=DIRECTION('center_axis',(0.,0.,1.));
#16193=DIRECTION('ref_axis',(1.,0.,0.));
#16194=DIRECTION('',(0.,0.,-1.));
#16195=DIRECTION('center_axis',(0.,0.,1.));
#16196=DIRECTION('ref_axis',(1.,0.,0.));
#16197=DIRECTION('center_axis',(0.,0.,1.));
#16198=DIRECTION('ref_axis',(1.,0.,0.));
#16199=DIRECTION('center_axis',(0.,0.,-1.));
#16200=DIRECTION('ref_axis',(1.,0.,0.));
#16201=DIRECTION('',(0.,0.,-1.));
#16202=DIRECTION('center_axis',(0.,0.,-1.));
#16203=DIRECTION('ref_axis',(1.,0.,0.));
#16204=DIRECTION('',(0.,0.,-1.));
#16205=DIRECTION('center_axis',(0.,0.,-1.));
#16206=DIRECTION('ref_axis',(1.,0.,0.));
#16207=DIRECTION('',(0.,0.,-1.));
#16208=DIRECTION('center_axis',(0.,0.,-1.));
#16209=DIRECTION('ref_axis',(1.,0.,0.));
#16210=DIRECTION('',(0.,0.,-1.));
#16211=DIRECTION('center_axis',(0.,0.,-1.));
#16212=DIRECTION('ref_axis',(1.,0.,0.));
#16213=DIRECTION('',(0.,0.,-1.));
#16214=DIRECTION('center_axis',(0.,0.,-1.));
#16215=DIRECTION('ref_axis',(1.,0.,0.));
#16216=DIRECTION('',(0.,0.,-1.));
#16217=DIRECTION('center_axis',(0.,0.,-1.));
#16218=DIRECTION('ref_axis',(1.,0.,0.));
#16219=DIRECTION('',(0.,0.,-1.));
#16220=DIRECTION('center_axis',(0.,0.,-1.));
#16221=DIRECTION('ref_axis',(1.,0.,0.));
#16222=DIRECTION('',(0.,0.,-1.));
#16223=DIRECTION('center_axis',(0.,0.,-1.));
#16224=DIRECTION('ref_axis',(1.,0.,0.));
#16225=DIRECTION('',(0.,0.,-1.));
#16226=DIRECTION('center_axis',(0.,0.,-1.));
#16227=DIRECTION('ref_axis',(1.,0.,0.));
#16228=DIRECTION('',(0.,0.,-1.));
#16229=DIRECTION('center_axis',(0.,0.,-1.));
#16230=DIRECTION('ref_axis',(1.,0.,0.));
#16231=DIRECTION('',(0.,0.,-1.));
#16232=DIRECTION('center_axis',(0.,0.,-1.));
#16233=DIRECTION('ref_axis',(1.,0.,0.));
#16234=DIRECTION('',(0.,0.,-1.));
#16235=DIRECTION('center_axis',(0.,0.,-1.));
#16236=DIRECTION('ref_axis',(1.,0.,0.));
#16237=DIRECTION('',(0.,0.,-1.));
#16238=DIRECTION('center_axis',(0.,0.,-1.));
#16239=DIRECTION('ref_axis',(1.,0.,0.));
#16240=DIRECTION('',(0.,0.,-1.));
#16241=DIRECTION('center_axis',(0.,0.,-1.));
#16242=DIRECTION('ref_axis',(1.,0.,0.));
#16243=DIRECTION('',(0.,0.,-1.));
#16244=DIRECTION('center_axis',(0.,0.,-1.));
#16245=DIRECTION('ref_axis',(1.,0.,0.));
#16246=DIRECTION('',(0.,0.,-1.));
#16247=DIRECTION('center_axis',(0.,0.,-1.));
#16248=DIRECTION('ref_axis',(1.,0.,0.));
#16249=DIRECTION('',(0.,0.,-1.));
#16250=DIRECTION('center_axis',(0.,0.,-1.));
#16251=DIRECTION('ref_axis',(1.,0.,0.));
#16252=DIRECTION('',(0.,0.,-1.));
#16253=DIRECTION('center_axis',(0.,0.,-1.));
#16254=DIRECTION('ref_axis',(1.,0.,0.));
#16255=DIRECTION('',(0.,0.,-1.));
#16256=DIRECTION('center_axis',(0.,0.,-1.));
#16257=DIRECTION('ref_axis',(1.,0.,0.));
#16258=DIRECTION('',(0.,0.,-1.));
#16259=DIRECTION('center_axis',(0.,0.,-1.));
#16260=DIRECTION('ref_axis',(1.,0.,0.));
#16261=DIRECTION('',(0.,0.,-1.));
#16262=DIRECTION('center_axis',(0.,0.,-1.));
#16263=DIRECTION('ref_axis',(1.,0.,0.));
#16264=DIRECTION('',(0.,0.,-1.));
#16265=DIRECTION('center_axis',(0.,0.,-1.));
#16266=DIRECTION('ref_axis',(1.,0.,0.));
#16267=DIRECTION('',(0.,0.,-1.));
#16268=DIRECTION('center_axis',(0.,0.,-1.));
#16269=DIRECTION('ref_axis',(0.938097899428847,-0.346370222575766,0.));
#16270=DIRECTION('',(0.,0.,-1.));
#16271=DIRECTION('center_axis',(0.,0.,-1.));
#16272=DIRECTION('ref_axis',(1.,0.,0.));
#16273=DIRECTION('center_axis',(0.,0.,-1.));
#16274=DIRECTION('ref_axis',(0.793346897669268,0.608769825105144,0.));
#16275=DIRECTION('',(1.22464679914735E-16,3.85574710022057E-30,-1.));
#16276=DIRECTION('center_axis',(0.,0.,1.));
#16277=DIRECTION('ref_axis',(1.,3.16070290694603E-14,0.));
#16278=DIRECTION('center_axis',(0.,0.,-1.));
#16279=DIRECTION('ref_axis',(1.,3.16070290694603E-14,0.));
#16280=DIRECTION('',(1.22464679914735E-16,3.85574710022057E-30,-1.));
#16281=DIRECTION('center_axis',(0.,0.,-1.));
#16282=DIRECTION('ref_axis',(1.,3.16070290694603E-14,0.));
#16283=DIRECTION('',(1.22464679914735E-16,3.85574710022057E-30,-1.));
#16284=DIRECTION('center_axis',(0.,0.,-1.));
#16285=DIRECTION('ref_axis',(1.,3.16070290694603E-14,0.));
#16286=DIRECTION('',(1.22464679914735E-16,3.85574710022057E-30,-1.));
#16287=DIRECTION('center_axis',(0.,0.,-1.));
#16288=DIRECTION('ref_axis',(1.,3.16070290694603E-14,0.));
#16289=DIRECTION('',(1.22464679914735E-16,3.85574710022057E-30,-1.));
#16290=DIRECTION('center_axis',(0.,0.,-1.));
#16291=DIRECTION('ref_axis',(1.,3.16070290694603E-14,0.));
#16292=DIRECTION('',(1.22464679914735E-16,3.85574710022057E-30,-1.));
#16293=DIRECTION('center_axis',(0.,0.,-1.));
#16294=DIRECTION('ref_axis',(1.,3.16070290694603E-14,0.));
#16295=DIRECTION('',(1.22464679914735E-16,3.85574710022057E-30,-1.));
#16296=DIRECTION('center_axis',(0.,0.,-1.));
#16297=DIRECTION('ref_axis',(1.,3.16070290694603E-14,0.));
#16298=DIRECTION('',(1.22464679914735E-16,3.85574710022057E-30,-1.));
#16299=DIRECTION('center_axis',(0.,0.,-1.));
#16300=DIRECTION('ref_axis',(1.,3.16070290694603E-14,0.));
#16301=DIRECTION('',(1.22464679914735E-16,3.85574710022057E-30,-1.));
#16302=DIRECTION('center_axis',(0.,0.,-1.));
#16303=DIRECTION('ref_axis',(1.,3.16070290694603E-14,0.));
#16304=DIRECTION('',(1.22464679914735E-16,3.85574710022057E-30,-1.));
#16305=DIRECTION('center_axis',(0.,0.,-1.));
#16306=DIRECTION('ref_axis',(1.,3.16070290694603E-14,0.));
#16307=DIRECTION('',(1.22464679914735E-16,3.85574710022057E-30,-1.));
#16308=DIRECTION('center_axis',(0.,0.,-1.));
#16309=DIRECTION('ref_axis',(1.,3.16070290694603E-14,0.));
#16310=DIRECTION('',(1.22464679914735E-16,3.85574710022057E-30,-1.));
#16311=DIRECTION('center_axis',(0.,0.,-1.));
#16312=DIRECTION('ref_axis',(1.,3.16070290694603E-14,0.));
#16313=DIRECTION('',(1.22464679914735E-16,3.85574710022057E-30,-1.));
#16314=DIRECTION('center_axis',(0.,0.,-1.));
#16315=DIRECTION('ref_axis',(1.,3.16070290694603E-14,0.));
#16316=DIRECTION('',(1.22464679914735E-16,3.85574710022057E-30,-1.));
#16317=DIRECTION('center_axis',(0.,0.,-1.));
#16318=DIRECTION('ref_axis',(1.,3.16070290694603E-14,0.));
#16319=DIRECTION('',(1.22464679914735E-16,3.85574710022057E-30,-1.));
#16320=DIRECTION('center_axis',(0.,0.,-1.));
#16321=DIRECTION('ref_axis',(1.,3.16070290694603E-14,0.));
#16322=DIRECTION('',(1.22464679914735E-16,3.85574710022057E-30,-1.));
#16323=DIRECTION('center_axis',(0.,0.,-1.));
#16324=DIRECTION('ref_axis',(1.,3.16070290694603E-14,0.));
#16325=DIRECTION('',(1.22464679914735E-16,3.85574710022057E-30,-1.));
#16326=DIRECTION('center_axis',(0.,0.,-1.));
#16327=DIRECTION('ref_axis',(1.,3.16070290694603E-14,0.));
#16328=DIRECTION('',(1.22464679914735E-16,3.85574710022057E-30,-1.));
#16329=DIRECTION('center_axis',(0.,0.,-1.));
#16330=DIRECTION('ref_axis',(1.,3.16070290694603E-14,0.));
#16331=DIRECTION('',(1.22464679914735E-16,3.85574710022057E-30,-1.));
#16332=DIRECTION('center_axis',(0.,0.,-1.));
#16333=DIRECTION('ref_axis',(1.,3.16070290694603E-14,0.));
#16334=DIRECTION('',(1.22464679914735E-16,3.85574710022057E-30,-1.));
#16335=DIRECTION('center_axis',(0.,0.,-1.));
#16336=DIRECTION('ref_axis',(1.,3.16070290694603E-14,0.));
#16337=DIRECTION('',(1.22464679914735E-16,3.85574710022057E-30,-1.));
#16338=DIRECTION('center_axis',(0.,0.,-1.));
#16339=DIRECTION('ref_axis',(1.,3.16070290694603E-14,0.));
#16340=DIRECTION('',(1.22464679914735E-16,3.85574710022057E-30,-1.));
#16341=DIRECTION('center_axis',(0.,0.,-1.));
#16342=DIRECTION('ref_axis',(1.,3.16070290694603E-14,0.));
#16343=DIRECTION('',(1.22464679914735E-16,3.85574710022057E-30,-1.));
#16344=DIRECTION('center_axis',(0.,0.,-1.));
#16345=DIRECTION('ref_axis',(1.,3.16070290694603E-14,0.));
#16346=DIRECTION('',(1.22464679914735E-16,3.85574710022057E-30,-1.));
#16347=DIRECTION('center_axis',(0.,0.,-1.));
#16348=DIRECTION('ref_axis',(-0.6087766502803,-0.793341660366766,0.));
#16349=DIRECTION('',(1.22464679914735E-16,3.85574710022057E-30,-1.));
#16350=DIRECTION('center_axis',(0.,0.,-1.));
#16351=DIRECTION('ref_axis',(1.,3.16070290694603E-14,0.));
#16352=DIRECTION('center_axis',(0.,0.,1.));
#16353=DIRECTION('ref_axis',(-1.,0.,0.));
#16354=DIRECTION('',(0.,0.,1.));
#16355=DIRECTION('center_axis',(0.,0.,-1.));
#16356=DIRECTION('ref_axis',(-1.,0.,0.));
#16357=DIRECTION('',(0.,0.,1.));
#16358=DIRECTION('center_axis',(0.,0.,-1.));
#16359=DIRECTION('ref_axis',(-1.,0.,0.));
#16360=DIRECTION('center_axis',(0.,0.,-1.));
#16361=DIRECTION('ref_axis',(-1.,0.,0.));
#16362=DIRECTION('center_axis',(0.,0.,1.));
#16363=DIRECTION('ref_axis',(-1.,0.,0.));
#16364=DIRECTION('',(0.,0.,1.));
#16365=DIRECTION('center_axis',(0.,0.,1.));
#16366=DIRECTION('ref_axis',(-1.,0.,0.));
#16367=DIRECTION('',(0.,0.,1.));
#16368=DIRECTION('center_axis',(0.,0.,1.));
#16369=DIRECTION('ref_axis',(-1.,0.,0.));
#16370=DIRECTION('',(0.,0.,1.));
#16371=DIRECTION('center_axis',(0.,0.,1.));
#16372=DIRECTION('ref_axis',(-1.,0.,0.));
#16373=DIRECTION('',(0.,0.,1.));
#16374=DIRECTION('center_axis',(0.,0.,1.));
#16375=DIRECTION('ref_axis',(-1.,0.,0.));
#16376=DIRECTION('',(0.,0.,1.));
#16377=DIRECTION('center_axis',(0.,0.,1.));
#16378=DIRECTION('ref_axis',(-1.,0.,0.));
#16379=DIRECTION('',(0.,0.,1.));
#16380=DIRECTION('center_axis',(0.,0.,1.));
#16381=DIRECTION('ref_axis',(-1.,0.,0.));
#16382=DIRECTION('',(0.,0.,1.));
#16383=DIRECTION('center_axis',(0.,0.,1.));
#16384=DIRECTION('ref_axis',(-1.,0.,0.));
#16385=DIRECTION('',(0.,0.,1.));
#16386=DIRECTION('center_axis',(0.,0.,1.));
#16387=DIRECTION('ref_axis',(-1.,0.,0.));
#16388=DIRECTION('',(0.,0.,1.));
#16389=DIRECTION('center_axis',(0.,0.,1.));
#16390=DIRECTION('ref_axis',(-1.,0.,0.));
#16391=DIRECTION('',(0.,0.,1.));
#16392=DIRECTION('center_axis',(0.,0.,1.));
#16393=DIRECTION('ref_axis',(-1.,0.,0.));
#16394=DIRECTION('',(0.,0.,1.));
#16395=DIRECTION('center_axis',(0.,0.,1.));
#16396=DIRECTION('ref_axis',(-1.,0.,0.));
#16397=DIRECTION('',(0.,0.,1.));
#16398=DIRECTION('center_axis',(0.,0.,1.));
#16399=DIRECTION('ref_axis',(-1.,0.,0.));
#16400=DIRECTION('',(0.,0.,1.));
#16401=DIRECTION('center_axis',(0.,0.,1.));
#16402=DIRECTION('ref_axis',(-1.,0.,0.));
#16403=DIRECTION('',(0.,0.,1.));
#16404=DIRECTION('center_axis',(0.,0.,1.));
#16405=DIRECTION('ref_axis',(-1.,0.,0.));
#16406=DIRECTION('',(0.,0.,1.));
#16407=DIRECTION('center_axis',(0.,0.,1.));
#16408=DIRECTION('ref_axis',(-1.,0.,0.));
#16409=DIRECTION('',(0.,0.,1.));
#16410=DIRECTION('center_axis',(0.,0.,1.));
#16411=DIRECTION('ref_axis',(-1.,0.,0.));
#16412=DIRECTION('',(0.,0.,1.));
#16413=DIRECTION('center_axis',(0.,0.,1.));
#16414=DIRECTION('ref_axis',(-1.,0.,0.));
#16415=DIRECTION('',(0.,0.,1.));
#16416=DIRECTION('center_axis',(0.,0.,1.));
#16417=DIRECTION('ref_axis',(-1.,0.,0.));
#16418=DIRECTION('',(0.,0.,1.));
#16419=DIRECTION('center_axis',(0.,0.,1.));
#16420=DIRECTION('ref_axis',(-1.,0.,0.));
#16421=DIRECTION('',(0.,0.,1.));
#16422=DIRECTION('center_axis',(0.,0.,1.));
#16423=DIRECTION('ref_axis',(-1.,0.,0.));
#16424=DIRECTION('',(0.,0.,1.));
#16425=DIRECTION('center_axis',(0.,0.,1.));
#16426=DIRECTION('ref_axis',(-1.,0.,0.));
#16427=DIRECTION('',(0.,0.,1.));
#16428=DIRECTION('center_axis',(0.,0.,1.));
#16429=DIRECTION('ref_axis',(-1.,0.,0.));
#16430=DIRECTION('',(0.,0.,1.));
#16431=DIRECTION('center_axis',(0.,0.,1.));
#16432=DIRECTION('ref_axis',(-1.,0.,0.));
#16433=DIRECTION('',(0.,0.,1.));
#16434=DIRECTION('center_axis',(0.,0.,1.));
#16435=DIRECTION('ref_axis',(-1.,0.,0.));
#16436=DIRECTION('',(0.,0.,1.));
#16437=DIRECTION('center_axis',(0.,0.,1.));
#16438=DIRECTION('ref_axis',(-1.,0.,0.));
#16439=DIRECTION('',(0.,0.,1.));
#16440=DIRECTION('center_axis',(0.,0.,1.));
#16441=DIRECTION('ref_axis',(-1.,0.,0.));
#16442=DIRECTION('',(0.,0.,1.));
#16443=DIRECTION('center_axis',(0.,0.,1.));
#16444=DIRECTION('ref_axis',(-1.,0.,0.));
#16445=DIRECTION('',(0.,0.,1.));
#16446=DIRECTION('center_axis',(0.,0.,1.));
#16447=DIRECTION('ref_axis',(-1.,0.,0.));
#16448=DIRECTION('',(0.,0.,1.));
#16449=DIRECTION('center_axis',(0.,0.,1.));
#16450=DIRECTION('ref_axis',(-1.,0.,0.));
#16451=DIRECTION('',(0.,0.,1.));
#16452=DIRECTION('center_axis',(0.,0.,1.));
#16453=DIRECTION('ref_axis',(-1.,0.,0.));
#16454=DIRECTION('',(0.,0.,1.));
#16455=DIRECTION('center_axis',(0.,0.,1.));
#16456=DIRECTION('ref_axis',(-1.,0.,0.));
#16457=DIRECTION('',(0.,0.,1.));
#16458=DIRECTION('center_axis',(0.,0.,1.));
#16459=DIRECTION('ref_axis',(-1.,0.,0.));
#16460=DIRECTION('',(0.,0.,1.));
#16461=DIRECTION('center_axis',(0.,0.,1.));
#16462=DIRECTION('ref_axis',(-1.,0.,0.));
#16463=DIRECTION('',(0.,0.,1.));
#16464=DIRECTION('center_axis',(0.,0.,1.));
#16465=DIRECTION('ref_axis',(-1.,0.,0.));
#16466=DIRECTION('',(0.,0.,1.));
#16467=DIRECTION('center_axis',(0.,0.,1.));
#16468=DIRECTION('ref_axis',(-1.,0.,0.));
#16469=DIRECTION('',(0.,0.,1.));
#16470=DIRECTION('center_axis',(0.,0.,1.));
#16471=DIRECTION('ref_axis',(-1.,0.,0.));
#16472=DIRECTION('',(0.,0.,1.));
#16473=DIRECTION('center_axis',(0.,0.,1.));
#16474=DIRECTION('ref_axis',(-1.,0.,0.));
#16475=DIRECTION('',(0.,0.,1.));
#16476=DIRECTION('center_axis',(0.,0.,1.));
#16477=DIRECTION('ref_axis',(-0.938097369934915,-0.346371656636617,0.));
#16478=DIRECTION('',(0.,0.,1.));
#16479=DIRECTION('center_axis',(0.,0.,-1.));
#16480=DIRECTION('ref_axis',(-1.,0.,0.));
#16481=DIRECTION('center_axis',(0.,0.,1.));
#16482=DIRECTION('ref_axis',(-0.793344496203991,0.608772954674266,0.));
#16483=DIRECTION('',(-1.22464679914735E-16,4.47534497895031E-29,1.));
#16484=DIRECTION('center_axis',(0.,0.,-1.));
#16485=DIRECTION('ref_axis',(-1.,3.65562114876707E-13,0.));
#16486=DIRECTION('center_axis',(0.,0.,1.));
#16487=DIRECTION('ref_axis',(-1.,3.65562114876707E-13,0.));
#16488=DIRECTION('',(-1.22464679914735E-16,4.47534497895031E-29,1.));
#16489=DIRECTION('center_axis',(0.,0.,1.));
#16490=DIRECTION('ref_axis',(-1.,3.65562114876707E-13,0.));
#16491=DIRECTION('',(-1.22464679914735E-16,4.47534497895031E-29,1.));
#16492=DIRECTION('center_axis',(0.,0.,1.));
#16493=DIRECTION('ref_axis',(-1.,3.65562114876707E-13,0.));
#16494=DIRECTION('',(-1.22464679914735E-16,4.47534497895031E-29,1.));
#16495=DIRECTION('center_axis',(0.,0.,1.));
#16496=DIRECTION('ref_axis',(-1.,3.65562114876707E-13,0.));
#16497=DIRECTION('',(-1.22464679914735E-16,4.47534497895031E-29,1.));
#16498=DIRECTION('center_axis',(0.,0.,1.));
#16499=DIRECTION('ref_axis',(-1.,3.65562114876707E-13,0.));
#16500=DIRECTION('',(-1.22464679914735E-16,4.47534497895031E-29,1.));
#16501=DIRECTION('center_axis',(0.,0.,1.));
#16502=DIRECTION('ref_axis',(-1.,3.65562114876707E-13,0.));
#16503=DIRECTION('',(-1.22464679914735E-16,4.47534497895031E-29,1.));
#16504=DIRECTION('center_axis',(0.,0.,1.));
#16505=DIRECTION('ref_axis',(-1.,3.65562114876707E-13,0.));
#16506=DIRECTION('',(-1.22464679914735E-16,4.47534497895031E-29,1.));
#16507=DIRECTION('center_axis',(0.,0.,1.));
#16508=DIRECTION('ref_axis',(-1.,3.65562114876707E-13,0.));
#16509=DIRECTION('',(-1.22464679914735E-16,4.47534497895031E-29,1.));
#16510=DIRECTION('center_axis',(0.,0.,1.));
#16511=DIRECTION('ref_axis',(-1.,3.65562114876707E-13,0.));
#16512=DIRECTION('',(-1.22464679914735E-16,4.47534497895031E-29,1.));
#16513=DIRECTION('center_axis',(0.,0.,1.));
#16514=DIRECTION('ref_axis',(-1.,3.65562114876707E-13,0.));
#16515=DIRECTION('',(-1.22464679914735E-16,4.47534497895031E-29,1.));
#16516=DIRECTION('center_axis',(0.,0.,1.));
#16517=DIRECTION('ref_axis',(-1.,3.65562114876707E-13,0.));
#16518=DIRECTION('',(-1.22464679914735E-16,4.47534497895031E-29,1.));
#16519=DIRECTION('center_axis',(0.,0.,1.));
#16520=DIRECTION('ref_axis',(-1.,3.65562114876707E-13,0.));
#16521=DIRECTION('',(-1.22464679914735E-16,4.47534497895031E-29,1.));
#16522=DIRECTION('center_axis',(0.,0.,1.));
#16523=DIRECTION('ref_axis',(-1.,3.65562114876707E-13,0.));
#16524=DIRECTION('',(-1.22464679914735E-16,4.47534497895031E-29,1.));
#16525=DIRECTION('center_axis',(0.,0.,1.));
#16526=DIRECTION('ref_axis',(-1.,3.65562114876707E-13,0.));
#16527=DIRECTION('',(-1.22464679914735E-16,4.47534497895031E-29,1.));
#16528=DIRECTION('center_axis',(0.,0.,1.));
#16529=DIRECTION('ref_axis',(-1.,3.65562114876707E-13,0.));
#16530=DIRECTION('',(-1.22464679914735E-16,4.47534497895031E-29,1.));
#16531=DIRECTION('center_axis',(0.,0.,1.));
#16532=DIRECTION('ref_axis',(-1.,3.65562114876707E-13,0.));
#16533=DIRECTION('',(-1.22464679914735E-16,4.47534497895031E-29,1.));
#16534=DIRECTION('center_axis',(0.,0.,1.));
#16535=DIRECTION('ref_axis',(-1.,3.65562114876707E-13,0.));
#16536=DIRECTION('',(-1.22464679914735E-16,4.47534497895031E-29,1.));
#16537=DIRECTION('center_axis',(0.,0.,1.));
#16538=DIRECTION('ref_axis',(-1.,3.65562114876707E-13,0.));
#16539=DIRECTION('',(-1.22464679914735E-16,4.47534497895031E-29,1.));
#16540=DIRECTION('center_axis',(0.,0.,1.));
#16541=DIRECTION('ref_axis',(-1.,3.65562114876707E-13,0.));
#16542=DIRECTION('',(-1.22464679914735E-16,4.47534497895031E-29,1.));
#16543=DIRECTION('center_axis',(0.,0.,1.));
#16544=DIRECTION('ref_axis',(-1.,3.65562114876707E-13,0.));
#16545=DIRECTION('',(-1.22464679914735E-16,4.47534497895031E-29,1.));
#16546=DIRECTION('center_axis',(0.,0.,1.));
#16547=DIRECTION('ref_axis',(-1.,3.65562114876707E-13,0.));
#16548=DIRECTION('',(-1.22464679914735E-16,4.47534497895031E-29,1.));
#16549=DIRECTION('center_axis',(0.,0.,1.));
#16550=DIRECTION('ref_axis',(-1.,3.65562114876707E-13,0.));
#16551=DIRECTION('',(-1.22464679914735E-16,4.47534497895031E-29,1.));
#16552=DIRECTION('center_axis',(0.,0.,1.));
#16553=DIRECTION('ref_axis',(-1.,3.65562114876707E-13,0.));
#16554=DIRECTION('',(-1.22464679914735E-16,4.47534497895031E-29,1.));
#16555=DIRECTION('center_axis',(0.,0.,1.));
#16556=DIRECTION('ref_axis',(-1.,3.65562114876707E-13,0.));
#16557=DIRECTION('',(-1.22464679914735E-16,4.47534497895031E-29,1.));
#16558=DIRECTION('center_axis',(0.,0.,1.));
#16559=DIRECTION('ref_axis',(-1.,3.65562114876707E-13,0.));
#16560=DIRECTION('',(-1.22464679914735E-16,4.47534497895031E-29,1.));
#16561=DIRECTION('center_axis',(0.,0.,1.));
#16562=DIRECTION('ref_axis',(-1.,3.65562114876707E-13,0.));
#16563=DIRECTION('',(-1.22464679914735E-16,4.47534497895031E-29,1.));
#16564=DIRECTION('center_axis',(0.,0.,1.));
#16565=DIRECTION('ref_axis',(-1.,3.65562114876707E-13,0.));
#16566=DIRECTION('',(-1.22464679914735E-16,4.47534497895031E-29,1.));
#16567=DIRECTION('center_axis',(0.,0.,1.));
#16568=DIRECTION('ref_axis',(-1.,3.65562114876707E-13,0.));
#16569=DIRECTION('',(-1.22464679914735E-16,4.47534497895031E-29,1.));
#16570=DIRECTION('center_axis',(0.,0.,1.));
#16571=DIRECTION('ref_axis',(-1.,3.65562114876707E-13,0.));
#16572=DIRECTION('',(-1.22464679914735E-16,4.47534497895031E-29,1.));
#16573=DIRECTION('center_axis',(0.,0.,1.));
#16574=DIRECTION('ref_axis',(-1.,3.65562114876707E-13,0.));
#16575=DIRECTION('',(-1.22464679914735E-16,4.47534497895031E-29,1.));
#16576=DIRECTION('center_axis',(0.,0.,1.));
#16577=DIRECTION('ref_axis',(-1.,3.65562114876707E-13,0.));
#16578=DIRECTION('',(-1.22464679914735E-16,4.47534497895031E-29,1.));
#16579=DIRECTION('center_axis',(0.,0.,1.));
#16580=DIRECTION('ref_axis',(-1.,3.65562114876707E-13,0.));
#16581=DIRECTION('',(-1.22464679914735E-16,4.47534497895031E-29,1.));
#16582=DIRECTION('center_axis',(0.,0.,1.));
#16583=DIRECTION('ref_axis',(-1.,3.65562114876707E-13,0.));
#16584=DIRECTION('',(-1.22464679914735E-16,4.47534497895031E-29,1.));
#16585=DIRECTION('center_axis',(0.,0.,1.));
#16586=DIRECTION('ref_axis',(-1.,3.65562114876707E-13,0.));
#16587=DIRECTION('',(-1.22464679914735E-16,4.47534497895031E-29,1.));
#16588=DIRECTION('center_axis',(0.,0.,1.));
#16589=DIRECTION('ref_axis',(-1.,3.65562114876707E-13,0.));
#16590=DIRECTION('',(-1.22464679914735E-16,4.47534497895031E-29,1.));
#16591=DIRECTION('center_axis',(0.,0.,1.));
#16592=DIRECTION('ref_axis',(-1.,3.65562114876707E-13,0.));
#16593=DIRECTION('',(-1.22464679914735E-16,4.47534497895031E-29,1.));
#16594=DIRECTION('center_axis',(0.,0.,1.));
#16595=DIRECTION('ref_axis',(-1.,3.65562114876707E-13,0.));
#16596=DIRECTION('',(-1.22464679914735E-16,4.47534497895031E-29,1.));
#16597=DIRECTION('center_axis',(0.,0.,1.));
#16598=DIRECTION('ref_axis',(-1.,3.65562114876707E-13,0.));
#16599=DIRECTION('',(-1.22464679914735E-16,4.47534497895031E-29,1.));
#16600=DIRECTION('center_axis',(0.,0.,1.));
#16601=DIRECTION('ref_axis',(0.608777863132373,-0.793340729674193,0.));
#16602=DIRECTION('',(-1.22464679914735E-16,4.47534497895031E-29,1.));
#16603=DIRECTION('center_axis',(0.,0.,1.));
#16604=DIRECTION('ref_axis',(-1.,3.65562114876707E-13,0.));
#16605=DIRECTION('center_axis',(0.,0.,1.));
#16606=DIRECTION('ref_axis',(1.,0.,0.));
#16607=DIRECTION('center_axis',(0.,0.,1.));
#16608=DIRECTION('ref_axis',(-1.,3.65562114876707E-13,0.));
#16609=DIRECTION('center_axis',(0.,0.,1.));
#16610=DIRECTION('ref_axis',(-1.,0.,0.));
#16611=DIRECTION('center_axis',(0.,0.,1.));
#16612=DIRECTION('ref_axis',(-1.,0.,0.));
#16613=DIRECTION('center_axis',(0.,0.,-1.));
#16614=DIRECTION('ref_axis',(1.,0.,0.));
#16615=DIRECTION('center_axis',(0.,0.,1.));
#16616=DIRECTION('ref_axis',(1.,0.,0.));
#16617=DIRECTION('center_axis',(0.,0.,-1.));
#16618=DIRECTION('ref_axis',(1.,3.16070290694603E-14,0.));
#16619=DIRECTION('center_axis',(0.,0.,-1.));
#16620=DIRECTION('ref_axis',(1.,0.,0.));
#16621=DIRECTION('center_axis',(0.,0.,-1.));
#16622=DIRECTION('ref_axis',(1.,0.,0.));
#16623=DIRECTION('center_axis',(0.,0.,1.));
#16624=DIRECTION('ref_axis',(1.,0.,0.));
#16625=DIRECTION('center_axis',(0.,0.,1.));
#16626=DIRECTION('ref_axis',(0.707106781186548,-0.707106781186547,0.));
#16627=DIRECTION('center_axis',(0.,0.,-1.));
#16628=DIRECTION('ref_axis',(0.707106781186548,-0.707106781186547,0.));
#16629=DIRECTION('',(0.,0.,-1.));
#16630=DIRECTION('center_axis',(0.,0.,1.));
#16631=DIRECTION('ref_axis',(0.707106781186548,-0.707106781186547,0.));
#16632=DIRECTION('',(0.,0.,1.));
#16633=DIRECTION('center_axis',(0.,-1.,0.));
#16634=DIRECTION('ref_axis',(1.,0.,0.));
#16635=DIRECTION('',(1.,0.,0.));
#16636=DIRECTION('',(0.,0.,1.));
#16637=DIRECTION('',(-1.,0.,0.));
#16638=DIRECTION('center_axis',(0.,0.,1.));
#16639=DIRECTION('ref_axis',(1.,0.,0.));
#16640=DIRECTION('',(0.,1.,0.));
#16641=DIRECTION('center_axis',(0.,0.,1.));
#16642=DIRECTION('ref_axis',(-0.707106781186548,0.707106781186547,0.));
#16643=DIRECTION('',(1.,0.,0.));
#16644=DIRECTION('center_axis',(0.,0.,1.));
#16645=DIRECTION('ref_axis',(0.707106781186547,0.707106781186548,0.));
#16646=DIRECTION('',(0.,-1.,0.));
#16647=DIRECTION('center_axis',(0.,0.,1.));
#16648=DIRECTION('ref_axis',(0.707106781186548,-0.707106781186548,0.));
#16649=DIRECTION('',(-1.,0.,0.));
#16650=DIRECTION('center_axis',(0.,0.,1.));
#16651=DIRECTION('ref_axis',(-0.707106781186548,-0.707106781186548,0.));
#16652=DIRECTION('',(0.,1.,0.));
#16653=DIRECTION('center_axis',(0.,0.,-1.));
#16654=DIRECTION('ref_axis',(0.707106781186548,0.707106781186547,0.));
#16655=DIRECTION('',(-1.,0.,0.));
#16656=DIRECTION('center_axis',(0.,0.,-1.));
#16657=DIRECTION('ref_axis',(-0.707106781186548,0.707106781186547,0.));
#16658=DIRECTION('',(0.,-1.,0.));
#16659=DIRECTION('center_axis',(0.,0.,-1.));
#16660=DIRECTION('ref_axis',(-0.707106781186548,-0.707106781186548,0.));
#16661=DIRECTION('',(1.,0.,0.));
#16662=DIRECTION('center_axis',(0.,0.,-1.));
#16663=DIRECTION('ref_axis',(0.707106781186547,-0.707106781186548,0.));
#16664=DIRECTION('',(0.,1.,0.));
#16665=DIRECTION('center_axis',(0.,0.,-1.));
#16666=DIRECTION('ref_axis',(0.707106781186547,0.707106781186548,0.));
#16667=DIRECTION('',(-1.,0.,0.));
#16668=DIRECTION('center_axis',(0.,0.,1.));
#16669=DIRECTION('ref_axis',(-0.707106781186547,-0.707106781186548,0.));
#16670=DIRECTION('',(0.,1.,0.));
#16671=DIRECTION('center_axis',(0.,0.,1.));
#16672=DIRECTION('ref_axis',(-0.707106781186548,0.707106781186547,0.));
#16673=DIRECTION('',(1.,0.,0.));
#16674=DIRECTION('center_axis',(0.,0.,1.));
#16675=DIRECTION('ref_axis',(0.707106781186548,0.707106781186548,0.));
#16676=DIRECTION('',(0.,-1.,0.));
#16677=DIRECTION('center_axis',(0.,0.,1.));
#16678=DIRECTION('ref_axis',(0.707106781186548,-0.707106781186548,0.));
#16679=DIRECTION('',(-1.,0.,0.));
#16680=DIRECTION('center_axis',(0.,0.,-1.));
#16681=DIRECTION('ref_axis',(-0.707106781186547,0.707106781186548,0.));
#16682=DIRECTION('',(0.,-1.,0.));
#16683=DIRECTION('center_axis',(0.,0.,-1.));
#16684=DIRECTION('ref_axis',(-0.707106781186547,-0.707106781186548,0.));
#16685=DIRECTION('',(1.,0.,0.));
#16686=DIRECTION('center_axis',(0.,0.,-1.));
#16687=DIRECTION('ref_axis',(0.707106781186548,-0.707106781186548,0.));
#16688=DIRECTION('',(0.,1.,0.));
#16689=DIRECTION('center_axis',(0.,0.,-1.));
#16690=DIRECTION('ref_axis',(0.707106781186548,0.707106781186547,0.));
#16691=DIRECTION('',(-1.,0.,0.));
#16692=DIRECTION('center_axis',(0.,0.,-1.));
#16693=DIRECTION('ref_axis',(-0.707106781186548,0.707106781186547,0.));
#16694=DIRECTION('',(0.,-1.,0.));
#16695=DIRECTION('center_axis',(0.,0.,1.));
#16696=DIRECTION('ref_axis',(0.707106781186548,-0.707106781186547,0.));
#16697=DIRECTION('',(-1.,0.,0.));
#16698=DIRECTION('center_axis',(0.,0.,1.));
#16699=DIRECTION('ref_axis',(-0.707106781186547,-0.707106781186548,0.));
#16700=DIRECTION('',(0.,1.,0.));
#16701=DIRECTION('center_axis',(0.,0.,1.));
#16702=DIRECTION('ref_axis',(-0.707106781186548,0.707106781186548,0.));
#16703=DIRECTION('',(1.,0.,0.));
#16704=DIRECTION('center_axis',(0.,0.,1.));
#16705=DIRECTION('ref_axis',(0.707106781186548,0.707106781186548,0.));
#16706=DIRECTION('',(0.,-1.,0.));
#16707=DIRECTION('center_axis',(0.,0.,-1.));
#16708=DIRECTION('ref_axis',(-0.707106781186548,-0.707106781186547,0.));
#16709=DIRECTION('',(1.,0.,0.));
#16710=DIRECTION('center_axis',(0.,0.,-1.));
#16711=DIRECTION('ref_axis',(0.707106781186548,-0.707106781186547,0.));
#16712=DIRECTION('',(0.,1.,0.));
#16713=DIRECTION('center_axis',(0.,0.,-1.));
#16714=DIRECTION('ref_axis',(0.707106781186548,0.707106781186548,0.));
#16715=DIRECTION('',(-1.,0.,0.));
#16716=DIRECTION('center_axis',(0.,0.,-1.));
#16717=DIRECTION('ref_axis',(-0.707106781186547,0.707106781186548,0.));
#16718=DIRECTION('',(0.,-1.,0.));
#16719=DIRECTION('center_axis',(0.,0.,-1.));
#16720=DIRECTION('ref_axis',(-0.707106781186547,-0.707106781186548,0.));
#16721=DIRECTION('',(1.,0.,0.));
#16722=DIRECTION('center_axis',(0.,0.,1.));
#16723=DIRECTION('ref_axis',(0.707106781186547,0.707106781186548,0.));
#16724=DIRECTION('',(0.,-1.,0.));
#16725=DIRECTION('center_axis',(0.,0.,1.));
#16726=DIRECTION('ref_axis',(0.707106781186548,-0.707106781186547,0.));
#16727=DIRECTION('',(-1.,0.,0.));
#16728=DIRECTION('center_axis',(0.,0.,1.));
#16729=DIRECTION('ref_axis',(-0.707106781186548,-0.707106781186548,0.));
#16730=DIRECTION('',(0.,1.,0.));
#16731=DIRECTION('center_axis',(0.,0.,1.));
#16732=DIRECTION('ref_axis',(-0.707106781186548,0.707106781186548,0.));
#16733=DIRECTION('',(1.,0.,0.));
#16734=DIRECTION('center_axis',(0.,0.,-1.));
#16735=DIRECTION('ref_axis',(0.707106781186547,-0.707106781186548,0.));
#16736=DIRECTION('',(0.,1.,0.));
#16737=DIRECTION('center_axis',(0.,0.,-1.));
#16738=DIRECTION('ref_axis',(0.707106781186547,0.707106781186548,0.));
#16739=DIRECTION('',(-1.,0.,0.));
#16740=DIRECTION('center_axis',(0.,0.,-1.));
#16741=DIRECTION('ref_axis',(-0.707106781186548,0.707106781186548,0.));
#16742=DIRECTION('',(0.,-1.,0.));
#16743=DIRECTION('center_axis',(0.,0.,-1.));
#16744=DIRECTION('ref_axis',(-0.707106781186548,-0.707106781186547,0.));
#16745=DIRECTION('center_axis',(0.,0.,-1.));
#16746=DIRECTION('ref_axis',(1.,0.,0.));
#16747=DIRECTION('center_axis',(0.,0.,-1.));
#16748=DIRECTION('ref_axis',(1.,0.,0.));
#16749=DIRECTION('center_axis',(0.,0.,-1.));
#16750=DIRECTION('ref_axis',(1.,0.,0.));
#16751=DIRECTION('center_axis',(0.,0.,-1.));
#16752=DIRECTION('ref_axis',(1.,0.,0.));
#16753=DIRECTION('center_axis',(0.,0.,1.));
#16754=DIRECTION('ref_axis',(-0.707106781186548,0.707106781186547,0.));
#16755=DIRECTION('center_axis',(0.,0.,-1.));
#16756=DIRECTION('ref_axis',(-0.707106781186548,0.707106781186547,0.));
#16757=DIRECTION('',(0.,0.,1.));
#16758=DIRECTION('',(0.,0.,-1.));
#16759=DIRECTION('center_axis',(0.,-1.,0.));
#16760=DIRECTION('ref_axis',(1.,0.,0.));
#16761=DIRECTION('',(-1.,0.,0.));
#16762=DIRECTION('',(0.,0.,-1.));
#16763=DIRECTION('center_axis',(0.,0.,1.));
#16764=DIRECTION('ref_axis',(0.707106781186547,0.707106781186548,0.));
#16765=DIRECTION('center_axis',(0.,0.,-1.));
#16766=DIRECTION('ref_axis',(0.707106781186547,0.707106781186548,0.));
#16767=DIRECTION('',(0.,0.,1.));
#16768=DIRECTION('center_axis',(-1.,0.,0.));
#16769=DIRECTION('ref_axis',(0.,-1.,0.));
#16770=DIRECTION('',(0.,1.,0.));
#16771=DIRECTION('',(0.,0.,-1.));
#16772=DIRECTION('center_axis',(0.,0.,1.));
#16773=DIRECTION('ref_axis',(0.707106781186548,-0.707106781186548,0.));
#16774=DIRECTION('center_axis',(0.,0.,-1.));
#16775=DIRECTION('ref_axis',(0.707106781186548,-0.707106781186548,0.));
#16776=DIRECTION('',(0.,0.,1.));
#16777=DIRECTION('center_axis',(0.,1.,0.));
#16778=DIRECTION('ref_axis',(-1.,0.,0.));
#16779=DIRECTION('',(1.,0.,0.));
#16780=DIRECTION('',(0.,0.,-1.));
#16781=DIRECTION('center_axis',(0.,0.,1.));
#16782=DIRECTION('ref_axis',(-0.707106781186548,-0.707106781186548,0.));
#16783=DIRECTION('center_axis',(0.,0.,-1.));
#16784=DIRECTION('ref_axis',(-0.707106781186548,-0.707106781186548,0.));
#16785=DIRECTION('',(0.,0.,1.));
#16786=DIRECTION('center_axis',(1.,0.,0.));
#16787=DIRECTION('ref_axis',(0.,1.,0.));
#16788=DIRECTION('',(0.,-1.,0.));
#16789=DIRECTION('',(0.,0.,-1.));
#16790=DIRECTION('center_axis',(0.,0.,1.));
#16791=DIRECTION('ref_axis',(0.707106781186548,0.707106781186547,0.));
#16792=DIRECTION('center_axis',(0.,0.,1.));
#16793=DIRECTION('ref_axis',(0.707106781186548,0.707106781186547,0.));
#16794=DIRECTION('',(0.,0.,1.));
#16795=DIRECTION('center_axis',(0.,0.,1.));
#16796=DIRECTION('ref_axis',(-0.707106781186548,0.707106781186547,0.));
#16797=DIRECTION('',(0.,0.,-1.));
#16798=DIRECTION('center_axis',(0.,0.,1.));
#16799=DIRECTION('ref_axis',(-0.707106781186548,0.707106781186547,0.));
#16800=DIRECTION('',(0.,0.,1.));
#16801=DIRECTION('center_axis',(-1.,0.,0.));
#16802=DIRECTION('ref_axis',(0.,-1.,0.));
#16803=DIRECTION('',(0.,1.,0.));
#16804=DIRECTION('',(0.,0.,-1.));
#16805=DIRECTION('center_axis',(0.,0.,1.));
#16806=DIRECTION('ref_axis',(-0.707106781186548,-0.707106781186548,0.));
#16807=DIRECTION('center_axis',(0.,0.,1.));
#16808=DIRECTION('ref_axis',(-0.707106781186548,-0.707106781186548,0.));
#16809=DIRECTION('',(0.,0.,1.));
#16810=DIRECTION('center_axis',(0.,0.,1.));
#16811=DIRECTION('ref_axis',(0.707106781186547,-0.707106781186548,0.));
#16812=DIRECTION('',(0.,0.,-1.));
#16813=DIRECTION('center_axis',(0.,0.,1.));
#16814=DIRECTION('ref_axis',(0.707106781186547,-0.707106781186548,0.));
#16815=DIRECTION('',(0.,0.,1.));
#16816=DIRECTION('center_axis',(1.,0.,0.));
#16817=DIRECTION('ref_axis',(0.,1.,0.));
#16818=DIRECTION('',(0.,-1.,0.));
#16819=DIRECTION('',(0.,0.,-1.));
#16820=DIRECTION('center_axis',(0.,0.,1.));
#16821=DIRECTION('ref_axis',(0.707106781186547,0.707106781186548,0.));
#16822=DIRECTION('center_axis',(0.,0.,1.));
#16823=DIRECTION('ref_axis',(0.707106781186547,0.707106781186548,0.));
#16824=DIRECTION('',(0.,0.,1.));
#16825=DIRECTION('center_axis',(0.,0.,1.));
#16826=DIRECTION('ref_axis',(-0.707106781186547,-0.707106781186548,0.));
#16827=DIRECTION('center_axis',(0.,0.,-1.));
#16828=DIRECTION('ref_axis',(-0.707106781186547,-0.707106781186548,0.));
#16829=DIRECTION('',(0.,0.,1.));
#16830=DIRECTION('',(0.,0.,-1.));
#16831=DIRECTION('center_axis',(1.,0.,0.));
#16832=DIRECTION('ref_axis',(0.,1.,0.));
#16833=DIRECTION('',(0.,-1.,0.));
#16834=DIRECTION('',(0.,0.,-1.));
#16835=DIRECTION('center_axis',(0.,0.,1.));
#16836=DIRECTION('ref_axis',(-0.707106781186548,0.707106781186547,0.));
#16837=DIRECTION('center_axis',(0.,0.,-1.));
#16838=DIRECTION('ref_axis',(-0.707106781186548,0.707106781186547,0.));
#16839=DIRECTION('',(0.,0.,1.));
#16840=DIRECTION('center_axis',(0.,-1.,0.));
#16841=DIRECTION('ref_axis',(1.,0.,0.));
#16842=DIRECTION('',(-1.,0.,0.));
#16843=DIRECTION('',(0.,0.,-1.));
#16844=DIRECTION('center_axis',(0.,0.,1.));
#16845=DIRECTION('ref_axis',(0.707106781186548,0.707106781186548,0.));
#16846=DIRECTION('center_axis',(0.,0.,-1.));
#16847=DIRECTION('ref_axis',(0.707106781186548,0.707106781186548,0.));
#16848=DIRECTION('',(0.,0.,1.));
#16849=DIRECTION('center_axis',(-1.,0.,0.));
#16850=DIRECTION('ref_axis',(0.,-1.,0.));
#16851=DIRECTION('',(0.,1.,0.));
#16852=DIRECTION('',(0.,0.,-1.));
#16853=DIRECTION('center_axis',(0.,0.,1.));
#16854=DIRECTION('ref_axis',(0.707106781186548,-0.707106781186548,0.));
#16855=DIRECTION('center_axis',(0.,0.,-1.));
#16856=DIRECTION('ref_axis',(0.707106781186548,-0.707106781186548,0.));
#16857=DIRECTION('',(0.,0.,1.));
#16858=DIRECTION('center_axis',(0.,1.,0.));
#16859=DIRECTION('ref_axis',(-1.,0.,0.));
#16860=DIRECTION('',(1.,0.,0.));
#16861=DIRECTION('',(0.,0.,-1.));
#16862=DIRECTION('center_axis',(0.,0.,1.));
#16863=DIRECTION('ref_axis',(-0.707106781186547,0.707106781186548,0.));
#16864=DIRECTION('center_axis',(0.,0.,1.));
#16865=DIRECTION('ref_axis',(-0.707106781186547,0.707106781186548,0.));
#16866=DIRECTION('',(0.,0.,1.));
#16867=DIRECTION('center_axis',(0.,0.,1.));
#16868=DIRECTION('ref_axis',(-0.707106781186547,-0.707106781186548,0.));
#16869=DIRECTION('',(0.,0.,-1.));
#16870=DIRECTION('center_axis',(0.,0.,1.));
#16871=DIRECTION('ref_axis',(-0.707106781186547,-0.707106781186548,0.));
#16872=DIRECTION('',(0.,0.,1.));
#16873=DIRECTION('center_axis',(0.,-1.,0.));
#16874=DIRECTION('ref_axis',(1.,0.,0.));
#16875=DIRECTION('',(-1.,0.,0.));
#16876=DIRECTION('',(0.,0.,-1.));
#16877=DIRECTION('center_axis',(0.,0.,1.));
#16878=DIRECTION('ref_axis',(0.707106781186548,-0.707106781186548,0.));
#16879=DIRECTION('center_axis',(0.,0.,1.));
#16880=DIRECTION('ref_axis',(0.707106781186548,-0.707106781186548,0.));
#16881=DIRECTION('',(0.,0.,1.));
#16882=DIRECTION('center_axis',(0.,0.,1.));
#16883=DIRECTION('ref_axis',(0.707106781186548,0.707106781186547,0.));
#16884=DIRECTION('',(0.,0.,-1.));
#16885=DIRECTION('center_axis',(0.,0.,1.));
#16886=DIRECTION('ref_axis',(0.707106781186548,0.707106781186547,0.));
#16887=DIRECTION('',(0.,0.,1.));
#16888=DIRECTION('center_axis',(0.,1.,0.));
#16889=DIRECTION('ref_axis',(-1.,0.,0.));
#16890=DIRECTION('',(1.,0.,0.));
#16891=DIRECTION('',(0.,0.,-1.));
#16892=DIRECTION('center_axis',(0.,0.,1.));
#16893=DIRECTION('ref_axis',(-0.707106781186548,0.707106781186547,0.));
#16894=DIRECTION('center_axis',(0.,0.,1.));
#16895=DIRECTION('ref_axis',(-0.707106781186548,0.707106781186547,0.));
#16896=DIRECTION('',(0.,0.,1.));
#16897=DIRECTION('center_axis',(0.,0.,1.));
#16898=DIRECTION('ref_axis',(0.707106781186548,-0.707106781186547,0.));
#16899=DIRECTION('center_axis',(0.,0.,-1.));
#16900=DIRECTION('ref_axis',(0.707106781186548,-0.707106781186547,0.));
#16901=DIRECTION('',(0.,0.,1.));
#16902=DIRECTION('',(0.,0.,-1.));
#16903=DIRECTION('center_axis',(0.,1.,0.));
#16904=DIRECTION('ref_axis',(-1.,0.,0.));
#16905=DIRECTION('',(1.,0.,0.));
#16906=DIRECTION('',(0.,0.,-1.));
#16907=DIRECTION('center_axis',(0.,0.,1.));
#16908=DIRECTION('ref_axis',(-0.707106781186547,-0.707106781186548,0.));
#16909=DIRECTION('center_axis',(0.,0.,-1.));
#16910=DIRECTION('ref_axis',(-0.707106781186547,-0.707106781186548,0.));
#16911=DIRECTION('',(0.,0.,1.));
#16912=DIRECTION('center_axis',(1.,0.,0.));
#16913=DIRECTION('ref_axis',(0.,1.,0.));
#16914=DIRECTION('',(0.,-1.,0.));
#16915=DIRECTION('',(0.,0.,-1.));
#16916=DIRECTION('center_axis',(0.,0.,1.));
#16917=DIRECTION('ref_axis',(-0.707106781186548,0.707106781186548,0.));
#16918=DIRECTION('center_axis',(0.,0.,-1.));
#16919=DIRECTION('ref_axis',(-0.707106781186548,0.707106781186548,0.));
#16920=DIRECTION('',(0.,0.,1.));
#16921=DIRECTION('center_axis',(0.,-1.,0.));
#16922=DIRECTION('ref_axis',(1.,0.,0.));
#16923=DIRECTION('',(-1.,0.,0.));
#16924=DIRECTION('',(0.,0.,-1.));
#16925=DIRECTION('center_axis',(0.,0.,1.));
#16926=DIRECTION('ref_axis',(0.707106781186548,0.707106781186548,0.));
#16927=DIRECTION('center_axis',(0.,0.,-1.));
#16928=DIRECTION('ref_axis',(0.707106781186548,0.707106781186548,0.));
#16929=DIRECTION('',(0.,0.,1.));
#16930=DIRECTION('center_axis',(-1.,0.,0.));
#16931=DIRECTION('ref_axis',(0.,-1.,0.));
#16932=DIRECTION('',(0.,1.,0.));
#16933=DIRECTION('',(0.,0.,-1.));
#16934=DIRECTION('center_axis',(0.,0.,1.));
#16935=DIRECTION('ref_axis',(-0.707106781186548,-0.707106781186547,0.));
#16936=DIRECTION('center_axis',(0.,0.,1.));
#16937=DIRECTION('ref_axis',(-0.707106781186548,-0.707106781186547,0.));
#16938=DIRECTION('',(0.,0.,1.));
#16939=DIRECTION('center_axis',(0.,0.,1.));
#16940=DIRECTION('ref_axis',(0.707106781186548,-0.707106781186547,0.));
#16941=DIRECTION('',(0.,0.,-1.));
#16942=DIRECTION('center_axis',(0.,0.,1.));
#16943=DIRECTION('ref_axis',(0.707106781186548,-0.707106781186547,0.));
#16944=DIRECTION('',(0.,0.,1.));
#16945=DIRECTION('center_axis',(1.,0.,0.));
#16946=DIRECTION('ref_axis',(0.,1.,0.));
#16947=DIRECTION('',(0.,-1.,0.));
#16948=DIRECTION('',(0.,0.,-1.));
#16949=DIRECTION('center_axis',(0.,0.,1.));
#16950=DIRECTION('ref_axis',(0.707106781186548,0.707106781186548,0.));
#16951=DIRECTION('center_axis',(0.,0.,1.));
#16952=DIRECTION('ref_axis',(0.707106781186548,0.707106781186548,0.));
#16953=DIRECTION('',(0.,0.,1.));
#16954=DIRECTION('center_axis',(0.,0.,1.));
#16955=DIRECTION('ref_axis',(-0.707106781186547,0.707106781186548,0.));
#16956=DIRECTION('',(0.,0.,-1.));
#16957=DIRECTION('center_axis',(0.,0.,1.));
#16958=DIRECTION('ref_axis',(-0.707106781186547,0.707106781186548,0.));
#16959=DIRECTION('',(0.,0.,1.));
#16960=DIRECTION('center_axis',(-1.,0.,0.));
#16961=DIRECTION('ref_axis',(0.,-1.,0.));
#16962=DIRECTION('',(0.,1.,0.));
#16963=DIRECTION('',(0.,0.,-1.));
#16964=DIRECTION('center_axis',(0.,0.,1.));
#16965=DIRECTION('ref_axis',(-0.707106781186547,-0.707106781186548,0.));
#16966=DIRECTION('center_axis',(0.,0.,1.));
#16967=DIRECTION('ref_axis',(-0.707106781186547,-0.707106781186548,0.));
#16968=DIRECTION('',(0.,0.,1.));
#16969=DIRECTION('center_axis',(0.,0.,1.));
#16970=DIRECTION('ref_axis',(0.707106781186547,0.707106781186548,0.));
#16971=DIRECTION('center_axis',(0.,0.,-1.));
#16972=DIRECTION('ref_axis',(0.707106781186547,0.707106781186548,0.));
#16973=DIRECTION('',(0.,0.,1.));
#16974=DIRECTION('',(0.,0.,-1.));
#16975=DIRECTION('center_axis',(-1.,0.,0.));
#16976=DIRECTION('ref_axis',(0.,-1.,0.));
#16977=DIRECTION('',(0.,1.,0.));
#16978=DIRECTION('',(0.,0.,-1.));
#16979=DIRECTION('center_axis',(0.,0.,1.));
#16980=DIRECTION('ref_axis',(0.707106781186548,-0.707106781186547,0.));
#16981=DIRECTION('center_axis',(0.,0.,-1.));
#16982=DIRECTION('ref_axis',(0.707106781186548,-0.707106781186547,0.));
#16983=DIRECTION('',(0.,0.,1.));
#16984=DIRECTION('center_axis',(0.,1.,0.));
#16985=DIRECTION('ref_axis',(-1.,0.,0.));
#16986=DIRECTION('',(1.,0.,0.));
#16987=DIRECTION('',(0.,0.,-1.));
#16988=DIRECTION('center_axis',(0.,0.,1.));
#16989=DIRECTION('ref_axis',(-0.707106781186548,-0.707106781186548,0.));
#16990=DIRECTION('center_axis',(0.,0.,-1.));
#16991=DIRECTION('ref_axis',(-0.707106781186548,-0.707106781186548,0.));
#16992=DIRECTION('',(0.,0.,1.));
#16993=DIRECTION('center_axis',(1.,0.,0.));
#16994=DIRECTION('ref_axis',(0.,1.,0.));
#16995=DIRECTION('',(0.,-1.,0.));
#16996=DIRECTION('',(0.,0.,-1.));
#16997=DIRECTION('center_axis',(0.,0.,1.));
#16998=DIRECTION('ref_axis',(-0.707106781186548,0.707106781186548,0.));
#16999=DIRECTION('center_axis',(0.,0.,-1.));
#17000=DIRECTION('ref_axis',(-0.707106781186548,0.707106781186548,0.));
#17001=DIRECTION('',(0.,0.,1.));
#17002=DIRECTION('center_axis',(0.,-1.,0.));
#17003=DIRECTION('ref_axis',(1.,0.,0.));
#17004=DIRECTION('',(-1.,0.,0.));
#17005=DIRECTION('',(0.,0.,-1.));
#17006=DIRECTION('center_axis',(0.,0.,1.));
#17007=DIRECTION('ref_axis',(0.707106781186547,-0.707106781186548,0.));
#17008=DIRECTION('center_axis',(0.,0.,1.));
#17009=DIRECTION('ref_axis',(0.707106781186547,-0.707106781186548,0.));
#17010=DIRECTION('',(0.,0.,1.));
#17011=DIRECTION('center_axis',(0.,0.,1.));
#17012=DIRECTION('ref_axis',(0.707106781186547,0.707106781186548,0.));
#17013=DIRECTION('',(0.,0.,-1.));
#17014=DIRECTION('center_axis',(0.,0.,1.));
#17015=DIRECTION('ref_axis',(0.707106781186547,0.707106781186548,0.));
#17016=DIRECTION('',(0.,0.,1.));
#17017=DIRECTION('center_axis',(0.,1.,0.));
#17018=DIRECTION('ref_axis',(-1.,0.,0.));
#17019=DIRECTION('',(1.,0.,0.));
#17020=DIRECTION('',(0.,0.,-1.));
#17021=DIRECTION('center_axis',(0.,0.,1.));
#17022=DIRECTION('ref_axis',(-0.707106781186548,0.707106781186548,0.));
#17023=DIRECTION('center_axis',(0.,0.,1.));
#17024=DIRECTION('ref_axis',(-0.707106781186548,0.707106781186548,0.));
#17025=DIRECTION('',(0.,0.,1.));
#17026=DIRECTION('center_axis',(0.,0.,1.));
#17027=DIRECTION('ref_axis',(-0.707106781186548,-0.707106781186547,0.));
#17028=DIRECTION('',(0.,0.,-1.));
#17029=DIRECTION('center_axis',(0.,0.,1.));
#17030=DIRECTION('ref_axis',(-0.707106781186548,-0.707106781186547,0.));
#17031=DIRECTION('center_axis',(0.,0.,1.));
#17032=DIRECTION('ref_axis',(1.,0.,0.));
#17033=DIRECTION('',(0.,0.,-1.));
#17034=DIRECTION('center_axis',(0.,0.,-1.));
#17035=DIRECTION('ref_axis',(1.,0.,0.));
#17036=DIRECTION('center_axis',(0.,0.,1.));
#17037=DIRECTION('ref_axis',(1.,0.,0.));
#17038=DIRECTION('',(0.,0.,-1.));
#17039=DIRECTION('center_axis',(0.,0.,-1.));
#17040=DIRECTION('ref_axis',(1.,0.,0.));
#17041=DIRECTION('center_axis',(0.,0.,1.));
#17042=DIRECTION('ref_axis',(1.,0.,0.));
#17043=DIRECTION('',(0.,0.,-1.));
#17044=DIRECTION('center_axis',(0.,0.,1.));
#17045=DIRECTION('ref_axis',(1.,0.,0.));
#17046=DIRECTION('',(0.,0.,-1.));
#17047=DIRECTION('center_axis',(0.,0.,-1.));
#17048=DIRECTION('ref_axis',(1.,0.,0.));
#17049=DIRECTION('center_axis',(0.,0.,1.));
#17050=DIRECTION('ref_axis',(1.,0.,0.));
#17051=DIRECTION('',(0.,0.,-1.));
#17052=DIRECTION('center_axis',(0.,0.,-1.));
#17053=DIRECTION('ref_axis',(1.,0.,0.));
#17054=DIRECTION('center_axis',(-1.,0.,0.));
#17055=DIRECTION('ref_axis',(0.,-1.,0.));
#17056=DIRECTION('',(0.,1.,0.));
#17057=DIRECTION('center_axis',(1.,0.,0.));
#17058=DIRECTION('ref_axis',(0.,1.,0.));
#17059=DIRECTION('',(0.,-1.,0.));
#17060=DIRECTION('center_axis',(0.,-1.,0.));
#17061=DIRECTION('ref_axis',(1.,0.,0.));
#17062=DIRECTION('',(-1.,0.,0.));
#17063=DIRECTION('center_axis',(0.,1.,0.));
#17064=DIRECTION('ref_axis',(-1.,0.,0.));
#17065=DIRECTION('',(1.,0.,0.));
#17066=DIRECTION('center_axis',(0.,-1.,0.));
#17067=DIRECTION('ref_axis',(1.,0.,0.));
#17068=DIRECTION('',(-1.,0.,0.));
#17069=DIRECTION('center_axis',(-1.,0.,0.));
#17070=DIRECTION('ref_axis',(0.,-1.,0.));
#17071=DIRECTION('',(0.,1.,0.));
#17072=DIRECTION('center_axis',(1.,0.,0.));
#17073=DIRECTION('ref_axis',(0.,1.,0.));
#17074=DIRECTION('',(0.,-1.,0.));
#17075=DIRECTION('center_axis',(-1.,0.,0.));
#17076=DIRECTION('ref_axis',(0.,-1.,0.));
#17077=DIRECTION('',(0.,1.,0.));
#17078=DIRECTION('center_axis',(0.,1.,0.));
#17079=DIRECTION('ref_axis',(-1.,0.,0.));
#17080=DIRECTION('',(1.,0.,0.));
#17081=DIRECTION('center_axis',(0.,-1.,0.));
#17082=DIRECTION('ref_axis',(1.,0.,0.));
#17083=DIRECTION('',(-1.,0.,0.));
#17084=DIRECTION('center_axis',(0.,1.,0.));
#17085=DIRECTION('ref_axis',(-1.,0.,0.));
#17086=DIRECTION('',(1.,0.,0.));
#17087=DIRECTION('center_axis',(1.,0.,0.));
#17088=DIRECTION('ref_axis',(0.,1.,0.));
#17089=DIRECTION('',(0.,-1.,0.));
#17090=DIRECTION('center_axis',(0.,0.,1.));
#17091=DIRECTION('ref_axis',(1.,0.,0.));
#17092=DIRECTION('axis',(0.,0.,1.));
#17093=DIRECTION('refdir',(1.,0.,0.));
#17094=DIRECTION('center_axis',(0.,0.,-1.));
#17095=DIRECTION('ref_axis',(1.,0.,0.));
#17096=DIRECTION('center_axis',(0.,0.,-1.));
#17097=DIRECTION('ref_axis',(1.,0.,0.));
#17098=DIRECTION('center_axis',(0.,0.,-1.));
#17099=DIRECTION('ref_axis',(1.,0.,0.));
#17100=DIRECTION('center_axis',(0.,0.,-1.));
#17101=DIRECTION('ref_axis',(1.,0.,0.));
#17102=DIRECTION('center_axis',(0.,0.,-1.));
#17103=DIRECTION('ref_axis',(1.,0.,0.));
#17104=DIRECTION('',(0.,0.,-1.));
#17105=DIRECTION('center_axis',(0.,0.,-1.));
#17106=DIRECTION('ref_axis',(1.,0.,0.));
#17107=DIRECTION('',(0.,0.,-1.));
#17108=DIRECTION('center_axis',(0.,0.,1.));
#17109=DIRECTION('ref_axis',(1.,0.,0.));
#17110=DIRECTION('center_axis',(0.,0.,-1.));
#17111=DIRECTION('ref_axis',(1.,0.,0.));
#17112=DIRECTION('center_axis',(0.,0.,-1.));
#17113=DIRECTION('ref_axis',(1.,0.,0.));
#17114=DIRECTION('',(0.,0.,-1.));
#17115=DIRECTION('center_axis',(0.,0.,1.));
#17116=DIRECTION('ref_axis',(1.,0.,0.));
#17117=DIRECTION('center_axis',(0.,0.,-1.));
#17118=DIRECTION('ref_axis',(1.,0.,0.));
#17119=DIRECTION('center_axis',(0.,0.,-1.));
#17120=DIRECTION('ref_axis',(1.,0.,0.));
#17121=DIRECTION('',(0.,0.,-1.));
#17122=DIRECTION('center_axis',(0.,0.,1.));
#17123=DIRECTION('ref_axis',(1.,0.,0.));
#17124=DIRECTION('center_axis',(0.,0.,-1.));
#17125=DIRECTION('ref_axis',(1.,0.,0.));
#17126=DIRECTION('center_axis',(0.,0.,-1.));
#17127=DIRECTION('ref_axis',(1.,0.,0.));
#17128=DIRECTION('',(0.,0.,-1.));
#17129=DIRECTION('center_axis',(0.,0.,1.));
#17130=DIRECTION('ref_axis',(1.,0.,0.));
#17131=DIRECTION('center_axis',(0.,0.,-1.));
#17132=DIRECTION('ref_axis',(1.,0.,0.));
#17133=DIRECTION('center_axis',(0.,0.,-1.));
#17134=DIRECTION('ref_axis',(1.,0.,0.));
#17135=DIRECTION('',(0.,0.,-1.));
#17136=DIRECTION('center_axis',(0.,0.,1.));
#17137=DIRECTION('ref_axis',(1.,0.,0.));
#17138=DIRECTION('center_axis',(0.,1.,0.));
#17139=DIRECTION('ref_axis',(-1.,0.,0.));
#17140=DIRECTION('',(-1.,0.,0.));
#17141=DIRECTION('',(0.,0.,1.));
#17142=DIRECTION('',(-1.,0.,0.));
#17143=DIRECTION('',(0.,0.,1.));
#17144=DIRECTION('center_axis',(1.,0.,0.));
#17145=DIRECTION('ref_axis',(0.,1.,0.));
#17146=DIRECTION('',(0.,1.,0.));
#17147=DIRECTION('',(0.,1.,0.));
#17148=DIRECTION('',(0.,0.,1.));
#17149=DIRECTION('center_axis',(0.,-1.,0.));
#17150=DIRECTION('ref_axis',(1.,0.,0.));
#17151=DIRECTION('',(1.,0.,0.));
#17152=DIRECTION('',(1.,0.,0.));
#17153=DIRECTION('',(0.,0.,1.));
#17154=DIRECTION('center_axis',(-1.,0.,0.));
#17155=DIRECTION('ref_axis',(0.,-1.,0.));
#17156=DIRECTION('',(0.,-1.,0.));
#17157=DIRECTION('',(0.,-1.,0.));
#17158=DIRECTION('center_axis',(0.,0.,1.));
#17159=DIRECTION('ref_axis',(1.,0.,0.));
#17160=DIRECTION('center_axis',(0.,0.,1.));
#17161=DIRECTION('ref_axis',(1.,0.,0.));
#17162=DIRECTION('axis',(0.,0.,1.));
#17163=DIRECTION('refdir',(1.,0.,0.));
#17164=DIRECTION('center_axis',(0.,0.,1.));
#17165=DIRECTION('ref_axis',(1.,0.,0.));
#17166=DIRECTION('',(0.,0.,-1.));
#17167=DIRECTION('center_axis',(0.,0.,-1.));
#17168=DIRECTION('ref_axis',(1.,0.,0.));
#17169=DIRECTION('center_axis',(0.,0.,1.));
#17170=DIRECTION('ref_axis',(1.,0.,0.));
#17171=DIRECTION('',(0.,0.,-1.));
#17172=DIRECTION('center_axis',(0.,0.,1.));
#17173=DIRECTION('ref_axis',(1.,0.,0.));
#17174=DIRECTION('',(0.,0.,-1.));
#17175=DIRECTION('center_axis',(0.,0.,1.));
#17176=DIRECTION('ref_axis',(1.,0.,0.));
#17177=DIRECTION('',(0.,0.,-1.));
#17178=DIRECTION('center_axis',(0.,0.,1.));
#17179=DIRECTION('ref_axis',(1.,0.,0.));
#17180=DIRECTION('',(0.,0.,-1.));
#17181=DIRECTION('center_axis',(0.,0.,1.));
#17182=DIRECTION('ref_axis',(1.,0.,0.));
#17183=DIRECTION('',(0.,0.,-1.));
#17184=DIRECTION('center_axis',(0.,0.,1.));
#17185=DIRECTION('ref_axis',(1.,0.,0.));
#17186=DIRECTION('',(0.,0.,-1.));
#17187=DIRECTION('center_axis',(0.,0.,1.));
#17188=DIRECTION('ref_axis',(1.,0.,0.));
#17189=DIRECTION('',(0.,0.,-1.));
#17190=DIRECTION('center_axis',(0.,0.,1.));
#17191=DIRECTION('ref_axis',(1.,0.,0.));
#17192=DIRECTION('',(0.,0.,-1.));
#17193=DIRECTION('center_axis',(0.,0.,1.));
#17194=DIRECTION('ref_axis',(1.,0.,0.));
#17195=DIRECTION('',(0.,0.,-1.));
#17196=DIRECTION('center_axis',(0.,0.,1.));
#17197=DIRECTION('ref_axis',(1.,0.,0.));
#17198=DIRECTION('',(0.,0.,-1.));
#17199=DIRECTION('center_axis',(0.,0.,1.));
#17200=DIRECTION('ref_axis',(1.,0.,0.));
#17201=DIRECTION('',(0.,0.,-1.));
#17202=DIRECTION('center_axis',(0.,0.,1.));
#17203=DIRECTION('ref_axis',(1.,0.,0.));
#17204=DIRECTION('',(0.,0.,-1.));
#17205=DIRECTION('center_axis',(0.,0.,1.));
#17206=DIRECTION('ref_axis',(1.,0.,0.));
#17207=DIRECTION('',(0.,0.,-1.));
#17208=DIRECTION('center_axis',(0.,0.,1.));
#17209=DIRECTION('ref_axis',(1.,0.,0.));
#17210=DIRECTION('',(0.,0.,-1.));
#17211=DIRECTION('center_axis',(0.,0.,1.));
#17212=DIRECTION('ref_axis',(1.,0.,0.));
#17213=DIRECTION('',(0.,0.,-1.));
#17214=DIRECTION('center_axis',(0.,0.,1.));
#17215=DIRECTION('ref_axis',(1.,0.,0.));
#17216=DIRECTION('',(0.,0.,-1.));
#17217=DIRECTION('center_axis',(0.,0.,1.));
#17218=DIRECTION('ref_axis',(1.,0.,0.));
#17219=DIRECTION('',(0.,0.,-1.));
#17220=DIRECTION('center_axis',(0.,0.,1.));
#17221=DIRECTION('ref_axis',(1.,0.,0.));
#17222=DIRECTION('',(0.,0.,-1.));
#17223=DIRECTION('center_axis',(0.,0.,1.));
#17224=DIRECTION('ref_axis',(0.997281310794726,-0.0736884464455154,0.));
#17225=DIRECTION('',(0.,0.,1.));
#17226=DIRECTION('center_axis',(0.,0.,-1.));
#17227=DIRECTION('ref_axis',(1.,1.00674340327557E-13,0.));
#17228=DIRECTION('center_axis',(0.,0.,1.));
#17229=DIRECTION('ref_axis',(1.,1.00674340327557E-13,0.));
#17230=DIRECTION('',(0.,0.,1.));
#17231=DIRECTION('center_axis',(0.,0.,1.));
#17232=DIRECTION('ref_axis',(1.,1.00674340327557E-13,0.));
#17233=DIRECTION('',(0.,0.,1.));
#17234=DIRECTION('center_axis',(0.,0.,1.));
#17235=DIRECTION('ref_axis',(1.,1.00674340327557E-13,0.));
#17236=DIRECTION('',(0.,0.,1.));
#17237=DIRECTION('center_axis',(0.,0.,1.));
#17238=DIRECTION('ref_axis',(1.,1.00674340327557E-13,0.));
#17239=DIRECTION('',(0.,0.,1.));
#17240=DIRECTION('center_axis',(0.,0.,1.));
#17241=DIRECTION('ref_axis',(1.,1.00674340327557E-13,0.));
#17242=DIRECTION('',(0.,0.,1.));
#17243=DIRECTION('center_axis',(0.,0.,1.));
#17244=DIRECTION('ref_axis',(1.,1.00674340327557E-13,0.));
#17245=DIRECTION('',(0.,0.,1.));
#17246=DIRECTION('center_axis',(0.,0.,1.));
#17247=DIRECTION('ref_axis',(1.,1.00674340327557E-13,0.));
#17248=DIRECTION('',(0.,0.,1.));
#17249=DIRECTION('center_axis',(0.,0.,1.));
#17250=DIRECTION('ref_axis',(1.,1.00674340327557E-13,0.));
#17251=DIRECTION('',(0.,0.,1.));
#17252=DIRECTION('center_axis',(0.,0.,1.));
#17253=DIRECTION('ref_axis',(1.,1.00674340327557E-13,0.));
#17254=DIRECTION('',(0.,0.,1.));
#17255=DIRECTION('center_axis',(0.,0.,1.));
#17256=DIRECTION('ref_axis',(1.,1.00674340327557E-13,0.));
#17257=DIRECTION('',(0.,0.,1.));
#17258=DIRECTION('center_axis',(0.,0.,1.));
#17259=DIRECTION('ref_axis',(1.,1.00674340327557E-13,0.));
#17260=DIRECTION('',(0.,0.,1.));
#17261=DIRECTION('center_axis',(0.,0.,1.));
#17262=DIRECTION('ref_axis',(1.,1.00674340327557E-13,0.));
#17263=DIRECTION('',(0.,0.,1.));
#17264=DIRECTION('center_axis',(0.,0.,1.));
#17265=DIRECTION('ref_axis',(1.,1.00674340327557E-13,0.));
#17266=DIRECTION('',(0.,0.,1.));
#17267=DIRECTION('center_axis',(0.,0.,1.));
#17268=DIRECTION('ref_axis',(1.,1.00674340327557E-13,0.));
#17269=DIRECTION('',(0.,0.,1.));
#17270=DIRECTION('center_axis',(0.,0.,1.));
#17271=DIRECTION('ref_axis',(1.,1.00674340327557E-13,0.));
#17272=DIRECTION('',(0.,0.,1.));
#17273=DIRECTION('center_axis',(0.,0.,1.));
#17274=DIRECTION('ref_axis',(1.,1.00674340327557E-13,0.));
#17275=DIRECTION('',(0.,0.,1.));
#17276=DIRECTION('center_axis',(0.,0.,1.));
#17277=DIRECTION('ref_axis',(1.,1.00674340327557E-13,0.));
#17278=DIRECTION('',(0.,0.,1.));
#17279=DIRECTION('center_axis',(0.,0.,1.));
#17280=DIRECTION('ref_axis',(1.,1.00674340327557E-13,0.));
#17281=DIRECTION('',(0.,0.,1.));
#17282=DIRECTION('center_axis',(0.,0.,-1.));
#17283=DIRECTION('ref_axis',(1.,0.,0.));
#17284=DIRECTION('center_axis',(0.,0.,-1.));
#17285=DIRECTION('ref_axis',(1.,0.,0.));
#17286=DIRECTION('',(0.707106781186547,8.65956056235493E-17,0.707106781186548));
#17287=DIRECTION('center_axis',(0.,0.,1.));
#17288=DIRECTION('ref_axis',(1.,0.,0.));
#17289=DIRECTION('center_axis',(0.,0.,1.));
#17290=DIRECTION('ref_axis',(1.,1.00674340327557E-13,0.));
#17291=DIRECTION('center_axis',(0.,0.,-1.));
#17292=DIRECTION('ref_axis',(1.,1.00674340327557E-13,0.));
#17293=DIRECTION('center_axis',(0.,0.,1.));
#17294=DIRECTION('ref_axis',(1.,0.,0.));
#17295=DIRECTION('center_axis',(-2.40370335797945E-16,-1.,0.));
#17296=DIRECTION('ref_axis',(1.,-2.40370335797945E-16,0.));
#17297=DIRECTION('',(1.,-2.40370335797945E-16,0.));
#17298=DIRECTION('',(0.,0.,1.));
#17299=DIRECTION('',(1.,-2.40370335797945E-16,0.));
#17300=DIRECTION('',(0.,0.,1.));
#17301=DIRECTION('center_axis',(-0.866025403784439,-0.5,0.));
#17302=DIRECTION('ref_axis',(0.5,-0.866025403784439,0.));
#17303=DIRECTION('',(0.5,-0.866025403784439,0.));
#17304=DIRECTION('',(0.,0.,1.));
#17305=DIRECTION('',(0.5,-0.866025403784439,0.));
#17306=DIRECTION('center_axis',(-0.866025403784439,0.5,0.));
#17307=DIRECTION('ref_axis',(-0.5,-0.866025403784439,0.));
#17308=DIRECTION('',(-0.5,-0.866025403784439,0.));
#17309=DIRECTION('',(0.,0.,1.));
#17310=DIRECTION('',(-0.5,-0.866025403784439,0.));
#17311=DIRECTION('center_axis',(1.20185167898973E-16,1.,0.));
#17312=DIRECTION('ref_axis',(-1.,1.20185167898973E-16,0.));
#17313=DIRECTION('',(-1.,1.20185167898973E-16,0.));
#17314=DIRECTION('',(0.,0.,1.));
#17315=DIRECTION('',(-1.,1.20185167898973E-16,0.));
#17316=DIRECTION('center_axis',(0.866025403784439,0.5,0.));
#17317=DIRECTION('ref_axis',(-0.5,0.866025403784439,0.));
#17318=DIRECTION('',(-0.5,0.866025403784439,0.));
#17319=DIRECTION('',(0.,0.,1.));
#17320=DIRECTION('',(-0.5,0.866025403784439,0.));
#17321=DIRECTION('center_axis',(0.866025403784439,-0.5,0.));
#17322=DIRECTION('ref_axis',(0.5,0.866025403784439,0.));
#17323=DIRECTION('',(0.5,0.866025403784439,0.));
#17324=DIRECTION('',(0.5,0.866025403784439,0.));
#17325=DIRECTION('center_axis',(0.,0.,1.));
#17326=DIRECTION('ref_axis',(1.,0.,0.));
#17327=DIRECTION('center_axis',(0.,0.,1.));
#17328=DIRECTION('ref_axis',(1.,0.,0.));
#17329=DIRECTION('center_axis',(0.,0.,1.));
#17330=DIRECTION('ref_axis',(1.,0.,0.));
#17331=DIRECTION('center_axis',(0.,0.,1.));
#17332=DIRECTION('ref_axis',(1.,0.,0.));
#17333=DIRECTION('',(0.,0.,-1.));
#17334=DIRECTION('center_axis',(0.,0.,1.));
#17335=DIRECTION('ref_axis',(1.,0.,0.));
#17336=DIRECTION('center_axis',(0.,0.,1.));
#17337=DIRECTION('ref_axis',(1.,0.,0.));
#17338=DIRECTION('center_axis',(0.,0.,1.));
#17339=DIRECTION('ref_axis',(1.,0.,0.));
#17340=DIRECTION('axis',(0.,0.,1.));
#17341=DIRECTION('refdir',(1.,0.,0.));
#17342=DIRECTION('center_axis',(0.,0.,1.));
#17343=DIRECTION('ref_axis',(1.,0.,0.));
#17344=DIRECTION('center_axis',(0.,0.,1.));
#17345=DIRECTION('ref_axis',(1.,0.,0.));
#17346=DIRECTION('',(0.,0.,-1.));
#17347=DIRECTION('center_axis',(0.,0.,1.));
#17348=DIRECTION('ref_axis',(1.,0.,0.));
#17349=DIRECTION('center_axis',(0.,0.,1.));
#17350=DIRECTION('ref_axis',(1.,0.,0.));
#17351=DIRECTION('center_axis',(0.,0.,1.));
#17352=DIRECTION('ref_axis',(1.,0.,0.));
#17353=DIRECTION('axis',(0.,0.,1.));
#17354=DIRECTION('refdir',(1.,0.,0.));
#17355=DIRECTION('center_axis',(0.,0.,-1.));
#17356=DIRECTION('ref_axis',(1.,0.,0.));
#17357=DIRECTION('',(0.,0.,-1.));
#17358=DIRECTION('center_axis',(0.,0.,1.));
#17359=DIRECTION('ref_axis',(1.,0.,0.));
#17360=DIRECTION('',(0.,0.,-1.));
#17361=DIRECTION('center_axis',(0.,0.,1.));
#17362=DIRECTION('ref_axis',(1.,0.,0.));
#17363=DIRECTION('center_axis',(0.,0.,1.));
#17364=DIRECTION('ref_axis',(1.,0.,0.));
#17365=DIRECTION('center_axis',(0.,0.,-1.));
#17366=DIRECTION('ref_axis',(1.,0.,0.));
#17367=DIRECTION('',(0.,0.,-1.));
#17368=DIRECTION('center_axis',(0.,0.,-1.));
#17369=DIRECTION('ref_axis',(1.,0.,0.));
#17370=DIRECTION('',(0.,0.,-1.));
#17371=DIRECTION('center_axis',(0.,0.,-1.));
#17372=DIRECTION('ref_axis',(1.,0.,0.));
#17373=DIRECTION('',(0.,0.,-1.));
#17374=DIRECTION('center_axis',(0.,0.,-1.));
#17375=DIRECTION('ref_axis',(1.,0.,0.));
#17376=DIRECTION('',(0.,0.,-1.));
#17377=DIRECTION('center_axis',(0.,0.,-1.));
#17378=DIRECTION('ref_axis',(1.,0.,0.));
#17379=DIRECTION('',(0.,0.,-1.));
#17380=DIRECTION('center_axis',(0.,0.,-1.));
#17381=DIRECTION('ref_axis',(1.,0.,0.));
#17382=DIRECTION('',(0.,0.,-1.));
#17383=DIRECTION('center_axis',(0.,0.,-1.));
#17384=DIRECTION('ref_axis',(0.937998542404131,-0.346639199237082,0.));
#17385=DIRECTION('',(0.,0.,-1.));
#17386=DIRECTION('center_axis',(0.,0.,-1.));
#17387=DIRECTION('ref_axis',(1.,0.,0.));
#17388=DIRECTION('center_axis',(0.,0.,-1.));
#17389=DIRECTION('ref_axis',(0.793234457633775,0.608916328589118,0.));
#17390=DIRECTION('',(1.22464679914735E-16,-2.66923102573661E-30,-1.));
#17391=DIRECTION('center_axis',(0.,0.,1.));
#17392=DIRECTION('ref_axis',(1.,-2.16734607052251E-14,0.));
#17393=DIRECTION('center_axis',(0.,0.,-1.));
#17394=DIRECTION('ref_axis',(1.,-2.16734607052251E-14,0.));
#17395=DIRECTION('',(1.22464679914735E-16,-2.66923102573661E-30,-1.));
#17396=DIRECTION('center_axis',(0.,0.,-1.));
#17397=DIRECTION('ref_axis',(1.,-2.16734607052251E-14,0.));
#17398=DIRECTION('',(1.22464679914735E-16,-2.66923102573661E-30,-1.));
#17399=DIRECTION('center_axis',(0.,0.,-1.));
#17400=DIRECTION('ref_axis',(1.,-2.16734607052251E-14,0.));
#17401=DIRECTION('',(1.22464679914735E-16,-2.66923102573661E-30,-1.));
#17402=DIRECTION('center_axis',(0.,0.,-1.));
#17403=DIRECTION('ref_axis',(1.,-2.16734607052251E-14,0.));
#17404=DIRECTION('',(1.22464679914735E-16,-2.66923102573661E-30,-1.));
#17405=DIRECTION('center_axis',(0.,0.,-1.));
#17406=DIRECTION('ref_axis',(1.,-2.16734607052251E-14,0.));
#17407=DIRECTION('',(1.22464679914735E-16,-2.66923102573661E-30,-1.));
#17408=DIRECTION('center_axis',(0.,0.,-1.));
#17409=DIRECTION('ref_axis',(1.,-2.16734607052251E-14,0.));
#17410=DIRECTION('',(1.22464679914735E-16,-2.66923102573661E-30,-1.));
#17411=DIRECTION('center_axis',(0.,0.,-1.));
#17412=DIRECTION('ref_axis',(-0.609099265708522,-0.793093994753042,0.));
#17413=DIRECTION('',(1.22464679914735E-16,-2.66923102573661E-30,-1.));
#17414=DIRECTION('center_axis',(0.,0.,-1.));
#17415=DIRECTION('ref_axis',(1.,-2.16734607052251E-14,0.));
#17416=DIRECTION('center_axis',(0.,0.,-1.));
#17417=DIRECTION('ref_axis',(1.,0.,0.));
#17418=DIRECTION('',(0.,0.,-1.));
#17419=DIRECTION('center_axis',(0.,0.,1.));
#17420=DIRECTION('ref_axis',(1.,0.,0.));
#17421=DIRECTION('',(0.,0.,-1.));
#17422=DIRECTION('center_axis',(0.,0.,1.));
#17423=DIRECTION('ref_axis',(1.,0.,0.));
#17424=DIRECTION('center_axis',(0.,0.,1.));
#17425=DIRECTION('ref_axis',(1.,0.,0.));
#17426=DIRECTION('center_axis',(0.,0.,-1.));
#17427=DIRECTION('ref_axis',(1.,0.,0.));
#17428=DIRECTION('',(0.,0.,-1.));
#17429=DIRECTION('center_axis',(0.,0.,-1.));
#17430=DIRECTION('ref_axis',(1.,0.,0.));
#17431=DIRECTION('',(0.,0.,-1.));
#17432=DIRECTION('center_axis',(0.,0.,-1.));
#17433=DIRECTION('ref_axis',(1.,0.,0.));
#17434=DIRECTION('',(0.,0.,-1.));
#17435=DIRECTION('center_axis',(0.,0.,-1.));
#17436=DIRECTION('ref_axis',(1.,0.,0.));
#17437=DIRECTION('',(0.,0.,-1.));
#17438=DIRECTION('center_axis',(0.,0.,-1.));
#17439=DIRECTION('ref_axis',(1.,0.,0.));
#17440=DIRECTION('',(0.,0.,-1.));
#17441=DIRECTION('center_axis',(0.,0.,-1.));
#17442=DIRECTION('ref_axis',(1.,0.,0.));
#17443=DIRECTION('',(0.,0.,-1.));
#17444=DIRECTION('center_axis',(0.,0.,-1.));
#17445=DIRECTION('ref_axis',(0.937998514609972,-0.346639274447495,0.));
#17446=DIRECTION('',(0.,0.,-1.));
#17447=DIRECTION('center_axis',(0.,0.,-1.));
#17448=DIRECTION('ref_axis',(1.,0.,0.));
#17449=DIRECTION('center_axis',(0.,0.,-1.));
#17450=DIRECTION('ref_axis',(0.793234421148473,0.608916376118468,0.));
#17451=DIRECTION('',(1.22464679914735E-16,-2.66923102573661E-30,-1.));
#17452=DIRECTION('center_axis',(0.,0.,1.));
#17453=DIRECTION('ref_axis',(1.,-2.16734607052251E-14,0.));
#17454=DIRECTION('center_axis',(0.,0.,-1.));
#17455=DIRECTION('ref_axis',(1.,-2.16734607052251E-14,0.));
#17456=DIRECTION('',(1.22464679914735E-16,-2.66923102573661E-30,-1.));
#17457=DIRECTION('center_axis',(0.,0.,-1.));
#17458=DIRECTION('ref_axis',(1.,-2.16734607052251E-14,0.));
#17459=DIRECTION('',(1.22464679914735E-16,-2.66923102573661E-30,-1.));
#17460=DIRECTION('center_axis',(0.,0.,-1.));
#17461=DIRECTION('ref_axis',(1.,-2.16734607052251E-14,0.));
#17462=DIRECTION('',(1.22464679914735E-16,-2.66923102573661E-30,-1.));
#17463=DIRECTION('center_axis',(0.,0.,-1.));
#17464=DIRECTION('ref_axis',(1.,-2.16734607052251E-14,0.));
#17465=DIRECTION('',(1.22464679914735E-16,-2.66923102573661E-30,-1.));
#17466=DIRECTION('center_axis',(0.,0.,-1.));
#17467=DIRECTION('ref_axis',(1.,-2.16734607052251E-14,0.));
#17468=DIRECTION('',(1.22464679914735E-16,-2.66923102573661E-30,-1.));
#17469=DIRECTION('center_axis',(0.,0.,-1.));
#17470=DIRECTION('ref_axis',(1.,-2.16734607052251E-14,0.));
#17471=DIRECTION('',(1.22464679914735E-16,-2.66923102573661E-30,-1.));
#17472=DIRECTION('center_axis',(0.,0.,-1.));
#17473=DIRECTION('ref_axis',(-0.609099316811134,-0.793093955506036,0.));
#17474=DIRECTION('',(1.22464679914735E-16,-2.66923102573661E-30,-1.));
#17475=DIRECTION('center_axis',(0.,0.,-1.));
#17476=DIRECTION('ref_axis',(1.,-2.16734607052251E-14,0.));
#17477=DIRECTION('center_axis',(0.,0.,-1.));
#17478=DIRECTION('ref_axis',(1.,0.,0.));
#17479=DIRECTION('',(0.,0.,-1.));
#17480=DIRECTION('center_axis',(0.,0.,1.));
#17481=DIRECTION('ref_axis',(1.,0.,0.));
#17482=DIRECTION('',(0.,0.,-1.));
#17483=DIRECTION('center_axis',(0.,0.,1.));
#17484=DIRECTION('ref_axis',(1.,0.,0.));
#17485=DIRECTION('center_axis',(0.,0.,1.));
#17486=DIRECTION('ref_axis',(1.,0.,0.));
#17487=DIRECTION('center_axis',(0.,0.,-1.));
#17488=DIRECTION('ref_axis',(1.,0.,0.));
#17489=DIRECTION('',(0.,0.,-1.));
#17490=DIRECTION('center_axis',(0.,0.,-1.));
#17491=DIRECTION('ref_axis',(1.,0.,0.));
#17492=DIRECTION('',(0.,0.,-1.));
#17493=DIRECTION('center_axis',(0.,0.,-1.));
#17494=DIRECTION('ref_axis',(1.,0.,0.));
#17495=DIRECTION('',(0.,0.,-1.));
#17496=DIRECTION('center_axis',(0.,0.,-1.));
#17497=DIRECTION('ref_axis',(1.,0.,0.));
#17498=DIRECTION('',(0.,0.,-1.));
#17499=DIRECTION('center_axis',(0.,0.,-1.));
#17500=DIRECTION('ref_axis',(1.,0.,0.));
#17501=DIRECTION('',(0.,0.,-1.));
#17502=DIRECTION('center_axis',(0.,0.,-1.));
#17503=DIRECTION('ref_axis',(1.,0.,0.));
#17504=DIRECTION('',(0.,0.,-1.));
#17505=DIRECTION('center_axis',(0.,0.,-1.));
#17506=DIRECTION('ref_axis',(0.937997876463511,-0.346641001253376,0.));
#17507=DIRECTION('',(0.,0.,-1.));
#17508=DIRECTION('center_axis',(0.,0.,-1.));
#17509=DIRECTION('ref_axis',(1.,0.,0.));
#17510=DIRECTION('center_axis',(0.,0.,-1.));
#17511=DIRECTION('ref_axis',(0.793233502010203,0.608917573476599,0.));
#17512=DIRECTION('',(1.22464679914735E-16,-2.67208401572961E-30,-1.));
#17513=DIRECTION('center_axis',(0.,0.,1.));
#17514=DIRECTION('ref_axis',(1.,-2.16967571364491E-14,0.));
#17515=DIRECTION('center_axis',(0.,0.,-1.));
#17516=DIRECTION('ref_axis',(1.,-2.16967571364491E-14,0.));
#17517=DIRECTION('',(1.22464679914735E-16,-2.67208401572961E-30,-1.));
#17518=DIRECTION('center_axis',(0.,0.,-1.));
#17519=DIRECTION('ref_axis',(1.,-2.16967571364491E-14,0.));
#17520=DIRECTION('',(1.22464679914735E-16,-2.67208401572961E-30,-1.));
#17521=DIRECTION('center_axis',(0.,0.,-1.));
#17522=DIRECTION('ref_axis',(1.,-2.16967571364491E-14,0.));
#17523=DIRECTION('',(1.22464679914735E-16,-2.67208401572961E-30,-1.));
#17524=DIRECTION('center_axis',(0.,0.,-1.));
#17525=DIRECTION('ref_axis',(1.,-2.16967571364491E-14,0.));
#17526=DIRECTION('',(1.22464679914735E-16,-2.67208401572961E-30,-1.));
#17527=DIRECTION('center_axis',(0.,0.,-1.));
#17528=DIRECTION('ref_axis',(1.,-2.16967571364491E-14,0.));
#17529=DIRECTION('',(1.22464679914735E-16,-2.67208401572961E-30,-1.));
#17530=DIRECTION('center_axis',(0.,0.,-1.));
#17531=DIRECTION('ref_axis',(1.,-2.16967571364491E-14,0.));
#17532=DIRECTION('',(1.22464679914735E-16,-2.67208401572961E-30,-1.));
#17533=DIRECTION('center_axis',(0.,0.,-1.));
#17534=DIRECTION('ref_axis',(-0.609100172155653,-0.793093298597305,0.));
#17535=DIRECTION('',(1.22464679914735E-16,-2.67208401572961E-30,-1.));
#17536=DIRECTION('center_axis',(0.,0.,-1.));
#17537=DIRECTION('ref_axis',(1.,-2.16967571364491E-14,0.));
#17538=DIRECTION('center_axis',(0.,0.,1.));
#17539=DIRECTION('ref_axis',(1.,0.,0.));
#17540=DIRECTION('center_axis',(0.,0.,-1.));
#17541=DIRECTION('ref_axis',(1.,-2.16967571364491E-14,0.));
#17542=DIRECTION('center_axis',(0.,0.,-1.));
#17543=DIRECTION('ref_axis',(1.,0.,0.));
#17544=DIRECTION('center_axis',(0.,0.,1.));
#17545=DIRECTION('ref_axis',(1.,0.,0.));
#17546=DIRECTION('center_axis',(0.,0.,-1.));
#17547=DIRECTION('ref_axis',(1.,-2.16734607052251E-14,0.));
#17548=DIRECTION('center_axis',(0.,0.,-1.));
#17549=DIRECTION('ref_axis',(1.,0.,0.));
#17550=DIRECTION('center_axis',(0.,0.,1.));
#17551=DIRECTION('ref_axis',(1.,0.,0.));
#17552=DIRECTION('center_axis',(0.,0.,-1.));
#17553=DIRECTION('ref_axis',(1.,-2.16734607052251E-14,0.));
#17554=DIRECTION('center_axis',(0.,0.,-1.));
#17555=DIRECTION('ref_axis',(1.,0.,0.));
#17556=DIRECTION('center_axis',(0.,0.,-1.));
#17557=DIRECTION('ref_axis',(1.,0.,0.));
#17558=DIRECTION('center_axis',(0.,0.,-1.));
#17559=DIRECTION('ref_axis',(1.,0.,0.));
#17560=DIRECTION('center_axis',(0.,0.,-1.));
#17561=DIRECTION('ref_axis',(1.,0.,0.));
#17562=DIRECTION('center_axis',(6.12323399573677E-17,0.,1.));
#17563=DIRECTION('ref_axis',(1.,0.,0.));
#17564=DIRECTION('center_axis',(0.,0.,-1.));
#17565=DIRECTION('ref_axis',(0.,1.,0.));
#17566=DIRECTION('center_axis',(-1.22464679914735E-16,1.,0.));
#17567=DIRECTION('ref_axis',(-1.,-1.22464679914735E-16,0.));
#17568=DIRECTION('center_axis',(0.,0.,1.));
#17569=DIRECTION('ref_axis',(1.,0.,0.));
#17570=DIRECTION('center_axis',(0.,0.,1.));
#17571=DIRECTION('ref_axis',(1.,0.,0.));
#17572=DIRECTION('',(0.,0.,-1.));
#17573=DIRECTION('center_axis',(0.,0.,1.));
#17574=DIRECTION('ref_axis',(1.,0.,0.));
#17575=DIRECTION('center_axis',(0.,0.,1.));
#17576=DIRECTION('ref_axis',(1.,0.,0.));
#17577=DIRECTION('center_axis',(0.,0.,1.));
#17578=DIRECTION('ref_axis',(1.,0.,0.));
#17579=DIRECTION('axis',(0.,0.,1.));
#17580=DIRECTION('refdir',(1.,0.,0.));
#17581=DIRECTION('center_axis',(0.,0.,-1.));
#17582=DIRECTION('ref_axis',(1.,0.,0.));
#17583=DIRECTION('center_axis',(0.,0.,-1.));
#17584=DIRECTION('ref_axis',(1.,0.,0.));
#17585=DIRECTION('',(0.,0.,-1.));
#17586=DIRECTION('center_axis',(0.,0.,1.));
#17587=DIRECTION('ref_axis',(1.,0.,0.));
#17588=DIRECTION('center_axis',(0.,0.,-1.));
#17589=DIRECTION('ref_axis',(1.,0.,0.));
#17590=DIRECTION('center_axis',(0.,0.,-1.));
#17591=DIRECTION('ref_axis',(1.,0.,0.));
#17592=DIRECTION('',(0.,0.,-1.));
#17593=DIRECTION('center_axis',(0.,0.,1.));
#17594=DIRECTION('ref_axis',(1.,0.,0.));
#17595=DIRECTION('center_axis',(0.,0.,-1.));
#17596=DIRECTION('ref_axis',(1.,0.,0.));
#17597=DIRECTION('center_axis',(0.,0.,-1.));
#17598=DIRECTION('ref_axis',(1.,0.,0.));
#17599=DIRECTION('',(0.,0.,-1.));
#17600=DIRECTION('center_axis',(0.,0.,1.));
#17601=DIRECTION('ref_axis',(1.,0.,0.));
#17602=DIRECTION('center_axis',(6.12323399573677E-17,0.,1.));
#17603=DIRECTION('ref_axis',(1.,0.,0.));
#17604=DIRECTION('center_axis',(0.,0.,1.));
#17605=DIRECTION('ref_axis',(0.,-1.,0.));
#17606=DIRECTION('center_axis',(-1.22464679914735E-16,1.,0.));
#17607=DIRECTION('ref_axis',(-1.,-1.22464679914735E-16,0.));
#17608=DIRECTION('center_axis',(0.,0.,-1.));
#17609=DIRECTION('ref_axis',(1.,0.,0.));
#17610=DIRECTION('center_axis',(0.,0.,1.));
#17611=DIRECTION('ref_axis',(1.,0.,0.));
#17612=DIRECTION('center_axis',(0.,0.,-1.));
#17613=DIRECTION('ref_axis',(1.,0.,0.));
#17614=DIRECTION('',(0.,0.,-1.));
#17615=DIRECTION('center_axis',(0.,0.,1.));
#17616=DIRECTION('ref_axis',(1.,0.,0.));
#17617=DIRECTION('center_axis',(0.,0.,1.));
#17618=DIRECTION('ref_axis',(1.,0.,0.));
#17619=DIRECTION('',(0.,0.,-1.));
#17620=DIRECTION('center_axis',(0.,0.,1.));
#17621=DIRECTION('ref_axis',(1.,0.,0.));
#17622=DIRECTION('center_axis',(0.,0.,1.));
#17623=DIRECTION('ref_axis',(1.,0.,0.));
#17624=DIRECTION('center_axis',(0.,0.,1.));
#17625=DIRECTION('ref_axis',(1.,0.,0.));
#17626=DIRECTION('axis',(0.,0.,1.));
#17627=DIRECTION('refdir',(1.,0.,0.));
#17628=DIRECTION('center_axis',(0.,0.,1.));
#17629=DIRECTION('ref_axis',(1.,0.,0.));
#17630=DIRECTION('',(0.,0.,-1.));
#17631=DIRECTION('center_axis',(0.,0.,-1.));
#17632=DIRECTION('ref_axis',(1.,0.,0.));
#17633=DIRECTION('center_axis',(0.,0.,1.));
#17634=DIRECTION('ref_axis',(1.,0.,0.));
#17635=DIRECTION('',(0.,0.,-1.));
#17636=DIRECTION('center_axis',(0.,0.,1.));
#17637=DIRECTION('ref_axis',(1.,0.,0.));
#17638=DIRECTION('',(0.,0.,-1.));
#17639=DIRECTION('center_axis',(0.,0.,1.));
#17640=DIRECTION('ref_axis',(1.,0.,0.));
#17641=DIRECTION('',(0.,0.,-1.));
#17642=DIRECTION('center_axis',(0.,0.,1.));
#17643=DIRECTION('ref_axis',(1.,0.,0.));
#17644=DIRECTION('',(0.,0.,-1.));
#17645=DIRECTION('center_axis',(0.,0.,1.));
#17646=DIRECTION('ref_axis',(1.,0.,0.));
#17647=DIRECTION('',(0.,0.,-1.));
#17648=DIRECTION('center_axis',(0.,0.,1.));
#17649=DIRECTION('ref_axis',(1.,0.,0.));
#17650=DIRECTION('',(0.,0.,-1.));
#17651=DIRECTION('center_axis',(0.,0.,1.));
#17652=DIRECTION('ref_axis',(1.,0.,0.));
#17653=DIRECTION('',(0.,0.,-1.));
#17654=DIRECTION('center_axis',(0.,0.,1.));
#17655=DIRECTION('ref_axis',(1.,0.,0.));
#17656=DIRECTION('',(0.,0.,-1.));
#17657=DIRECTION('center_axis',(0.,0.,1.));
#17658=DIRECTION('ref_axis',(1.,0.,0.));
#17659=DIRECTION('',(0.,0.,-1.));
#17660=DIRECTION('center_axis',(0.,0.,1.));
#17661=DIRECTION('ref_axis',(1.,0.,0.));
#17662=DIRECTION('',(0.,0.,-1.));
#17663=DIRECTION('center_axis',(0.,0.,1.));
#17664=DIRECTION('ref_axis',(1.,0.,0.));
#17665=DIRECTION('',(0.,0.,-1.));
#17666=DIRECTION('center_axis',(0.,0.,1.));
#17667=DIRECTION('ref_axis',(1.,0.,0.));
#17668=DIRECTION('',(0.,0.,-1.));
#17669=DIRECTION('center_axis',(0.,0.,1.));
#17670=DIRECTION('ref_axis',(1.,0.,0.));
#17671=DIRECTION('',(0.,0.,-1.));
#17672=DIRECTION('center_axis',(0.,0.,1.));
#17673=DIRECTION('ref_axis',(1.,0.,0.));
#17674=DIRECTION('',(0.,0.,-1.));
#17675=DIRECTION('center_axis',(0.,0.,1.));
#17676=DIRECTION('ref_axis',(1.,0.,0.));
#17677=DIRECTION('',(0.,0.,-1.));
#17678=DIRECTION('center_axis',(0.,0.,1.));
#17679=DIRECTION('ref_axis',(1.,0.,0.));
#17680=DIRECTION('',(0.,0.,-1.));
#17681=DIRECTION('center_axis',(0.,0.,1.));
#17682=DIRECTION('ref_axis',(1.,0.,0.));
#17683=DIRECTION('',(0.,0.,-1.));
#17684=DIRECTION('center_axis',(0.,0.,1.));
#17685=DIRECTION('ref_axis',(1.,0.,0.));
#17686=DIRECTION('',(0.,0.,-1.));
#17687=DIRECTION('center_axis',(0.,0.,1.));
#17688=DIRECTION('ref_axis',(1.,0.,0.));
#17689=DIRECTION('',(0.,0.,-1.));
#17690=DIRECTION('center_axis',(0.,0.,1.));
#17691=DIRECTION('ref_axis',(1.,0.,0.));
#17692=DIRECTION('',(0.,0.,-1.));
#17693=DIRECTION('center_axis',(0.,0.,1.));
#17694=DIRECTION('ref_axis',(1.,0.,0.));
#17695=DIRECTION('',(0.,0.,-1.));
#17696=DIRECTION('center_axis',(0.,0.,1.));
#17697=DIRECTION('ref_axis',(1.,0.,0.));
#17698=DIRECTION('',(0.,0.,-1.));
#17699=DIRECTION('center_axis',(0.,0.,1.));
#17700=DIRECTION('ref_axis',(1.,0.,0.));
#17701=DIRECTION('',(0.,0.,-1.));
#17702=DIRECTION('center_axis',(0.,0.,1.));
#17703=DIRECTION('ref_axis',(1.,0.,0.));
#17704=DIRECTION('',(0.,0.,-1.));
#17705=DIRECTION('center_axis',(0.,0.,1.));
#17706=DIRECTION('ref_axis',(1.,0.,0.));
#17707=DIRECTION('',(0.,0.,-1.));
#17708=DIRECTION('center_axis',(0.,0.,1.));
#17709=DIRECTION('ref_axis',(1.,0.,0.));
#17710=DIRECTION('',(0.,0.,-1.));
#17711=DIRECTION('center_axis',(0.,0.,1.));
#17712=DIRECTION('ref_axis',(1.,0.,0.));
#17713=DIRECTION('',(0.,0.,-1.));
#17714=DIRECTION('center_axis',(0.,0.,1.));
#17715=DIRECTION('ref_axis',(1.,0.,0.));
#17716=DIRECTION('',(0.,0.,-1.));
#17717=DIRECTION('center_axis',(0.,0.,1.));
#17718=DIRECTION('ref_axis',(1.,0.,0.));
#17719=DIRECTION('',(0.,0.,-1.));
#17720=DIRECTION('center_axis',(0.,0.,1.));
#17721=DIRECTION('ref_axis',(1.,0.,0.));
#17722=DIRECTION('',(0.,0.,-1.));
#17723=DIRECTION('center_axis',(0.,0.,1.));
#17724=DIRECTION('ref_axis',(1.,0.,0.));
#17725=DIRECTION('',(0.,0.,-1.));
#17726=DIRECTION('center_axis',(0.,0.,1.));
#17727=DIRECTION('ref_axis',(1.,0.,0.));
#17728=DIRECTION('',(0.,0.,-1.));
#17729=DIRECTION('center_axis',(0.,0.,1.));
#17730=DIRECTION('ref_axis',(1.,0.,0.));
#17731=DIRECTION('',(0.,0.,-1.));
#17732=DIRECTION('center_axis',(0.,0.,1.));
#17733=DIRECTION('ref_axis',(1.,0.,0.));
#17734=DIRECTION('',(0.,0.,-1.));
#17735=DIRECTION('center_axis',(0.,0.,1.));
#17736=DIRECTION('ref_axis',(1.,0.,0.));
#17737=DIRECTION('',(0.,0.,-1.));
#17738=DIRECTION('center_axis',(0.,0.,1.));
#17739=DIRECTION('ref_axis',(1.,0.,0.));
#17740=DIRECTION('',(0.,0.,-1.));
#17741=DIRECTION('center_axis',(0.,0.,1.));
#17742=DIRECTION('ref_axis',(1.,0.,0.));
#17743=DIRECTION('',(0.,0.,-1.));
#17744=DIRECTION('center_axis',(0.,0.,1.));
#17745=DIRECTION('ref_axis',(1.,0.,0.));
#17746=DIRECTION('',(0.,0.,-1.));
#17747=DIRECTION('center_axis',(0.,0.,1.));
#17748=DIRECTION('ref_axis',(1.,0.,0.));
#17749=DIRECTION('',(0.,0.,-1.));
#17750=DIRECTION('center_axis',(0.,0.,1.));
#17751=DIRECTION('ref_axis',(1.,0.,0.));
#17752=DIRECTION('',(0.,0.,-1.));
#17753=DIRECTION('center_axis',(0.,0.,1.));
#17754=DIRECTION('ref_axis',(1.,0.,0.));
#17755=DIRECTION('',(0.,0.,-1.));
#17756=DIRECTION('center_axis',(0.,0.,1.));
#17757=DIRECTION('ref_axis',(1.,0.,0.));
#17758=DIRECTION('',(0.,0.,-1.));
#17759=DIRECTION('center_axis',(0.,0.,1.));
#17760=DIRECTION('ref_axis',(1.,0.,0.));
#17761=DIRECTION('',(0.,0.,-1.));
#17762=DIRECTION('center_axis',(0.,0.,1.));
#17763=DIRECTION('ref_axis',(1.,0.,0.));
#17764=DIRECTION('',(0.,0.,-1.));
#17765=DIRECTION('center_axis',(0.,0.,1.));
#17766=DIRECTION('ref_axis',(1.,0.,0.));
#17767=DIRECTION('',(0.,0.,-1.));
#17768=DIRECTION('center_axis',(0.,0.,1.));
#17769=DIRECTION('ref_axis',(1.,0.,0.));
#17770=DIRECTION('',(0.,0.,-1.));
#17771=DIRECTION('center_axis',(0.,0.,1.));
#17772=DIRECTION('ref_axis',(1.,0.,0.));
#17773=DIRECTION('',(0.,0.,-1.));
#17774=DIRECTION('center_axis',(0.,0.,1.));
#17775=DIRECTION('ref_axis',(1.,0.,0.));
#17776=DIRECTION('',(0.,0.,-1.));
#17777=DIRECTION('center_axis',(0.,0.,1.));
#17778=DIRECTION('ref_axis',(1.,0.,0.));
#17779=DIRECTION('',(0.,0.,-1.));
#17780=DIRECTION('center_axis',(0.,0.,1.));
#17781=DIRECTION('ref_axis',(1.,0.,0.));
#17782=DIRECTION('',(0.,0.,-1.));
#17783=DIRECTION('center_axis',(0.,0.,1.));
#17784=DIRECTION('ref_axis',(1.,0.,0.));
#17785=DIRECTION('',(0.,0.,-1.));
#17786=DIRECTION('center_axis',(0.,0.,1.));
#17787=DIRECTION('ref_axis',(1.,0.,0.));
#17788=DIRECTION('',(0.,0.,-1.));
#17789=DIRECTION('center_axis',(0.,0.,1.));
#17790=DIRECTION('ref_axis',(1.,0.,0.));
#17791=DIRECTION('',(0.,0.,-1.));
#17792=DIRECTION('center_axis',(0.,0.,1.));
#17793=DIRECTION('ref_axis',(1.,0.,0.));
#17794=DIRECTION('',(0.,0.,-1.));
#17795=DIRECTION('center_axis',(0.,0.,1.));
#17796=DIRECTION('ref_axis',(1.,0.,0.));
#17797=DIRECTION('',(0.,0.,-1.));
#17798=DIRECTION('center_axis',(0.,0.,1.));
#17799=DIRECTION('ref_axis',(1.,0.,0.));
#17800=DIRECTION('',(0.,0.,-1.));
#17801=DIRECTION('center_axis',(0.,0.,1.));
#17802=DIRECTION('ref_axis',(1.,0.,0.));
#17803=DIRECTION('',(0.,0.,-1.));
#17804=DIRECTION('center_axis',(0.,0.,1.));
#17805=DIRECTION('ref_axis',(1.,0.,0.));
#17806=DIRECTION('',(0.,0.,-1.));
#17807=DIRECTION('center_axis',(0.,0.,1.));
#17808=DIRECTION('ref_axis',(1.,0.,0.));
#17809=DIRECTION('',(0.,0.,-1.));
#17810=DIRECTION('center_axis',(0.,0.,1.));
#17811=DIRECTION('ref_axis',(-0.457630590434842,-0.889142419805881,0.));
#17812=DIRECTION('',(0.,0.,1.));
#17813=DIRECTION('center_axis',(0.,0.,1.));
#17814=DIRECTION('ref_axis',(1.,-8.75189148499889E-13,0.));
#17815=DIRECTION('center_axis',(0.,0.,1.));
#17816=DIRECTION('ref_axis',(1.,-8.75189148499889E-13,0.));
#17817=DIRECTION('',(0.,0.,1.));
#17818=DIRECTION('center_axis',(0.,0.,1.));
#17819=DIRECTION('ref_axis',(1.,-8.75189148499889E-13,0.));
#17820=DIRECTION('',(0.,0.,1.));
#17821=DIRECTION('center_axis',(0.,0.,1.));
#17822=DIRECTION('ref_axis',(1.,-8.75189148499889E-13,0.));
#17823=DIRECTION('',(0.,0.,1.));
#17824=DIRECTION('center_axis',(0.,0.,1.));
#17825=DIRECTION('ref_axis',(1.,-8.75189148499889E-13,0.));
#17826=DIRECTION('',(0.,0.,1.));
#17827=DIRECTION('center_axis',(0.,0.,1.));
#17828=DIRECTION('ref_axis',(1.,-8.75189148499889E-13,0.));
#17829=DIRECTION('',(0.,0.,1.));
#17830=DIRECTION('center_axis',(0.,0.,1.));
#17831=DIRECTION('ref_axis',(1.,-8.75189148499889E-13,0.));
#17832=DIRECTION('',(0.,0.,1.));
#17833=DIRECTION('center_axis',(0.,0.,1.));
#17834=DIRECTION('ref_axis',(1.,-8.75189148499889E-13,0.));
#17835=DIRECTION('',(0.,0.,1.));
#17836=DIRECTION('center_axis',(0.,0.,1.));
#17837=DIRECTION('ref_axis',(1.,-8.75189148499889E-13,0.));
#17838=DIRECTION('',(0.,0.,1.));
#17839=DIRECTION('center_axis',(0.,0.,1.));
#17840=DIRECTION('ref_axis',(1.,-8.75189148499889E-13,0.));
#17841=DIRECTION('',(0.,0.,1.));
#17842=DIRECTION('center_axis',(0.,0.,1.));
#17843=DIRECTION('ref_axis',(1.,-8.75189148499889E-13,0.));
#17844=DIRECTION('',(0.,0.,1.));
#17845=DIRECTION('center_axis',(0.,0.,1.));
#17846=DIRECTION('ref_axis',(1.,-8.75189148499889E-13,0.));
#17847=DIRECTION('',(0.,0.,1.));
#17848=DIRECTION('center_axis',(0.,0.,1.));
#17849=DIRECTION('ref_axis',(1.,-8.75189148499889E-13,0.));
#17850=DIRECTION('',(0.,0.,1.));
#17851=DIRECTION('center_axis',(0.,0.,1.));
#17852=DIRECTION('ref_axis',(1.,-8.75189148499889E-13,0.));
#17853=DIRECTION('',(0.,0.,1.));
#17854=DIRECTION('center_axis',(0.,0.,1.));
#17855=DIRECTION('ref_axis',(1.,-8.75189148499889E-13,0.));
#17856=DIRECTION('',(0.,0.,1.));
#17857=DIRECTION('center_axis',(0.,0.,1.));
#17858=DIRECTION('ref_axis',(1.,-8.75189148499889E-13,0.));
#17859=DIRECTION('',(0.,0.,1.));
#17860=DIRECTION('center_axis',(0.,0.,1.));
#17861=DIRECTION('ref_axis',(1.,-8.75189148499889E-13,0.));
#17862=DIRECTION('',(0.,0.,1.));
#17863=DIRECTION('center_axis',(0.,0.,1.));
#17864=DIRECTION('ref_axis',(1.,-8.75189148499889E-13,0.));
#17865=DIRECTION('',(0.,0.,1.));
#17866=DIRECTION('center_axis',(0.,0.,1.));
#17867=DIRECTION('ref_axis',(1.,-8.75189148499889E-13,0.));
#17868=DIRECTION('',(0.,0.,1.));
#17869=DIRECTION('center_axis',(0.,0.,1.));
#17870=DIRECTION('ref_axis',(1.,-8.75189148499889E-13,0.));
#17871=DIRECTION('',(0.,0.,1.));
#17872=DIRECTION('center_axis',(0.,0.,1.));
#17873=DIRECTION('ref_axis',(1.,-8.75189148499889E-13,0.));
#17874=DIRECTION('',(0.,0.,1.));
#17875=DIRECTION('center_axis',(0.,0.,1.));
#17876=DIRECTION('ref_axis',(1.,-8.75189148499889E-13,0.));
#17877=DIRECTION('',(0.,0.,1.));
#17878=DIRECTION('center_axis',(0.,0.,1.));
#17879=DIRECTION('ref_axis',(1.,-8.75189148499889E-13,0.));
#17880=DIRECTION('',(0.,0.,1.));
#17881=DIRECTION('center_axis',(0.,0.,1.));
#17882=DIRECTION('ref_axis',(1.,-8.75189148499889E-13,0.));
#17883=DIRECTION('',(0.,0.,1.));
#17884=DIRECTION('center_axis',(0.,0.,1.));
#17885=DIRECTION('ref_axis',(1.,-8.75189148499889E-13,0.));
#17886=DIRECTION('',(0.,0.,1.));
#17887=DIRECTION('center_axis',(0.,0.,1.));
#17888=DIRECTION('ref_axis',(1.,-8.75189148499889E-13,0.));
#17889=DIRECTION('',(0.,0.,1.));
#17890=DIRECTION('center_axis',(0.,0.,1.));
#17891=DIRECTION('ref_axis',(1.,-8.75189148499889E-13,0.));
#17892=DIRECTION('',(0.,0.,1.));
#17893=DIRECTION('center_axis',(0.,0.,1.));
#17894=DIRECTION('ref_axis',(1.,-8.75189148499889E-13,0.));
#17895=DIRECTION('',(0.,0.,1.));
#17896=DIRECTION('center_axis',(0.,0.,1.));
#17897=DIRECTION('ref_axis',(1.,-8.75189148499889E-13,0.));
#17898=DIRECTION('',(0.,0.,1.));
#17899=DIRECTION('center_axis',(0.,0.,1.));
#17900=DIRECTION('ref_axis',(1.,-8.75189148499889E-13,0.));
#17901=DIRECTION('',(0.,0.,1.));
#17902=DIRECTION('center_axis',(0.,0.,1.));
#17903=DIRECTION('ref_axis',(1.,-8.75189148499889E-13,0.));
#17904=DIRECTION('',(0.,0.,1.));
#17905=DIRECTION('center_axis',(0.,0.,1.));
#17906=DIRECTION('ref_axis',(1.,-8.75189148499889E-13,0.));
#17907=DIRECTION('',(0.,0.,1.));
#17908=DIRECTION('center_axis',(0.,0.,1.));
#17909=DIRECTION('ref_axis',(1.,-8.75189148499889E-13,0.));
#17910=DIRECTION('',(0.,0.,1.));
#17911=DIRECTION('center_axis',(0.,0.,1.));
#17912=DIRECTION('ref_axis',(1.,-8.75189148499889E-13,0.));
#17913=DIRECTION('',(0.,0.,1.));
#17914=DIRECTION('center_axis',(0.,0.,1.));
#17915=DIRECTION('ref_axis',(1.,-8.75189148499889E-13,0.));
#17916=DIRECTION('',(0.,0.,1.));
#17917=DIRECTION('center_axis',(0.,0.,1.));
#17918=DIRECTION('ref_axis',(1.,-8.75189148499889E-13,0.));
#17919=DIRECTION('',(0.,0.,1.));
#17920=DIRECTION('center_axis',(0.,0.,1.));
#17921=DIRECTION('ref_axis',(1.,-8.75189148499889E-13,0.));
#17922=DIRECTION('',(0.,0.,1.));
#17923=DIRECTION('center_axis',(0.,0.,1.));
#17924=DIRECTION('ref_axis',(1.,-8.75189148499889E-13,0.));
#17925=DIRECTION('',(0.,0.,1.));
#17926=DIRECTION('center_axis',(0.,0.,1.));
#17927=DIRECTION('ref_axis',(1.,-8.75189148499889E-13,0.));
#17928=DIRECTION('',(0.,0.,1.));
#17929=DIRECTION('center_axis',(0.,0.,1.));
#17930=DIRECTION('ref_axis',(1.,-8.75189148499889E-13,0.));
#17931=DIRECTION('',(0.,0.,1.));
#17932=DIRECTION('center_axis',(0.,0.,1.));
#17933=DIRECTION('ref_axis',(1.,-8.75189148499889E-13,0.));
#17934=DIRECTION('',(0.,0.,1.));
#17935=DIRECTION('center_axis',(0.,0.,1.));
#17936=DIRECTION('ref_axis',(1.,-8.75189148499889E-13,0.));
#17937=DIRECTION('',(0.,0.,1.));
#17938=DIRECTION('center_axis',(0.,0.,1.));
#17939=DIRECTION('ref_axis',(1.,-8.75189148499889E-13,0.));
#17940=DIRECTION('',(0.,0.,1.));
#17941=DIRECTION('center_axis',(0.,0.,1.));
#17942=DIRECTION('ref_axis',(1.,-8.75189148499889E-13,0.));
#17943=DIRECTION('',(0.,0.,1.));
#17944=DIRECTION('center_axis',(0.,0.,1.));
#17945=DIRECTION('ref_axis',(1.,-8.75189148499889E-13,0.));
#17946=DIRECTION('',(0.,0.,1.));
#17947=DIRECTION('center_axis',(0.,0.,1.));
#17948=DIRECTION('ref_axis',(1.,-8.75189148499889E-13,0.));
#17949=DIRECTION('',(0.,0.,1.));
#17950=DIRECTION('center_axis',(0.,0.,1.));
#17951=DIRECTION('ref_axis',(1.,-8.75189148499889E-13,0.));
#17952=DIRECTION('',(0.,0.,1.));
#17953=DIRECTION('center_axis',(0.,0.,1.));
#17954=DIRECTION('ref_axis',(1.,-8.75189148499889E-13,0.));
#17955=DIRECTION('',(0.,0.,1.));
#17956=DIRECTION('center_axis',(0.,0.,1.));
#17957=DIRECTION('ref_axis',(1.,-8.75189148499889E-13,0.));
#17958=DIRECTION('',(0.,0.,1.));
#17959=DIRECTION('center_axis',(0.,0.,1.));
#17960=DIRECTION('ref_axis',(1.,-8.75189148499889E-13,0.));
#17961=DIRECTION('',(0.,0.,1.));
#17962=DIRECTION('center_axis',(0.,0.,1.));
#17963=DIRECTION('ref_axis',(1.,-8.75189148499889E-13,0.));
#17964=DIRECTION('',(0.,0.,1.));
#17965=DIRECTION('center_axis',(0.,0.,1.));
#17966=DIRECTION('ref_axis',(1.,-8.75189148499889E-13,0.));
#17967=DIRECTION('',(0.,0.,1.));
#17968=DIRECTION('center_axis',(0.,0.,1.));
#17969=DIRECTION('ref_axis',(1.,-8.75189148499889E-13,0.));
#17970=DIRECTION('',(0.,0.,1.));
#17971=DIRECTION('center_axis',(0.,0.,1.));
#17972=DIRECTION('ref_axis',(1.,-8.75189148499889E-13,0.));
#17973=DIRECTION('',(0.,0.,1.));
#17974=DIRECTION('center_axis',(0.,0.,1.));
#17975=DIRECTION('ref_axis',(1.,-8.75189148499889E-13,0.));
#17976=DIRECTION('',(0.,0.,1.));
#17977=DIRECTION('center_axis',(0.,0.,1.));
#17978=DIRECTION('ref_axis',(1.,-8.75189148499889E-13,0.));
#17979=DIRECTION('',(0.,0.,1.));
#17980=DIRECTION('center_axis',(0.,0.,1.));
#17981=DIRECTION('ref_axis',(1.,-8.75189148499889E-13,0.));
#17982=DIRECTION('',(0.,0.,1.));
#17983=DIRECTION('center_axis',(0.,0.,1.));
#17984=DIRECTION('ref_axis',(1.,-8.75189148499889E-13,0.));
#17985=DIRECTION('',(0.,0.,1.));
#17986=DIRECTION('center_axis',(0.,0.,1.));
#17987=DIRECTION('ref_axis',(1.,-8.75189148499889E-13,0.));
#17988=DIRECTION('',(0.,0.,1.));
#17989=DIRECTION('center_axis',(0.,0.,1.));
#17990=DIRECTION('ref_axis',(1.,-8.75189148499889E-13,0.));
#17991=DIRECTION('',(0.,0.,1.));
#17992=DIRECTION('center_axis',(0.,0.,1.));
#17993=DIRECTION('ref_axis',(1.,-8.75189148499889E-13,0.));
#17994=DIRECTION('center_axis',(0.,0.,-1.));
#17995=DIRECTION('ref_axis',(1.,-8.75189148499889E-13,0.));
#17996=DIRECTION('center_axis',(0.,0.,1.));
#17997=DIRECTION('ref_axis',(1.,0.,0.));
#17998=DIRECTION('center_axis',(0.,0.,-1.));
#17999=DIRECTION('ref_axis',(1.,0.,0.));
#18000=DIRECTION('center_axis',(0.,0.,1.));
#18001=DIRECTION('ref_axis',(1.,0.,0.));
#18002=DIRECTION('',(0.5,0.866025403784439,0.));
#18003=DIRECTION('',(-0.5,0.866025403784439,0.));
#18004=DIRECTION('',(-1.,1.20185167898973E-16,0.));
#18005=DIRECTION('',(-0.5,-0.866025403784439,0.));
#18006=DIRECTION('',(0.5,-0.866025403784439,0.));
#18007=DIRECTION('',(1.,-2.40370335797945E-16,0.));
#18008=DIRECTION('center_axis',(0.,0.,1.));
#18009=DIRECTION('ref_axis',(1.,0.,0.));
#18010=DIRECTION('',(0.5,0.866025403784439,0.));
#18011=DIRECTION('',(1.,-2.40370335797945E-16,0.));
#18012=DIRECTION('',(0.5,-0.866025403784439,0.));
#18013=DIRECTION('',(-0.5,-0.866025403784439,0.));
#18014=DIRECTION('',(-1.,1.20185167898973E-16,0.));
#18015=DIRECTION('',(-0.5,0.866025403784439,0.));
#18016=DIRECTION('center_axis',(0.,0.,-1.));
#18017=DIRECTION('ref_axis',(1.,0.,0.));
#18018=DIRECTION('center_axis',(-2.40370335797945E-16,-1.,0.));
#18019=DIRECTION('ref_axis',(1.,-2.40370335797945E-16,0.));
#18020=DIRECTION('',(0.,0.,1.));
#18021=DIRECTION('',(0.,0.,1.));
#18022=DIRECTION('center_axis',(-0.866025403784439,-0.5,0.));
#18023=DIRECTION('ref_axis',(0.5,-0.866025403784439,0.));
#18024=DIRECTION('',(0.,0.,1.));
#18025=DIRECTION('center_axis',(-0.866025403784439,0.5,0.));
#18026=DIRECTION('ref_axis',(-0.5,-0.866025403784439,0.));
#18027=DIRECTION('',(0.,0.,1.));
#18028=DIRECTION('center_axis',(1.20185167898973E-16,1.,0.));
#18029=DIRECTION('ref_axis',(-1.,1.20185167898973E-16,0.));
#18030=DIRECTION('',(0.,0.,1.));
#18031=DIRECTION('center_axis',(0.866025403784439,0.5,0.));
#18032=DIRECTION('ref_axis',(-0.5,0.866025403784439,0.));
#18033=DIRECTION('',(0.,0.,1.));
#18034=DIRECTION('center_axis',(0.866025403784439,-0.5,0.));
#18035=DIRECTION('ref_axis',(0.5,0.866025403784439,0.));
#18036=DIRECTION('center_axis',(0.,0.,1.));
#18037=DIRECTION('ref_axis',(1.,0.,0.));
#18038=DIRECTION('',(0.,0.,-1.));
#18039=DIRECTION('center_axis',(0.,0.,-1.));
#18040=DIRECTION('ref_axis',(1.,0.,0.));
#18041=DIRECTION('center_axis',(0.,0.,1.));
#18042=DIRECTION('ref_axis',(1.,0.,0.));
#18043=DIRECTION('center_axis',(6.12323399573677E-17,0.,1.));
#18044=DIRECTION('ref_axis',(1.,0.,0.));
#18045=DIRECTION('center_axis',(1.22464679914735E-16,-1.,0.));
#18046=DIRECTION('ref_axis',(-1.,-1.22464679914735E-16,0.));
#18047=DIRECTION('axis',(0.,0.,1.));
#18048=DIRECTION('refdir',(1.,0.,0.));
#18049=DIRECTION('center_axis',(0.,0.,-1.));
#18050=DIRECTION('ref_axis',(-0.346147419294793,0.938180134150982,0.));
#18051=DIRECTION('',(0.,0.,-1.));
#18052=DIRECTION('center_axis',(0.,0.,-1.));
#18053=DIRECTION('ref_axis',(1.,0.,0.));
#18054=DIRECTION('center_axis',(0.,0.,-1.));
#18055=DIRECTION('ref_axis',(1.,0.,0.));
#18056=DIRECTION('',(0.,0.,-1.));
#18057=DIRECTION('center_axis',(0.,0.,-1.));
#18058=DIRECTION('ref_axis',(1.,0.,0.));
#18059=DIRECTION('',(0.,0.,-1.));
#18060=DIRECTION('center_axis',(0.,0.,-1.));
#18061=DIRECTION('ref_axis',(1.,0.,0.));
#18062=DIRECTION('',(0.,0.,-1.));
#18063=DIRECTION('center_axis',(0.,0.,-1.));
#18064=DIRECTION('ref_axis',(1.,0.,0.));
#18065=DIRECTION('',(0.,0.,-1.));
#18066=DIRECTION('center_axis',(0.,0.,-1.));
#18067=DIRECTION('ref_axis',(1.,0.,0.));
#18068=DIRECTION('',(0.,0.,-1.));
#18069=DIRECTION('center_axis',(0.,0.,-1.));
#18070=DIRECTION('ref_axis',(1.,0.,0.));
#18071=DIRECTION('',(0.,0.,-1.));
#18072=DIRECTION('center_axis',(0.,0.,-1.));
#18073=DIRECTION('ref_axis',(0.938064160696058,-0.346461585774816,0.));
#18074=DIRECTION('',(0.,0.,-1.));
#18075=DIRECTION('center_axis',(0.,0.,-1.));
#18076=DIRECTION('ref_axis',(1.,0.,0.));
#18077=DIRECTION('center_axis',(0.,0.,-1.));
#18078=DIRECTION('ref_axis',(0.793491609261867,0.608581190993456,0.));
#18079=DIRECTION('',(1.22464679914735E-16,-2.66964461005383E-30,-1.));
#18080=DIRECTION('center_axis',(0.,0.,1.));
#18081=DIRECTION('ref_axis',(1.,-2.16768378774637E-14,0.));
#18082=DIRECTION('center_axis',(0.,0.,-1.));
#18083=DIRECTION('ref_axis',(1.,-2.16768378774637E-14,0.));
#18084=DIRECTION('',(1.22464679914735E-16,-2.66964461005383E-30,-1.));
#18085=DIRECTION('center_axis',(0.,0.,-1.));
#18086=DIRECTION('ref_axis',(1.,-2.16768378774637E-14,0.));
#18087=DIRECTION('',(1.22464679914735E-16,-2.66964461005383E-30,-1.));
#18088=DIRECTION('center_axis',(0.,0.,-1.));
#18089=DIRECTION('ref_axis',(1.,-2.16768378774637E-14,0.));
#18090=DIRECTION('',(1.22464679914735E-16,-2.66964461005383E-30,-1.));
#18091=DIRECTION('center_axis',(0.,0.,-1.));
#18092=DIRECTION('ref_axis',(1.,-2.16768378774637E-14,0.));
#18093=DIRECTION('',(1.22464679914735E-16,-2.66964461005383E-30,-1.));
#18094=DIRECTION('center_axis',(0.,0.,-1.));
#18095=DIRECTION('ref_axis',(1.,-2.16768378774637E-14,0.));
#18096=DIRECTION('',(1.22464679914735E-16,-2.66964461005383E-30,-1.));
#18097=DIRECTION('center_axis',(0.,0.,-1.));
#18098=DIRECTION('ref_axis',(1.,-2.16768378774637E-14,0.));
#18099=DIRECTION('',(1.22464679914735E-16,-2.66964461005383E-30,-1.));
#18100=DIRECTION('center_axis',(0.,0.,-1.));
#18101=DIRECTION('ref_axis',(-0.608751959302999,-0.793360606562211,0.));
#18102=DIRECTION('',(1.22464679914735E-16,-2.66964461005383E-30,-1.));
#18103=DIRECTION('center_axis',(0.,0.,-1.));
#18104=DIRECTION('ref_axis',(1.,-2.16768378774637E-14,0.));
#18105=DIRECTION('center_axis',(0.,0.,-1.));
#18106=DIRECTION('ref_axis',(1.,-2.16768378774637E-14,0.));
#18107=DIRECTION('center_axis',(0.,0.,1.));
#18108=DIRECTION('ref_axis',(1.,0.,0.));
#18109=DIRECTION('',(0.5,0.866025403784439,0.));
#18110=DIRECTION('',(-0.5,0.866025403784439,0.));
#18111=DIRECTION('',(-1.,0.,0.));
#18112=DIRECTION('',(-0.5,-0.866025403784439,0.));
#18113=DIRECTION('',(0.5,-0.866025403784439,0.));
#18114=DIRECTION('',(1.,-3.39346356420629E-16,0.));
#18115=DIRECTION('center_axis',(0.,0.,-1.));
#18116=DIRECTION('ref_axis',(1.,0.,0.));
#18117=DIRECTION('center_axis',(-3.39346356420629E-16,-1.,0.));
#18118=DIRECTION('ref_axis',(1.,-3.39346356420629E-16,0.));
#18119=DIRECTION('',(1.,-3.39346356420629E-16,0.));
#18120=DIRECTION('',(0.,0.,1.));
#18121=DIRECTION('',(0.,0.,1.));
#18122=DIRECTION('center_axis',(-0.866025403784439,-0.5,0.));
#18123=DIRECTION('ref_axis',(0.5,-0.866025403784439,0.));
#18124=DIRECTION('',(0.5,-0.866025403784439,0.));
#18125=DIRECTION('',(0.,0.,1.));
#18126=DIRECTION('center_axis',(-0.866025403784439,0.5,0.));
#18127=DIRECTION('ref_axis',(-0.5,-0.866025403784438,0.));
#18128=DIRECTION('',(-0.5,-0.866025403784439,0.));
#18129=DIRECTION('',(0.,0.,1.));
#18130=DIRECTION('center_axis',(0.,1.,0.));
#18131=DIRECTION('ref_axis',(-1.,0.,0.));
#18132=DIRECTION('',(-1.,0.,0.));
#18133=DIRECTION('',(0.,0.,1.));
#18134=DIRECTION('center_axis',(0.866025403784439,0.5,0.));
#18135=DIRECTION('ref_axis',(-0.5,0.866025403784439,0.));
#18136=DIRECTION('',(-0.5,0.866025403784439,0.));
#18137=DIRECTION('',(0.,0.,1.));
#18138=DIRECTION('center_axis',(0.866025403784439,-0.5,0.));
#18139=DIRECTION('ref_axis',(0.5,0.866025403784439,0.));
#18140=DIRECTION('',(0.5,0.866025403784439,0.));
#18141=DIRECTION('center_axis',(0.,0.,1.));
#18142=DIRECTION('ref_axis',(1.,0.,0.));
#18143=DIRECTION('axis',(0.,0.,1.));
#18144=DIRECTION('refdir',(1.,0.,0.));
#18145=DIRECTION('center_axis',(0.,0.,1.));
#18146=DIRECTION('ref_axis',(1.,0.,0.));
#18147=DIRECTION('center_axis',(0.,0.,-1.));
#18148=DIRECTION('ref_axis',(1.,0.,0.));
#18149=DIRECTION('',(0.,0.,-1.));
#18150=DIRECTION('center_axis',(0.,0.,-1.));
#18151=DIRECTION('ref_axis',(1.,0.,0.));
#18152=DIRECTION('center_axis',(0.,0.,1.));
#18153=DIRECTION('ref_axis',(1.,0.,0.));
#18154=DIRECTION('center_axis',(0.,0.,1.));
#18155=DIRECTION('ref_axis',(1.,0.,0.));
#18156=DIRECTION('',(0.,0.,-1.));
#18157=DIRECTION('center_axis',(0.,0.,1.));
#18158=DIRECTION('ref_axis',(1.,0.,0.));
#18159=DIRECTION('center_axis',(0.,0.,1.));
#18160=DIRECTION('ref_axis',(1.,0.,0.));
#18161=DIRECTION('center_axis',(0.,0.,1.));
#18162=DIRECTION('ref_axis',(1.,0.,0.));
#18163=DIRECTION('axis',(0.,0.,1.));
#18164=DIRECTION('refdir',(1.,0.,0.));
#18165=DIRECTION('center_axis',(0.,0.,1.));
#18166=DIRECTION('ref_axis',(1.,0.,0.));
#18167=DIRECTION('',(0.,0.,-1.));
#18168=DIRECTION('center_axis',(0.,0.,-1.));
#18169=DIRECTION('ref_axis',(1.,0.,0.));
#18170=DIRECTION('center_axis',(0.,0.,1.));
#18171=DIRECTION('ref_axis',(1.,0.,0.));
#18172=DIRECTION('',(0.,0.,-1.));
#18173=DIRECTION('center_axis',(0.,0.,1.));
#18174=DIRECTION('ref_axis',(1.,0.,0.));
#18175=DIRECTION('',(0.,0.,-1.));
#18176=DIRECTION('center_axis',(0.,0.,1.));
#18177=DIRECTION('ref_axis',(1.,0.,0.));
#18178=DIRECTION('',(0.,0.,-1.));
#18179=DIRECTION('center_axis',(0.,0.,1.));
#18180=DIRECTION('ref_axis',(1.,0.,0.));
#18181=DIRECTION('',(0.,0.,-1.));
#18182=DIRECTION('center_axis',(0.,0.,1.));
#18183=DIRECTION('ref_axis',(1.,0.,0.));
#18184=DIRECTION('',(0.,0.,-1.));
#18185=DIRECTION('center_axis',(0.,0.,1.));
#18186=DIRECTION('ref_axis',(1.,0.,0.));
#18187=DIRECTION('',(0.,0.,-1.));
#18188=DIRECTION('center_axis',(0.,0.,1.));
#18189=DIRECTION('ref_axis',(1.,0.,0.));
#18190=DIRECTION('',(0.,0.,-1.));
#18191=DIRECTION('center_axis',(0.,0.,1.));
#18192=DIRECTION('ref_axis',(1.,0.,0.));
#18193=DIRECTION('',(0.,0.,-1.));
#18194=DIRECTION('center_axis',(0.,0.,1.));
#18195=DIRECTION('ref_axis',(1.,0.,0.));
#18196=DIRECTION('',(0.,0.,-1.));
#18197=DIRECTION('center_axis',(0.,0.,1.));
#18198=DIRECTION('ref_axis',(1.,0.,0.));
#18199=DIRECTION('',(0.,0.,-1.));
#18200=DIRECTION('center_axis',(0.,0.,1.));
#18201=DIRECTION('ref_axis',(1.,0.,0.));
#18202=DIRECTION('',(0.,0.,-1.));
#18203=DIRECTION('center_axis',(0.,0.,1.));
#18204=DIRECTION('ref_axis',(1.,0.,0.));
#18205=DIRECTION('',(0.,0.,-1.));
#18206=DIRECTION('center_axis',(0.,0.,1.));
#18207=DIRECTION('ref_axis',(1.,0.,0.));
#18208=DIRECTION('',(0.,0.,-1.));
#18209=DIRECTION('center_axis',(0.,0.,1.));
#18210=DIRECTION('ref_axis',(1.,0.,0.));
#18211=DIRECTION('',(0.,0.,-1.));
#18212=DIRECTION('center_axis',(0.,0.,1.));
#18213=DIRECTION('ref_axis',(0.997339946684471,-0.0728905394918792,0.));
#18214=DIRECTION('',(0.,0.,1.));
#18215=DIRECTION('center_axis',(0.,0.,-1.));
#18216=DIRECTION('ref_axis',(1.,1.10476514494527E-13,0.));
#18217=DIRECTION('center_axis',(0.,0.,1.));
#18218=DIRECTION('ref_axis',(1.,1.10476514494527E-13,0.));
#18219=DIRECTION('',(0.,0.,1.));
#18220=DIRECTION('center_axis',(0.,0.,1.));
#18221=DIRECTION('ref_axis',(1.,1.10476514494527E-13,0.));
#18222=DIRECTION('',(0.,0.,1.));
#18223=DIRECTION('center_axis',(0.,0.,1.));
#18224=DIRECTION('ref_axis',(1.,1.10476514494527E-13,0.));
#18225=DIRECTION('',(0.,0.,1.));
#18226=DIRECTION('center_axis',(0.,0.,1.));
#18227=DIRECTION('ref_axis',(1.,1.10476514494527E-13,0.));
#18228=DIRECTION('',(0.,0.,1.));
#18229=DIRECTION('center_axis',(0.,0.,1.));
#18230=DIRECTION('ref_axis',(1.,1.10476514494527E-13,0.));
#18231=DIRECTION('',(0.,0.,1.));
#18232=DIRECTION('center_axis',(0.,0.,1.));
#18233=DIRECTION('ref_axis',(1.,1.10476514494527E-13,0.));
#18234=DIRECTION('',(0.,0.,1.));
#18235=DIRECTION('center_axis',(0.,0.,1.));
#18236=DIRECTION('ref_axis',(1.,1.10476514494527E-13,0.));
#18237=DIRECTION('',(0.,0.,1.));
#18238=DIRECTION('center_axis',(0.,0.,1.));
#18239=DIRECTION('ref_axis',(1.,1.10476514494527E-13,0.));
#18240=DIRECTION('',(0.,0.,1.));
#18241=DIRECTION('center_axis',(0.,0.,1.));
#18242=DIRECTION('ref_axis',(1.,1.10476514494527E-13,0.));
#18243=DIRECTION('',(0.,0.,1.));
#18244=DIRECTION('center_axis',(0.,0.,1.));
#18245=DIRECTION('ref_axis',(1.,1.10476514494527E-13,0.));
#18246=DIRECTION('',(0.,0.,1.));
#18247=DIRECTION('center_axis',(0.,0.,1.));
#18248=DIRECTION('ref_axis',(1.,1.10476514494527E-13,0.));
#18249=DIRECTION('',(0.,0.,1.));
#18250=DIRECTION('center_axis',(0.,0.,1.));
#18251=DIRECTION('ref_axis',(1.,1.10476514494527E-13,0.));
#18252=DIRECTION('',(0.,0.,1.));
#18253=DIRECTION('center_axis',(0.,0.,1.));
#18254=DIRECTION('ref_axis',(1.,1.10476514494527E-13,0.));
#18255=DIRECTION('',(0.,0.,1.));
#18256=DIRECTION('center_axis',(0.,0.,1.));
#18257=DIRECTION('ref_axis',(1.,1.10476514494527E-13,0.));
#18258=DIRECTION('',(0.,0.,1.));
#18259=DIRECTION('center_axis',(0.,0.,-1.));
#18260=DIRECTION('ref_axis',(1.,0.,0.));
#18261=DIRECTION('center_axis',(0.,0.,-1.));
#18262=DIRECTION('ref_axis',(1.,0.,0.));
#18263=DIRECTION('',(0.707106781186547,8.65956056235493E-17,0.707106781186548));
#18264=DIRECTION('center_axis',(0.,0.,1.));
#18265=DIRECTION('ref_axis',(1.,0.,0.));
#18266=DIRECTION('center_axis',(0.,0.,1.));
#18267=DIRECTION('ref_axis',(1.,1.10476514494527E-13,0.));
#18268=DIRECTION('center_axis',(0.,0.,-1.));
#18269=DIRECTION('ref_axis',(1.,1.10476514494527E-13,0.));
#18270=DIRECTION('center_axis',(0.,0.,1.));
#18271=DIRECTION('ref_axis',(1.,0.,0.));
#18272=DIRECTION('center_axis',(-1.92296268638356E-16,-1.,0.));
#18273=DIRECTION('ref_axis',(1.,-1.92296268638356E-16,0.));
#18274=DIRECTION('',(1.,-1.92296268638356E-16,0.));
#18275=DIRECTION('',(0.,0.,1.));
#18276=DIRECTION('',(1.,-1.92296268638356E-16,0.));
#18277=DIRECTION('',(0.,0.,1.));
#18278=DIRECTION('center_axis',(-0.866025403784439,-0.5,0.));
#18279=DIRECTION('ref_axis',(0.5,-0.866025403784439,0.));
#18280=DIRECTION('',(0.5,-0.866025403784439,0.));
#18281=DIRECTION('',(0.,0.,1.));
#18282=DIRECTION('',(0.5,-0.866025403784439,0.));
#18283=DIRECTION('center_axis',(-0.866025403784439,0.5,0.));
#18284=DIRECTION('ref_axis',(-0.5,-0.866025403784438,0.));
#18285=DIRECTION('',(-0.5,-0.866025403784438,0.));
#18286=DIRECTION('',(0.,0.,1.));
#18287=DIRECTION('',(-0.5,-0.866025403784439,0.));
#18288=DIRECTION('center_axis',(1.92296268638356E-16,1.,0.));
#18289=DIRECTION('ref_axis',(-1.,1.92296268638356E-16,0.));
#18290=DIRECTION('',(-1.,1.92296268638356E-16,0.));
#18291=DIRECTION('',(0.,0.,1.));
#18292=DIRECTION('',(-1.,1.92296268638356E-16,0.));
#18293=DIRECTION('center_axis',(0.866025403784439,0.5,0.));
#18294=DIRECTION('ref_axis',(-0.5,0.866025403784439,0.));
#18295=DIRECTION('',(-0.5,0.866025403784439,0.));
#18296=DIRECTION('',(0.,0.,1.));
#18297=DIRECTION('',(-0.5,0.866025403784439,0.));
#18298=DIRECTION('center_axis',(0.866025403784439,-0.5,0.));
#18299=DIRECTION('ref_axis',(0.5,0.866025403784439,0.));
#18300=DIRECTION('',(0.5,0.866025403784439,0.));
#18301=DIRECTION('',(0.5,0.866025403784439,0.));
#18302=DIRECTION('center_axis',(0.,0.,1.));
#18303=DIRECTION('ref_axis',(1.,0.,0.));
#18304=DIRECTION('center_axis',(0.,0.,1.));
#18305=DIRECTION('ref_axis',(1.,0.,0.));
#18306=DIRECTION('center_axis',(0.,0.,1.));
#18307=DIRECTION('ref_axis',(1.,0.,0.));
#18308=DIRECTION('center_axis',(0.,0.,1.));
#18309=DIRECTION('ref_axis',(1.,0.,0.));
#18310=DIRECTION('',(0.,0.,-1.));
#18311=DIRECTION('center_axis',(0.,0.,1.));
#18312=DIRECTION('ref_axis',(1.,0.,0.));
#18313=DIRECTION('center_axis',(0.,0.,1.));
#18314=DIRECTION('ref_axis',(1.,0.,0.));
#18315=DIRECTION('center_axis',(0.,0.,1.));
#18316=DIRECTION('ref_axis',(1.,0.,0.));
#18317=DIRECTION('axis',(0.,0.,1.));
#18318=DIRECTION('refdir',(1.,0.,0.));
#18319=DIRECTION('center_axis',(0.,0.,1.));
#18320=DIRECTION('ref_axis',(1.,0.,0.));
#18321=DIRECTION('center_axis',(0.,0.,-1.));
#18322=DIRECTION('ref_axis',(1.,0.,0.));
#18323=DIRECTION('',(0.,0.,-1.));
#18324=DIRECTION('center_axis',(0.,0.,-1.));
#18325=DIRECTION('ref_axis',(1.,0.,0.));
#18326=DIRECTION('center_axis',(0.,0.,1.));
#18327=DIRECTION('ref_axis',(1.,0.,0.));
#18328=DIRECTION('center_axis',(0.,0.,1.));
#18329=DIRECTION('ref_axis',(1.,0.,0.));
#18330=DIRECTION('',(0.,0.,-1.));
#18331=DIRECTION('center_axis',(0.,0.,1.));
#18332=DIRECTION('ref_axis',(1.,0.,0.));
#18333=DIRECTION('center_axis',(0.,0.,1.));
#18334=DIRECTION('ref_axis',(1.,0.,0.));
#18335=DIRECTION('center_axis',(0.,0.,1.));
#18336=DIRECTION('ref_axis',(1.,0.,0.));
#18337=DIRECTION('',(0.,0.,1.));
#18338=DIRECTION('',(1.,0.,0.));
#18339=DIRECTION('',(0.,0.,1.));
#18340=DIRECTION('',(1.,0.,0.));
#18341=DIRECTION('',(0.,-1.22464679914735E-16,-1.));
#18342=DIRECTION('',(1.,0.,0.));
#18343=DIRECTION('',(0.,0.,1.));
#18344=DIRECTION('',(1.,0.,0.));
#18345=DIRECTION('',(0.,0.,1.));
#18346=DIRECTION('',(1.,0.,0.));
#18347=DIRECTION('',(0.,0.,1.));
#18348=DIRECTION('',(1.,0.,0.));
#18349=DIRECTION('',(0.,0.,1.));
#18350=DIRECTION('',(-1.,1.22464679914735E-16,0.));
#18351=DIRECTION('',(0.,0.,1.));
#18352=DIRECTION('',(1.,0.,0.));
#18353=DIRECTION('',(0.,0.,1.));
#18354=DIRECTION('',(1.,0.,0.));
#18355=DIRECTION('',(0.,-1.22464679914735E-16,-1.));
#18356=DIRECTION('',(1.,0.,0.));
#18357=DIRECTION('',(0.,0.,1.));
#18358=DIRECTION('',(1.,0.,0.));
#18359=DIRECTION('',(0.,-1.22464679914735E-16,-1.));
#18360=DIRECTION('',(1.,0.,0.));
#18361=DIRECTION('',(0.,0.,1.));
#18362=DIRECTION('',(1.,0.,0.));
#18363=DIRECTION('',(0.,-1.22464679914735E-16,-1.));
#18364=DIRECTION('',(1.,0.,0.));
#18365=DIRECTION('',(0.,0.,1.));
#18366=DIRECTION('',(1.,0.,0.));
#18367=DIRECTION('',(0.,0.,1.));
#18368=DIRECTION('',(1.,0.,0.));
#18369=DIRECTION('',(0.,0.,1.));
#18370=DIRECTION('',(1.,0.,0.));
#18371=DIRECTION('',(0.,0.,1.));
#18372=DIRECTION('',(1.,0.,0.));
#18373=DIRECTION('',(0.,0.,1.));
#18374=DIRECTION('',(1.,0.,0.));
#18375=DIRECTION('',(0.,0.,1.));
#18376=DIRECTION('',(1.,0.,0.));
#18377=CARTESIAN_POINT('',(0.,0.,0.));
#18378=CARTESIAN_POINT('',(0.,0.,0.));
#18379=CARTESIAN_POINT('',(0.,0.,0.));
#18380=CARTESIAN_POINT('Origin',(16.,-21.,0.));
#18381=CARTESIAN_POINT('',(16.,-21.,0.));
#18382=CARTESIAN_POINT('',(-16.,-21.,0.));
#18383=CARTESIAN_POINT('',(-16.,-21.,0.));
#18384=CARTESIAN_POINT('',(-16.,-21.,600.));
#18385=CARTESIAN_POINT('',(-16.,-21.,0.));
#18386=CARTESIAN_POINT('',(16.,-21.,600.));
#18387=CARTESIAN_POINT('',(-16.,-21.,600.));
#18388=CARTESIAN_POINT('',(16.,-21.,0.));
#18389=CARTESIAN_POINT('Origin',(16.,21.,0.));
#18390=CARTESIAN_POINT('',(16.,21.,0.));
#18391=CARTESIAN_POINT('',(16.,-21.,0.));
#18392=CARTESIAN_POINT('',(16.,21.,600.));
#18393=CARTESIAN_POINT('',(16.,-21.,600.));
#18394=CARTESIAN_POINT('',(16.,21.,0.));
#18395=CARTESIAN_POINT('Origin',(-16.,21.,0.));
#18396=CARTESIAN_POINT('',(-16.,21.,0.));
#18397=CARTESIAN_POINT('',(16.,21.,0.));
#18398=CARTESIAN_POINT('',(-16.,21.,600.));
#18399=CARTESIAN_POINT('',(16.,21.,600.));
#18400=CARTESIAN_POINT('',(-16.,21.,0.));
#18401=CARTESIAN_POINT('Origin',(-16.,-21.,0.));
#18402=CARTESIAN_POINT('',(-16.,21.,0.));
#18403=CARTESIAN_POINT('',(-16.,21.,600.));
#18404=CARTESIAN_POINT('Origin',(20.,25.,0.));
#18405=CARTESIAN_POINT('',(20.,25.,0.));
#18406=CARTESIAN_POINT('',(-20.,25.,0.));
#18407=CARTESIAN_POINT('',(20.,25.,0.));
#18408=CARTESIAN_POINT('',(-20.,25.,600.));
#18409=CARTESIAN_POINT('',(-20.,25.,0.));
#18410=CARTESIAN_POINT('',(20.,25.,600.));
#18411=CARTESIAN_POINT('',(20.,25.,600.));
#18412=CARTESIAN_POINT('',(20.,25.,0.));
#18413=CARTESIAN_POINT('Origin',(20.,-25.,0.));
#18414=CARTESIAN_POINT('',(20.,-25.,0.));
#18415=CARTESIAN_POINT('',(20.,-25.,0.));
#18416=CARTESIAN_POINT('',(20.,-25.,600.));
#18417=CARTESIAN_POINT('',(20.,-25.,600.));
#18418=CARTESIAN_POINT('',(20.,-25.,0.));
#18419=CARTESIAN_POINT('Origin',(-20.,-25.,0.));
#18420=CARTESIAN_POINT('',(-20.,-25.,0.));
#18421=CARTESIAN_POINT('',(-20.,-25.,0.));
#18422=CARTESIAN_POINT('',(-20.,-25.,600.));
#18423=CARTESIAN_POINT('',(-20.,-25.,600.));
#18424=CARTESIAN_POINT('',(-20.,-25.,0.));
#18425=CARTESIAN_POINT('Origin',(-20.,25.,0.));
#18426=CARTESIAN_POINT('',(-20.,25.,0.));
#18427=CARTESIAN_POINT('',(-20.,25.,600.));
#18428=CARTESIAN_POINT('Origin',(0.,0.,600.));
#18429=CARTESIAN_POINT('Origin',(0.,0.,0.));
#18430=CARTESIAN_POINT('',(0.,0.,0.));
#18431=CARTESIAN_POINT('Origin',(16.,-21.,0.));
#18432=CARTESIAN_POINT('',(16.,-21.,0.));
#18433=CARTESIAN_POINT('',(-16.,-21.,0.));
#18434=CARTESIAN_POINT('',(-16.,-21.,0.));
#18435=CARTESIAN_POINT('',(-16.,-21.,400.));
#18436=CARTESIAN_POINT('',(-16.,-21.,0.));
#18437=CARTESIAN_POINT('',(16.,-21.,400.));
#18438=CARTESIAN_POINT('',(-16.,-21.,400.));
#18439=CARTESIAN_POINT('',(16.,-21.,0.));
#18440=CARTESIAN_POINT('Origin',(16.,21.,0.));
#18441=CARTESIAN_POINT('',(16.,21.,0.));
#18442=CARTESIAN_POINT('',(16.,-21.,0.));
#18443=CARTESIAN_POINT('',(16.,21.,400.));
#18444=CARTESIAN_POINT('',(16.,-21.,400.));
#18445=CARTESIAN_POINT('',(16.,21.,0.));
#18446=CARTESIAN_POINT('Origin',(-16.,21.,0.));
#18447=CARTESIAN_POINT('',(-16.,21.,0.));
#18448=CARTESIAN_POINT('',(16.,21.,0.));
#18449=CARTESIAN_POINT('',(-16.,21.,400.));
#18450=CARTESIAN_POINT('',(16.,21.,400.));
#18451=CARTESIAN_POINT('',(-16.,21.,0.));
#18452=CARTESIAN_POINT('Origin',(-16.,-21.,0.));
#18453=CARTESIAN_POINT('',(-16.,21.,0.));
#18454=CARTESIAN_POINT('',(-16.,21.,400.));
#18455=CARTESIAN_POINT('Origin',(20.,25.,0.));
#18456=CARTESIAN_POINT('',(20.,25.,0.));
#18457=CARTESIAN_POINT('',(-20.,25.,0.));
#18458=CARTESIAN_POINT('',(20.,25.,0.));
#18459=CARTESIAN_POINT('',(-20.,25.,400.));
#18460=CARTESIAN_POINT('',(-20.,25.,0.));
#18461=CARTESIAN_POINT('',(20.,25.,400.));
#18462=CARTESIAN_POINT('',(20.,25.,400.));
#18463=CARTESIAN_POINT('',(20.,25.,0.));
#18464=CARTESIAN_POINT('Origin',(20.,-25.,0.));
#18465=CARTESIAN_POINT('',(20.,-25.,0.));
#18466=CARTESIAN_POINT('',(20.,-25.,0.));
#18467=CARTESIAN_POINT('',(20.,-25.,400.));
#18468=CARTESIAN_POINT('',(20.,-25.,400.));
#18469=CARTESIAN_POINT('',(20.,-25.,0.));
#18470=CARTESIAN_POINT('Origin',(-20.,-25.,0.));
#18471=CARTESIAN_POINT('',(-20.,-25.,0.));
#18472=CARTESIAN_POINT('',(-20.,-25.,0.));
#18473=CARTESIAN_POINT('',(-20.,-25.,400.));
#18474=CARTESIAN_POINT('',(-20.,-25.,400.));
#18475=CARTESIAN_POINT('',(-20.,-25.,0.));
#18476=CARTESIAN_POINT('Origin',(-20.,25.,0.));
#18477=CARTESIAN_POINT('',(-20.,25.,0.));
#18478=CARTESIAN_POINT('',(-20.,25.,400.));
#18479=CARTESIAN_POINT('Origin',(0.,0.,400.));
#18480=CARTESIAN_POINT('Origin',(0.,0.,0.));
#18481=CARTESIAN_POINT('',(0.,0.,0.));
#18482=CARTESIAN_POINT('Origin',(35.,35.,4.));
#18483=CARTESIAN_POINT('',(31.4879724201494,34.9998624352662,0.387416697508018));
#18484=CARTESIAN_POINT('',(31.4848003100606,34.9953496614248,0.112583302491981));
#18485=CARTESIAN_POINT('',(31.4825,35.,4.));
#18486=CARTESIAN_POINT('',(32.3264680662286,37.2858331630075,0.));
#18487=CARTESIAN_POINT('Ctrl Pts',(31.4848003100606,34.9953496614248,0.112583302491981));
#18488=CARTESIAN_POINT('Ctrl Pts',(31.491976688325,35.8232723665277,0.0750555349946529));
#18489=CARTESIAN_POINT('Ctrl Pts',(31.7874825103136,36.6554305951821,0.0375277674973252));
#18490=CARTESIAN_POINT('Ctrl Pts',(32.3264680662287,37.2858331630075,-2.22044604925031E-15));
#18491=CARTESIAN_POINT('',(37.6785012740241,37.2890246412443,7.00840805882243E-15));
#18492=CARTESIAN_POINT('Origin',(35.,35.,0.));
#18493=CARTESIAN_POINT('Ctrl Pts',(37.6785244495407,37.2890395253442,4.78783679369599E-15));
#18494=CARTESIAN_POINT('Ctrl Pts',(36.9607517209778,38.1233243316157,0.0499978774624456));
#18495=CARTESIAN_POINT('Ctrl Pts',(35.818670130213,38.598920544762,0.0999957549248864));
#18496=CARTESIAN_POINT('Ctrl Pts',(34.7217021974699,38.5118549254553,0.149993632387327));
#18497=CARTESIAN_POINT('Ctrl Pts',(33.5734927541699,38.4207223013458,0.202327008171411));
#18498=CARTESIAN_POINT('Ctrl Pts',(32.4747101009944,37.7131340510847,0.254660383955495));
#18499=CARTESIAN_POINT('Ctrl Pts',(31.9173289273845,36.7055535968161,0.306993759739579));
#18500=CARTESIAN_POINT('Ctrl Pts',(31.6318117612872,36.1894229315936,0.333801405662392));
#18501=CARTESIAN_POINT('Ctrl Pts',(31.4883570437126,35.5945750322157,0.360609051585205));
#18502=CARTESIAN_POINT('Ctrl Pts',(31.4879724201494,34.9998624352662,0.387416697508018));
#18503=CARTESIAN_POINT('Origin',(35.,35.,4.));
#18504=CARTESIAN_POINT('',(31.4787691259179,34.9978480355345,1.38741669750802));
#18505=CARTESIAN_POINT('',(31.4779837004207,35.0016823853973,1.11258330249198));
#18506=CARTESIAN_POINT('',(31.4825,35.,4.));
#18507=CARTESIAN_POINT('Ctrl Pts',(31.4779837004207,35.0016823853973,1.11258330249198));
#18508=CARTESIAN_POINT('Ctrl Pts',(31.4773936874682,35.1013890235937,1.10805583214991));
#18509=CARTESIAN_POINT('Ctrl Pts',(31.4812693590031,35.201048825548,1.10352836180784));
#18510=CARTESIAN_POINT('Ctrl Pts',(31.4897612702936,35.3003133216161,1.09900089146578));
#18511=CARTESIAN_POINT('Ctrl Pts',(31.5879199220602,36.4477192198909,1.04666751568169));
#18512=CARTESIAN_POINT('Ctrl Pts',(32.3028647460417,37.5423074099748,0.994334139897606));
#18513=CARTESIAN_POINT('Ctrl Pts',(33.3140597553874,38.0934397445863,0.942000764113521));
#18514=CARTESIAN_POINT('Ctrl Pts',(34.3252547647332,38.6445720791978,0.889667388329437));
#18515=CARTESIAN_POINT('Ctrl Pts',(35.632699959443,38.652248558337,0.837334012545353));
#18516=CARTESIAN_POINT('Ctrl Pts',(36.6501699298679,38.1127741860318,0.785000636761269));
#18517=CARTESIAN_POINT('Ctrl Pts',(37.6676399002927,37.5732998137267,0.732667260977184));
#18518=CARTESIAN_POINT('Ctrl Pts',(38.3951346464326,36.4866745899774,0.680333885193099));
#18519=CARTESIAN_POINT('Ctrl Pts',(38.5065308772508,35.3406022936711,0.628000509409014));
#18520=CARTESIAN_POINT('Ctrl Pts',(38.617927108069,34.1945299973649,0.57566713362493));
#18521=CARTESIAN_POINT('Ctrl Pts',(38.1132248235656,32.9890106285018,0.523333757840846));
#18522=CARTESIAN_POINT('Ctrl Pts',(37.2186051779362,32.2635143561234,0.471000382056762));
#18523=CARTESIAN_POINT('Ctrl Pts',(36.3239855323068,31.538018083745,0.418667006272677));
#18524=CARTESIAN_POINT('Ctrl Pts',(35.0394485255514,31.2925449078513,0.366333630488592));
#18525=CARTESIAN_POINT('Ctrl Pts',(33.9411234140671,31.6392615363868,0.314000254704508));
#18526=CARTESIAN_POINT('Ctrl Pts',(32.8427983025828,31.9859781649222,0.261666878920424));
#18527=CARTESIAN_POINT('Ctrl Pts',(31.9306850863697,32.9248845978868,0.20933350313634));
#18528=CARTESIAN_POINT('Ctrl Pts',(31.6136954419349,34.0300704557469,0.157000127352256));
#18529=CARTESIAN_POINT('Ctrl Pts',(31.5240160655112,34.3427380154138,0.142194519065497));
#18530=CARTESIAN_POINT('Ctrl Pts',(31.481969055963,34.6687142103727,0.127388910778739));
#18531=CARTESIAN_POINT('Ctrl Pts',(31.4848003100606,34.9953496614248,0.112583302491981));
#18532=CARTESIAN_POINT('Ctrl Pts',(31.4879724201494,34.9998624352662,0.387416697508018));
#18533=CARTESIAN_POINT('Ctrl Pts',(31.4876061889182,34.4335884275247,0.41294242736929));
#18534=CARTESIAN_POINT('Ctrl Pts',(31.6169542536305,33.8674370915364,0.438468157230561));
#18535=CARTESIAN_POINT('Ctrl Pts',(31.8768865080858,33.3694813094911,0.463993887091832));
#18536=CARTESIAN_POINT('Ctrl Pts',(32.4098049564414,32.3485621347107,0.516327262875917));
#18537=CARTESIAN_POINT('Ctrl Pts',(33.4916215471969,31.6142964434261,0.568660638660002));
#18538=CARTESIAN_POINT('Ctrl Pts',(34.6371338346999,31.4957027110504,0.620994014444087));
#18539=CARTESIAN_POINT('Ctrl Pts',(35.7826461222029,31.3771089786747,0.673327390228171));
#18540=CARTESIAN_POINT('Ctrl Pts',(36.9918541064533,31.8741872052079,0.725660766012256));
#18541=CARTESIAN_POINT('Ctrl Pts',(37.7226853676378,32.7641657941898,0.77799414179634));
#18542=CARTESIAN_POINT('Ctrl Pts',(38.4535166288223,33.6541443831717,0.830327517580425));
#18543=CARTESIAN_POINT('Ctrl Pts',(38.7059711669407,34.9370233346023,0.882660893364508));
#18544=CARTESIAN_POINT('Ctrl Pts',(38.3668191926393,36.0375701678912,0.934994269148593));
#18545=CARTESIAN_POINT('Ctrl Pts',(38.0276672183379,37.13811700118,0.987327644932677));
#18546=CARTESIAN_POINT('Ctrl Pts',(37.0969087316166,38.0563317163271,1.03966102071676));
#18547=CARTESIAN_POINT('Ctrl Pts',(35.9918739069821,38.3805519391724,1.09199439650085));
#18548=CARTESIAN_POINT('Ctrl Pts',(34.8868390823475,38.7047721620176,1.14432777228493));
#18549=CARTESIAN_POINT('Ctrl Pts',(33.6075279197997,38.4349978925611,1.19666114806902));
#18550=CARTESIAN_POINT('Ctrl Pts',(32.727515719297,37.6921720072953,1.2489945238531));
#18551=CARTESIAN_POINT('Ctrl Pts',(31.9516360834601,37.0372453176186,1.29513524840474));
#18552=CARTESIAN_POINT('Ctrl Pts',(31.4861477200874,36.0145964274628,1.34127597295638));
#18553=CARTESIAN_POINT('Ctrl Pts',(31.4787691259179,34.9978480355345,1.38741669750802));
#18554=CARTESIAN_POINT('Origin',(35.,35.,4.));
#18555=CARTESIAN_POINT('',(31.4830373600778,35.0030273041289,2.38741669750802));
#18556=CARTESIAN_POINT('',(31.4877387493273,35.0007919718047,2.11258330249198));
#18557=CARTESIAN_POINT('',(31.4825,35.,4.));
#18558=CARTESIAN_POINT('Ctrl Pts',(31.4877387493273,35.0007919718047,2.11258330249198));
#18559=CARTESIAN_POINT('Ctrl Pts',(31.4866495532798,35.5300199293211,2.08872275352109));
#18560=CARTESIAN_POINT('Ctrl Pts',(31.5990326814287,36.0588086783673,2.06486220455019));
#18561=CARTESIAN_POINT('Ctrl Pts',(31.8273024854561,36.5316518026084,2.0410016555793));
#18562=CARTESIAN_POINT('Ctrl Pts',(32.3279669692824,37.5687392953569,1.98866827979521));
#18563=CARTESIAN_POINT('Ctrl Pts',(33.3861125458452,38.3366963827873,1.93633490401113));
#18564=CARTESIAN_POINT('Ctrl Pts',(34.5273147643209,38.4912077048459,1.88400152822704));
#18565=CARTESIAN_POINT('Ctrl Pts',(35.6685169827965,38.6457190269045,1.83166815244296));
#18566=CARTESIAN_POINT('Ctrl Pts',(36.8927758431849,38.1867845835912,1.77933477665887));
#18567=CARTESIAN_POINT('Ctrl Pts',(37.6511886219643,37.3201660399649,1.72700140087479));
#18568=CARTESIAN_POINT('Ctrl Pts',(38.4096014007438,36.4535474963386,1.6746680250907));
#18569=CARTESIAN_POINT('Ctrl Pts',(38.7021680979142,35.1792448523993,1.62233464930662));
#18570=CARTESIAN_POINT('Ctrl Pts',(38.3977158188189,34.0686054522412,1.57000127352253));
#18571=CARTESIAN_POINT('Ctrl Pts',(38.0932635397237,32.9579660520831,1.51766789773845));
#18572=CARTESIAN_POINT('Ctrl Pts',(37.1917922843629,32.0109898957062,1.46533452195437));
#18573=CARTESIAN_POINT('Ctrl Pts',(36.0974794284194,31.6522428960312,1.41300114617028));
#18574=CARTESIAN_POINT('Ctrl Pts',(35.0031665724759,31.2934958963563,1.3606677703862));
#18575=CARTESIAN_POINT('Ctrl Pts',(33.7160121159498,31.5229780533832,1.30833439460211));
#18576=CARTESIAN_POINT('Ctrl Pts',(32.8131211274626,32.2378309351295,1.25600101881803));
#18577=CARTESIAN_POINT('Ctrl Pts',(31.9883411362357,32.8908403914793,1.20819511337601));
#18578=CARTESIAN_POINT('Ctrl Pts',(31.4842136922894,33.9488723706596,1.160389207934));
#18579=CARTESIAN_POINT('Ctrl Pts',(31.4779837004207,35.0016823853973,1.11258330249198));
#18580=CARTESIAN_POINT('Ctrl Pts',(31.4787691259179,34.9978480355345,1.38741669750802));
#18581=CARTESIAN_POINT('Ctrl Pts',(31.4777788280689,34.86138792912,1.39360934874046));
#18582=CARTESIAN_POINT('Ctrl Pts',(31.4850404305936,34.725034107982,1.39980199997291));
#18583=CARTESIAN_POINT('Ctrl Pts',(31.5009110513053,34.5896898261078,1.40599465120535));
#18584=CARTESIAN_POINT('Ctrl Pts',(31.6350318222736,33.445911031261,1.45832802698944));
#18585=CARTESIAN_POINT('Ctrl Pts',(32.3839866026675,32.3742309426426,1.51066140277352));
#18586=CARTESIAN_POINT('Ctrl Pts',(33.411975462032,31.855139584126,1.56299477855761));
#18587=CARTESIAN_POINT('Ctrl Pts',(34.4399643213965,31.3360482256093,1.61532815434169));
#18588=CARTESIAN_POINT('Ctrl Pts',(35.7469872597314,31.3695455971944,1.66766153012578));
#18589=CARTESIAN_POINT('Ctrl Pts',(36.7470354950296,31.9406144231743,1.71999490590986));
#18590=CARTESIAN_POINT('Ctrl Pts',(37.7470837303277,32.5116832491543,1.77232828169395));
#18591=CARTESIAN_POINT('Ctrl Pts',(38.4401572625891,33.620323529529,1.82466165747803));
#18592=CARTESIAN_POINT('Ctrl Pts',(38.5155126426898,34.7694703662421,1.87699503326212));
#18593=CARTESIAN_POINT('Ctrl Pts',(38.5908680227905,35.9186172029552,1.9293284090462));
#18594=CARTESIAN_POINT('Ctrl Pts',(38.0485052507305,37.1082705960066,1.98166178483028));
#18595=CARTESIAN_POINT('Ctrl Pts',(37.1315955779125,37.8050440926957,2.03399516061437));
#18596=CARTESIAN_POINT('Ctrl Pts',(36.2146859050945,38.5018175893848,2.08632853639845));
#18597=CARTESIAN_POINT('Ctrl Pts',(34.9232293315183,38.7057111897115,2.13866191218254));
#18598=CARTESIAN_POINT('Ctrl Pts',(33.836256457425,38.3253080449544,2.19099528796662));
#18599=CARTESIAN_POINT('Ctrl Pts',(32.7492835833317,37.9449049001973,2.24332866375071));
#18600=CARTESIAN_POINT('Ctrl Pts',(31.8667944087212,36.9802050103563,2.29566203953479));
#18601=CARTESIAN_POINT('Ctrl Pts',(31.5844572622636,35.8637362853384,2.34799541531888));
#18602=CARTESIAN_POINT('Ctrl Pts',(31.5135650119789,35.583401298313,2.36113584271526));
#18603=CARTESIAN_POINT('Ctrl Pts',(31.4805102901148,35.2934978064005,2.37427627011164));
#18604=CARTESIAN_POINT('Ctrl Pts',(31.4830373600778,35.0030273041289,2.38741669750802));
#18605=CARTESIAN_POINT('Origin',(35.,35.,4.));
#18606=CARTESIAN_POINT('',(31.4866348863052,34.9979909502101,3.38741669750802));
#18607=CARTESIAN_POINT('',(31.48047694743,34.9972296622465,3.11258330249198));
#18608=CARTESIAN_POINT('',(31.4825,35.,4.));
#18609=CARTESIAN_POINT('Ctrl Pts',(31.48047694743,34.9972296622465,3.11258330249198));
#18610=CARTESIAN_POINT('Ctrl Pts',(31.4887007318231,35.9502403897084,3.06938967489226));
#18611=CARTESIAN_POINT('Ctrl Pts',(31.8903810058125,36.9093635615769,3.02619604729254));
#18612=CARTESIAN_POINT('Ctrl Pts',(32.5815433671812,37.5618418521763,2.98300241969282));
#18613=CARTESIAN_POINT('Ctrl Pts',(33.4189553095288,38.352384195351,2.93066904390873));
#18614=CARTESIAN_POINT('Ctrl Pts',(34.6813192114488,38.6927800566904,2.87833566812465));
#18615=CARTESIAN_POINT('Ctrl Pts',(35.8026481651385,38.4304113471867,2.82600229234057));
#18616=CARTESIAN_POINT('Ctrl Pts',(36.9239771188282,38.1680426376829,2.77366891655648));
#18617=CARTESIAN_POINT('Ctrl Pts',(37.9042711242876,37.3029093573359,2.7213355407724));
#18618=CARTESIAN_POINT('Ctrl Pts',(38.3040106560533,36.2228981053939,2.66900216498831));
#18619=CARTESIAN_POINT('Ctrl Pts',(38.703750187819,35.1428868534519,2.61666878920423));
#18620=CARTESIAN_POINT('Ctrl Pts',(38.5229352458909,33.8479976299149,2.56433541342014));
#18621=CARTESIAN_POINT('Ctrl Pts',(37.8426350886114,32.9188003439573,2.51200203763606));
#18622=CARTESIAN_POINT('Ctrl Pts',(37.1623349313319,31.9896030579996,2.45966866185197));
#18623=CARTESIAN_POINT('Ctrl Pts',(35.9825495587008,31.4260977096214,2.40733528606789));
#18624=CARTESIAN_POINT('Ctrl Pts',(34.8322413779487,31.4809343941795,2.3550019102838));
#18625=CARTESIAN_POINT('Ctrl Pts',(33.6819331971966,31.5357710787376,2.30266853449972));
#18626=CARTESIAN_POINT('Ctrl Pts',(32.5611022083236,32.208949796232,2.25033515871564));
#18627=CARTESIAN_POINT('Ctrl Pts',(31.9722784094319,33.1986481040126,2.19800178293155));
#18628=CARTESIAN_POINT('Ctrl Pts',(31.6519192161228,33.7371096133752,2.16952895611836));
#18629=CARTESIAN_POINT('Ctrl Pts',(31.4890384885104,34.3692635020513,2.14105612930517));
#18630=CARTESIAN_POINT('Ctrl Pts',(31.4877387493273,35.0007919718047,2.11258330249198));
#18631=CARTESIAN_POINT('Ctrl Pts',(31.4830373600778,35.0030273041289,2.38741669750802));
#18632=CARTESIAN_POINT('Ctrl Pts',(31.4905746584961,34.1366631395343,2.42660964589572));
#18633=CARTESIAN_POINT('Ctrl Pts',(31.8146491184789,33.2652548262212,2.46580259428343));
#18634=CARTESIAN_POINT('Ctrl Pts',(32.3954080438652,32.6276439552295,2.50499554267113));
#18635=CARTESIAN_POINT('Ctrl Pts',(33.1708810902294,31.7762579103332,2.55732891845521));
#18636=CARTESIAN_POINT('Ctrl Pts',(34.4040123012624,31.3417233807355,2.6096622942393));
#18637=CARTESIAN_POINT('Ctrl Pts',(35.5419214016919,31.5188660285384,2.66199567002338));
#18638=CARTESIAN_POINT('Ctrl Pts',(36.6798305021214,31.6960086763413,2.71432904580747));
#18639=CARTESIAN_POINT('Ctrl Pts',(37.7225174919474,32.4848285015448,2.76666242159155));
#18640=CARTESIAN_POINT('Ctrl Pts',(38.2024886486778,33.5316543411059,2.81899579737563));
#18641=CARTESIAN_POINT('Ctrl Pts',(38.6824598054083,34.5784801806669,2.87132917315972));
#18642=CARTESIAN_POINT('Ctrl Pts',(38.5997151290432,35.8833120345855,2.9236625489438));
#18643=CARTESIAN_POINT('Ctrl Pts',(37.9913535966355,36.8611222874319,2.97599592472789));
#18644=CARTESIAN_POINT('Ctrl Pts',(37.3829920642279,37.8389325402782,3.02832930051197));
#18645=CARTESIAN_POINT('Ctrl Pts',(36.2490136757777,38.4897211920522,3.08066267629606));
#18646=CARTESIAN_POINT('Ctrl Pts',(35.0978430789634,38.5217040264218,3.13299605208014));
#18647=CARTESIAN_POINT('Ctrl Pts',(33.946672482149,38.5536868607913,3.18532942786423));
#18648=CARTESIAN_POINT('Ctrl Pts',(32.7783096769706,37.9668638777563,3.23766280364831));
#18649=CARTESIAN_POINT('Ctrl Pts',(32.1165957326192,37.0243399779266,3.2899961794324));
#18650=CARTESIAN_POINT('Ctrl Pts',(31.7059940575521,36.4394922573,3.3224696854576));
#18651=CARTESIAN_POINT('Ctrl Pts',(31.4904702191063,35.7176870288261,3.35494319148281));
#18652=CARTESIAN_POINT('Ctrl Pts',(31.4866348863052,34.9979909502101,3.38741669750802));
#18653=CARTESIAN_POINT('Origin',(35.,35.,4.));
#18654=CARTESIAN_POINT('',(31.4769533103746,34.9997936499005,4.38741669750802));
#18655=CARTESIAN_POINT('',(31.4811433043907,35.0029051520383,4.11258330249198));
#18656=CARTESIAN_POINT('',(31.4825,35.,4.));
#18657=CARTESIAN_POINT('Ctrl Pts',(31.4811433043907,35.0029051520383,4.11258330249198));
#18658=CARTESIAN_POINT('Ctrl Pts',(31.4791554024968,35.227917919132,4.10238997204752));
#18659=CARTESIAN_POINT('Ctrl Pts',(31.4989360215654,35.4525827818457,4.09219664160306));
#18660=CARTESIAN_POINT('Ctrl Pts',(31.5417697834626,35.6727628942377,4.08200331115859));
#18661=CARTESIAN_POINT('Ctrl Pts',(31.761681751374,36.8031852448886,4.02966993537451));
#18662=CARTESIAN_POINT('Ctrl Pts',(32.5892464227109,37.815395051703,3.97733655959042));
#18663=CARTESIAN_POINT('Ctrl Pts',(33.6534212074435,38.2555631921955,3.92500318380634));
#18664=CARTESIAN_POINT('Ctrl Pts',(34.7175959921761,38.6957313326879,3.87266980802225));
#18665=CARTESIAN_POINT('Ctrl Pts',(36.0183808903044,38.5638578068583,3.82033643223817));
#18666=CARTESIAN_POINT('Ctrl Pts',(36.9725627531969,37.9190687430238,3.76800305645409));
#18667=CARTESIAN_POINT('Ctrl Pts',(37.9267446160893,37.2742796791893,3.71566968067));
#18668=CARTESIAN_POINT('Ctrl Pts',(38.5343234437459,36.1165750773498,3.66333630488592));
#18669=CARTESIAN_POINT('Ctrl Pts',(38.5228883542836,34.965017348136,3.61100292910183));
#18670=CARTESIAN_POINT('Ctrl Pts',(38.5114532648213,33.8134596189221,3.55866955331775));
#18671=CARTESIAN_POINT('Ctrl Pts',(37.8810042582401,32.6680487623339,3.50633617753366));
#18672=CARTESIAN_POINT('Ctrl Pts',(36.9142061709404,32.0423352319303,3.45400280174958));
#18673=CARTESIAN_POINT('Ctrl Pts',(35.9474080836407,31.4166217015266,3.40166942596549));
#18674=CARTESIAN_POINT('Ctrl Pts',(34.6442609156224,31.3106054973076,3.34933605018141));
#18675=CARTESIAN_POINT('Ctrl Pts',(33.5890369502264,31.7718194895137,3.29700267439732));
#18676=CARTESIAN_POINT('Ctrl Pts',(32.5338129848304,32.2330334817198,3.24466929861324));
#18677=CARTESIAN_POINT('Ctrl Pts',(31.7265122220568,33.2614776703508,3.19233592282916));
#18678=CARTESIAN_POINT('Ctrl Pts',(31.5290918320576,34.3960441771713,3.14000254704507));
#18679=CARTESIAN_POINT('Ctrl Pts',(31.4946134017248,34.5941902362662,3.13086279886071));
#18680=CARTESIAN_POINT('Ctrl Pts',(31.4787367991106,34.7955731089531,3.12172305067635));
#18681=CARTESIAN_POINT('Ctrl Pts',(31.48047694743,34.9972296622465,3.11258330249198));
#18682=CARTESIAN_POINT('Ctrl Pts',(31.4866348863052,34.9979909502101,3.38741669750802));
#18683=CARTESIAN_POINT('Ctrl Pts',(31.4842893061927,34.5578453627213,3.4072765672669));
#18684=CARTESIAN_POINT('Ctrl Pts',(31.5611193891505,34.1184886387468,3.42713643702577));
#18685=CARTESIAN_POINT('Ctrl Pts',(31.7209246555095,33.7117308512332,3.44699630678465));
#18686=CARTESIAN_POINT('Ctrl Pts',(32.1420326062756,32.6398704409937,3.49932968256873));
#18687=CARTESIAN_POINT('Ctrl Pts',(33.1393135913321,31.7943744371391,3.55166305835282));
#18688=CARTESIAN_POINT('Ctrl Pts',(34.2656318975588,31.5543250290031,3.6039964341369));
#18689=CARTESIAN_POINT('Ctrl Pts',(35.3919502037855,31.3142756208671,3.65632980992098));
#18690=CARTESIAN_POINT('Ctrl Pts',(36.6473058311824,31.6796728084497,3.70866318570507));
#18691=CARTESIAN_POINT('Ctrl Pts',(37.4688540624077,32.4866890097577,3.76099656148916));
#18692=CARTESIAN_POINT('Ctrl Pts',(38.2904022936331,33.2937052110658,3.81332993727324));
#18693=CARTESIAN_POINT('Ctrl Pts',(38.6781431286869,34.5423404260991,3.86566331305732));
#18694=CARTESIAN_POINT('Ctrl Pts',(38.4582311043207,35.6727630669474,3.91799668884141));
#18695=CARTESIAN_POINT('Ctrl Pts',(38.2383190799545,36.8031857077956,3.97033006462549));
#18696=CARTESIAN_POINT('Ctrl Pts',(37.4107541961682,37.8153957744587,4.02266344040958));
#18697=CARTESIAN_POINT('Ctrl Pts',(36.3465791382448,38.2555640279499,4.07499681619366));
#18698=CARTESIAN_POINT('Ctrl Pts',(35.2824040803214,38.6957322814412,4.12733019197775));
#18699=CARTESIAN_POINT('Ctrl Pts',(33.9816188482609,38.5638587217606,4.17966356776183));
#18700=CARTESIAN_POINT('Ctrl Pts',(33.0274367404146,37.9190694923971,4.23199694354592));
#18701=CARTESIAN_POINT('Ctrl Pts',(32.0828594910996,37.2807707529301,4.28380352819995));
#18702=CARTESIAN_POINT('Ctrl Pts',(31.4779426270586,36.1398304565742,4.33561011285398));
#18703=CARTESIAN_POINT('Ctrl Pts',(31.4769533103746,34.9997936499005,4.38741669750802));
#18704=CARTESIAN_POINT('Origin',(35.,35.,4.));
#18705=CARTESIAN_POINT('',(31.4861926565527,35.0022702467704,5.38741669750802));
#18706=CARTESIAN_POINT('',(31.4875431178521,34.9988611670469,5.11258330249198));
#18707=CARTESIAN_POINT('',(31.4825,35.,4.));
#18708=CARTESIAN_POINT('Ctrl Pts',(31.4875431178521,34.9988611670469,5.11258330249198));
#18709=CARTESIAN_POINT('Ctrl Pts',(31.4894883427227,35.6536666001145,5.08305689341869));
#18710=CARTESIAN_POINT('Ctrl Pts',(31.6654106307538,36.3094429302072,5.0535304843454));
#18711=CARTESIAN_POINT('Ctrl Pts',(32.0086471712983,36.8611218096429,5.02400407527211));
#18712=CARTESIAN_POINT('Ctrl Pts',(32.6170085475347,37.8389318114614,4.97167069948803));
#18713=CARTESIAN_POINT('Ctrl Pts',(33.7509866448637,38.4897202961854,4.91933732370394));
#18714=CARTESIAN_POINT('Ctrl Pts',(34.9021569461515,38.5217031223488,4.86700394791986));
#18715=CARTESIAN_POINT('Ctrl Pts',(36.0533272474394,38.5536859485121,4.81467057213577));
#18716=CARTESIAN_POINT('Ctrl Pts',(37.2216897526861,37.9668631161147,4.76233719635169));
#18717=CARTESIAN_POINT('Ctrl Pts',(37.8834035271664,37.0243394582438,4.71000382056761));
#18718=CARTESIAN_POINT('Ctrl Pts',(38.5451173016466,36.0818158003729,4.65767044478352));
#18719=CARTESIAN_POINT('Ctrl Pts',(38.7001823453603,34.7835913170285,4.60533706899944));
#18720=CARTESIAN_POINT('Ctrl Pts',(38.2790745026986,33.7117311819539,4.55300369321535));
#18721=CARTESIAN_POINT('Ctrl Pts',(37.857966660037,32.6398710468792,4.50067031743127));
#18722=CARTESIAN_POINT('Ctrl Pts',(36.860685931,31.7943752600742,4.44833694164718));
#18723=CARTESIAN_POINT('Ctrl Pts',(35.7343679139176,31.5543259135622,4.3960035658631));
#18724=CARTESIAN_POINT('Ctrl Pts',(34.6080498968352,31.3142765670502,4.34367019007902));
#18725=CARTESIAN_POINT('Ctrl Pts',(33.3526945917074,31.6796736608312,4.29133681429493));
#18726=CARTESIAN_POINT('Ctrl Pts',(32.5311465713864,32.4866896549654,4.23900343851085));
#18727=CARTESIAN_POINT('Ctrl Pts',(31.8696170922289,33.1365176103207,4.19686339317123));
#18728=CARTESIAN_POINT('Ctrl Pts',(31.4893614502066,34.0726843317691,4.15472334783161));
#18729=CARTESIAN_POINT('Ctrl Pts',(31.4811433043907,35.0029051520383,4.11258330249198));
#18730=CARTESIAN_POINT('Ctrl Pts',(31.4769533103746,34.9997936499005,4.38741669750802));
#18731=CARTESIAN_POINT('Ctrl Pts',(31.4769432505867,34.9882012764272,4.38794348863807));
#18732=CARTESIAN_POINT('Ctrl Pts',(31.476995634958,34.9766089963718,4.38847027976812));
#18733=CARTESIAN_POINT('Ctrl Pts',(31.4771107413343,34.9650173391525,4.38899707089817));
#18734=CARTESIAN_POINT('Ctrl Pts',(31.4885458337323,33.8134593143178,4.44133044668225));
#18735=CARTESIAN_POINT('Ctrl Pts',(32.1189950021604,32.6680481636951,4.49366382246634));
#18736=CARTESIAN_POINT('Ctrl Pts',(33.0857933376524,32.0423344726558,4.54599719825042));
#18737=CARTESIAN_POINT('Ctrl Pts',(34.0525916731444,31.4166207816165,4.59833057403451));
#18738=CARTESIAN_POINT('Ctrl Pts',(35.3557391757004,31.3106045501606,4.65066394981859));
#18739=CARTESIAN_POINT('Ctrl Pts',(36.4109634119899,31.7718186607773,4.70299732560267));
#18740=CARTESIAN_POINT('Ctrl Pts',(37.4661876482795,32.233032771394,4.75533070138676));
#18741=CARTESIAN_POINT('Ctrl Pts',(38.2734886183026,33.2614772240832,4.80766407717084));
#18742=CARTESIAN_POINT('Ctrl Pts',(38.4709090589814,34.3960440221467,4.85999745295493));
#18743=CARTESIAN_POINT('Ctrl Pts',(38.6683294996601,35.5306108202102,4.91233082873901));
#18744=CARTESIAN_POINT('Ctrl Pts',(38.2558694109946,36.771299963648,4.9646642045231));
#18745=CARTESIAN_POINT('Ctrl Pts',(37.4184572536729,37.5618425098028,5.01699758030718));
#18746=CARTESIAN_POINT('Ctrl Pts',(36.5810450963513,38.3523850559575,5.06933095609127));
#18747=CARTESIAN_POINT('Ctrl Pts',(35.3186808703736,38.6927810048293,5.12166433187535));
#18748=CARTESIAN_POINT('Ctrl Pts',(34.1973516288142,38.4304122279041,5.17399770765944));
#18749=CARTESIAN_POINT('Ctrl Pts',(33.0760223872548,38.168043450979,5.22633108344352));
#18750=CARTESIAN_POINT('Ctrl Pts',(32.0957281301138,37.302909948257,5.2786644592276));
#18751=CARTESIAN_POINT('Ctrl Pts',(31.6959884957425,36.2228984191863,5.33099783501169));
#18752=CARTESIAN_POINT('Ctrl Pts',(31.5523398513352,35.834790313921,5.34980412251047));
#18753=CARTESIAN_POINT('Ctrl Pts',(31.4836619352111,35.4189336360054,5.36861041000924));
#18754=CARTESIAN_POINT('Ctrl Pts',(31.4861926565527,35.0022702467704,5.38741669750802));
#18755=CARTESIAN_POINT('Origin',(35.,35.,4.));
#18756=CARTESIAN_POINT('',(31.4836963557363,34.997016753135,6.38741669750802));
#18757=CARTESIAN_POINT('',(31.4775764275568,34.998690818207,6.11258330249198));
#18758=CARTESIAN_POINT('',(31.4825,35.,4.));
#18759=CARTESIAN_POINT('Ctrl Pts',(31.4775764275568,34.998690818207,6.11258330249198));
#18760=CARTESIAN_POINT('Ctrl Pts',(31.4827872982739,36.074383472183,6.06372381478987));
#18761=CARTESIAN_POINT('Ctrl Pts',(32.0123599558151,37.1545218488605,6.01486432708775));
#18762=CARTESIAN_POINT('Ctrl Pts',(32.8684049695572,37.8050433721304,5.96600483938563));
#18763=CARTESIAN_POINT('Ctrl Pts',(33.7853144071958,38.5018166895356,5.91367146360154));
#18764=CARTESIAN_POINT('Ctrl Pts',(35.0767706487491,38.7057102384231,5.86133808781746));
#18765=CARTESIAN_POINT('Ctrl Pts',(36.1637432436869,38.3253071915374,5.80900471203338));
#18766=CARTESIAN_POINT('Ctrl Pts',(37.2507158386246,37.9449041446517,5.75667133624929));
#18767=CARTESIAN_POINT('Ctrl Pts',(38.1332047869467,36.9802045019929,5.70433796046521));
#18768=CARTESIAN_POINT('Ctrl Pts',(38.4155418609846,35.8637360634774,5.65200458468113));
#18769=CARTESIAN_POINT('Ctrl Pts',(38.6978789350226,34.7472676249618,5.59967120889704));
#18770=CARTESIAN_POINT('Ctrl Pts',(38.3800641347763,33.4790303905896,5.54733783311296));
#18771=CARTESIAN_POINT('Ctrl Pts',(37.604591287456,32.6276445643168,5.49500445732887));
#18772=CARTESIAN_POINT('Ctrl Pts',(36.8291184401356,31.7762587380439,5.44267108154479));
#18773=CARTESIAN_POINT('Ctrl Pts',(35.595987545741,31.3417243198703,5.3903377057607));
#18774=CARTESIAN_POINT('Ctrl Pts',(34.4580787374483,31.5188669221671,5.33800432997662));
#18775=CARTESIAN_POINT('Ctrl Pts',(33.3201699291557,31.6960095244639,5.28567095419254));
#18776=CARTESIAN_POINT('Ctrl Pts',(32.277483206965,32.4848291472311,5.23333757840845));
#18777=CARTESIAN_POINT('Ctrl Pts',(31.7975121734416,33.5316547180712,5.18100420262437));
#18778=CARTESIAN_POINT('Ctrl Pts',(31.5883400491575,33.9878629329714,5.15819723591357));
#18779=CARTESIAN_POINT('Ctrl Pts',(31.4860405755429,34.4930724110572,5.13539026920278));
#18780=CARTESIAN_POINT('Ctrl Pts',(31.4875431178521,34.9988611670469,5.11258330249198));
#18781=CARTESIAN_POINT('Ctrl Pts',(31.4861926565527,35.0022702467704,5.38741669750802));
#18782=CARTESIAN_POINT('Ctrl Pts',(31.4907043241454,34.2594596183014,5.42094378579333));
#18783=CARTESIAN_POINT('Ctrl Pts',(31.7215335296905,33.5140850744687,5.45447087407864));
#18784=CARTESIAN_POINT('Ctrl Pts',(32.1573641816635,32.9187998099572,5.48799796236395));
#18785=CARTESIAN_POINT('Ctrl Pts',(32.8376645135573,31.9896022852182,5.54033133814803));
#18786=CARTESIAN_POINT('Ctrl Pts',(34.0174501889464,31.4260967911598,5.59266471393211));
#18787=CARTESIAN_POINT('Ctrl Pts',(35.1677586650642,31.4809334902507,5.64499808971619));
#18788=CARTESIAN_POINT('Ctrl Pts',(36.318067141182,31.5357701893416,5.69733146550028));
#18789=CARTESIAN_POINT('Ctrl Pts',(37.4388984180285,32.2089490815819,5.74966484128437));
#18790=CARTESIAN_POINT('Ctrl Pts',(38.027722367947,33.1986476425792,5.80199821706845));
#18791=CARTESIAN_POINT('Ctrl Pts',(38.6165463178655,34.1883462035765,5.85433159285254));
#18792=CARTESIAN_POINT('Ctrl Pts',(38.6733629408561,35.4945644333309,5.90666496863662));
#18793=CARTESIAN_POINT('Ctrl Pts',(38.1726983287836,36.5316521939121,5.9589983444207));
#18794=CARTESIAN_POINT('Ctrl Pts',(37.6720337167111,37.5687399544933,6.01133172020479));
#18795=CARTESIAN_POINT('Ctrl Pts',(36.6138878695757,38.3366972459014,6.06366509598887));
#18796=CARTESIAN_POINT('Ctrl Pts',(35.4726853575398,38.491208604665,6.11599847177296));
#18797=CARTESIAN_POINT('Ctrl Pts',(34.3314828455038,38.6457199634287,6.16833184755704));
#18798=CARTESIAN_POINT('Ctrl Pts',(33.1072236685675,38.1867853895479,6.22066522334113));
#18799=CARTESIAN_POINT('Ctrl Pts',(32.3488106963438,37.3201666288988,6.27299859912521));
#18800=CARTESIAN_POINT('Ctrl Pts',(31.7960966856348,36.6885947168973,6.31113796525281));
#18801=CARTESIAN_POINT('Ctrl Pts',(31.490801080199,35.8404951819918,6.34927733138042));
#18802=CARTESIAN_POINT('Ctrl Pts',(31.4836963557363,34.997016753135,6.38741669750802));
#18803=CARTESIAN_POINT('Origin',(35.,35.,4.));
#18804=CARTESIAN_POINT('',(31.47826034488,35.0017653187145,7.38741669750802));
#18805=CARTESIAN_POINT('',(31.4846882532079,35.0028111988253,7.11258330249198));
#18806=CARTESIAN_POINT('',(31.4825,35.,4.));
#18807=CARTESIAN_POINT('',(37.6735319337713,37.2858331630075,8.));
#18808=CARTESIAN_POINT('Ctrl Pts',(31.47826034488,35.0017653187145,7.38741669750802));
#18809=CARTESIAN_POINT('Ctrl Pts',(31.4849539836961,33.9623976729958,7.43461100431976));
#18810=CARTESIAN_POINT('Ctrl Pts',(31.9746240526108,32.9177662403339,7.4818053111315));
#18811=CARTESIAN_POINT('Ctrl Pts',(32.7813938443113,32.2635129435208,7.52899961794324));
#18812=CARTESIAN_POINT('Ctrl Pts',(33.6760141816485,31.5380168836533,7.58133299372733));
#18813=CARTESIAN_POINT('Ctrl Pts',(34.9605532865631,31.292545720314,7.63366636951141));
#18814=CARTESIAN_POINT('Ctrl Pts',(36.0588773921206,31.639261394405,7.68599974529549));
#18815=CARTESIAN_POINT('Ctrl Pts',(37.1572014976782,31.985977068496,7.73833312107957));
#18816=CARTESIAN_POINT('Ctrl Pts',(38.0693106038786,32.9248795800174,7.79066649686366));
#18817=CARTESIAN_POINT('Ctrl Pts',(38.3863002982481,34.0300657119841,7.84299987264775));
#18818=CARTESIAN_POINT('Ctrl Pts',(38.7032899926177,35.1352518439507,7.89533324843183));
#18819=CARTESIAN_POINT('Ctrl Pts',(38.4251602751564,36.4067215963626,7.94766662421592));
#18820=CARTESIAN_POINT('Ctrl Pts',(37.6735319337713,37.2858331630076,8.));
#18821=CARTESIAN_POINT('',(32.321499452735,37.2890251664065,7.99999999999999));
#18822=CARTESIAN_POINT('Origin',(35.,35.,8.));
#18823=CARTESIAN_POINT('Ctrl Pts',(32.321476328717,37.2890400220486,8.));
#18824=CARTESIAN_POINT('Ctrl Pts',(33.0392492598742,38.1233257780545,7.95000212253755));
#18825=CARTESIAN_POINT('Ctrl Pts',(34.1813302937714,38.5989193684354,7.90000424507511));
#18826=CARTESIAN_POINT('Ctrl Pts',(35.278297796919,38.5118532074872,7.85000636761267));
#18827=CARTESIAN_POINT('Ctrl Pts',(36.4265067905564,38.4207200164352,7.79767299182859));
#18828=CARTESIAN_POINT('Ctrl Pts',(37.5252891335093,37.7131334793234,7.74533961604451));
#18829=CARTESIAN_POINT('Ctrl Pts',(38.0826702008662,36.7055536192858,7.69300624026042));
#18830=CARTESIAN_POINT('Ctrl Pts',(38.6400512682231,35.6979737592483,7.64067286447634));
#18831=CARTESIAN_POINT('Ctrl Pts',(38.6560310599838,34.390400576285,7.58833948869225));
#18832=CARTESIAN_POINT('Ctrl Pts',(38.1231127521292,33.3694814726124,7.53600611290816));
#18833=CARTESIAN_POINT('Ctrl Pts',(37.5901944442746,32.3485623689397,7.48367273712408));
#18834=CARTESIAN_POINT('Ctrl Pts',(36.5083780368047,31.6142973445577,7.43133936134));
#18835=CARTESIAN_POINT('Ctrl Pts',(35.3628660305036,31.4957037502949,7.37900598555592));
#18836=CARTESIAN_POINT('Ctrl Pts',(34.2173540242026,31.3771101560321,7.32667260977183));
#18837=CARTESIAN_POINT('Ctrl Pts',(33.0081464190704,31.8741879918886,7.27433923398774));
#18838=CARTESIAN_POINT('Ctrl Pts',(32.2773153573829,32.7641662925145,7.22200585820366));
#18839=CARTESIAN_POINT('Ctrl Pts',(31.7679565185591,33.3844441344804,7.18553167296643));
#18840=CARTESIAN_POINT('Ctrl Pts',(31.4909695616634,34.1955737681155,7.14905748772921));
#18841=CARTESIAN_POINT('Ctrl Pts',(31.4846882532079,35.0028111988253,7.11258330249198));
#18842=CARTESIAN_POINT('Origin',(-35.,35.,4.));
#18843=CARTESIAN_POINT('',(-38.5120268522747,34.9998626667344,0.387416697508021));
#18844=CARTESIAN_POINT('',(-38.5151985683976,34.9953484440209,0.112583302491983));
#18845=CARTESIAN_POINT('',(-38.5175,35.,4.));
#18846=CARTESIAN_POINT('',(-37.6735319337713,37.2858331630075,0.));
#18847=CARTESIAN_POINT('Ctrl Pts',(-38.5151985683976,34.9953484440209,0.112583302491983));
#18848=CARTESIAN_POINT('Ctrl Pts',(-38.508022599206,35.8232716101844,0.0750555349946553));
#18849=CARTESIAN_POINT('Ctrl Pts',(-38.2125174896864,36.6554305951821,0.0375277674973274));
#18850=CARTESIAN_POINT('Ctrl Pts',(-37.6735319337713,37.2858331630075,0.));
#18851=CARTESIAN_POINT('',(-32.3214993158099,37.289025066123,6.74947782880687E-15));
#18852=CARTESIAN_POINT('Origin',(-35.,35.,0.));
#18853=CARTESIAN_POINT('Ctrl Pts',(-32.3214761820288,37.2890399271607,4.52762827229947E-15));
#18854=CARTESIAN_POINT('Ctrl Pts',(-33.0392490750158,38.123325504421,0.0499978774624455));
#18855=CARTESIAN_POINT('Ctrl Pts',(-34.1813302139117,38.5989195898449,0.0999957549248864));
#18856=CARTESIAN_POINT('Ctrl Pts',(-35.2782977979761,38.5118535311589,0.149993632387327));
#18857=CARTESIAN_POINT('Ctrl Pts',(-36.42650687631,38.420720447146,0.202327008171411));
#18858=CARTESIAN_POINT('Ctrl Pts',(-37.5252892775753,37.7131335867401,0.254660383955495));
#18859=CARTESIAN_POINT('Ctrl Pts',(-38.0826703648835,36.7055536147166,0.30699375973958));
#18860=CARTESIAN_POINT('Ctrl Pts',(-38.368187486773,36.189423196523,0.333801405662393));
#18861=CARTESIAN_POINT('Ctrl Pts',(-38.511642203595,35.5945753060192,0.360609051585207));
#18862=CARTESIAN_POINT('Ctrl Pts',(-38.5120268522747,34.9998626667344,0.387416697508021));
#18863=CARTESIAN_POINT('Origin',(-35.,35.,4.));
#18864=CARTESIAN_POINT('',(-38.5212301417031,34.9978480330234,1.38741669750802));
#18865=CARTESIAN_POINT('',(-38.5220165881118,35.0016823567161,1.11258330249198));
#18866=CARTESIAN_POINT('',(-38.5175,35.,4.));
#18867=CARTESIAN_POINT('Ctrl Pts',(-38.5220165881118,35.0016823567161,1.11258330249198));
#18868=CARTESIAN_POINT('Ctrl Pts',(-38.5226066014871,35.1013890040059,1.10805583214991));
#18869=CARTESIAN_POINT('Ctrl Pts',(-38.5187309301454,35.2010488154761,1.10352836180785));
#18870=CARTESIAN_POINT('Ctrl Pts',(-38.5102390188272,35.3003133215195,1.09900089146578));
#18871=CARTESIAN_POINT('Ctrl Pts',(-38.4120803667407,36.4477193350987,1.04666751568169));
#18872=CARTESIAN_POINT('Ctrl Pts',(-37.6971355129363,37.5423077018709,0.994334139897609));
#18873=CARTESIAN_POINT('Ctrl Pts',(-36.6859404016511,38.0934400513324,0.942000764113524));
#18874=CARTESIAN_POINT('Ctrl Pts',(-35.6747452903659,38.6445724007939,0.88966738832944));
#18875=CARTESIAN_POINT('Ctrl Pts',(-34.3672999215998,38.6522487329447,0.837334012545356));
#18876=CARTESIAN_POINT('Ctrl Pts',(-33.3498298999919,38.1127743676805,0.785000636761271));
#18877=CARTESIAN_POINT('Ctrl Pts',(-32.332359878384,37.5733000024162,0.732667260977186));
#18878=CARTESIAN_POINT('Ctrl Pts',(-31.6048652039344,36.4866749397369,0.680333885193101));
#18879=CARTESIAN_POINT('Ctrl Pts',(-31.4934688910568,35.3406024624848,0.628000509409016));
#18880=CARTESIAN_POINT('Ctrl Pts',(-31.3820725781792,34.1945299852327,0.575667133624932));
#18881=CARTESIAN_POINT('Ctrl Pts',(-31.8867746268736,32.9890100934079,0.523333757840848));
#18882=CARTESIAN_POINT('Ctrl Pts',(-32.7813945002955,32.26351389125,0.471000382056763));
#18883=CARTESIAN_POINT('Ctrl Pts',(-33.6760143737173,31.5380176890922,0.418667006272678));
#18884=CARTESIAN_POINT('Ctrl Pts',(-34.9605520718666,31.2925451766014,0.366333630488594));
#18885=CARTESIAN_POINT('Ctrl Pts',(-36.0588768524004,31.6392614911932,0.31400025470451));
#18886=CARTESIAN_POINT('Ctrl Pts',(-37.1572016329341,31.9859778057849,0.261666878920425));
#18887=CARTESIAN_POINT('Ctrl Pts',(-38.0693134958523,32.9248829474593,0.209333503136341));
#18888=CARTESIAN_POINT('Ctrl Pts',(-38.3863031564079,34.0300688951037,0.157000127352256));
#18889=CARTESIAN_POINT('Ctrl Pts',(-38.4759825373922,34.3427364801714,0.142194519065498));
#18890=CARTESIAN_POINT('Ctrl Pts',(-38.5180296611061,34.6687128110693,0.127388910778741));
#18891=CARTESIAN_POINT('Ctrl Pts',(-38.5151985683976,34.9953484440209,0.112583302491983));
#18892=CARTESIAN_POINT('Ctrl Pts',(-38.5120268522747,34.9998626667344,0.387416697508021));
#18893=CARTESIAN_POINT('Ctrl Pts',(-38.5123931074215,34.4335886186821,0.412942427369291));
#18894=CARTESIAN_POINT('Ctrl Pts',(-38.3830450900788,33.8674371959539,0.438468157230563));
#18895=CARTESIAN_POINT('Ctrl Pts',(-38.1231128912653,33.3694814421284,0.463993887091834));
#18896=CARTESIAN_POINT('Ctrl Pts',(-37.5901945569878,32.348562325205,0.516327262875918));
#18897=CARTESIAN_POINT('Ctrl Pts',(-36.5083781150815,31.6142971749993,0.568660638660002));
#18898=CARTESIAN_POINT('Ctrl Pts',(-35.3628660558844,31.4957035546786,0.620994014444087));
#18899=CARTESIAN_POINT('Ctrl Pts',(-34.2173539966873,31.3771099343579,0.673327390228171));
#18900=CARTESIAN_POINT('Ctrl Pts',(-33.0081463201995,31.8741878439222,0.725660766012255));
#18901=CARTESIAN_POINT('Ctrl Pts',(-32.2773152209783,32.7641661988384,0.77799414179634));
#18902=CARTESIAN_POINT('Ctrl Pts',(-31.5464841217571,33.6541445537545,0.830327517580424));
#18903=CARTESIAN_POINT('Ctrl Pts',(-31.2940295998026,34.9370233540225,0.882660893364509));
#18904=CARTESIAN_POINT('Ctrl Pts',(-31.6331814964185,36.0375699846378,0.934994269148593));
#18905=CARTESIAN_POINT('Ctrl Pts',(-31.9723333930344,37.1381166152532,0.987327644932678));
#18906=CARTESIAN_POINT('Ctrl Pts',(-32.9030917082208,38.0563310762161,1.03966102071676));
#18907=CARTESIAN_POINT('Ctrl Pts',(-34.0081263071124,38.3805512169411,1.09199439650085));
#18908=CARTESIAN_POINT('Ctrl Pts',(-35.1131609060039,38.7047713576661,1.14432777228493));
#18909=CARTESIAN_POINT('Ctrl Pts',(-36.3924717886008,38.4349971781534,1.19666114806902));
#18910=CARTESIAN_POINT('Ctrl Pts',(-37.2724838028734,37.6921714555696,1.2489945238531));
#18911=CARTESIAN_POINT('Ctrl Pts',(-38.0483632745171,37.0372449093246,1.29513524840474));
#18912=CARTESIAN_POINT('Ctrl Pts',(-38.5138515465497,36.0145962191428,1.34127597295638));
#18913=CARTESIAN_POINT('Ctrl Pts',(-38.5212301417031,34.9978480330234,1.38741669750802));
#18914=CARTESIAN_POINT('Origin',(-35.,35.,4.));
#18915=CARTESIAN_POINT('',(-38.516961906974,35.0030273033746,2.38741669750802));
#18916=CARTESIAN_POINT('',(-38.512261546942,35.0007919713519,2.11258330249198));
#18917=CARTESIAN_POINT('',(-38.5175,35.,4.));
#18918=CARTESIAN_POINT('Ctrl Pts',(-38.512261546942,35.0007919713519,2.11258330249198));
#18919=CARTESIAN_POINT('Ctrl Pts',(-38.513350743052,35.5300199732952,2.08872275352109));
#18920=CARTESIAN_POINT('Ctrl Pts',(-38.400967605409,36.0588087668393,2.06486220455019));
#18921=CARTESIAN_POINT('Ctrl Pts',(-38.1726977821637,36.5316519312173,2.0410016555793));
#18922=CARTESIAN_POINT('Ctrl Pts',(-37.6720332561867,37.568739511998,1.98866827979521));
#18923=CARTESIAN_POINT('Ctrl Pts',(-36.6138875906958,38.3366966664809,1.93633490401113));
#18924=CARTESIAN_POINT('Ctrl Pts',(-35.472685275733,38.4912080005995,1.88400152822705));
#18925=CARTESIAN_POINT('Ctrl Pts',(-34.3314829607702,38.6457193347182,1.83166815244296));
#18926=CARTESIAN_POINT('Ctrl Pts',(-33.1072239963354,38.1867848484726,1.77933477665888));
#18927=CARTESIAN_POINT('Ctrl Pts',(-32.3488111539779,37.3201662335233,1.72700140087479));
#18928=CARTESIAN_POINT('Ctrl Pts',(-31.5903983116205,36.453547618574,1.67466802509071));
#18929=CARTESIAN_POINT('Ctrl Pts',(-31.2978315913404,35.179244874921,1.62233464930662));
#18930=CARTESIAN_POINT('Ctrl Pts',(-31.6022838952552,34.0686053777681,1.57000127352254));
#18931=CARTESIAN_POINT('Ctrl Pts',(-31.90673619917,32.9579658806151,1.51766789773845));
#18932=CARTESIAN_POINT('Ctrl Pts',(-32.8082075272796,32.0109896299622,1.46533452195437));
#18933=CARTESIAN_POINT('Ctrl Pts',(-33.9025204773781,31.6522426059455,1.41300114617028));
#18934=CARTESIAN_POINT('Ctrl Pts',(-34.9968334274766,31.2934955819288,1.3606677703862));
#18935=CARTESIAN_POINT('Ctrl Pts',(-36.283987999564,31.5229777845482,1.30833439460212));
#18936=CARTESIAN_POINT('Ctrl Pts',(-37.1868790604233,32.2378307160511,1.25600101881803));
#18937=CARTESIAN_POINT('Ctrl Pts',(-38.0116591177612,32.8908402178529,1.20819511337602));
#18938=CARTESIAN_POINT('Ctrl Pts',(-38.5157865917788,33.94887224596,1.160389207934));
#18939=CARTESIAN_POINT('Ctrl Pts',(-38.5220165881118,35.0016823567161,1.11258330249198));
#18940=CARTESIAN_POINT('Ctrl Pts',(-38.5212301417031,34.9978480330234,1.38741669750802));
#18941=CARTESIAN_POINT('Ctrl Pts',(-38.5222204396842,34.8613879542309,1.39360934874046));
#18942=CARTESIAN_POINT('Ctrl Pts',(-38.5149588389545,34.7250341608202,1.39980199997291));
#18943=CARTESIAN_POINT('Ctrl Pts',(-38.499088221748,34.5896899066556,1.40599465120535));
#18944=CARTESIAN_POINT('Ctrl Pts',(-38.3649674804015,33.4459113459803,1.45832802698944));
#18945=CARTESIAN_POINT('Ctrl Pts',(-37.6160128517601,32.3742314902846,1.51066140277352));
#18946=CARTESIAN_POINT('Ctrl Pts',(-36.5880242056904,31.8551402422105,1.56299477855761));
#18947=CARTESIAN_POINT('Ctrl Pts',(-35.5600355596207,31.3360489941365,1.61532815434169));
#18948=CARTESIAN_POINT('Ctrl Pts',(-34.2530128961227,31.3695463536841,1.66766153012578));
#18949=CARTESIAN_POINT('Ctrl Pts',(-33.2529648698024,31.9406150594439,1.71999490590986));
#18950=CARTESIAN_POINT('Ctrl Pts',(-32.2529168434821,32.5116837652037,1.77232828169395));
#18951=CARTESIAN_POINT('Ctrl Pts',(-31.5598434543395,33.6203238171756,1.82466165747803));
#18952=CARTESIAN_POINT('Ctrl Pts',(-31.4844880896413,34.7694704150121,1.87699503326211));
#18953=CARTESIAN_POINT('Ctrl Pts',(-31.4091327249431,35.9186170128485,1.9293284090462));
#18954=CARTESIAN_POINT('Ctrl Pts',(-31.9514953846893,37.1082701565493,1.98166178483028));
#18955=CARTESIAN_POINT('Ctrl Pts',(-32.8684048665688,37.8050435076812,2.03399516061437));
#18956=CARTESIAN_POINT('Ctrl Pts',(-33.7853143484484,38.5018168588132,2.08632853639845));
#18957=CARTESIAN_POINT('Ctrl Pts',(-35.0767706524612,38.7057104173762,2.13866191218254));
#18958=CARTESIAN_POINT('Ctrl Pts',(-36.1637432999128,38.325307352079,2.19099528796662));
#18959=CARTESIAN_POINT('Ctrl Pts',(-37.2507159473644,37.9449042867818,2.24332866375071));
#18960=CARTESIAN_POINT('Ctrl Pts',(-38.1332049382548,36.9802045976245,2.29566203953479));
#18961=CARTESIAN_POINT('Ctrl Pts',(-38.4155420259161,35.8637361052132,2.34799541531887));
#18962=CARTESIAN_POINT('Ctrl Pts',(-38.4864342614375,35.5834011765932,2.36113584271526));
#18963=CARTESIAN_POINT('Ctrl Pts',(-38.5194889764144,35.2934977450987,2.37427627011164));
#18964=CARTESIAN_POINT('Ctrl Pts',(-38.516961906974,35.0030273033746,2.38741669750802));
#18965=CARTESIAN_POINT('Origin',(-35.,35.,4.));
#18966=CARTESIAN_POINT('',(-38.5133643814276,34.9979909506281,3.38741669750802));
#18967=CARTESIAN_POINT('',(-38.5195233495341,34.9972296620149,3.11258330249199));
#18968=CARTESIAN_POINT('',(-38.5175,35.,4.));
#18969=CARTESIAN_POINT('Ctrl Pts',(-38.5195233495341,34.9972296620149,3.11258330249199));
#18970=CARTESIAN_POINT('Ctrl Pts',(-38.5112995644464,35.9502404698791,3.06938967489226));
#18971=CARTESIAN_POINT('Ctrl Pts',(-38.1096192565637,36.9093637226591,3.02619604729254));
#18972=CARTESIAN_POINT('Ctrl Pts',(-37.4184568368782,37.5618420683218,2.98300241969282));
#18973=CARTESIAN_POINT('Ctrl Pts',(-36.581044823874,38.3523844782111,2.93066904390873));
#18974=CARTESIAN_POINT('Ctrl Pts',(-35.3186808154442,38.6927803683205,2.87833566812465));
#18975=CARTESIAN_POINT('Ctrl Pts',(-34.1973517671389,38.4304116366569,2.82600229234057));
#18976=CARTESIAN_POINT('Ctrl Pts',(-33.0760227188335,38.1680429049932,2.77366891655648));
#18977=CARTESIAN_POINT('Ctrl Pts',(-32.0957286306525,37.3029095515566,2.7213355407724));
#18978=CARTESIAN_POINT('Ctrl Pts',(-31.6959890651629,36.2228982085294,2.66900216498831));
#18979=CARTESIAN_POINT('Ctrl Pts',(-31.2962494996734,35.1428868655023,2.61666878920423));
#18980=CARTESIAN_POINT('Ctrl Pts',(-31.4770644568753,33.8479975328846,2.56433541342014));
#18981=CARTESIAN_POINT('Ctrl Pts',(-32.1573646715461,32.9188001684451,2.51200203763606));
#18982=CARTESIAN_POINT('Ctrl Pts',(-32.837664886217,31.9896028040056,2.45966866185197));
#18983=CARTESIAN_POINT('Ctrl Pts',(-34.0174503583568,31.4260974077442,2.40733528606789));
#18984=CARTESIAN_POINT('Ctrl Pts',(-35.1677586361884,31.4809340970796,2.3550019102838));
#18985=CARTESIAN_POINT('Ctrl Pts',(-36.3180669140201,31.535770786415,2.30266853449972));
#18986=CARTESIAN_POINT('Ctrl Pts',(-37.4388979975435,32.2089495613471,2.25033515871564));
#18987=CARTESIAN_POINT('Ctrl Pts',(-38.0277218460737,33.1986479523525,2.19800178293155));
#18988=CARTESIAN_POINT('Ctrl Pts',(-38.3480810663893,33.737109506995,2.16952895611836));
#18989=CARTESIAN_POINT('Ctrl Pts',(-38.5109618076844,34.3692634485841,2.14105612930517));
#18990=CARTESIAN_POINT('Ctrl Pts',(-38.512261546942,35.0007919713519,2.11258330249198));
#18991=CARTESIAN_POINT('Ctrl Pts',(-38.516961906974,35.0030273033746,2.38741669750802));
#18992=CARTESIAN_POINT('Ctrl Pts',(-38.5094246101142,34.1366633193706,2.42660964589572));
#18993=CARTESIAN_POINT('Ctrl Pts',(-38.1853502176079,33.2652551878002,2.46580259428343));
#18994=CARTESIAN_POINT('Ctrl Pts',(-37.6045914132455,32.6276444497373,2.50499554267113));
#18995=CARTESIAN_POINT('Ctrl Pts',(-36.8291185284818,31.7762585823377,2.55732891845521));
#18996=CARTESIAN_POINT('Ctrl Pts',(-35.5959875745222,31.3417241432036,2.6096622942393));
#18997=CARTESIAN_POINT('Ctrl Pts',(-34.4580787112737,31.5188667540608,2.66199567002338));
#18998=CARTESIAN_POINT('Ctrl Pts',(-33.3201698480253,31.6960093649181,2.71432904580747));
#18999=CARTESIAN_POINT('Ctrl Pts',(-32.277483075488,32.4848290257668,2.76666242159155));
#19000=CARTESIAN_POINT('Ctrl Pts',(-31.7975120187873,33.5316546471577,2.81899579737563));
#19001=CARTESIAN_POINT('Ctrl Pts',(-31.3175409620866,34.5784802685486,2.87132917315972));
#19002=CARTESIAN_POINT('Ctrl Pts',(-31.4002856212225,35.8833118504819,2.9236625489438));
#19003=CARTESIAN_POINT('Ctrl Pts',(-32.0086470268372,36.8611218995229,2.97599592472789));
#19004=CARTESIAN_POINT('Ctrl Pts',(-32.617008432452,37.8389319485639,3.02832930051197));
#19005=CARTESIAN_POINT('Ctrl Pts',(-33.7509865845457,38.4897204647128,3.08066267629606));
#19006=CARTESIAN_POINT('Ctrl Pts',(-34.902156941427,38.5217032924198,3.13299605208014));
#19007=CARTESIAN_POINT('Ctrl Pts',(-36.0533272983083,38.5536861201269,3.18532942786423));
#19008=CARTESIAN_POINT('Ctrl Pts',(-37.2216898599771,37.9668632593921,3.23766280364831));
#19009=CARTESIAN_POINT('Ctrl Pts',(-37.8834036664129,37.0243395560048,3.2899961794324));
#19010=CARTESIAN_POINT('Ctrl Pts',(-38.2940052559017,36.439491957273,3.3224696854576));
#19011=CARTESIAN_POINT('Ctrl Pts',(-38.5095290494265,35.7176868792413,3.35494319148281));
#19012=CARTESIAN_POINT('Ctrl Pts',(-38.5133643814276,34.9979909506281,3.38741669750802));
#19013=CARTESIAN_POINT('Origin',(-35.,35.,4.));
#19014=CARTESIAN_POINT('',(-38.5230459553398,34.9997936499459,4.38741669750802));
#19015=CARTESIAN_POINT('',(-38.5188569925171,35.0029051522836,4.11258330249198));
#19016=CARTESIAN_POINT('',(-38.5175,35.,4.));
#19017=CARTESIAN_POINT('Ctrl Pts',(-38.5188569925171,35.0029051522836,4.11258330249198));
#19018=CARTESIAN_POINT('Ctrl Pts',(-38.5208448945788,35.2279179383631,4.10238997204752));
#19019=CARTESIAN_POINT('Ctrl Pts',(-38.5010642738412,35.4525828200332,4.09219664160306));
#19020=CARTESIAN_POINT('Ctrl Pts',(-38.4582305083298,35.6727629510031,4.08200331115859));
#19021=CARTESIAN_POINT('Ctrl Pts',(-38.2383185218631,36.8031853970347,4.02966993537451));
#19022=CARTESIAN_POINT('Ctrl Pts',(-37.4107537806994,37.8153952892549,3.97733655959042));
#19023=CARTESIAN_POINT('Ctrl Pts',(-36.3465789061757,38.2555634668873,3.92500318380634));
#19024=CARTESIAN_POINT('Ctrl Pts',(-35.282404031652,38.6957316445196,3.87266980802226));
#19025=CARTESIAN_POINT('Ctrl Pts',(-33.9816190237685,38.5638581075641,3.82033643223817));
#19026=CARTESIAN_POINT('Ctrl Pts',(-33.0274370803658,37.9190689893243,3.76800305645409));
#19027=CARTESIAN_POINT('Ctrl Pts',(-32.0732551369631,37.2742798710845,3.71566968067));
#19028=CARTESIAN_POINT('Ctrl Pts',(-31.4656762580412,36.1165751715604,3.66333630488592));
#19029=CARTESIAN_POINT('Ctrl Pts',(-31.4771113484684,34.9650173451833,3.61100292910183));
#19030=CARTESIAN_POINT('Ctrl Pts',(-31.4885464388956,33.8134595188062,3.55866955331775));
#19031=CARTESIAN_POINT('Ctrl Pts',(-32.1189954986718,32.6680485655762,3.50633617753366));
#19032=CARTESIAN_POINT('Ctrl Pts',(-33.0857936675462,32.0423349823756,3.45400280174958));
#19033=CARTESIAN_POINT('Ctrl Pts',(-34.0525918364206,31.4166213991749,3.40166942596549));
#19034=CARTESIAN_POINT('Ctrl Pts',(-35.3557391143932,31.3106051860038,3.34933605018141));
#19035=CARTESIAN_POINT('Ctrl Pts',(-36.4109631688252,31.7718192171285,3.29700267439732));
#19036=CARTESIAN_POINT('Ctrl Pts',(-37.4661872232571,32.2330332482532,3.24466929861324));
#19037=CARTESIAN_POINT('Ctrl Pts',(-38.2734880541485,33.2614775236738,3.19233592282916));
#19038=CARTESIAN_POINT('Ctrl Pts',(-38.4709084608049,34.3960441262186,3.14000254704507));
#19039=CARTESIAN_POINT('Ctrl Pts',(-38.5053868940467,34.5941902020313,3.13086279886071));
#19040=CARTESIAN_POINT('Ctrl Pts',(-38.5212634980004,34.7955730917084,3.12172305067635));
#19041=CARTESIAN_POINT('Ctrl Pts',(-38.5195233495341,34.9972296620149,3.11258330249199));
#19042=CARTESIAN_POINT('Ctrl Pts',(-38.5133643814276,34.9979909506281,3.38741669750802));
#19043=CARTESIAN_POINT('Ctrl Pts',(-38.5157099610507,34.5578454548766,3.4072765672669));
#19044=CARTESIAN_POINT('Ctrl Pts',(-38.4388798941057,34.1184888224752,3.42713643702577));
#19045=CARTESIAN_POINT('Ctrl Pts',(-38.2790746610536,33.7117311197398,3.44699630678465));
#19046=CARTESIAN_POINT('Ctrl Pts',(-37.8579667980557,32.6398709329021,3.49932968256873));
#19047=CARTESIAN_POINT('Ctrl Pts',(-36.8606860208572,31.7943751052665,3.55166305835282));
#19048=CARTESIAN_POINT('Ctrl Pts',(-35.734367949382,31.554325747162,3.6039964341369));
#19049=CARTESIAN_POINT('Ctrl Pts',(-34.6080498779068,31.3142763890575,3.65632980992099));
#19050=CARTESIAN_POINT('Ctrl Pts',(-33.3526945121549,31.6796735004841,3.70866318570507));
#19051=CARTESIAN_POINT('Ctrl Pts',(-32.5311464521593,32.4866895335911,3.76099656148916));
#19052=CARTESIAN_POINT('Ctrl Pts',(-31.7095983921637,33.2937055666981,3.81332993727324));
#19053=CARTESIAN_POINT('Ctrl Pts',(-31.3218576379244,34.5423405214855,3.86566331305732));
#19054=CARTESIAN_POINT('Ctrl Pts',(-31.5417696164559,35.6727629267273,3.91799668884141));
#19055=CARTESIAN_POINT('Ctrl Pts',(-31.7616815949873,36.8031853319691,3.97033006462549));
#19056=CARTESIAN_POINT('Ctrl Pts',(-32.5892463062895,37.8153951876653,4.02266344040958));
#19057=CARTESIAN_POINT('Ctrl Pts',(-33.6534211424138,38.2555633494147,4.07499681619366));
#19058=CARTESIAN_POINT('Ctrl Pts',(-34.7175959785381,38.6957315111641,4.12733019197775));
#19059=CARTESIAN_POINT('Ctrl Pts',(-36.0183809394846,38.5638579789666,4.17966356776183));
#19060=CARTESIAN_POINT('Ctrl Pts',(-36.9725628484569,37.9190688839933,4.23199694354592));
#19061=CARTESIAN_POINT('Ctrl Pts',(-37.9171399008999,37.2807702775639,4.28380352819995));
#19062=CARTESIAN_POINT('Ctrl Pts',(-38.5220566388619,36.1398302190111,4.33561011285399));
#19063=CARTESIAN_POINT('Ctrl Pts',(-38.5230459553398,34.9997936499459,4.38741669750802));
#19064=CARTESIAN_POINT('Origin',(-35.,35.,4.));
#19065=CARTESIAN_POINT('',(-38.5138066110977,35.0022702462197,5.38741669750802));
#19066=CARTESIAN_POINT('',(-38.5124571785126,34.9988611669454,5.11258330249198));
#19067=CARTESIAN_POINT('',(-38.5175,35.,4.));
#19068=CARTESIAN_POINT('Ctrl Pts',(-38.5124571785126,34.9988611669454,5.11258330249198));
#19069=CARTESIAN_POINT('Ctrl Pts',(-38.5105119534794,35.6536666552656,5.08305689341869));
#19070=CARTESIAN_POINT('Ctrl Pts',(-38.3345896506072,36.3094430406945,5.0535304843454));
#19071=CARTESIAN_POINT('Ctrl Pts',(-37.9913530811025,36.8611219666803,5.02400407527211));
#19072=CARTESIAN_POINT('Ctrl Pts',(-37.3829916535365,37.8389320510055,4.97167069948803));
#19073=CARTESIAN_POINT('Ctrl Pts',(-36.2490134605232,38.4897205906347,4.91933732370395));
#19074=CARTESIAN_POINT('Ctrl Pts',(-35.0978430621031,38.5217034194952,4.86700394791986));
#19075=CARTESIAN_POINT('Ctrl Pts',(-33.946672663683,38.5536862483557,4.81467057213578));
#19076=CARTESIAN_POINT('Ctrl Pts',(-32.7783100598561,37.9668633664475,4.76233719635169));
#19077=CARTESIAN_POINT('Ctrl Pts',(-32.1165962295435,37.0243396290507,4.71000382056761));
#19078=CARTESIAN_POINT('Ctrl Pts',(-31.4548823992308,36.081815891654,4.65767044478352));
#19079=CARTESIAN_POINT('Ctrl Pts',(-31.2998173424323,34.7835912987687,4.60533706899944));
#19080=CARTESIAN_POINT('Ctrl Pts',(-31.7209252206252,33.7117310732541,4.55300369321535));
#19081=CARTESIAN_POINT('Ctrl Pts',(-32.1420330988181,32.6398708477396,4.50067031743127));
#19082=CARTESIAN_POINT('Ctrl Pts',(-33.1393139120024,31.7943749895958,4.44833694164718));
#19083=CARTESIAN_POINT('Ctrl Pts',(-34.2656320241194,31.5543256228295,4.3960035658631));
#19084=CARTESIAN_POINT('Ctrl Pts',(-35.3919501362363,31.3142762560632,4.34367019007901));
#19085=CARTESIAN_POINT('Ctrl Pts',(-36.647305547286,31.6796733806745,4.29133681429493));
#19086=CARTESIAN_POINT('Ctrl Pts',(-37.4688536369261,32.4866894429016,4.23900343851085));
#19087=CARTESIAN_POINT('Ctrl Pts',(-38.1303831719009,33.1365174530869,4.19686339317123));
#19088=CARTESIAN_POINT('Ctrl Pts',(-38.5106388460078,34.0726842535258,4.15472334783161));
#19089=CARTESIAN_POINT('Ctrl Pts',(-38.5188569925171,35.0029051522836,4.11258330249198));
#19090=CARTESIAN_POINT('Ctrl Pts',(-38.5230459553398,34.9997936499459,4.38741669750802));
#19091=CARTESIAN_POINT('Ctrl Pts',(-38.5230560151256,34.9882012788887,4.38794348863807));
#19092=CARTESIAN_POINT('Ctrl Pts',(-38.5230036307651,34.9766090012494,4.38847027976812));
#19093=CARTESIAN_POINT('Ctrl Pts',(-38.5228885244128,34.9650173464461,4.38899707089817));
#19094=CARTESIAN_POINT('Ctrl Pts',(-38.5114534343983,33.813459561621,4.44133044668225));
#19095=CARTESIAN_POINT('Ctrl Pts',(-37.881004397371,32.66804864972,4.49366382246634));
#19096=CARTESIAN_POINT('Ctrl Pts',(-36.9142062633822,32.0423350890982,4.54599719825042));
#19097=CARTESIAN_POINT('Ctrl Pts',(-35.9474081293934,31.4166215284763,4.59833057403451));
#19098=CARTESIAN_POINT('Ctrl Pts',(-34.6442608984431,31.3106053191336,4.65066394981859));
#19099=CARTESIAN_POINT('Ctrl Pts',(-33.5890368820876,31.7718193336147,4.70299732560267));
#19100=CARTESIAN_POINT('Ctrl Pts',(-32.533812865732,32.2330333480957,4.75533070138676));
#19101=CARTESIAN_POINT('Ctrl Pts',(-31.7265120639713,33.2614775864005,4.80766407717084));
#19102=CARTESIAN_POINT('Ctrl Pts',(-31.5290916644384,34.3960441480086,4.85999745295493));
#19103=CARTESIAN_POINT('Ctrl Pts',(-31.3316712649055,35.5306107096167,4.91233082873901));
#19104=CARTESIAN_POINT('Ctrl Pts',(-31.7441312676005,36.771299594528,4.9646642045231));
#19105=CARTESIAN_POINT('Ctrl Pts',(-32.5815432503882,37.5618419758867,5.01699758030718));
#19106=CARTESIAN_POINT('Ctrl Pts',(-33.418955233176,38.3523843572453,5.06933095609127));
#19107=CARTESIAN_POINT('Ctrl Pts',(-34.6813191960565,38.6927802350512,5.12166433187535));
#19108=CARTESIAN_POINT('Ctrl Pts',(-35.8026482038993,38.4304115128643,5.17399770765944));
#19109=CARTESIAN_POINT('Ctrl Pts',(-36.9239772117421,38.1680427906774,5.22633108344352));
#19110=CARTESIAN_POINT('Ctrl Pts',(-37.9042712645471,37.3029094684976,5.2786644592276));
#19111=CARTESIAN_POINT('Ctrl Pts',(-38.3040108156146,36.2228981644233,5.33099783501169));
#19112=CARTESIAN_POINT('Ctrl Pts',(-38.4476594300862,35.8347901400117,5.34980412251047));
#19113=CARTESIAN_POINT('Ctrl Pts',(-38.5163373319043,35.4189335486904,5.36861041000924));
#19114=CARTESIAN_POINT('Ctrl Pts',(-38.5138066110977,35.0022702462197,5.38741669750802));
#19115=CARTESIAN_POINT('Origin',(-35.,35.,4.));
#19116=CARTESIAN_POINT('',(-38.5163029138352,34.997016742257,6.38741669750802));
#19117=CARTESIAN_POINT('',(-38.5224238694764,34.9986908177615,6.11258330249199));
#19118=CARTESIAN_POINT('',(-38.5175,35.,4.));
#19119=CARTESIAN_POINT('Ctrl Pts',(-38.5224238694764,34.9986908177615,6.11258330249199));
#19120=CARTESIAN_POINT('Ctrl Pts',(-38.5172129982537,36.0743835623573,6.06372381478987));
#19121=CARTESIAN_POINT('Ctrl Pts',(-37.9876402962914,37.154522030678,6.01486432708775));
#19122=CARTESIAN_POINT('Ctrl Pts',(-37.1315952103829,37.8050436089632,5.96600483938563));
#19123=CARTESIAN_POINT('Ctrl Pts',(-36.2146856954469,38.5018169852953,5.91367146360155));
#19124=CARTESIAN_POINT('Ctrl Pts',(-34.9232293447652,38.705710551088,5.86133808781746));
#19125=CARTESIAN_POINT('Ctrl Pts',(-33.8362566580758,38.325307472034,5.80900471203338));
#19126=CARTESIAN_POINT('Ctrl Pts',(-32.7492839713864,37.9449043929801,5.75667133624929));
#19127=CARTESIAN_POINT('Ctrl Pts',(-31.8667949486893,36.9802046690794,5.70433796046521));
#19128=CARTESIAN_POINT('Ctrl Pts',(-31.5844578508488,35.8637361363978,5.65200458468113));
#19129=CARTESIAN_POINT('Ctrl Pts',(-31.3021207530084,34.7472676037162,5.59967120889704));
#19130=CARTESIAN_POINT('Ctrl Pts',(-31.6199355800247,33.4790302622538,5.54733783311296));
#19131=CARTESIAN_POINT('Ctrl Pts',(-32.3954084927658,32.6276443641247,5.49500445732887));
#19132=CARTESIAN_POINT('Ctrl Pts',(-33.1708814055069,31.7762584659956,5.44267108154479));
#19133=CARTESIAN_POINT('Ctrl Pts',(-34.4040124039728,31.3417240112,5.39033770576071));
#19134=CARTESIAN_POINT('Ctrl Pts',(-35.5419213082836,31.5188666284535,5.33800432997662));
#19135=CARTESIAN_POINT('Ctrl Pts',(-36.6798302125945,31.6960092457071,5.28567095419254));
#19136=CARTESIAN_POINT('Ctrl Pts',(-37.7225170227502,32.4848289350099,5.23333757840845));
#19137=CARTESIAN_POINT('Ctrl Pts',(-38.2024880967687,33.5316545941719,5.18100420262437));
#19138=CARTESIAN_POINT('Ctrl Pts',(-38.4116602387006,33.987862847563,5.15819723591357));
#19139=CARTESIAN_POINT('Ctrl Pts',(-38.5139597209473,34.4930723682773,5.13539026920278));
#19140=CARTESIAN_POINT('Ctrl Pts',(-38.5124571785126,34.9988611669454,5.11258330249198));
#19141=CARTESIAN_POINT('Ctrl Pts',(-38.5138066110977,35.0022702462197,5.38741669750802));
#19142=CARTESIAN_POINT('Ctrl Pts',(-38.5092949444589,34.2594597724306,5.42094378579333));
#19143=CARTESIAN_POINT('Ctrl Pts',(-38.2784657870358,33.5140853838181,5.45447087407863));
#19144=CARTESIAN_POINT('Ctrl Pts',(-37.8426352258847,32.9188002435034,5.48799796236394));
#19145=CARTESIAN_POINT('Ctrl Pts',(-37.1623350357574,31.9896029126267,5.54033133814803));
#19146=CARTESIAN_POINT('Ctrl Pts',(-35.9825496061728,31.4260975368425,5.59266471393211));
#19147=CARTESIAN_POINT('Ctrl Pts',(-34.8322413698574,31.4809342241349,5.6449980897162));
#19148=CARTESIAN_POINT('Ctrl Pts',(-33.681933133542,31.5357709114273,5.69733146550028));
#19149=CARTESIAN_POINT('Ctrl Pts',(-32.5611020904959,32.2089496617965,5.74966484128436));
#19150=CARTESIAN_POINT('Ctrl Pts',(-31.9722782631938,33.1986480172104,5.80199821706845));
#19151=CARTESIAN_POINT('Ctrl Pts',(-31.3834544358917,34.1883463726244,5.85433159285253));
#19152=CARTESIAN_POINT('Ctrl Pts',(-31.3266378243335,35.4945643330831,5.90666496863662));
#19153=CARTESIAN_POINT('Ctrl Pts',(-31.8273023322845,36.531651876217,5.95899834442071));
#19154=CARTESIAN_POINT('Ctrl Pts',(-32.3279668402356,37.5687394193509,6.01133172020479));
#19155=CARTESIAN_POINT('Ctrl Pts',(-33.3861124676959,38.3366965451598,6.06366509598887));
#19156=CARTESIAN_POINT('Ctrl Pts',(-34.5273147413959,38.4912078741205,6.11599847177296));
#19157=CARTESIAN_POINT('Ctrl Pts',(-35.668517015096,38.6457192030811,6.16833184755704));
#19158=CARTESIAN_POINT('Ctrl Pts',(-36.8927759350357,38.1867847351935,6.22066522334113));
#19159=CARTESIAN_POINT('Ctrl Pts',(-37.6511887502036,37.3201661507465,6.27299859912521));
#19160=CARTESIAN_POINT('Ctrl Pts',(-38.2039026464539,36.688594367157,6.31113796525282));
#19161=CARTESIAN_POINT('Ctrl Pts',(-38.5091981905113,35.8404949979527,6.34927733138042));
#19162=CARTESIAN_POINT('Ctrl Pts',(-38.5163029138352,34.997016742257,6.38741669750802));
#19163=CARTESIAN_POINT('Origin',(-35.,35.,4.));
#19164=CARTESIAN_POINT('',(-38.521739013009,35.0017650567249,7.38741669750802));
#19165=CARTESIAN_POINT('',(-38.5153120432796,35.002811202661,7.11258330249199));
#19166=CARTESIAN_POINT('',(-38.5175,35.,4.));
#19167=CARTESIAN_POINT('',(-32.3264680662287,37.2858331630075,8.));
#19168=CARTESIAN_POINT('Ctrl Pts',(-38.521739013009,35.0017650567249,7.38741669750802));
#19169=CARTESIAN_POINT('Ctrl Pts',(-38.515045138314,33.9623979425516,7.43461100431976));
#19170=CARTESIAN_POINT('Ctrl Pts',(-38.025374647688,32.917767542155,7.4818053111315));
#19171=CARTESIAN_POINT('Ctrl Pts',(-37.2186053621485,32.2635140899837,7.52899961794324));
#19172=CARTESIAN_POINT('Ctrl Pts',(-36.3239855860891,31.5380178578407,7.58133299372732));
#19173=CARTESIAN_POINT('Ctrl Pts',(-35.039448183402,31.2925450618756,7.63366636951141));
#19174=CARTESIAN_POINT('Ctrl Pts',(-33.9411232613757,31.6392615106971,7.68599974529549));
#19175=CARTESIAN_POINT('Ctrl Pts',(-32.8427983393495,31.9859779595187,7.73833312107958));
#19176=CARTESIAN_POINT('Ctrl Pts',(-31.9306858979841,32.9248836531268,7.79066649686366));
#19177=CARTESIAN_POINT('Ctrl Pts',(-31.6136962443577,34.0300695623378,7.84299987264775));
#19178=CARTESIAN_POINT('Ctrl Pts',(-31.2967065907312,35.1352554715487,7.89533324843183));
#19179=CARTESIAN_POINT('Ctrl Pts',(-31.5748397248436,36.4067215963625,7.94766662421592));
#19180=CARTESIAN_POINT('Ctrl Pts',(-32.3264680662287,37.2858331630075,8.));
#19181=CARTESIAN_POINT('',(-37.6785007864356,37.2890249916441,8.));
#19182=CARTESIAN_POINT('Origin',(-35.,35.,8.));
#19183=CARTESIAN_POINT('Ctrl Pts',(-37.6785239274887,37.2890398567007,8.));
#19184=CARTESIAN_POINT('Ctrl Pts',(-36.9607510630042,38.1233253004298,7.95000212253756));
#19185=CARTESIAN_POINT('Ctrl Pts',(-35.8186698457281,38.5989197552422,7.90000424507511));
#19186=CARTESIAN_POINT('Ctrl Pts',(-34.7217022012346,38.5118537728532,7.85000636761267));
#19187=CARTESIAN_POINT('Ctrl Pts',(-33.5734930596489,38.4207207687012,7.79767299182859));
#19188=CARTESIAN_POINT('Ctrl Pts',(-32.4747106147993,37.7131336670436,7.7453396160445));
#19189=CARTESIAN_POINT('Ctrl Pts',(-31.9173295125726,36.7055536114064,7.69300624026042));
#19190=CARTESIAN_POINT('Ctrl Pts',(-31.3599484103458,35.6979735557692,7.64067286447633));
#19191=CARTESIAN_POINT('Ctrl Pts',(-31.3439686507417,34.3904005461523,7.58833948869225));
#19192=CARTESIAN_POINT('Ctrl Pts',(-31.8768870047646,33.3694814192899,7.53600611290817));
#19193=CARTESIAN_POINT('Ctrl Pts',(-32.4098053587874,32.3485622924274,7.48367273712408));
#19194=CARTESIAN_POINT('Ctrl Pts',(-33.4916218264372,31.6142970483194,7.43133936134));
#19195=CARTESIAN_POINT('Ctrl Pts',(-34.6371339251584,31.4957034085517,7.37900598555591));
#19196=CARTESIAN_POINT('Ctrl Pts',(-35.7826460238797,31.3771097687841,7.32667260977183));
#19197=CARTESIAN_POINT('Ctrl Pts',(-36.9918537536724,31.8741877333568,7.27433923398774));
#19198=CARTESIAN_POINT('Ctrl Pts',(-37.7226848809369,32.7641661288242,7.22200585820366));
#19199=CARTESIAN_POINT('Ctrl Pts',(-38.232043765465,33.3844440368906,7.18553167296644));
#19200=CARTESIAN_POINT('Ctrl Pts',(-38.5090307393652,34.1955737201714,7.14905748772921));
#19201=CARTESIAN_POINT('Ctrl Pts',(-38.5153120432796,35.002811202661,7.11258330249199));
#19202=CARTESIAN_POINT('Origin',(-35.,-35.,4.));
#19203=CARTESIAN_POINT('',(-38.5120271382808,-35.0001374244476,0.387416697508025));
#19204=CARTESIAN_POINT('',(-38.5151976130935,-35.0046525930694,0.112583302491978));
#19205=CARTESIAN_POINT('',(-38.5175,-35.,4.));
#19206=CARTESIAN_POINT('',(-37.6735319337713,-32.7141668369925,0.));
#19207=CARTESIAN_POINT('Ctrl Pts',(-38.5151976130935,-35.0046525930694,
0.112583302491978));
#19208=CARTESIAN_POINT('Ctrl Pts',(-38.5080219923978,-34.1767290340604,
0.075055534994651));
#19209=CARTESIAN_POINT('Ctrl Pts',(-38.2125174896864,-33.3445694048179,
0.0375277674973242));
#19210=CARTESIAN_POINT('Ctrl Pts',(-37.6735319337713,-32.7141668369925,
-2.28983498828939E-15));
#19211=CARTESIAN_POINT('',(-32.3214990837181,-32.7109751024398,8.09549783939668E-17));
#19212=CARTESIAN_POINT('Origin',(-35.,-35.,0.));
#19213=CARTESIAN_POINT('Ctrl Pts',(-32.3214759334524,-32.7109602322923,
3.12480707463443E-17));
#19214=CARTESIAN_POINT('Ctrl Pts',(-33.0392487617403,-31.8766749582113,
0.0499978774624439));
#19215=CARTESIAN_POINT('Ctrl Pts',(-34.1813300785248,-31.4010800346315,
0.099995754924887));
#19216=CARTESIAN_POINT('Ctrl Pts',(-35.2782977997678,-31.4881459202074,
0.149993632387331));
#19217=CARTESIAN_POINT('Ctrl Pts',(-36.4265070216881,-31.5792788230239,
0.202327008171415));
#19218=CARTESIAN_POINT('Ctrl Pts',(-37.5252895219377,-32.2868662308611,
0.254660383955499));
#19219=CARTESIAN_POINT('Ctrl Pts',(-38.0826706431354,-33.2944463926721,
0.306993759739583));
#19220=CARTESIAN_POINT('Ctrl Pts',(-38.3681877823846,-33.8105769080839,
0.333801405662397));
#19221=CARTESIAN_POINT('Ctrl Pts',(-38.5116424994856,-34.4054248019609,
0.360609051585211));
#19222=CARTESIAN_POINT('Ctrl Pts',(-38.5120271382808,-35.0001374244476,
0.387416697508025));
#19223=CARTESIAN_POINT('Origin',(-35.,-35.,4.));
#19224=CARTESIAN_POINT('',(-38.5212304296149,-35.0021519659852,1.38741669750803));
#19225=CARTESIAN_POINT('',(-38.5220168341852,-34.9983176676613,1.11258330249198));
#19226=CARTESIAN_POINT('',(-38.5175,-35.,4.));
#19227=CARTESIAN_POINT('Ctrl Pts',(-38.5220168341852,-34.9983176676613,
1.11258330249198));
#19228=CARTESIAN_POINT('Ctrl Pts',(-38.52260684792,-34.8986110126186,1.10805583214991));
#19229=CARTESIAN_POINT('Ctrl Pts',(-38.5187311767415,-34.7989511930367,
1.10352836180784));
#19230=CARTESIAN_POINT('Ctrl Pts',(-38.5102392653976,-34.699686678491,1.09900089146577));
#19231=CARTESIAN_POINT('Ctrl Pts',(-38.4120806130139,-33.5522805666331,
1.04666751568169));
#19232=CARTESIAN_POINT('Ctrl Pts',(-37.6971357336766,-32.4576920494149,
0.994334139897603));
#19233=CARTESIAN_POINT('Ctrl Pts',(-36.6859405355102,-31.906559687218,0.942000764113519));
#19234=CARTESIAN_POINT('Ctrl Pts',(-35.6747453373438,-31.355427325021,0.889667388329434));
#19235=CARTESIAN_POINT('Ctrl Pts',(-34.3672998203483,-31.3477511178455,
0.83733401254535));
#19236=CARTESIAN_POINT('Ctrl Pts',(-33.3498297550083,-31.8872254772169,
0.785000636761265));
#19237=CARTESIAN_POINT('Ctrl Pts',(-32.3323596896683,-32.4266998365882,
0.732667260977181));
#19238=CARTESIAN_POINT('Ctrl Pts',(-31.6048650759839,-33.5133247625066,
0.680333885193095));
#19239=CARTESIAN_POINT('Ctrl Pts',(-31.4934686932928,-34.6593973938948,
0.628000509409011));
#19240=CARTESIAN_POINT('Ctrl Pts',(-31.3820723106017,-35.8054700252831,
0.575667133624927));
#19241=CARTESIAN_POINT('Ctrl Pts',(-31.8867741589039,-37.0109903621411,
0.523333757840844));
#19242=CARTESIAN_POINT('Ctrl Pts',(-32.7813942262272,-37.7364865047087,
0.47100038205676));
#19243=CARTESIAN_POINT('Ctrl Pts',(-33.6760142935505,-38.4619826472763,
0.418667006272675));
#19244=CARTESIAN_POINT('Ctrl Pts',(-34.9605525798949,-38.7074545955534,
0.366333630488589));
#19245=CARTESIAN_POINT('Ctrl Pts',(-36.0588770784695,-38.3607385484851,
0.314000254704505));
#19246=CARTESIAN_POINT('Ctrl Pts',(-37.157201577044,-38.0140225014167,0.26166687892042));
#19247=CARTESIAN_POINT('Ctrl Pts',(-38.0693122878488,-37.0751184590028,
0.209333503136336));
#19248=CARTESIAN_POINT('Ctrl Pts',(-38.3863019623769,-35.9699324345579,
0.157000127352251));
#19249=CARTESIAN_POINT('Ctrl Pts',(-38.4759813473142,-35.6572648277626,
0.142194519065493));
#19250=CARTESIAN_POINT('Ctrl Pts',(-38.518028568312,-35.3312883810079,0.127388910778735));
#19251=CARTESIAN_POINT('Ctrl Pts',(-38.5151976130935,-35.0046525930694,
0.112583302491978));
#19252=CARTESIAN_POINT('Ctrl Pts',(-38.5120271382808,-35.0001374244476,
0.387416697508025));
#19253=CARTESIAN_POINT('Ctrl Pts',(-38.5123933840156,-35.5664114565052,
0.412942427369296));
#19254=CARTESIAN_POINT('Ctrl Pts',(-38.3830453480461,-36.1325628449505,
0.438468157230567));
#19255=CARTESIAN_POINT('Ctrl Pts',(-38.1231131273625,-36.6305186098067,
0.463993887091838));
#19256=CARTESIAN_POINT('Ctrl Pts',(-37.5901947482463,-37.6514377493457,
0.516327262875923));
#19257=CARTESIAN_POINT('Ctrl Pts',(-36.5083782478681,-38.3857031126391,
0.568660638660007));
#19258=CARTESIAN_POINT('Ctrl Pts',(-35.362866098922,-38.5042967770896,0.620994014444091));
#19259=CARTESIAN_POINT('Ctrl Pts',(-34.2173539499758,-38.6228904415402,
0.673327390228176));
#19260=CARTESIAN_POINT('Ctrl Pts',(-33.0081461524618,-38.1258124071479,
0.72566076601226));
#19261=CARTESIAN_POINT('Ctrl Pts',(-32.2773149895643,-37.2358339601687,
0.777994141796345));
#19262=CARTESIAN_POINT('Ctrl Pts',(-31.5464838266669,-36.3458555131895,
0.83032751758043));
#19263=CARTESIAN_POINT('Ctrl Pts',(-31.294029298386,-35.0629766536234,0.882660893364515));
#19264=CARTESIAN_POINT('Ctrl Pts',(-31.6331812255463,-33.9624299433603,
0.934994269148599));
#19265=CARTESIAN_POINT('Ctrl Pts',(-31.9723331527066,-32.8618832330971,
0.987327644932684));
#19266=CARTESIAN_POINT('Ctrl Pts',(-32.9030915353081,-31.9436686721369,
1.03966102071677));
#19267=CARTESIAN_POINT('Ctrl Pts',(-34.0081262229406,-31.6194484991129,
1.09199439650085));
#19268=CARTESIAN_POINT('Ctrl Pts',(-35.1131609105731,-31.2952283260889,
1.14432777228494));
#19269=CARTESIAN_POINT('Ctrl Pts',(-36.3924719032364,-31.5650025410011,
1.19666114806902));
#19270=CARTESIAN_POINT('Ctrl Pts',(-37.2724839907223,-32.3078283275476,
1.24899452385311));
#19271=CARTESIAN_POINT('Ctrl Pts',(-38.0483635269158,-32.9627549301865,
1.29513524840475));
#19272=CARTESIAN_POINT('Ctrl Pts',(-38.5138518348506,-33.9854036989656,
1.34127597295639));
#19273=CARTESIAN_POINT('Ctrl Pts',(-38.5212304296149,-35.0021519659852,
1.38741669750803));
#19274=CARTESIAN_POINT('Origin',(-35.,-35.,4.));
#19275=CARTESIAN_POINT('',(-38.5169621951111,-34.9969726963287,2.38741669750803));
#19276=CARTESIAN_POINT('',(-38.5122617995812,-34.9992080290324,2.11258330249198));
#19277=CARTESIAN_POINT('',(-38.5175,-35.,4.));
#19278=CARTESIAN_POINT('Ctrl Pts',(-38.5122617995812,-34.9992080290324,
2.11258330249198));
#19279=CARTESIAN_POINT('Ctrl Pts',(-38.5133509957446,-34.4699799892041,
2.08872275352108));
#19280=CARTESIAN_POINT('Ctrl Pts',(-38.4009678500058,-33.9411911577145,
2.06486220455019));
#19281=CARTESIAN_POINT('Ctrl Pts',(-38.1726980103725,-33.4683479591114,
2.04100165557929));
#19282=CARTESIAN_POINT('Ctrl Pts',(-37.6720334484517,-32.4312603032644,
1.98866827979521));
#19283=CARTESIAN_POINT('Ctrl Pts',(-36.613887707127,-31.6633030916115,1.93633490401112));
#19284=CARTESIAN_POINT('Ctrl Pts',(-35.4726853098873,-31.5087917472057,
1.88400152822704));
#19285=CARTESIAN_POINT('Ctrl Pts',(-34.3314829126475,-31.3542804028,1.83166815244296));
#19286=CARTESIAN_POINT('Ctrl Pts',(-33.1072238594927,-31.8132149256414,
1.77933477665887));
#19287=CARTESIAN_POINT('Ctrl Pts',(-32.3488109629184,-32.6798336014156,
1.72700140087479));
#19288=CARTESIAN_POINT('Ctrl Pts',(-31.5903980663441,-33.5464522771898,
1.6746680250907));
#19289=CARTESIAN_POINT('Ctrl Pts',(-31.2978313263503,-34.8207551058968,
1.62233464930662));
#19290=CARTESIAN_POINT('Ctrl Pts',(-31.602283651433,-35.931394685751,1.57000127352253));
#19291=CARTESIAN_POINT('Ctrl Pts',(-31.9067359765157,-37.0420342656052,
1.51766789773845));
#19292=CARTESIAN_POINT('Ctrl Pts',(-32.808207366675,-37.9890105966065,1.46533452195436));
#19293=CARTESIAN_POINT('Ctrl Pts',(-33.9025203970559,-38.3477576413965,
1.41300114617028));
#19294=CARTESIAN_POINT('Ctrl Pts',(-34.9968334274368,-38.7065046861866,
1.36066777038619));
#19295=CARTESIAN_POINT('Ctrl Pts',(-36.2839880980393,-38.4770224447653,
1.30833439460211));
#19296=CARTESIAN_POINT('Ctrl Pts',(-37.1868792206255,-37.7621694708059,
1.25600101881803));
#19297=CARTESIAN_POINT('Ctrl Pts',(-38.0116593343501,-37.1091599302205,
1.20819511337601));
#19298=CARTESIAN_POINT('Ctrl Pts',(-38.515786834056,-36.0511278602802,1.16038920793399));
#19299=CARTESIAN_POINT('Ctrl Pts',(-38.5220168341852,-34.9983176676613,
1.11258330249198));
#19300=CARTESIAN_POINT('Ctrl Pts',(-38.5212304296149,-35.0021519659852,
1.38741669750803));
#19301=CARTESIAN_POINT('Ctrl Pts',(-38.5222207275437,-35.1386120556355,
1.39360934874047));
#19302=CARTESIAN_POINT('Ctrl Pts',(-38.5149591261082,-35.2749658599455,
1.39980199997291));
#19303=CARTESIAN_POINT('Ctrl Pts',(-38.4990885075235,-35.4103101250027,
1.40599465120536));
#19304=CARTESIAN_POINT('Ctrl Pts',(-38.3649677545306,-36.5540887777307,
1.45832802698944));
#19305=CARTESIAN_POINT('Ctrl Pts',(-37.6160130662365,-37.6257687250057,
1.51066140277353));
#19306=CARTESIAN_POINT('Ctrl Pts',(-36.5880243363171,-38.1448600164999,
1.56299477855761));
#19307=CARTESIAN_POINT('Ctrl Pts',(-35.5600356063977,-38.6639513079941,
1.6153281543417));
#19308=CARTESIAN_POINT('Ctrl Pts',(-34.2530128348529,-38.6304539437074,
1.66766153012578));
#19309=CARTESIAN_POINT('Ctrl Pts',(-33.2529647263785,-38.059385190685,1.71999490590987));
#19310=CARTESIAN_POINT('Ctrl Pts',(-32.2529166179041,-37.4883164376626,
1.77232828169395));
#19311=CARTESIAN_POINT('Ctrl Pts',(-31.5598431725,-36.3796762959045,1.82466165747803));
#19312=CARTESIAN_POINT('Ctrl Pts',(-31.4844878017471,-35.2305296041615,
1.87699503326212));
#19313=CARTESIAN_POINT('Ctrl Pts',(-31.4091324309942,-34.0813829124186,
1.9293284090462));
#19314=CARTESIAN_POINT('Ctrl Pts',(-31.9514951348924,-32.8917296706907,
1.98166178483029));
#19315=CARTESIAN_POINT('Ctrl Pts',(-32.8684046918336,-32.1949562623368,
2.03399516061437));
#19316=CARTESIAN_POINT('Ctrl Pts',(-33.7853142487749,-31.4981828539828,
2.08632853639846));
#19317=CARTESIAN_POINT('Ctrl Pts',(-35.0767706587592,-31.2942892790027,
2.13866191218254));
#19318=CARTESIAN_POINT('Ctrl Pts',(-36.1637433953085,-31.6746923755375,
2.19099528796663));
#19319=CARTESIAN_POINT('Ctrl Pts',(-37.2507161318578,-32.0550954720723,
2.24332866375071));
#19320=CARTESIAN_POINT('Ctrl Pts',(-38.1332051949721,-33.019795240122,2.29566203953479));
#19321=CARTESIAN_POINT('Ctrl Pts',(-38.4155423057474,-34.1362638239756,
2.34799541531888));
#19322=CARTESIAN_POINT('Ctrl Pts',(-38.4864345470726,-34.416598775556,2.36113584271526));
#19323=CARTESIAN_POINT('Ctrl Pts',(-38.519489264757,-34.7065022308021,2.37427627011164));
#19324=CARTESIAN_POINT('Ctrl Pts',(-38.5169621951111,-34.9969726963287,
2.38741669750803));
#19325=CARTESIAN_POINT('Origin',(-35.,-35.,4.));
#19326=CARTESIAN_POINT('',(-38.5133646692972,-35.0020090495363,3.38741669750803));
#19327=CARTESIAN_POINT('',(-38.5195236027652,-35.0027703381826,3.11258330249198));
#19328=CARTESIAN_POINT('',(-38.5175,-35.,4.));
#19329=CARTESIAN_POINT('Ctrl Pts',(-38.5195236027652,-35.0027703381826,
3.11258330249198));
#19330=CARTESIAN_POINT('Ctrl Pts',(-38.5112998170852,-34.0497594617567,
3.06938967489226));
#19331=CARTESIAN_POINT('Ctrl Pts',(-38.1096194803006,-33.0906361399806,
3.02619604729253));
#19332=CARTESIAN_POINT('Ctrl Pts',(-37.4184570108864,-32.4381577473637,
2.98300241969281));
#19333=CARTESIAN_POINT('Ctrl Pts',(-36.5810449376309,-31.6476152805848,
2.93066904390873));
#19334=CARTESIAN_POINT('Ctrl Pts',(-35.3186808383768,-31.3072193659425,
2.87833566812464));
#19335=CARTESIAN_POINT('Ctrl Pts',(-34.1973517093896,-31.5695881165025,
2.82600229234056));
#19336=CARTESIAN_POINT('Ctrl Pts',(-33.0760225804023,-31.8319568670625,
2.77366891655648));
#19337=CARTESIAN_POINT('Ctrl Pts',(-32.0957284216819,-32.6970902828246,
2.72133554077239));
#19338=CARTESIAN_POINT('Ctrl Pts',(-31.6959888274348,-33.7771017035233,
2.66900216498831));
#19339=CARTESIAN_POINT('Ctrl Pts',(-31.2962492331877,-34.8571131242219,
2.61666878920422));
#19340=CARTESIAN_POINT('Ctrl Pts',(-31.477064203414,-36.1520025498569,2.56433541342014));
#19341=CARTESIAN_POINT('Ctrl Pts',(-32.1573644670244,-37.0811999812203,
2.51200203763605));
#19342=CARTESIAN_POINT('Ctrl Pts',(-32.8376647306348,-38.0103974125836,
2.45966866185197));
#19343=CARTESIAN_POINT('Ctrl Pts',(-34.0174502876292,-38.5739028496752,
2.40733528606788));
#19344=CARTESIAN_POINT('Ctrl Pts',(-35.1677586482437,-38.5190661562666,
2.3550019102838));
#19345=CARTESIAN_POINT('Ctrl Pts',(-36.3180670088582,-38.4642294628581,
2.30266853449971));
#19346=CARTESIAN_POINT('Ctrl Pts',(-37.4388981730927,-37.7910506389493,
2.25033515871563));
#19347=CARTESIAN_POINT('Ctrl Pts',(-38.0277220639514,-36.8013521769744,
2.19800178293155));
#19348=CARTESIAN_POINT('Ctrl Pts',(-38.3480813072967,-36.2628905837198,
2.16952895611836));
#19349=CARTESIAN_POINT('Ctrl Pts',(-38.5109620602598,-35.6307365970085,
2.14105612930517));
#19350=CARTESIAN_POINT('Ctrl Pts',(-38.5122617995812,-34.9992080290324,
2.11258330249198));
#19351=CARTESIAN_POINT('Ctrl Pts',(-38.5169621951111,-34.9969726963287,
2.38741669750803));
#19352=CARTESIAN_POINT('Ctrl Pts',(-38.5094248976387,-35.8633367513267,
2.42660964589573));
#19353=CARTESIAN_POINT('Ctrl Pts',(-38.1853504786061,-36.7347449543441,
2.46580259428343));
#19354=CARTESIAN_POINT('Ctrl Pts',(-37.6045916266667,-37.3723557446642,
2.50499554267113));
#19355=CARTESIAN_POINT('Ctrl Pts',(-36.8291186783745,-38.2237416818415,
2.55732891845522));
#19356=CARTESIAN_POINT('Ctrl Pts',(-35.5959876233539,-38.6582761565386,
2.6096622942393));
#19357=CARTESIAN_POINT('Ctrl Pts',(-34.4580786668646,-38.4811335311572,
2.66199567002338));
#19358=CARTESIAN_POINT('Ctrl Pts',(-33.3201697103753,-38.3039909057758,
2.71432904580747));
#19359=CARTESIAN_POINT('Ctrl Pts',(-32.2774828524173,-37.5151711803159,
2.76666242159156));
#19360=CARTESIAN_POINT('Ctrl Pts',(-31.7975117563928,-36.4683454731577,
2.81899579737564));
#19361=CARTESIAN_POINT('Ctrl Pts',(-31.3175406603683,-35.4215197659996,
2.87132917315973));
#19362=CARTESIAN_POINT('Ctrl Pts',(-31.4002853262773,-34.1166880771431,
2.92366254894381));
#19363=CARTESIAN_POINT('Ctrl Pts',(-32.008646781737,-33.138877947982,2.97599592472789));
#19364=CARTESIAN_POINT('Ctrl Pts',(-32.6170082371967,-32.1610678188208,
3.02832930051198));
#19365=CARTESIAN_POINT('Ctrl Pts',(-33.7509864822071,-31.5102792493549,
3.08066267629606));
#19366=CARTESIAN_POINT('Ctrl Pts',(-34.9021569334111,-31.4782964190287,
3.13299605208015));
#19367=CARTESIAN_POINT('Ctrl Pts',(-36.0533273846151,-31.4463135887025,
3.18532942786423));
#19368=CARTESIAN_POINT('Ctrl Pts',(-37.2216900420126,-32.033136497516,3.23766280364832));
#19369=CARTESIAN_POINT('Ctrl Pts',(-37.883403902666,-32.9756602781289,3.2899961794324));
#19370=CARTESIAN_POINT('Ctrl Pts',(-38.2940055257973,-33.5605079247801,
3.32246968545761));
#19371=CARTESIAN_POINT('Ctrl Pts',(-38.5095293369816,-34.2823130619538,
3.35494319148282));
#19372=CARTESIAN_POINT('Ctrl Pts',(-38.5133646692972,-35.0020090495363,
3.38741669750803));
#19373=CARTESIAN_POINT('Origin',(-35.,-35.,4.));
#19374=CARTESIAN_POINT('',(-38.5230462440028,-35.0002063500719,4.38741669750802));
#19375=CARTESIAN_POINT('',(-38.5188572457002,-34.9970948475072,4.11258330249198));
#19376=CARTESIAN_POINT('',(-38.5175,-35.,4.));
#19377=CARTESIAN_POINT('Ctrl Pts',(-38.5188572457002,-34.9970948475072,
4.11258330249198));
#19378=CARTESIAN_POINT('Ctrl Pts',(-38.5208451479049,-34.772082045238,4.10238997204752));
#19379=CARTESIAN_POINT('Ctrl Pts',(-38.5010645257441,-34.5474171474031,
4.09219664160305));
#19380=CARTESIAN_POINT('Ctrl Pts',(-38.4582307571508,-34.3272370005912,
4.08200331115859));
#19381=CARTESIAN_POINT('Ctrl Pts',(-38.2383187548614,-33.1968144732253,
4.0296699353745));
#19382=CARTESIAN_POINT('Ctrl Pts',(-37.410753954154,-32.1846045081767,3.97733655959042));
#19383=CARTESIAN_POINT('Ctrl Pts',(-36.3465790030625,-31.7444362988739,
3.92500318380633));
#19384=CARTESIAN_POINT('Ctrl Pts',(-35.2824040519711,-31.3042680895711,
3.87266980802225));
#19385=CARTESIAN_POINT('Ctrl Pts',(-33.9816189504956,-31.4361416360142,
3.82033643223816));
#19386=CARTESIAN_POINT('Ctrl Pts',(-33.0274369384391,-32.0809308006472,
3.76800305645408));
#19387=CARTESIAN_POINT('Ctrl Pts',(-32.0732549263827,-32.7257199652802,
3.71566968067));
#19388=CARTESIAN_POINT('Ctrl Pts',(-31.4656760037452,-33.8834247481031,
3.66333630488591));
#19389=CARTESIAN_POINT('Ctrl Pts',(-31.4771110949952,-35.0349826573345,
3.61100292910183));
#19390=CARTESIAN_POINT('Ctrl Pts',(-31.4885461862452,-36.1865405665659,
3.55866955331774));
#19391=CARTESIAN_POINT('Ctrl Pts',(-32.1189952913826,-37.3319516022057,
3.50633617753366));
#19392=CARTESIAN_POINT('Ctrl Pts',(-33.0857935298184,-37.957665230428,3.45400280174958));
#19393=CARTESIAN_POINT('Ctrl Pts',(-34.0525917682542,-38.5833788586504,
3.40166942596549));
#19394=CARTESIAN_POINT('Ctrl Pts',(-35.3557391399884,-38.6893950794552,
3.3493360501814));
#19395=CARTESIAN_POINT('Ctrl Pts',(-36.4109632703443,-38.2281810151433,
3.29700267439732));
#19396=CARTESIAN_POINT('Ctrl Pts',(-37.4661874007003,-37.7669669508313,
3.24466929861323));
#19397=CARTESIAN_POINT('Ctrl Pts',(-38.273488289678,-36.7385226014027,3.19233592282915));
#19398=CARTESIAN_POINT('Ctrl Pts',(-38.4709087105384,-35.6039559172305,
3.14000254704507));
#19399=CARTESIAN_POINT('Ctrl Pts',(-38.5053871462609,-35.4058098271621,
3.1308627988607));
#19400=CARTESIAN_POINT('Ctrl Pts',(-38.5212637513569,-35.2044269229967,
3.12172305067634));
#19401=CARTESIAN_POINT('Ctrl Pts',(-38.5195236027652,-35.0027703381826,
3.11258330249198));
#19402=CARTESIAN_POINT('Ctrl Pts',(-38.5133646692972,-35.0020090495363,
3.38741669750803));
#19403=CARTESIAN_POINT('Ctrl Pts',(-38.5157102491126,-35.4421545813516,
3.4072765672669));
#19404=CARTESIAN_POINT('Ctrl Pts',(-38.4388801758726,-35.8815112497523,
3.42713643702578));
#19405=CARTESIAN_POINT('Ctrl Pts',(-38.2790749297269,-36.2882689858157,
3.44699630678465));
#19406=CARTESIAN_POINT('Ctrl Pts',(-37.8579670322255,-37.3601292604774,
3.49932968256874));
#19407=CARTESIAN_POINT('Ctrl Pts',(-36.8606861733137,-38.2056251573884,
3.55166305835282));
#19408=CARTESIAN_POINT('Ctrl Pts',(-35.7343680095528,-38.4456745351613,
3.60399643413691));
#19409=CARTESIAN_POINT('Ctrl Pts',(-34.6080498457918,-38.6857239129342,
3.65632980992099));
#19410=CARTESIAN_POINT('Ctrl Pts',(-33.3526943771818,-38.3203267715691,
3.70866318570508));
#19411=CARTESIAN_POINT('Ctrl Pts',(-32.5311462498722,-37.5133106723387,
3.76099656148916));
#19412=CARTESIAN_POINT('Ctrl Pts',(-31.7095981225626,-36.7062945731084,
3.81332993727325));
#19413=CARTESIAN_POINT('Ctrl Pts',(-31.3218573365535,-35.4576595160129,
3.86566331305733));
#19414=CARTESIAN_POINT('Ctrl Pts',(-31.5417693331035,-34.3272370181493,
3.91799668884141));
#19415=CARTESIAN_POINT('Ctrl Pts',(-31.7616813296536,-33.1968145202857,
3.9703300646255));
#19416=CARTESIAN_POINT('Ctrl Pts',(-32.5892461087628,-32.184604581654,4.02266344040958));
#19417=CARTESIAN_POINT('Ctrl Pts',(-33.653421032081,-31.7444363838389,4.07499681619367));
#19418=CARTESIAN_POINT('Ctrl Pts',(-34.7175959553992,-31.3042681860239,
4.12733019197775));
#19419=CARTESIAN_POINT('Ctrl Pts',(-36.0183810229263,-31.4361417290255,
4.17966356776184));
#19420=CARTESIAN_POINT('Ctrl Pts',(-36.9725630100801,-32.0809308768304,
4.23199694354592));
#19421=CARTESIAN_POINT('Ctrl Pts',(-37.9171401399176,-32.7192295355597,
4.28380352819995));
#19422=CARTESIAN_POINT('Ctrl Pts',(-38.5220569274439,-33.8601696875978,
4.33561011285399));
#19423=CARTESIAN_POINT('Ctrl Pts',(-38.5230462440028,-35.0002063500719,
4.38741669750802));
#19424=CARTESIAN_POINT('Origin',(-35.,-35.,4.));
#19425=CARTESIAN_POINT('',(-38.5138068989996,-34.9977297535637,5.38741669750802));
#19426=CARTESIAN_POINT('',(-38.5124574312326,-35.001138833141,5.11258330249198));
#19427=CARTESIAN_POINT('',(-38.5175,-35.,4.));
#19428=CARTESIAN_POINT('Ctrl Pts',(-38.5124574312326,-35.001138833141,5.11258330249198));
#19429=CARTESIAN_POINT('Ctrl Pts',(-38.5105122060607,-34.3463332977053,
5.08305689341869));
#19430=CARTESIAN_POINT('Ctrl Pts',(-38.3345898905329,-33.6905568650893,
5.0535304843454));
#19431=CARTESIAN_POINT('Ctrl Pts',(-37.9913532963331,-33.1388778994087,
5.02400407527211));
#19432=CARTESIAN_POINT('Ctrl Pts',(-37.3829918249966,-32.1610677447274,
4.97167069948802));
#19433=CARTESIAN_POINT('Ctrl Pts',(-36.2490135503901,-31.5102791582787,
4.91933732370394));
#19434=CARTESIAN_POINT('Ctrl Pts',(-35.0978430691422,-31.4782963271182,
4.86700394791986));
#19435=CARTESIAN_POINT('Ctrl Pts',(-33.9466725878942,-31.4463134959578,
4.81467057213577));
#19436=CARTESIAN_POINT('Ctrl Pts',(-32.7783099000047,-32.0331364200855,
4.76233719635169));
#19437=CARTESIAN_POINT('Ctrl Pts',(-32.1165960220819,-32.9756602252966,
4.7100038205676));
#19438=CARTESIAN_POINT('Ctrl Pts',(-31.454882144159,-33.9181840305077,4.65767044478352));
#19439=CARTESIAN_POINT('Ctrl Pts',(-31.2998170762027,-35.216408716802,4.60533706899943));
#19440=CARTESIAN_POINT('Ctrl Pts',(-31.7209249846943,-36.2882690194377,
4.55300369321535));
#19441=CARTESIAN_POINT('Ctrl Pts',(-32.1420328931859,-37.3601293220733,
4.50067031743126));
#19442=CARTESIAN_POINT('Ctrl Pts',(-33.1393137781253,-38.2056252410501,
4.44833694164718));
#19443=CARTESIAN_POINT('Ctrl Pts',(-34.2656319712814,-38.4456746250879,
4.39600356586309));
#19444=CARTESIAN_POINT('Ctrl Pts',(-35.3919501644375,-38.6857240091257,
4.34367019007901));
#19445=CARTESIAN_POINT('Ctrl Pts',(-36.6473056658103,-38.3203268582244,
4.29133681429492));
#19446=CARTESIAN_POINT('Ctrl Pts',(-37.468853814561,-37.5133107379322,4.23900343851084));
#19447=CARTESIAN_POINT('Ctrl Pts',(-38.1303833971331,-36.8634826809916,
4.19686339317122));
#19448=CARTESIAN_POINT('Ctrl Pts',(-38.5106390985996,-35.9273158131948,
4.1547233478316));
#19449=CARTESIAN_POINT('Ctrl Pts',(-38.5188572457002,-34.9970948475072,
4.11258330249198));
#19450=CARTESIAN_POINT('Ctrl Pts',(-38.5230462440028,-35.0002063500719,
4.38741669750802));
#19451=CARTESIAN_POINT('Ctrl Pts',(-38.5230563037894,-35.0117987220789,
4.38794348863807));
#19452=CARTESIAN_POINT('Ctrl Pts',(-38.5230039194247,-35.023391000668,4.38847027976812));
#19453=CARTESIAN_POINT('Ctrl Pts',(-38.5228888130629,-35.0349826564212,
4.38899707089817));
#19454=CARTESIAN_POINT('Ctrl Pts',(-38.5114537221114,-36.186540535599,4.44133044668226));
#19455=CARTESIAN_POINT('Ctrl Pts',(-37.8810046334278,-37.3319515413465,
4.49366382246634));
#19456=CARTESIAN_POINT('Ctrl Pts',(-36.9142064202239,-37.9576651532382,
4.54599719825043));
#19457=CARTESIAN_POINT('Ctrl Pts',(-35.94740820702,-38.5833787651299,4.59833057403451));
#19458=CARTESIAN_POINT('Ctrl Pts',(-34.6442608692957,-38.6893949831658,
4.6506639498186));
#19459=CARTESIAN_POINT('Ctrl Pts',(-33.5890367664795,-38.2281809308918,
4.70299732560268));
#19460=CARTESIAN_POINT('Ctrl Pts',(-32.5338126636633,-37.7669668786178,
4.75533070138677));
#19461=CARTESIAN_POINT('Ctrl Pts',(-31.7265117957552,-36.7385225560339,
4.80766407717085));
#19462=CARTESIAN_POINT('Ctrl Pts',(-31.529091380047,-35.6039559014703,4.85999745295494));
#19463=CARTESIAN_POINT('Ctrl Pts',(-31.3316709643388,-34.4693892469067,
4.91233082873902));
#19464=CARTESIAN_POINT('Ctrl Pts',(-31.7441310008306,-33.2287002603633,
4.9646642045231));
#19465=CARTESIAN_POINT('Ctrl Pts',(-32.5815430522312,-32.4381578142198,
5.01699758030719));
#19466=CARTESIAN_POINT('Ctrl Pts',(-33.4189551036319,-31.6476153680763,
5.06933095609127));
#19467=CARTESIAN_POINT('Ctrl Pts',(-34.6813191699414,-31.3072194623328,
5.12166433187536));
#19468=CARTESIAN_POINT('Ctrl Pts',(-35.8026482696631,-31.5695882060385,
5.17399770765944));
#19469=CARTESIAN_POINT('Ctrl Pts',(-36.9239773693848,-31.8319569497442,
5.22633108344353));
#19470=CARTESIAN_POINT('Ctrl Pts',(-37.9042715025186,-32.6970903428993,
5.27866445922761));
#19471=CARTESIAN_POINT('Ctrl Pts',(-38.3040110863345,-33.7771017354242,
5.33099783501169));
#19472=CARTESIAN_POINT('Ctrl Pts',(-38.4476597125745,-34.1652097916211,
5.34980412251047));
#19473=CARTESIAN_POINT('Ctrl Pts',(-38.5163376200166,-34.5810664169843,
5.36861041000925));
#19474=CARTESIAN_POINT('Ctrl Pts',(-38.5138068989996,-34.9977297535637,
5.38741669750802));
#19475=CARTESIAN_POINT('Origin',(-35.,-35.,4.));
#19476=CARTESIAN_POINT('',(-38.5163032009778,-35.0029832534533,6.38741669750803));
#19477=CARTESIAN_POINT('',(-38.522424122767,-35.0013091826171,6.11258330249198));
#19478=CARTESIAN_POINT('',(-38.5175,-35.,4.));
#19479=CARTESIAN_POINT('Ctrl Pts',(-38.522424122767,-35.0013091826171,6.11258330249198));
#19480=CARTESIAN_POINT('Ctrl Pts',(-38.5172132511134,-33.9256163607463,
6.06372381478986));
#19481=CARTESIAN_POINT('Ctrl Pts',(-37.9876405112709,-32.8454778142804,
6.01486432708775));
#19482=CARTESIAN_POINT('Ctrl Pts',(-37.1315953638235,-32.1949561890823,
5.96600483938563));
#19483=CARTESIAN_POINT('Ctrl Pts',(-36.2146857829733,-31.4981827625019,
5.91367146360154));
#19484=CARTESIAN_POINT('Ctrl Pts',(-34.9232293392347,-31.2942891822923,
5.86133808781746));
#19485=CARTESIAN_POINT('Ctrl Pts',(-33.8362565743057,-31.6746922887769,
5.80900471203338));
#19486=CARTESIAN_POINT('Ctrl Pts',(-32.7492838093767,-32.0550953952615,
5.75667133624929));
#19487=CARTESIAN_POINT('Ctrl Pts',(-31.8667947232573,-33.0197951884404,
5.7043379604652));
#19488=CARTESIAN_POINT('Ctrl Pts',(-31.5844576051196,-34.1362638014206,
5.65200458468112));
#19489=CARTESIAN_POINT('Ctrl Pts',(-31.302120486982,-35.2527324144008,5.59967120889704));
#19490=CARTESIAN_POINT('Ctrl Pts',(-31.6199353368261,-36.5209698471824,
5.54733783311296));
#19491=CARTESIAN_POINT('Ctrl Pts',(-32.3954083053537,-37.3723558065856,
5.49500445732887));
#19492=CARTESIAN_POINT('Ctrl Pts',(-33.1708812738812,-38.2237417659887,
5.44267108154479));
#19493=CARTESIAN_POINT('Ctrl Pts',(-34.4040123610921,-38.6582762520135,
5.3903377057607));
#19494=CARTESIAN_POINT('Ctrl Pts',(-35.5419213472807,-38.4811336220058,
5.33800432997661));
#19495=CARTESIAN_POINT('Ctrl Pts',(-36.6798303334694,-38.3039909919981,
5.28567095419253));
#19496=CARTESIAN_POINT('Ctrl Pts',(-37.722517218636,-37.515171245958,5.23333757840845));
#19497=CARTESIAN_POINT('Ctrl Pts',(-38.202488327186,-36.468345511481,5.18100420262436));
#19498=CARTESIAN_POINT('Ctrl Pts',(-38.4116604841668,-36.0121372252676,
5.15819723591357));
#19499=CARTESIAN_POINT('Ctrl Pts',(-38.5139599737744,-35.5069276682025,
5.13539026920277));
#19500=CARTESIAN_POINT('Ctrl Pts',(-38.5124574312326,-35.001138833141,5.11258330249198));
#19501=CARTESIAN_POINT('Ctrl Pts',(-38.5138068989996,-34.9977297535637,
5.38741669750802));
#19502=CARTESIAN_POINT('Ctrl Pts',(-38.5092952319858,-35.7405402881605,
5.42094378579333));
#19503=CARTESIAN_POINT('Ctrl Pts',(-38.2784660556449,-36.4859147377931,
5.45447087407864));
#19504=CARTESIAN_POINT('Ctrl Pts',(-37.8426354587898,-37.0811999269324,
5.48799796236395));
#19505=CARTESIAN_POINT('Ctrl Pts',(-37.1623352129312,-38.0103973340206,
5.54033133814803));
#19506=CARTESIAN_POINT('Ctrl Pts',(-35.982549686716,-38.5739027563021,5.59266471393212));
#19507=CARTESIAN_POINT('Ctrl Pts',(-34.8322413561292,-38.5190660643709,
5.6449980897162));
#19508=CARTESIAN_POINT('Ctrl Pts',(-33.6819330255423,-38.4642293724398,
5.69733146550029));
#19509=CARTESIAN_POINT('Ctrl Pts',(-32.5611018905839,-37.791050566296,5.74966484128437));
#19510=CARTESIAN_POINT('Ctrl Pts',(-31.9722780150789,-36.8013521300638,
5.80199821706845));
#19511=CARTESIAN_POINT('Ctrl Pts',(-31.3834541395739,-35.8116536938316,
5.85433159285254));
#19512=CARTESIAN_POINT('Ctrl Pts',(-31.3266375235224,-34.5054356275111,
5.90666496863662));
#19513=CARTESIAN_POINT('Ctrl Pts',(-31.8273020724053,-33.4683479988925,
5.95899834442071));
#19514=CARTESIAN_POINT('Ctrl Pts',(-32.3279666212882,-32.431260370274,6.01133172020479));
#19515=CARTESIAN_POINT('Ctrl Pts',(-33.3861123351056,-31.6633031793574,
6.06366509598888));
#19516=CARTESIAN_POINT('Ctrl Pts',(-34.5273147025013,-31.5087918386834,
6.11599847177296));
#19517=CARTESIAN_POINT('Ctrl Pts',(-35.668517069897,-31.3542804980094,6.16833184755705));
#19518=CARTESIAN_POINT('Ctrl Pts',(-36.892776090871,-31.8132150075779,6.22066522334113));
#19519=CARTESIAN_POINT('Ctrl Pts',(-37.6511889677791,-32.6798336612887,
6.27299859912521));
#19520=CARTESIAN_POINT('Ctrl Pts',(-38.2039029090244,-33.3114054953559,
6.31113796525282));
#19521=CARTESIAN_POINT('Ctrl Pts',(-38.509198477207,-34.1595049296877,6.34927733138042));
#19522=CARTESIAN_POINT('Ctrl Pts',(-38.5163032009778,-35.0029832534533,
6.38741669750803));
#19523=CARTESIAN_POINT('Origin',(-35.,-35.,4.));
#19524=CARTESIAN_POINT('',(-38.5217392653161,-34.9982348400382,7.38741669750802));
#19525=CARTESIAN_POINT('',(-38.5153122961063,-34.9971887940747,7.11258330249198));
#19526=CARTESIAN_POINT('',(-38.5175,-35.,4.));
#19527=CARTESIAN_POINT('',(-32.3264680662287,-32.7141668369925,8.));
#19528=CARTESIAN_POINT('Ctrl Pts',(-38.5217392653161,-34.9982348400382,
7.38741669750802));
#19529=CARTESIAN_POINT('Ctrl Pts',(-38.5150454835571,-36.0376021634142,
7.43461100431976));
#19530=CARTESIAN_POINT('Ctrl Pts',(-38.0253751592018,-37.0822329702746,
7.48180531113151));
#19531=CARTESIAN_POINT('Ctrl Pts',(-37.2186056743939,-37.7364863611315,
7.52899961794325));
#19532=CARTESIAN_POINT('Ctrl Pts',(-36.3239856773675,-38.4619825252834,
7.58133299372733));
#19533=CARTESIAN_POINT('Ctrl Pts',(-35.0394476042314,-38.7074546780583,
7.63366636951141));
#19534=CARTESIAN_POINT('Ctrl Pts',(-33.9411230034093,-38.3607385339716,
7.68599974529549));
#19535=CARTESIAN_POINT('Ctrl Pts',(-32.8427984025871,-38.0140223898848,
7.73833312107958));
#19536=CARTESIAN_POINT('Ctrl Pts',(-31.9306872740789,-37.0751179489365,
7.79066649686366));
#19537=CARTESIAN_POINT('Ctrl Pts',(-31.613697604643,-35.9699319523746,7.84299987264775));
#19538=CARTESIAN_POINT('Ctrl Pts',(-31.2967079352071,-34.8647459558128,
7.89533324843184));
#19539=CARTESIAN_POINT('Ctrl Pts',(-31.5748397248436,-33.5932784036375,
7.94766662421592));
#19540=CARTESIAN_POINT('Ctrl Pts',(-32.3264680662287,-32.7141668369925,
8.));
#19541=CARTESIAN_POINT('',(-37.6785009901498,-32.7109751557132,8.));
#19542=CARTESIAN_POINT('Origin',(-35.,-35.,8.));
#19543=CARTESIAN_POINT('Ctrl Pts',(-37.6785241456451,-32.7109602826759,
8.));
#19544=CARTESIAN_POINT('Ctrl Pts',(-36.9607513379489,-31.8766751051408,
7.95000212253756));
#19545=CARTESIAN_POINT('Ctrl Pts',(-35.8186699645707,-31.4010799150529,
7.90000424507511));
#19546=CARTESIAN_POINT('Ctrl Pts',(-34.7217021996619,-31.4881457455928,
7.85000636761267));
#19547=CARTESIAN_POINT('Ctrl Pts',(-33.573492932036,-31.5792785908026,7.79767299182859));
#19548=CARTESIAN_POINT('Ctrl Pts',(-32.4747104002448,-32.2868661727234,
7.7453396160445));
#19549=CARTESIAN_POINT('Ctrl Pts',(-31.9173292682424,-33.2944463949298,
7.69300624026042));
#19550=CARTESIAN_POINT('Ctrl Pts',(-31.3599481362399,-34.3020266171361,
7.64067286447633));
#19551=CARTESIAN_POINT('Ctrl Pts',(-31.3439684040262,-35.609599479628,7.58833948869224));
#19552=CARTESIAN_POINT('Ctrl Pts',(-31.8768867974267,-36.6305186264058,
7.53600611290816));
#19553=CARTESIAN_POINT('Ctrl Pts',(-32.4098051908272,-37.6514377731836,
7.48367273712407));
#19554=CARTESIAN_POINT('Ctrl Pts',(-33.491621709842,-38.3857032042473,7.43133936134));
#19555=CARTESIAN_POINT('Ctrl Pts',(-34.6371338873761,-38.5042968827328,
7.37900598555591));
#19556=CARTESIAN_POINT('Ctrl Pts',(-35.7826460649101,-38.6228905612183,
7.32667260977183));
#19557=CARTESIAN_POINT('Ctrl Pts',(-36.9918539009634,-38.1258124871256,
7.27433923398775));
#19558=CARTESIAN_POINT('Ctrl Pts',(-37.7226850841419,-37.2358340108349,
7.22200585820366));
#19559=CARTESIAN_POINT('Ctrl Pts',(-38.2320440076398,-36.615556046438,7.18553167296643));
#19560=CARTESIAN_POINT('Ctrl Pts',(-38.5090309960538,-35.8044263207662,
7.14905748772921));
#19561=CARTESIAN_POINT('Ctrl Pts',(-38.5153122961063,-34.9971887940747,
7.11258330249198));
#19562=CARTESIAN_POINT('Origin',(35.,-35.,4.));
#19563=CARTESIAN_POINT('',(31.4879726191333,-35.0001375015905,0.387416697508024));
#19564=CARTESIAN_POINT('',(31.4847993146864,-35.0046492582639,0.112583302491975));
#19565=CARTESIAN_POINT('',(31.4825,-35.,4.));
#19566=CARTESIAN_POINT('',(32.3264680662287,-32.7141668369925,0.));
#19567=CARTESIAN_POINT('Ctrl Pts',(31.4847993146864,-35.0046492582639,0.112583302491975));
#19568=CARTESIAN_POINT('Ctrl Pts',(31.4919760559448,-34.1767269622227,0.0750555349946493));
#19569=CARTESIAN_POINT('Ctrl Pts',(31.7874825103136,-33.3445694048179,0.037527767497323));
#19570=CARTESIAN_POINT('Ctrl Pts',(32.3264680662287,-32.7141668369925,-2.98372437868011E-15));
#19571=CARTESIAN_POINT('',(37.6785011129036,-32.7109752438421,-5.55678203018928E-16));
#19572=CARTESIAN_POINT('Origin',(35.,-35.,0.));
#19573=CARTESIAN_POINT('Ctrl Pts',(37.6785242770714,-32.7109603660127,-2.86292032689789E-16));
#19574=CARTESIAN_POINT('Ctrl Pts',(36.9607515035944,-31.8766753489742,0.0499978774624439));
#19575=CARTESIAN_POINT('Ctrl Pts',(35.8186700361932,-31.4010797162719,0.099995754924888));
#19576=CARTESIAN_POINT('Ctrl Pts',(34.7217021987141,-31.4881454554173,0.149993632387332));
#19577=CARTESIAN_POINT('Ctrl Pts',(33.5734928551282,-31.5792782049632,0.202327008171416));
#19578=CARTESIAN_POINT('Ctrl Pts',(32.4747102708807,-32.2868660760186,0.2546603839555));
#19579=CARTESIAN_POINT('Ctrl Pts',(31.9173291209027,-33.2944463985812,0.306993759739584));
#19580=CARTESIAN_POINT('Ctrl Pts',(31.6318119669108,-33.8105769963377,0.333801405662397));
#19581=CARTESIAN_POINT('Ctrl Pts',(31.488357249556,-34.4054248931928,0.360609051585211));
#19582=CARTESIAN_POINT('Ctrl Pts',(31.4879726191333,-35.0001375015905,0.387416697508024));
#19583=CARTESIAN_POINT('Origin',(35.,-35.,4.));
#19584=CARTESIAN_POINT('',(31.4787693262007,-35.0021519651487,1.38741669750802));
#19585=CARTESIAN_POINT('',(31.4779839561681,-34.998317589092,1.11258330249197));
#19586=CARTESIAN_POINT('',(31.4825,-35.,4.));
#19587=CARTESIAN_POINT('Ctrl Pts',(31.4779839561681,-34.998317589092,1.11258330249197));
#19588=CARTESIAN_POINT('Ctrl Pts',(31.4773939435915,-34.8986109589584,1.10805583214991));
#19589=CARTESIAN_POINT('Ctrl Pts',(31.4812696152992,-34.7989511654426,1.10352836180784));
#19590=CARTESIAN_POINT('Ctrl Pts',(31.4897615265674,-34.6996866782215,1.09900089146577));
#19591=CARTESIAN_POINT('Ctrl Pts',(31.5879201780762,-33.5522808822113,1.04666751568169));
#19592=CARTESIAN_POINT('Ctrl Pts',(32.3028649757287,-32.457692848996,0.994334139897601));
#19593=CARTESIAN_POINT('Ctrl Pts',(33.314059894657,-31.906560527472,0.942000764113516));
#19594=CARTESIAN_POINT('Ctrl Pts',(34.3252548135852,-31.3554282059481,0.889667388329432));
#19595=CARTESIAN_POINT('Ctrl Pts',(35.6326998537893,-31.3477515961155,0.837334012545348));
#19596=CARTESIAN_POINT('Ctrl Pts',(36.650169778933,-31.8872259747803,0.785000636761264));
#19597=CARTESIAN_POINT('Ctrl Pts',(37.6676397040767,-32.4267003534451,0.732667260977179));
#19598=CARTESIAN_POINT('Ctrl Pts',(38.39513451416,-33.5133257206073,0.680333885193094));
#19599=CARTESIAN_POINT('Ctrl Pts',(38.5065306720619,-34.6593978563341,0.628000509409009));
#19600=CARTESIAN_POINT('Ctrl Pts',(38.6179268299637,-35.8054699920609,0.575667133624925));
#19601=CARTESIAN_POINT('Ctrl Pts',(38.1132243356843,-37.0109888963523,0.523333757840841));
#19602=CARTESIAN_POINT('Ctrl Pts',(37.2186048923566,-37.7364852312874,0.471000382056757));
#19603=CARTESIAN_POINT('Ctrl Pts',(36.3239854490289,-38.4619815662224,0.418667006272672));
#19604=CARTESIAN_POINT('Ctrl Pts',(35.0394490566529,-38.7074553318012,0.366333630488587));
#19605=CARTESIAN_POINT('Ctrl Pts',(33.9411236515154,-38.3607384247595,0.314000254704503));
#19606=CARTESIAN_POINT('Ctrl Pts',(32.842798246378,-38.0140215177178,0.261666878920419));
#19607=CARTESIAN_POINT('Ctrl Pts',(31.930683828479,-37.0751139380558,0.209333503136335));
#19608=CARTESIAN_POINT('Ctrl Pts',(31.6136941980954,-35.9699281595357,0.157000127352251));
#19609=CARTESIAN_POINT('Ctrl Pts',(31.524014825647,-35.6572606223148,0.142194519065492));
#19610=CARTESIAN_POINT('Ctrl Pts',(31.4819679173789,-35.3312845479312,0.127388910778734));
#19611=CARTESIAN_POINT('Ctrl Pts',(31.4847993146864,-35.0046492582639,0.112583302491975));
#19612=CARTESIAN_POINT('Ctrl Pts',(31.4879726191333,-35.0001375015905,0.387416697508024));
#19613=CARTESIAN_POINT('Ctrl Pts',(31.4876063813705,-35.5664115202329,0.412942427369295));
#19614=CARTESIAN_POINT('Ctrl Pts',(31.6169544331328,-36.1325628797889,0.438468157230566));
#19615=CARTESIAN_POINT('Ctrl Pts',(31.8768866723687,-36.6305186540646,0.463993887091838));
#19616=CARTESIAN_POINT('Ctrl Pts',(32.4098050895213,-37.6514378129155,0.516327262875923));
#19617=CARTESIAN_POINT('Ctrl Pts',(33.491621639535,-38.3857033565476,0.568660638660007));
#19618=CARTESIAN_POINT('Ctrl Pts',(34.6371338646016,-38.5042970583454,0.620994014444092));
#19619=CARTESIAN_POINT('Ctrl Pts',(35.7826460896681,-38.6228907601432,0.673327390228177));
#19620=CARTESIAN_POINT('Ctrl Pts',(36.9918539897876,-38.1258126201067,0.725660766012261));
#19621=CARTESIAN_POINT('Ctrl Pts',(37.7226852066847,-37.235834095095,0.777994141796346));
#19622=CARTESIAN_POINT('Ctrl Pts',(38.4535164235819,-36.3458555700833,0.83032751758043));
#19623=CARTESIAN_POINT('Ctrl Pts',(38.7059709572567,-35.0629766600964,0.882660893364514));
#19624=CARTESIAN_POINT('Ctrl Pts',(38.3668190041959,-33.9624298822548,0.934994269148598));
#19625=CARTESIAN_POINT('Ctrl Pts',(38.027667051135,-32.8618831044132,0.987327644932683));
#19626=CARTESIAN_POINT('Ctrl Pts',(37.0969086113384,-31.9436684587171,1.03966102071677));
#19627=CARTESIAN_POINT('Ctrl Pts',(35.9918738484399,-31.6194482583158,1.09199439650085));
#19628=CARTESIAN_POINT('Ctrl Pts',(34.8868390855414,-31.2952280579146,1.14432777228494));
#19629=CARTESIAN_POINT('Ctrl Pts',(33.607527999541,-31.5650023028083,1.19666114806902));
#19630=CARTESIAN_POINT('Ctrl Pts',(32.7275158499642,-32.3078281435934,1.24899452385311));
#19631=CARTESIAN_POINT('Ctrl Pts',(31.9516362590269,-32.9627547940529,1.29513524840474));
#19632=CARTESIAN_POINT('Ctrl Pts',(31.4861479206373,-33.9854036295086,1.34127597295638));
#19633=CARTESIAN_POINT('Ctrl Pts',(31.4787693262007,-35.0021519651487,1.38741669750802));
#19634=CARTESIAN_POINT('Origin',(35.,-35.,4.));
#19635=CARTESIAN_POINT('',(31.4830375605149,-34.9969726960772,2.38741669750802));
#19636=CARTESIAN_POINT('',(31.4877390119671,-34.9992080277921,2.11258330249198));
#19637=CARTESIAN_POINT('',(31.4825,-35.,4.));
#19638=CARTESIAN_POINT('Ctrl Pts',(31.4877390119671,-34.9992080277921,2.11258330249198));
#19639=CARTESIAN_POINT('Ctrl Pts',(31.4866498159747,-34.4699801096587,2.08872275352108));
#19640=CARTESIAN_POINT('Ctrl Pts',(31.5990329357071,-33.9411914000592,2.06486220455019));
#19641=CARTESIAN_POINT('Ctrl Pts',(31.8273027226982,-33.4683483113999,2.04100165557929));
#19642=CARTESIAN_POINT('Ctrl Pts',(32.3279671691587,-32.431260896693,1.98866827979521));
#19643=CARTESIAN_POINT('Ctrl Pts',(33.3861126668897,-31.6633038687123,1.93633490401112));
#19644=CARTESIAN_POINT('Ctrl Pts',(34.5273147998293,-31.5087925573416,1.88400152822704));
#19645=CARTESIAN_POINT('Ctrl Pts',(35.6685169327689,-31.3542812459709,1.83166815244295));
#19646=CARTESIAN_POINT('Ctrl Pts',(36.892775700917,-31.8132156512101,1.77933477665887));
#19647=CARTESIAN_POINT('Ctrl Pts',(37.651188423337,-32.679834131615,1.72700140087478));
#19648=CARTESIAN_POINT('Ctrl Pts',(38.409601145757,-33.5464526120198,1.6746680250907));
#19649=CARTESIAN_POINT('Ctrl Pts',(38.7021678224488,-34.8207551675903,1.62233464930661));
#19650=CARTESIAN_POINT('Ctrl Pts',(38.3977155653522,-35.9313944817532,1.57000127352253));
#19651=CARTESIAN_POINT('Ctrl Pts',(38.0932633082556,-37.0420337959161,1.51766789773845));
#19652=CARTESIAN_POINT('Ctrl Pts',(37.1917921173706,-37.9890098686715,1.46533452195436));
#19653=CARTESIAN_POINT('Ctrl Pts',(36.0974793449018,-38.347756846785,1.41300114617028));
#19654=CARTESIAN_POINT('Ctrl Pts',(35.0031665724331,-38.7065038248986,1.36066777038619));
#19655=CARTESIAN_POINT('Ctrl Pts',(33.7160122183805,-38.4770217083703,1.30833439460211));
#19656=CARTESIAN_POINT('Ctrl Pts',(32.8131212940369,-37.7621688707036,1.25600101881802));
#19657=CARTESIAN_POINT('Ctrl Pts',(31.9883413614044,-37.10915945462,1.20819511337601));
#19658=CARTESIAN_POINT('Ctrl Pts',(31.4842139440677,-36.051127518694,1.16038920793399));
#19659=CARTESIAN_POINT('Ctrl Pts',(31.4779839561681,-34.998317589092,1.11258330249197));
#19660=CARTESIAN_POINT('Ctrl Pts',(31.4787693262007,-35.0021519651487,1.38741669750802));
#19661=CARTESIAN_POINT('Ctrl Pts',(31.4777790283158,-35.1386120640087,1.39360934874047));
#19662=CARTESIAN_POINT('Ctrl Pts',(31.4850406303498,-35.2749658775635,1.39980199997291));
#19663=CARTESIAN_POINT('Ctrl Pts',(31.5009112501032,-35.4103101518596,1.40599465120536));
#19664=CARTESIAN_POINT('Ctrl Pts',(31.6350320129721,-36.554088882664,1.45832802698944));
#19665=CARTESIAN_POINT('Ctrl Pts',(32.3839867518631,-37.6257689075961,1.51066140277353));
#19666=CARTESIAN_POINT('Ctrl Pts',(33.4119755528977,-38.1448602359127,1.56299477855761));
#19667=CARTESIAN_POINT('Ctrl Pts',(34.4399643539324,-38.6639515642293,1.6153281543417));
#19668=CARTESIAN_POINT('Ctrl Pts',(35.7469872171107,-38.6304541959304,1.66766153012578));
#19669=CARTESIAN_POINT('Ctrl Pts',(36.7470353952608,-38.0593854028254,1.71999490590987));
#19670=CARTESIAN_POINT('Ctrl Pts',(37.7470835734109,-37.4883166097203,1.77232828169395));
#19671=CARTESIAN_POINT('Ctrl Pts',(38.4401570665328,-36.3796763918093,1.82466165747804));
#19672=CARTESIAN_POINT('Ctrl Pts',(38.5155124424211,-35.2305296204218,1.87699503326212));
#19673=CARTESIAN_POINT('Ctrl Pts',(38.5908678183095,-34.0813828490343,1.9293284090462));
#19674=CARTESIAN_POINT('Ctrl Pts',(38.0485050769643,-32.8917295241703,1.98166178483029));
#19675=CARTESIAN_POINT('Ctrl Pts',(37.1315954563618,-32.1949560672859,2.03399516061437));
#19676=CARTESIAN_POINT('Ctrl Pts',(36.2146858357593,-31.4981826104015,2.08632853639846));
#19677=CARTESIAN_POINT('Ctrl Pts',(34.9232293358993,-31.2942890214966,2.13866191218254));
#19678=CARTESIAN_POINT('Ctrl Pts',(33.8362565237849,-31.6746921445243,2.19099528796663));
#19679=CARTESIAN_POINT('Ctrl Pts',(32.7492837116705,-32.055095267552,2.24332866375071));
#19680=CARTESIAN_POINT('Ctrl Pts',(31.8667945873017,-33.0197951025121,2.2956620395348));
#19681=CARTESIAN_POINT('Ctrl Pts',(31.5844574569229,-34.1362637639197,2.34799541531888));
#19682=CARTESIAN_POINT('Ctrl Pts',(31.5135652106755,-34.4165987349732,2.36113584271526));
#19683=CARTESIAN_POINT('Ctrl Pts',(31.4805104906949,-34.7065022103634,2.37427627011164));
#19684=CARTESIAN_POINT('Ctrl Pts',(31.4830375605149,-34.9969726960772,2.38741669750802));
#19685=CARTESIAN_POINT('Origin',(35.,-35.,4.));
#19686=CARTESIAN_POINT('',(31.486635086556,-35.0020090496756,3.38741669750802));
#19687=CARTESIAN_POINT('',(31.4804772106861,-35.0027703375482,3.11258330249198));
#19688=CARTESIAN_POINT('',(31.4825,-35.,4.));
#19689=CARTESIAN_POINT('Ctrl Pts',(31.4804772106861,-35.0027703375482,3.11258330249198));
#19690=CARTESIAN_POINT('Ctrl Pts',(31.4887009944635,-34.0497596813621,3.06938967489225));
#19691=CARTESIAN_POINT('Ctrl Pts',(31.8903812384068,-33.090636581221,3.02619604729253));
#19692=CARTESIAN_POINT('Ctrl Pts',(32.5815435480781,-32.4381583394347,2.98300241969281));
#19693=CARTESIAN_POINT('Ctrl Pts',(33.4189554277892,-31.647616055402,2.93066904390873));
#19694=CARTESIAN_POINT('Ctrl Pts',(34.6813192352892,-31.3072202195671,2.87833566812464));
#19695=CARTESIAN_POINT('Ctrl Pts',(35.8026481051029,-31.5695889094262,2.82600229234056));
#19696=CARTESIAN_POINT('Ctrl Pts',(36.9239769749167,-31.8319575992854,2.77366891655647));
#19697=CARTESIAN_POINT('Ctrl Pts',(37.904270907044,-32.6970908148387,2.72133554077239));
#19698=CARTESIAN_POINT('Ctrl Pts',(38.3040104089138,-33.7771019860347,2.66900216498831));
#19699=CARTESIAN_POINT('Ctrl Pts',(38.7037499107836,-34.8571131572306,2.61666878920422));
#19700=CARTESIAN_POINT('Ctrl Pts',(38.5229349823959,-36.1520022840693,2.56433541342014));
#19701=CARTESIAN_POINT('Ctrl Pts',(37.8426348759932,-37.0811995004531,2.51200203763605));
#19702=CARTESIAN_POINT('Ctrl Pts',(37.1623347695905,-38.0103967168369,2.45966866185197));
#19703=CARTESIAN_POINT('Ctrl Pts',(35.9825494851727,-38.5739020227658,2.40733528606788));
#19704=CARTESIAN_POINT('Ctrl Pts',(34.832241390481,-38.5190653424433,2.3550019102838));
#19705=CARTESIAN_POINT('Ctrl Pts',(33.6819332957892,-38.4642286621207,2.30266853449971));
#19706=CARTESIAN_POINT('Ctrl Pts',(32.5611023908235,-37.7910499955468,2.25033515871563));
#19707=CARTESIAN_POINT('Ctrl Pts',(31.9722786359356,-36.8013517615434,2.19800178293155));
#19708=CARTESIAN_POINT('Ctrl Pts',(31.6519194665675,-36.2628902923203,2.16952895611836));
#19709=CARTESIAN_POINT('Ctrl Pts',(31.4890387510844,-35.6307364505496,2.14105612930517));
#19710=CARTESIAN_POINT('Ctrl Pts',(31.4877390119671,-34.9992080277921,2.11258330249198));
#19711=CARTESIAN_POINT('Ctrl Pts',(31.4830375605149,-34.9969726960772,2.38741669750802));
#19712=CARTESIAN_POINT('Ctrl Pts',(31.490574858507,-35.8633368112863,2.42660964589573));
#19713=CARTESIAN_POINT('Ctrl Pts',(31.8146493000371,-36.734745074899,2.46580259428343));
#19714=CARTESIAN_POINT('Ctrl Pts',(32.3954081923274,-37.3723559095391,2.50499554267113));
#19715=CARTESIAN_POINT('Ctrl Pts',(33.1708811944992,-38.223741905896,2.55732891845522));
#19716=CARTESIAN_POINT('Ctrl Pts',(34.4040123352312,-38.6582764107548,2.60966229423931));
#19717=CARTESIAN_POINT('Ctrl Pts',(35.5419213707996,-38.4811337730552,2.66199567002339));
#19718=CARTESIAN_POINT('Ctrl Pts',(36.679830406368,-38.3039911353557,2.71432904580747));
#19719=CARTESIAN_POINT('Ctrl Pts',(37.7225173367726,-37.5151713550979,2.76666242159156));
#19720=CARTESIAN_POINT('Ctrl Pts',(38.2024884661482,-36.4683455751991,2.81899579737564));
#19721=CARTESIAN_POINT('Ctrl Pts',(38.6824595955238,-35.4215197953004,2.87132917315972));
#19722=CARTESIAN_POINT('Ctrl Pts',(38.5997149238704,-34.1166880157607,2.92366254894381));
#19723=CARTESIAN_POINT('Ctrl Pts',(37.9913534261364,-33.1388778186484,2.97599592472789));
#19724=CARTESIAN_POINT('Ctrl Pts',(37.3829919284024,-32.161067621536,3.02832930051198));
#19725=CARTESIAN_POINT('Ctrl Pts',(36.2490136045879,-31.510279006851,3.08066267629606));
#19726=CARTESIAN_POINT('Ctrl Pts',(35.0978430733873,-31.4782961743034,3.13299605208015));
#19727=CARTESIAN_POINT('Ctrl Pts',(33.9466725421867,-31.4463133417559,3.18532942786423));
#19728=CARTESIAN_POINT('Ctrl Pts',(32.7783098036,-32.0331362913458,3.23766280364832));
#19729=CARTESIAN_POINT('Ctrl Pts',(32.116595896964,-32.975660137455,3.2899961794324));
#19730=CARTESIAN_POINT('Ctrl Pts',(31.7059942452997,-33.5605078247475,3.32246968545761));
#19731=CARTESIAN_POINT('Ctrl Pts',(31.4904704191383,-34.2823130120804,3.35494319148282));
#19732=CARTESIAN_POINT('Ctrl Pts',(31.486635086556,-35.0020090496756,3.38741669750802));
#19733=CARTESIAN_POINT('Origin',(35.,-35.,4.));
#19734=CARTESIAN_POINT('',(31.4769535111774,-35.000206350087,4.38741669750802));
#19735=CARTESIAN_POINT('',(31.481143567597,-34.9970948481792,4.11258330249198));
#19736=CARTESIAN_POINT('',(31.4825,-35.,4.));
#19737=CARTESIAN_POINT('Ctrl Pts',(31.481143567597,-34.9970948481792,4.11258330249198));
#19738=CARTESIAN_POINT('Ctrl Pts',(31.4791556658517,-34.7720820979161,4.10238997204751));
#19739=CARTESIAN_POINT('Ctrl Pts',(31.4989362834408,-34.5474172520071,4.09219664160305));
#19740=CARTESIAN_POINT('Ctrl Pts',(31.5417700421341,-34.3272371560843,4.08200331115859));
#19741=CARTESIAN_POINT('Ctrl Pts',(31.7616819935963,-33.1968148899876,4.0296699353745));
#19742=CARTESIAN_POINT('Ctrl Pts',(32.5892466030323,-32.1846051588847,3.97733655959042));
#19743=CARTESIAN_POINT('Ctrl Pts',(33.6534213081659,-31.7444370513165,3.92500318380633));
#19744=CARTESIAN_POINT('Ctrl Pts',(34.7175960132996,-31.3042689437483,3.87266980802225));
#19745=CARTESIAN_POINT('Ctrl Pts',(36.0183808141308,-31.4361424597148,3.82033643223816));
#19746=CARTESIAN_POINT('Ctrl Pts',(36.9725626056516,-32.0809314753194,3.76800305645408));
#19747=CARTESIAN_POINT('Ctrl Pts',(37.9267443971724,-32.7257204909241,3.71566968066999));
#19748=CARTESIAN_POINT('Ctrl Pts',(38.5343231793827,-33.883425006167,3.66333630488591));
#19749=CARTESIAN_POINT('Ctrl Pts',(38.5228880907758,-35.0349826492465,3.61100292910183));
#19750=CARTESIAN_POINT('Ctrl Pts',(38.5114530021688,-36.186540292326,3.55866955331774));
#19751=CARTESIAN_POINT('Ctrl Pts',(37.8810040427447,-37.3319510632421,3.50633617753366));
#19752=CARTESIAN_POINT('Ctrl Pts',(36.9142060277602,-37.9576645468416,3.45400280174957));
#19753=CARTESIAN_POINT('Ctrl Pts',(35.9474080127757,-38.5833780304411,3.40166942596549));
#19754=CARTESIAN_POINT('Ctrl Pts',(34.6442609422309,-38.6893942267241,3.3493360501814));
#19755=CARTESIAN_POINT('Ctrl Pts',(33.5890370557646,-38.2281802690192,3.29700267439732));
#19756=CARTESIAN_POINT('Ctrl Pts',(32.5338131692983,-37.7669663113142,3.24466929861323));
#19757=CARTESIAN_POINT('Ctrl Pts',(31.7265124669105,-36.7385221996213,3.19233592282915));
#19758=CARTESIAN_POINT('Ctrl Pts',(31.5290920916777,-35.6039557776596,3.14000254704507));
#19759=CARTESIAN_POINT('Ctrl Pts',(31.4946136639238,-35.4058097333848,3.1308627988607));
#19760=CARTESIAN_POINT('Ctrl Pts',(31.478737062497,-35.2044268757596,3.12172305067634));
#19761=CARTESIAN_POINT('Ctrl Pts',(31.4804772106861,-35.0027703375482,3.11258330249198));
#19762=CARTESIAN_POINT('Ctrl Pts',(31.486635086556,-35.0020090496756,3.38741669750802));
#19763=CARTESIAN_POINT('Ctrl Pts',(31.4842895065774,-35.4421546120773,3.4072765672669));
#19764=CARTESIAN_POINT('Ctrl Pts',(31.5611195851562,-35.8815113110096,3.42713643702578));
#19765=CARTESIAN_POINT('Ctrl Pts',(31.7209248424069,-36.2882690753391,3.44699630678465));
#19766=CARTESIAN_POINT('Ctrl Pts',(32.1420327691713,-37.3601294244856,3.49932968256874));
#19767=CARTESIAN_POINT('Ctrl Pts',(33.1393136973855,-38.2056253801502,3.55166305835282));
#19768=CARTESIAN_POINT('Ctrl Pts',(34.2656319394155,-38.4456747746043,3.60399643413691));
#19769=CARTESIAN_POINT('Ctrl Pts',(35.3919501814454,-38.6857241690583,3.65632980992099));
#19770=CARTESIAN_POINT('Ctrl Pts',(36.647305737291,-38.3203270023018,3.70866318570508));
#19771=CARTESIAN_POINT('Ctrl Pts',(37.4688539216907,-37.5133108469912,3.76099656148916));
#19772=CARTESIAN_POINT('Ctrl Pts',(38.2904021060904,-36.7062946916805,3.81332993727324));
#19773=CARTESIAN_POINT('Ctrl Pts',(38.6781429190441,-35.4576595478158,3.86566331305733));
#19774=CARTESIAN_POINT('Ctrl Pts',(38.4582309072122,-34.3272369713982,3.91799668884141));
#19775=CARTESIAN_POINT('Ctrl Pts',(38.2383188953802,-33.1968143949805,3.9703300646255));
#19776=CARTESIAN_POINT('Ctrl Pts',(37.4107540587627,-32.1846043860099,4.02266344040958));
#19777=CARTESIAN_POINT('Ctrl Pts',(36.346579061494,-31.744436157607,4.07499681619367));
#19778=CARTESIAN_POINT('Ctrl Pts',(35.2824040642253,-31.3042679292041,4.12733019197775));
#19779=CARTESIAN_POINT('Ctrl Pts',(33.9816189063054,-31.4361414813689,4.17966356776183));
#19780=CARTESIAN_POINT('Ctrl Pts',(33.0274368528446,-32.0809306739812,4.23199694354592));
#19781=CARTESIAN_POINT('Ctrl Pts',(32.0828596573675,-32.7192293770668,4.28380352819995));
#19782=CARTESIAN_POINT('Ctrl Pts',(31.477942827805,-33.8601696083914,4.33561011285399));
#19783=CARTESIAN_POINT('Ctrl Pts',(31.4769535111774,-35.000206350087,4.38741669750802));
#19784=CARTESIAN_POINT('Origin',(35.,-35.,4.));
#19785=CARTESIAN_POINT('',(31.4861928568261,-34.9977297533801,5.38741669750802));
#19786=CARTESIAN_POINT('',(31.4875433805768,-35.0011388328632,5.11258330249198));
#19787=CARTESIAN_POINT('',(31.4825,-35.,4.));
#19788=CARTESIAN_POINT('Ctrl Pts',(31.4875433805768,-35.0011388328632,5.11258330249198));
#19789=CARTESIAN_POINT('Ctrl Pts',(31.4894886053032,-34.3463334487764,5.08305689341869));
#19790=CARTESIAN_POINT('Ctrl Pts',(31.6654108801779,-33.6905571677388,5.0535304843454));
#19791=CARTESIAN_POINT('Ctrl Pts',(32.0086473950495,-33.1388783295694,5.02400407527211));
#19792=CARTESIAN_POINT('Ctrl Pts',(32.6170087257827,-32.1610684008923,4.97167069948802));
#19793=CARTESIAN_POINT('Ctrl Pts',(33.7509867382882,-31.5102799648413,4.91933732370394));
#19794=CARTESIAN_POINT('Ctrl Pts',(34.9021569534692,-31.478297141069,4.86700394791986));
#19795=CARTESIAN_POINT('Ctrl Pts',(36.0533271686501,-31.4463143172967,4.81467057213577));
#19796=CARTESIAN_POINT('Ctrl Pts',(37.2216895865065,-32.0331371058031,4.76233719635168));
#19797=CARTESIAN_POINT('Ctrl Pts',(37.8834033114917,-32.975660693175,4.7100038205676));
#19798=CARTESIAN_POINT('Ctrl Pts',(38.5451170364769,-33.9181842805469,4.65767044478351));
#19799=CARTESIAN_POINT('Ctrl Pts',(38.7001820685911,-35.2164086667843,4.60533706899943));
#19800=CARTESIAN_POINT('Ctrl Pts',(38.2790742574276,-36.2882687216848,4.55300369321535));
#19801=CARTESIAN_POINT('Ctrl Pts',(37.8579664462641,-37.3601287765853,4.50067031743126));
#19802=CARTESIAN_POINT('Ctrl Pts',(36.8606857918229,-38.205624500149,4.44833694164718));
#19803=CARTESIAN_POINT('Ctrl Pts',(35.7343678589879,-38.4456738287057,4.39600356586309));
#19804=CARTESIAN_POINT('Ctrl Pts',(34.6080499261528,-38.6857231572625,4.34367019007901));
#19805=CARTESIAN_POINT('Ctrl Pts',(33.3526947149239,-38.3203260908123,4.29133681429492));
#19806=CARTESIAN_POINT('Ctrl Pts',(32.5311467560536,-37.5133101570419,4.23900343851084));
#19807=CARTESIAN_POINT('Ctrl Pts',(31.8696173263776,-36.863482250293,4.19686339317122));
#19808=CARTESIAN_POINT('Ctrl Pts',(31.489361712798,-35.9273155988689,4.1547233478316));
#19809=CARTESIAN_POINT('Ctrl Pts',(31.481143567597,-34.9970948481792,4.11258330249198));
#19810=CARTESIAN_POINT('Ctrl Pts',(31.4769535111774,-35.000206350087,4.38741669750802));
#19811=CARTESIAN_POINT('Ctrl Pts',(31.47694345139,-35.0117987228996,4.38794348863807));
#19812=CARTESIAN_POINT('Ctrl Pts',(31.4769958357584,-35.0233910022943,4.38847027976812));
#19813=CARTESIAN_POINT('Ctrl Pts',(31.4771109421281,-35.034982658853,4.38899707089817));
#19814=CARTESIAN_POINT('Ctrl Pts',(31.4885460338743,-36.1865406180529,4.44133044668226));
#19815=CARTESIAN_POINT('Ctrl Pts',(32.1189951663686,-37.3319517033932,4.49366382246634));
#19816=CARTESIAN_POINT('Ctrl Pts',(33.0857934467562,-37.9576653587677,4.54599719825043));
#19817=CARTESIAN_POINT('Ctrl Pts',(34.0525917271438,-38.5833790141421,4.59833057403451));
#19818=CARTESIAN_POINT('Ctrl Pts',(35.3557391554246,-38.6893952395508,4.6506639498186));
#19819=CARTESIAN_POINT('Ctrl Pts',(36.4109633315695,-38.228181155224,4.70299732560268));
#19820=CARTESIAN_POINT('Ctrl Pts',(37.4661875077144,-37.7669670708972,4.75533070138676));
#19821=CARTESIAN_POINT('Ctrl Pts',(38.2734884317233,-36.738522676835,4.80766407717085));
#19822=CARTESIAN_POINT('Ctrl Pts',(38.47090886115,-35.6039559434342,4.85999745295493));
#19823=CARTESIAN_POINT('Ctrl Pts',(38.6683292905767,-34.4693892100334,4.91233082873902));
#19824=CARTESIAN_POINT('Ctrl Pts',(38.2558692254213,-33.2287001372941,4.9646642045231));
#19825=CARTESIAN_POINT('Ctrl Pts',(37.4184571158289,-32.4381576362056,5.01699758030719));
#19826=CARTESIAN_POINT('Ctrl Pts',(36.5810450062365,-31.6476151351171,5.06933095609127));
#19827=CARTESIAN_POINT('Ctrl Pts',(35.3186808522071,-31.3072192056794,5.12166433187536));
#19828=CARTESIAN_POINT('Ctrl Pts',(34.1973516745615,-31.5695879676355,5.17399770765944));
#19829=CARTESIAN_POINT('Ctrl Pts',(33.0760224969158,-31.8319567295916,5.22633108344352));
#19830=CARTESIAN_POINT('Ctrl Pts',(32.0957282956539,-32.6970901829416,5.27866445922761));
#19831=CARTESIAN_POINT('Ctrl Pts',(31.6959886840635,-33.7771016504831,5.33099783501169));
#19832=CARTESIAN_POINT('Ctrl Pts',(31.5523400478426,-34.1652097336376,5.34980412251047));
#19833=CARTESIAN_POINT('Ctrl Pts',(31.4836621356307,-34.5810663878724,5.36861041000924));
#19834=CARTESIAN_POINT('Ctrl Pts',(31.4861928568261,-34.9977297533801,5.38741669750802));
#19835=CARTESIAN_POINT('Origin',(35.,-35.,4.));
#19836=CARTESIAN_POINT('',(31.4836965554877,-35.0029832498286,6.38741669750802));
#19837=CARTESIAN_POINT('',(31.4775766908735,-35.0013091813966,6.11258330249198));
#19838=CARTESIAN_POINT('',(31.4825,-35.,4.));
#19839=CARTESIAN_POINT('Ctrl Pts',(31.4775766908735,-35.0013091813966,6.11258330249198));
#19840=CARTESIAN_POINT('Ctrl Pts',(31.4827875611424,-33.9256166077537,6.06372381478986));
#19841=CARTESIAN_POINT('Ctrl Pts',(32.0123601793055,-32.8454783123193,6.01486432708774));
#19842=CARTESIAN_POINT('Ctrl Pts',(32.8684051290729,-32.1949568378204,5.96600483938563));
#19843=CARTESIAN_POINT('Ctrl Pts',(33.7853144981881,-31.4981835726539,5.91367146360154));
#19844=CARTESIAN_POINT('Ctrl Pts',(35.0767706429996,-31.2942900387516,5.86133808781746));
#19845=CARTESIAN_POINT('Ctrl Pts',(36.1637431566001,-31.6746930571201,5.80900471203337));
#19846=CARTESIAN_POINT('Ctrl Pts',(37.2507156702007,-32.0550960754886,5.75667133624929));
#19847=CARTESIAN_POINT('Ctrl Pts',(38.1332045525903,-33.0197956461279,5.70433796046521));
#19848=CARTESIAN_POINT('Ctrl Pts',(38.4155416055276,-34.1362640011663,5.65200458468112));
#19849=CARTESIAN_POINT('Ctrl Pts',(38.6978786584649,-35.2527323562045,5.59967120889703));
#19850=CARTESIAN_POINT('Ctrl Pts',(38.3800638819499,-36.5209694956418,5.54733783311295));
#19851=CARTESIAN_POINT('Ctrl Pts',(37.6045910926243,-37.3723552582146,5.49500445732887));
#19852=CARTESIAN_POINT('Ctrl Pts',(36.8291183032988,-38.2237410207875,5.44267108154478));
#19853=CARTESIAN_POINT('Ctrl Pts',(35.5959875011627,-38.658275406496,5.3903377057607));
#19854=CARTESIAN_POINT('Ctrl Pts',(34.4580787779894,-38.4811328174583,5.33800432997662));
#19855=CARTESIAN_POINT('Ctrl Pts',(33.3201700548161,-38.3039902284206,5.28567095419253));
#19856=CARTESIAN_POINT('Ctrl Pts',(32.2774834106055,-37.5151706646368,5.23333757840844));
#19857=CARTESIAN_POINT('Ctrl Pts',(31.7975124129806,-36.4683451720932,5.18100420262436));
#19858=CARTESIAN_POINT('Ctrl Pts',(31.5883403043411,-36.0121369913148,5.15819723591357));
#19859=CARTESIAN_POINT('Ctrl Pts',(31.486040838379,-35.5069275510188,5.13539026920277));
#19860=CARTESIAN_POINT('Ctrl Pts',(31.4875433805768,-35.0011388328632,5.11258330249198));
#19861=CARTESIAN_POINT('Ctrl Pts',(31.4861928568261,-34.9977297533801,5.38741669750802));
#19862=CARTESIAN_POINT('Ctrl Pts',(31.4907045241579,-35.7405403395491,5.42094378579333));
#19863=CARTESIAN_POINT('Ctrl Pts',(31.7215337165433,-36.4859148409341,5.45447087407864));
#19864=CARTESIAN_POINT('Ctrl Pts',(32.1573643436795,-37.081200071482,5.48799796236395));
#19865=CARTESIAN_POINT('Ctrl Pts',(32.8376646368048,-38.0103975432063,5.54033133814803));
#19866=CARTESIAN_POINT('Ctrl Pts',(34.0174502449743,-38.5739030049216,5.59266471393212));
#19867=CARTESIAN_POINT('Ctrl Pts',(35.1677586555142,-38.5190663090568,5.6449980897162));
#19868=CARTESIAN_POINT('Ctrl Pts',(36.318067066054,-38.464229613192,5.69733146550028));
#19869=CARTESIAN_POINT('Ctrl Pts',(37.4388982789643,-37.7910507597469,5.74966484128437));
#19870=CARTESIAN_POINT('Ctrl Pts',(38.0277221953511,-36.8013522549706,5.80199821706845));
#19871=CARTESIAN_POINT('Ctrl Pts',(38.6165461117379,-35.8116537501943,5.85433159285254));
#19872=CARTESIAN_POINT('Ctrl Pts',(38.6733627316013,-34.5054355940866,5.90666496863662));
#19873=CARTESIAN_POINT('Ctrl Pts',(38.172698148003,-33.4683478929687,5.9589983444207));
#19874=CARTESIAN_POINT('Ctrl Pts',(37.6720335644046,-32.4312601918508,6.01133172020479));
#19875=CARTESIAN_POINT('Ctrl Pts',(36.6138877773445,-31.6633029457227,6.06366509598888));
#19876=CARTESIAN_POINT('Ctrl Pts',(35.4726853304849,-31.5087915951115,6.11599847177296));
#19877=CARTESIAN_POINT('Ctrl Pts',(34.3314828836252,-31.3542802445004,6.16833184755705));
#19878=CARTESIAN_POINT('Ctrl Pts',(33.107223776966,-31.8132147894062,6.22066522334113));
#19879=CARTESIAN_POINT('Ctrl Pts',(32.3488108476933,-32.6798335018657,6.27299859912521));
#19880=CARTESIAN_POINT('Ctrl Pts',(31.7960968682859,-33.3114053787477,6.31113796525282));
#19881=CARTESIAN_POINT('Ctrl Pts',(31.4908012796383,-34.1595048683285,6.34927733138042));
#19882=CARTESIAN_POINT('Ctrl Pts',(31.4836965554877,-35.0029832498286,6.38741669750802));
#19883=CARTESIAN_POINT('Origin',(35.,-35.,4.));
#19884=CARTESIAN_POINT('',(31.478260520576,-34.9982347527286,7.38741669750802));
#19885=CARTESIAN_POINT('',(31.4846885160394,-34.9971888045819,7.11258330249198));
#19886=CARTESIAN_POINT('',(31.4825,-35.,4.));
#19887=CARTESIAN_POINT('',(37.6735319337713,-32.7141668369925,8.));
#19888=CARTESIAN_POINT('Ctrl Pts',(31.478260520576,-34.9982347527286,7.38741669750802));
#19889=CARTESIAN_POINT('Ctrl Pts',(31.4849542237249,-36.0376022532878,7.43461100431976));
#19890=CARTESIAN_POINT('Ctrl Pts',(31.9746244075585,-37.0822334042073,7.4818053111315));
#19891=CARTESIAN_POINT('Ctrl Pts',(32.7813940610787,-37.7364867433061,7.52899961794324));
#19892=CARTESIAN_POINT('Ctrl Pts',(33.6760142451889,-38.4619828500639,7.58133299372733));
#19893=CARTESIAN_POINT('Ctrl Pts',(34.9605528856554,-38.7074544587316,7.63366636951141));
#19894=CARTESIAN_POINT('Ctrl Pts',(36.0588772142959,-38.3607385729207,7.6859997452955));
#19895=CARTESIAN_POINT('Ctrl Pts',(37.1572015429365,-38.0140226871098,7.73833312107958));
#19896=CARTESIAN_POINT('Ctrl Pts',(38.069311559751,-37.0751193068202,7.79066649686367));
#19897=CARTESIAN_POINT('Ctrl Pts',(38.386301242806,-35.9699332359521,7.84299987264775));
#19898=CARTESIAN_POINT('Ctrl Pts',(38.703290925861,-34.864747165084,7.89533324843183));
#19899=CARTESIAN_POINT('Ctrl Pts',(38.4251602751564,-33.5932784036374,7.94766662421592));
#19900=CARTESIAN_POINT('Ctrl Pts',(37.6735319337713,-32.7141668369925,8.));
#19901=CARTESIAN_POINT('',(32.3214996650065,-32.7109746768979,8.));
#19902=CARTESIAN_POINT('Origin',(35.,-35.,8.));
#19903=CARTESIAN_POINT('Ctrl Pts',(32.3214765561793,-32.7109598296518,8.));
#19904=CARTESIAN_POINT('Ctrl Pts',(33.0392495465109,-31.8766737967152,7.95000212253756));
#19905=CARTESIAN_POINT('Ctrl Pts',(34.181330417556,-31.4010809746138,7.90000424507511));
#19906=CARTESIAN_POINT('Ctrl Pts',(35.2782977952799,-31.4881472942925,7.85000636761267));
#19907=CARTESIAN_POINT('Ctrl Pts',(36.4265066576347,-31.5792806514897,7.79767299182859));
#19908=CARTESIAN_POINT('Ctrl Pts',(37.5252889103119,-32.2868666869212,7.74533961604451));
#19909=CARTESIAN_POINT('Ctrl Pts',(38.0826699468004,-33.2944463733222,7.69300624026042));
#19910=CARTESIAN_POINT('Ctrl Pts',(38.6400509832889,-34.302026059723,7.64067286447634));
#19911=CARTESIAN_POINT('Ctrl Pts',(38.6560308035887,-35.6095993970933,7.58833948869224));
#19912=CARTESIAN_POINT('Ctrl Pts',(38.1231125366528,-36.6305184803578,7.53600611290816));
#19913=CARTESIAN_POINT('Ctrl Pts',(37.5901942697169,-37.6514375636223,7.48367273712407));
#19914=CARTESIAN_POINT('Ctrl Pts',(36.5083779155453,-38.3857023927811,7.43133936133999));
#19915=CARTESIAN_POINT('Ctrl Pts',(35.3628659911708,-38.5042959466132,7.37900598555591));
#19916=CARTESIAN_POINT('Ctrl Pts',(34.2173540667963,-38.6228895004453,7.32667260977183));
#19917=CARTESIAN_POINT('Ctrl Pts',(33.0081465722189,-38.1258117789507,7.27433923398774));
#19918=CARTESIAN_POINT('Ctrl Pts',(32.2773155686706,-37.2358335624551,7.22200585820366));
#19919=CARTESIAN_POINT('Ctrl Pts',(31.7679567703675,-36.6155557791246,7.18553167296643));
#19920=CARTESIAN_POINT('Ctrl Pts',(31.4909698285316,-35.80442618944,7.1490574877292));
#19921=CARTESIAN_POINT('Ctrl Pts',(31.4846885160394,-34.9971888045819,7.11258330249198));
#19922=CARTESIAN_POINT('Origin',(-35.,35.,10.2084234471775));
#19923=CARTESIAN_POINT('',(-39.0787305107814,35.0019482814736,0.791576552822544));
#19924=CARTESIAN_POINT('',(-39.0671617292797,34.9998409589035,0.708423447177453));
#19925=CARTESIAN_POINT('',(-39.0735,35.0000000000001,10.2084234471775));
#19926=CARTESIAN_POINT('',(-33.9479286229388,31.0647048309474,0.));
#19927=CARTESIAN_POINT('Ctrl Pts',(-39.0671617292797,34.9998409589035,0.708423447177453));
#19928=CARTESIAN_POINT('Ctrl Pts',(-39.0667162804106,35.6885579272407,0.68161580125464));
#19929=CARTESIAN_POINT('Ctrl Pts',(-38.5762700272017,37.7222374436051,0.602474779547742));
#19930=CARTESIAN_POINT('Ctrl Pts',(-35.379526836985,39.7808556694562,0.471000382056761));
#19931=CARTESIAN_POINT('Ctrl Pts',(-31.2187001848465,37.9557862959725,0.314000254704507));
#19932=CARTESIAN_POINT('Ctrl Pts',(-30.4549372314006,33.4726351387477,0.157000127352253));
#19933=CARTESIAN_POINT('Ctrl Pts',(-32.6539236935135,31.4106472544613,0.0523333757840845));
#19934=CARTESIAN_POINT('Ctrl Pts',(-33.9479286229388,31.0647048309474,0.));
#19935=CARTESIAN_POINT('',(-36.0547197101746,31.058399207452,2.73005324693302E-15));
#19936=CARTESIAN_POINT('Origin',(-35.,35.,0.));
#19937=CARTESIAN_POINT('Ctrl Pts',(-39.0787305107814,35.0019482814736,0.791576552822544));
#19938=CARTESIAN_POINT('Ctrl Pts',(-39.0794137856881,35.117415240318,0.787049082480477));
#19939=CARTESIAN_POINT('Ctrl Pts',(-39.0230450544057,36.5668924114048,0.730188236354325));
#19940=CARTESIAN_POINT('Ctrl Pts',(-37.2955092110801,39.2117686241983,0.620994014444089));
#19941=CARTESIAN_POINT('Ctrl Pts',(-32.7531819533668,39.2384377406302,0.463993887091835));
#19942=CARTESIAN_POINT('Ctrl Pts',(-30.2257196451616,35.46328448449,0.306993759739582));
#19943=CARTESIAN_POINT('Ctrl Pts',(-31.9530720002325,31.3373697401077,0.152329130708971));
#19944=CARTESIAN_POINT('Ctrl Pts',(-34.822442511108,30.7329994872565,0.0499978774624443));
#19945=CARTESIAN_POINT('Ctrl Pts',(-36.0547320440515,31.0583698407595,2.40774197454718E-15));
#19946=CARTESIAN_POINT('Origin',(-35.,35.,10.2084234471775));
#19947=CARTESIAN_POINT('',(-39.0674335213841,35.0009171557363,1.79157655282254));
#19948=CARTESIAN_POINT('',(-39.0778197532985,34.9975078784707,1.70842344717745));
#19949=CARTESIAN_POINT('',(-39.0735,35.0000000000001,10.2084234471775));
#19950=CARTESIAN_POINT('Ctrl Pts',(-39.0778197532985,34.9975078784707,1.70842344717745));
#19951=CARTESIAN_POINT('Ctrl Pts',(-39.0692748471557,36.1749702057365,1.66228272262582));
#19952=CARTESIAN_POINT('Ctrl Pts',(-37.9187924724061,38.702508200362,1.56380862229009));
#19953=CARTESIAN_POINT('Ctrl Pts',(-33.6495204180096,39.602789266723,1.41300114617028));
#19954=CARTESIAN_POINT('Ctrl Pts',(-30.4158794824773,36.4127281948833,1.25600101881803));
#19955=CARTESIAN_POINT('Ctrl Pts',(-31.2929570903083,31.9557501199225,1.09900089146578));
#19956=CARTESIAN_POINT('Ctrl Pts',(-35.4939869156159,30.2288018345407,0.942000764113521));
#19957=CARTESIAN_POINT('Ctrl Pts',(-38.6106822216958,32.3442076080298,0.811808282684081));
#19958=CARTESIAN_POINT('Ctrl Pts',(-39.0675858772087,34.3440577791618,0.733949177038725));
#19959=CARTESIAN_POINT('Ctrl Pts',(-39.0671617292797,34.9998409589035,0.708423447177453));
#19960=CARTESIAN_POINT('Ctrl Pts',(-39.0674335213841,35.0009171557363,1.79157655282255));
#19961=CARTESIAN_POINT('Ctrl Pts',(-39.0686948832473,35.6137985390812,1.76771600385165));
#19962=CARTESIAN_POINT('Ctrl Pts',(-38.6530957043657,37.569289309386,1.69152207909667));
#19963=CARTESIAN_POINT('Ctrl Pts',(-35.6435862778458,39.7534633517259,1.56299477855761));
#19964=CARTESIAN_POINT('Ctrl Pts',(-31.3902652615342,38.1590329639038,1.40599465120536));
#19965=CARTESIAN_POINT('Ctrl Pts',(-30.3738298371754,33.7318498284919,1.2489945238531));
#19966=CARTESIAN_POINT('Ctrl Pts',(-33.5057219097166,30.4418645346457,1.09199439650085));
#19967=CARTESIAN_POINT('Ctrl Pts',(-37.8485989831919,31.216140614721,0.939521739490665));
#19968=CARTESIAN_POINT('Ctrl Pts',(-39.0715157588091,33.7827238362241,0.839382458264561));
#19969=CARTESIAN_POINT('Ctrl Pts',(-39.0787305107814,35.0019482814736,0.791576552822544));
#19970=CARTESIAN_POINT('Origin',(-35.,35.,10.2084234471775));
#19971=CARTESIAN_POINT('',(-39.0758431739381,34.9967917635303,2.79157655282255));
#19972=CARTESIAN_POINT('',(-39.0728768523265,35.0035058195583,2.70842344717746));
#19973=CARTESIAN_POINT('',(-39.0735,35.0000000000001,10.2084234471775));
#19974=CARTESIAN_POINT('Ctrl Pts',(-39.0728768523265,35.0035058195583,2.70842344717746));
#19975=CARTESIAN_POINT('Ctrl Pts',(-39.075803367569,35.3398899970603,2.69528301978107));
#19976=CARTESIAN_POINT('Ctrl Pts',(-38.8850706886071,37.0126939576436,2.62980921660061));
#19977=CARTESIAN_POINT('Ctrl Pts',(-36.5844982252159,39.5275826001387,2.51200203763606));
#19978=CARTESIAN_POINT('Ctrl Pts',(-32.0977201830868,38.819215512031,2.3550019102838));
#19979=CARTESIAN_POINT('Ctrl Pts',(-30.2134435993119,34.6861220528707,2.19800178293155));
#19980=CARTESIAN_POINT('Ctrl Pts',(-32.6213194634248,30.8344843115421,2.04100165557929));
#19981=CARTESIAN_POINT('Ctrl Pts',(-37.1621781583154,30.7181077707172,1.88400152822704));
#19982=CARTESIAN_POINT('Ctrl Pts',(-38.9994901450348,33.3471191547144,1.77314212542643));
#19983=CARTESIAN_POINT('Ctrl Pts',(-39.0789665845212,34.8394779904932,1.7146160984099));
#19984=CARTESIAN_POINT('Ctrl Pts',(-39.0778197532985,34.9975078784707,1.70842344717745));
#19985=CARTESIAN_POINT('Ctrl Pts',(-39.0758431739381,34.9967917635303,2.79157655282255));
#19986=CARTESIAN_POINT('Ctrl Pts',(-39.0663194813852,36.100441948558,2.74838292522283));
#19987=CARTESIAN_POINT('Ctrl Pts',(-38.0375439399374,38.5569291706849,2.65285592183902));
#19988=CARTESIAN_POINT('Ctrl Pts',(-33.9071518161688,39.6706875589806,2.50499554267113));
#19989=CARTESIAN_POINT('Ctrl Pts',(-30.5014136769744,36.6650408935442,2.34799541531887));
#19990=CARTESIAN_POINT('Ctrl Pts',(-31.1296010783918,32.1663358219723,2.19099528796663));
#19991=CARTESIAN_POINT('Ctrl Pts',(-35.2284122688067,30.2086051339802,2.03399516061437));
#19992=CARTESIAN_POINT('Ctrl Pts',(-38.5306034134223,32.1919236036427,1.90085558223301));
#19993=CARTESIAN_POINT('Ctrl Pts',(-39.0659283364897,34.2695649347001,1.82004937963574));
#19994=CARTESIAN_POINT('Ctrl Pts',(-39.0674335213841,35.0009171557363,1.79157655282255));
#19995=CARTESIAN_POINT('Origin',(-35.,35.,10.2084234471775));
#19996=CARTESIAN_POINT('',(-39.0750714879939,35.0033643604342,3.79157655282255));
#19997=CARTESIAN_POINT('',(-39.0687106773974,34.997673386605,3.70842344717746));
#19998=CARTESIAN_POINT('',(-39.0735,35.0000000000001,10.2084234471775));
#19999=CARTESIAN_POINT('Ctrl Pts',(-39.0687106773974,34.997673386605,3.70842344717746));
#20000=CARTESIAN_POINT('Ctrl Pts',(-39.0642691067062,35.8311293539699,3.67594994115225));
#20001=CARTESIAN_POINT('Ctrl Pts',(-38.4124444982778,38.0141380355395,3.59114305934295));
#20002=CARTESIAN_POINT('Ctrl Pts',(-34.866781479659,39.7949860223284,3.45400280174958));
#20003=CARTESIAN_POINT('Ctrl Pts',(-30.9271141000824,37.5340162820022,3.29700267439732));
#20004=CARTESIAN_POINT('Ctrl Pts',(-30.6396425700269,33.0007698436185,3.14000254704507));
#20005=CARTESIAN_POINT('Ctrl Pts',(-34.2621453998186,30.2602522415144,2.98300241969281));
#20006=CARTESIAN_POINT('Ctrl Pts',(-38.1877198129624,31.6435581024348,2.83914271973695));
#20007=CARTESIAN_POINT('Ctrl Pts',(-39.064148159005,34.0001984453322,2.74761639556516));
#20008=CARTESIAN_POINT('Ctrl Pts',(-39.0728768523265,35.0035058195583,2.70842344717746));
#20009=CARTESIAN_POINT('Ctrl Pts',(-39.0750714879939,35.0033643604342,3.79157655282255));
#20010=CARTESIAN_POINT('Ctrl Pts',(-39.0773736113907,35.2639441995514,3.78138322237809));
#20011=CARTESIAN_POINT('Ctrl Pts',(-38.9368585171591,36.8598904257655,3.71885651614954));
#20012=CARTESIAN_POINT('Ctrl Pts',(-36.8334386787628,39.4326225179073,3.6039964341369));
#20013=CARTESIAN_POINT('Ctrl Pts',(-32.314250849668,38.9744674195804,3.44699630678465));
#20014=CARTESIAN_POINT('Ctrl Pts',(-30.2034000494222,34.9523692588031,3.2899961794324));
#20015=CARTESIAN_POINT('Ctrl Pts',(-32.3937064417451,30.9729820366429,3.13299605208014));
#20016=CARTESIAN_POINT('Ctrl Pts',(-36.9211012705904,30.6046604636344,2.97599592472789));
#20017=CARTESIAN_POINT('Ctrl Pts',(-38.9541946698804,33.1946779489209,2.86218942497536));
#20018=CARTESIAN_POINT('Ctrl Pts',(-39.0778583821194,34.7632599826793,2.80071630100691));
#20019=CARTESIAN_POINT('Ctrl Pts',(-39.0758431739381,34.9967917635303,2.79157655282255));
#20020=CARTESIAN_POINT('Origin',(-35.,35.,10.2084234471775));
#20021=CARTESIAN_POINT('',(-39.0676600758127,34.9986811552388,4.79157655282255));
#20022=CARTESIAN_POINT('',(-39.0799225868021,34.9997610328513,4.70842344717746));
#20023=CARTESIAN_POINT('',(-39.0735,35.0000000000001,10.2084234471775));
#20024=CARTESIAN_POINT('Ctrl Pts',(-39.0799225868021,34.9997610328513,4.70842344717746));
#20025=CARTESIAN_POINT('Ctrl Pts',(-39.0787768922257,36.3199995443189,4.65661686252342));
#20026=CARTESIAN_POINT('Ctrl Pts',(-37.6705855754179,38.9760045490164,4.5524769020853));
#20027=CARTESIAN_POINT('Ctrl Pts',(-33.1665613873943,39.4326223579625,4.3960035658631));
#20028=CARTESIAN_POINT('Ctrl Pts',(-30.2914357144823,35.9160024456566,4.23900343851084));
#20029=CARTESIAN_POINT('Ctrl Pts',(-31.6385248082081,31.5779943532675,4.08200331115859));
#20030=CARTESIAN_POINT('Ctrl Pts',(-35.9998809552364,30.3085315529294,3.92500318380634));
#20031=CARTESIAN_POINT('Ctrl Pts',(-38.7479935181635,32.6383846484188,3.80047656247929));
#20032=CARTESIAN_POINT('Ctrl Pts',(-39.0714270153063,34.4879554969268,3.72828331693633));
#20033=CARTESIAN_POINT('Ctrl Pts',(-39.0687106773974,34.997673386605,3.70842344717746));
#20034=CARTESIAN_POINT('Ctrl Pts',(-39.0676600758127,34.9986811552388,4.79157655282255));
#20035=CARTESIAN_POINT('Ctrl Pts',(-39.065407375266,35.756989657491,4.76205014374926));
#20036=CARTESIAN_POINT('Ctrl Pts',(-38.500581632009,37.8624610972284,4.68019035889188));
#20037=CARTESIAN_POINT('Ctrl Pts',(-35.1332185251462,39.7949861953461,4.54599719825043));
#20038=CARTESIAN_POINT('Ctrl Pts',(-31.0740926686951,37.7562458887763,4.38899707089817));
#20039=CARTESIAN_POINT('Ctrl Pts',(-30.5353655822401,33.2459534545604,4.23199694354592));
#20040=CARTESIAN_POINT('Ctrl Pts',(-34.0001190086845,30.3085313836444,4.07499681619366));
#20041=CARTESIAN_POINT('Ctrl Pts',(-38.0783115555367,31.4955735687615,3.92819001928588));
#20042=CARTESIAN_POINT('Ctrl Pts',(-39.0655543252915,33.9261064127185,3.83371659816217));
#20043=CARTESIAN_POINT('Ctrl Pts',(-39.0750714879939,35.0033643604342,3.79157655282255));
#20044=CARTESIAN_POINT('Origin',(-35.,35.,10.2084234471775));
#20045=CARTESIAN_POINT('',(-39.0792021698116,34.998483879503,5.79157655282255));
#20046=CARTESIAN_POINT('',(-39.0692228089002,35.0026290967949,5.70842344717746));
#20047=CARTESIAN_POINT('',(-39.0735,35.0000000000001,10.2084234471775));
#20048=CARTESIAN_POINT('Ctrl Pts',(-39.0692228089002,35.0026290967949,5.70842344717746));
#20049=CARTESIAN_POINT('Ctrl Pts',(-39.0721535526687,35.4851530378365,5.68961715967868));
#20050=CARTESIAN_POINT('Ctrl Pts',(-38.7712970745332,37.3068911247937,5.61847749639582));
#20051=CARTESIAN_POINT('Ctrl Pts',(-36.092848144401,39.6706873903976,5.49500445732886));
#20052=CARTESIAN_POINT('Ctrl Pts',(-31.7071427262397,38.4880838865661,5.33800432997662));
#20053=CARTESIAN_POINT('Ctrl Pts',(-30.2741740089879,34.1776820335287,5.18100420262436));
#20054=CARTESIAN_POINT('Ctrl Pts',(-33.0788987987297,30.6046606222411,5.02400407527212));
#20055=CARTESIAN_POINT('Ctrl Pts',(-37.6062934642105,30.9729821819491,4.86700394791985));
#20056=CARTESIAN_POINT('Ctrl Pts',(-39.073846927859,33.6392591565121,4.76181040522164));
#20057=CARTESIAN_POINT('Ctrl Pts',(-39.0799342367062,34.9863362926946,4.70895023830751));
#20058=CARTESIAN_POINT('Ctrl Pts',(-39.0799225868021,34.9997610328513,4.70842344717746));
#20059=CARTESIAN_POINT('Ctrl Pts',(-39.0792021698116,34.998483879503,5.79157655282255));
#20060=CARTESIAN_POINT('Ctrl Pts',(-39.0731676328035,36.2442079435004,5.74271706512043));
#20061=CARTESIAN_POINT('Ctrl Pts',(-37.8030025161425,38.8348894467969,5.64152420163423));
#20062=CARTESIAN_POINT('Ctrl Pts',(-33.4155017175264,39.5275827633586,5.48799796236395));
#20063=CARTESIAN_POINT('Ctrl Pts',(-30.3495579785441,36.176022571197,5.33099783501169));
#20064=CARTESIAN_POINT('Ctrl Pts',(-31.4537103860929,31.7699118586619,5.17399770765944));
#20065=CARTESIAN_POINT('Ctrl Pts',(-35.7378546268185,30.2602520705083,5.01699758030719));
#20066=CARTESIAN_POINT('Ctrl Pts',(-38.6790874120226,32.4853711659013,4.88952386202822));
#20067=CARTESIAN_POINT('Ctrl Pts',(-39.0694001203352,34.4129439352318,4.81438351953334));
#20068=CARTESIAN_POINT('Ctrl Pts',(-39.0676600758127,34.9986811552388,4.79157655282255));
#20069=CARTESIAN_POINT('Origin',(-35.,35.,10.2084234471775));
#20070=CARTESIAN_POINT('',(-39.070966199943,35.0032555604945,6.79157655282255));
#20071=CARTESIAN_POINT('',(-39.0721136942453,34.9965451882256,6.70842344717746));
#20072=CARTESIAN_POINT('',(-39.0735,35.0000000000001,10.2084234471775));
#20073=CARTESIAN_POINT('Ctrl Pts',(-39.0721136942453,34.9965451882256,6.70842344717746));
#20074=CARTESIAN_POINT('Ctrl Pts',(-39.0638859499781,35.9733493601025,6.67028408104985));
#20075=CARTESIAN_POINT('Ctrl Pts',(-38.2252019424137,38.3031815231405,6.57981133913817));
#20076=CARTESIAN_POINT('Ctrl Pts',(-34.3564137457339,39.7534631780217,6.4370052214424));
#20077=CARTESIAN_POINT('Ctrl Pts',(-30.6802037555765,37.0854262040492,6.28000509409013));
#20078=CARTESIAN_POINT('Ctrl Pts',(-30.8775960516807,32.5473632088007,6.12300496673789));
#20079=CARTESIAN_POINT('Ctrl Pts',(-34.7715877393978,30.2086053071985,5.96600483938563));
#20080=CARTESIAN_POINT('Ctrl Pts',(-38.3794219899756,31.9318288223888,5.82781099953215));
#20081=CARTESIAN_POINT('Ctrl Pts',(-39.0639979975134,34.142404941861,5.74195053546276));
#20082=CARTESIAN_POINT('Ctrl Pts',(-39.0692228089002,35.0026290967949,5.70842344717746));
#20083=CARTESIAN_POINT('Ctrl Pts',(-39.070966199943,35.0032555604945,6.79157655282255));
#20084=CARTESIAN_POINT('Ctrl Pts',(-39.0741290517156,35.409727295843,6.77571736227569));
#20085=CARTESIAN_POINT('Ctrl Pts',(-38.8328829256554,37.1538415310843,6.70752479594475));
#20086=CARTESIAN_POINT('Ctrl Pts',(-36.3504796357983,39.6027894460767,6.58699885382972));
#20087=CARTESIAN_POINT('Ctrl Pts',(-31.905897053523,38.6655398223873,6.42999872647746));
#20088=CARTESIAN_POINT('Ctrl Pts',(-30.2358031812474,34.4413383659989,6.27299859912522));
#20089=CARTESIAN_POINT('Ctrl Pts',(-32.8378217627235,30.7181076142107,6.11599847177296));
#20090=CARTESIAN_POINT('Ctrl Pts',(-37.3786806229274,30.8344841622903,5.95899834442071));
#20091=CARTESIAN_POINT('Ctrl Pts',(-39.0372095034026,33.4874666211437,5.85085770477057));
#20092=CARTESIAN_POINT('Ctrl Pts',(-39.0796312227382,34.9099134465561,5.79505044090451));
#20093=CARTESIAN_POINT('Ctrl Pts',(-39.0792021698116,34.998483879503,5.79157655282255));
#20094=CARTESIAN_POINT('Origin',(-35.,35.,10.2084234471775));
#20095=CARTESIAN_POINT('',(-39.0691248821302,34.9959228837483,7.79157655282255));
#20096=CARTESIAN_POINT('',(-39.0784090602678,35.0020440536087,7.70842344717746));
#20097=CARTESIAN_POINT('',(-39.0735,35.0000000000001,10.2084234471775));
#20098=CARTESIAN_POINT('',(-36.0520713770612,31.0647048309474,8.));
#20099=CARTESIAN_POINT('Ctrl Pts',(-36.0520713770612,31.0647048309474,8.));
#20100=CARTESIAN_POINT('Ctrl Pts',(-37.3460763064866,31.4106472544613,7.94766662421592));
#20101=CARTESIAN_POINT('Ctrl Pts',(-38.8056938328118,32.7793309690615,7.87819214182344));
#20102=CARTESIAN_POINT('Ctrl Pts',(-39.0721267560147,34.5563414191054,7.80871765943095));
#20103=CARTESIAN_POINT('Ctrl Pts',(-39.0691248821302,34.9959228837483,7.79157655282255));
#20104=CARTESIAN_POINT('',(-33.9452804362612,31.0583992034428,8.));
#20105=CARTESIAN_POINT('Origin',(-35.,35.,8.));
#20106=CARTESIAN_POINT('Ctrl Pts',(-33.9452681066883,31.058369845356,8.));
#20107=CARTESIAN_POINT('Ctrl Pts',(-35.1775577544271,30.7329993831125,7.95000212253756));
#20108=CARTESIAN_POINT('Ctrl Pts',(-37.9028280459028,31.3070187859893,7.85280993826337));
#20109=CARTESIAN_POINT('Ctrl Pts',(-39.0706571061612,33.7983874965128,7.7556177539892));
#20110=CARTESIAN_POINT('Ctrl Pts',(-39.0784090602678,35.0020440536087,7.70842344717747));
#20111=CARTESIAN_POINT('Origin',(35.,35.,10.2084234471775));
#20112=CARTESIAN_POINT('',(30.9212698233586,35.0019483146883,0.791576552822542));
#20113=CARTESIAN_POINT('',(30.9328374281389,34.9998406908479,0.708423447177449));
#20114=CARTESIAN_POINT('',(30.9265,35.0000000000001,10.2084234471775));
#20115=CARTESIAN_POINT('',(36.0520713770613,31.0647048309474,0.));
#20116=CARTESIAN_POINT('Ctrl Pts',(30.9328374281389,34.9998406908479,0.708423447177449));
#20117=CARTESIAN_POINT('Ctrl Pts',(30.9332828479214,35.688557610158,0.681615801254637));
#20118=CARTESIAN_POINT('Ctrl Pts',(31.423729103703,37.7222371568615,0.602474779547742));
#20119=CARTESIAN_POINT('Ctrl Pts',(34.620473026815,39.7808594262888,0.47100038205676));
#20120=CARTESIAN_POINT('Ctrl Pts',(38.7813013396977,37.9557820285754,0.314000254704507));
#20121=CARTESIAN_POINT('Ctrl Pts',(39.5450610063768,33.4726465453437,0.157000127352254));
#20122=CARTESIAN_POINT('Ctrl Pts',(37.3460763064866,31.4106472544613,0.0523333757840845));
#20123=CARTESIAN_POINT('Ctrl Pts',(36.0520713770613,31.0647048309474,0.));
#20124=CARTESIAN_POINT('',(33.9452806327216,31.0583991975554,1.9516645121422E-15));
#20125=CARTESIAN_POINT('Origin',(35.,35.,0.));
#20126=CARTESIAN_POINT('Ctrl Pts',(30.9212698233586,35.0019483146883,0.791576552822542));
#20127=CARTESIAN_POINT('Ctrl Pts',(30.9205865489415,35.1174152630019,0.787049082480475));
#20128=CARTESIAN_POINT('Ctrl Pts',(30.9769552830328,36.5668922956884,0.730188236354323));
#20129=CARTESIAN_POINT('Ctrl Pts',(32.7044910542971,39.2117680815463,0.620994014444087));
#20130=CARTESIAN_POINT('Ctrl Pts',(37.246817707304,39.2384377086451,0.463993887091833));
#20131=CARTESIAN_POINT('Ctrl Pts',(39.7742802645754,35.4632838929154,0.30699375973958));
#20132=CARTESIAN_POINT('Ctrl Pts',(38.0469271024438,31.3373709383794,0.152329130708969));
#20133=CARTESIAN_POINT('Ctrl Pts',(35.1775581103468,30.7329992432291,0.0499978774624438));
#20134=CARTESIAN_POINT('Ctrl Pts',(33.9452683089267,31.0583698510224,2.42915496745377E-15));
#20135=CARTESIAN_POINT('Origin',(35.,35.,10.2084234471775));
#20136=CARTESIAN_POINT('',(30.9325668217157,35.0009171562606,1.79157655282254));
#20137=CARTESIAN_POINT('',(30.9221793985577,34.9975078813789,1.70842344717745));
#20138=CARTESIAN_POINT('',(30.9265,35.0000000000001,10.2084234471775));
#20139=CARTESIAN_POINT('Ctrl Pts',(30.9221793985577,34.9975078813789,1.70842344717745));
#20140=CARTESIAN_POINT('Ctrl Pts',(30.9307243035611,36.174970446985,1.66228272262581));
#20141=CARTESIAN_POINT('Ctrl Pts',(32.0812069040633,38.7025089358584,1.56380862229009));
#20142=CARTESIAN_POINT('Ctrl Pts',(36.3504798927025,39.6027903023767,1.41300114617028));
#20143=CARTESIAN_POINT('Ctrl Pts',(39.5841214241815,36.41272834745,1.25600101881803));
#20144=CARTESIAN_POINT('Ctrl Pts',(38.7070437601939,31.9557497473198,1.09900089146578));
#20145=CARTESIAN_POINT('Ctrl Pts',(34.5060128656572,30.2288003607244,0.942000764113522));
#20146=CARTESIAN_POINT('Ctrl Pts',(31.3893171307454,32.344207693053,0.811808282684079));
#20147=CARTESIAN_POINT('Ctrl Pts',(30.9324133079056,34.3440575577889,0.733949177038721));
#20148=CARTESIAN_POINT('Ctrl Pts',(30.9328374281389,34.9998406908479,0.708423447177449));
#20149=CARTESIAN_POINT('Ctrl Pts',(30.9325668217157,35.0009171562606,1.79157655282254));
#20150=CARTESIAN_POINT('Ctrl Pts',(30.9313054599248,35.6137984881563,1.76771600385165));
#20151=CARTESIAN_POINT('Ctrl Pts',(31.3469046036967,37.5692890939049,1.69152207909667));
#20152=CARTESIAN_POINT('Ctrl Pts',(34.3564137772933,39.7534629455386,1.56299477855761));
#20153=CARTESIAN_POINT('Ctrl Pts',(38.6097344321268,38.159032706872,1.40599465120535));
#20154=CARTESIAN_POINT('Ctrl Pts',(39.6261697761982,33.7318499178854,1.2489945238531));
#20155=CARTESIAN_POINT('Ctrl Pts',(36.4942779564007,30.441864951573,1.09199439650085));
#20156=CARTESIAN_POINT('Ctrl Pts',(32.1514012728307,31.2161408778184,0.939521739490661));
#20157=CARTESIAN_POINT('Ctrl Pts',(30.9284845701608,33.7827239806345,0.839382458264559));
#20158=CARTESIAN_POINT('Ctrl Pts',(30.9212698233586,35.0019483146883,0.791576552822542));
#20159=CARTESIAN_POINT('Origin',(35.,35.,10.2084234471775));
#20160=CARTESIAN_POINT('',(30.9241571699662,34.9967917637985,2.79157655282254));
#20161=CARTESIAN_POINT('',(30.9271222988705,35.0035058204319,2.70842344717745));
#20162=CARTESIAN_POINT('',(30.9265,35.0000000000001,10.2084234471775));
#20163=CARTESIAN_POINT('Ctrl Pts',(30.9271222988705,35.0035058204319,2.70842344717745));
#20164=CARTESIAN_POINT('Ctrl Pts',(30.9241957830228,35.3398900680519,2.69528301978107));
#20165=CARTESIAN_POINT('Ctrl Pts',(31.1149285017256,37.0126943772598,2.62980921660061));
#20166=CARTESIAN_POINT('Ctrl Pts',(33.415501444059,39.52758354292,2.51200203763605));
#20167=CARTESIAN_POINT('Ctrl Pts',(37.902280422705,38.8192163097165,2.3550019102838));
#20168=CARTESIAN_POINT('Ctrl Pts',(39.7865573966804,34.6861219842625,2.19800178293155));
#20169=CARTESIAN_POINT('Ctrl Pts',(37.3786810353442,30.8344834494167,2.0410016555793));
#20170=CARTESIAN_POINT('Ctrl Pts',(32.8378213856151,30.7181068667712,1.88400152822704));
#20171=CARTESIAN_POINT('Ctrl Pts',(31.0005090266209,33.347118822167,1.77314212542643));
#20172=CARTESIAN_POINT('Ctrl Pts',(30.9210325674879,34.839477961413,1.7146160984099));
#20173=CARTESIAN_POINT('Ctrl Pts',(30.9221793985577,34.9975078813789,1.70842344717745));
#20174=CARTESIAN_POINT('Ctrl Pts',(30.9241571699662,34.9967917637985,2.79157655282254));
#20175=CARTESIAN_POINT('Ctrl Pts',(30.9336808617147,36.100441855715,2.74838292522282));
#20176=CARTESIAN_POINT('Ctrl Pts',(31.9624563163556,38.5569288706128,2.65285592183902));
#20177=CARTESIAN_POINT('Ctrl Pts',(36.0928480916297,39.6706871647746,2.50499554267113));
#20178=CARTESIAN_POINT('Ctrl Pts',(39.4985859434327,36.6650407532663,2.34799541531887));
#20179=CARTESIAN_POINT('Ctrl Pts',(38.8703985950797,32.1663360606625,2.19099528796662));
#20180=CARTESIAN_POINT('Ctrl Pts',(34.7715877503781,30.208605539026,2.03399516061437));
#20181=CARTESIAN_POINT('Ctrl Pts',(31.4693968846214,32.1919238394657,1.90085558223301));
#20182=CARTESIAN_POINT('Ctrl Pts',(30.9340720065237,34.2695649966187,1.82004937963573));
#20183=CARTESIAN_POINT('Ctrl Pts',(30.9325668217157,35.0009171562606,1.79157655282254));
#20184=CARTESIAN_POINT('Origin',(35.,35.,10.2084234471775));
#20185=CARTESIAN_POINT('',(30.9249288558452,35.0033643601501,3.79157655282254));
#20186=CARTESIAN_POINT('',(30.9312884745882,34.9976733861211,3.70842344717745));
#20187=CARTESIAN_POINT('',(30.9265,35.0000000000001,10.2084234471775));
#20188=CARTESIAN_POINT('Ctrl Pts',(30.9312884745882,34.9976733861211,3.70842344717745));
#20189=CARTESIAN_POINT('Ctrl Pts',(30.935730046206,35.8311295271992,3.67594994115225));
#20190=CARTESIAN_POINT('Ctrl Pts',(31.587554790492,38.0141386637623,3.59114305934295));
#20191=CARTESIAN_POINT('Ctrl Pts',(35.1332185480963,39.7949870216991,3.45400280174957));
#20192=CARTESIAN_POINT('Ctrl Pts',(39.0728867488228,37.5340168101838,3.29700267439732));
#20193=CARTESIAN_POINT('Ctrl Pts',(39.360358338736,33.0007694268683,3.14000254704507));
#20194=CARTESIAN_POINT('Ctrl Pts',(35.7378547540399,30.2602512537625,2.98300241969282));
#20195=CARTESIAN_POINT('Ctrl Pts',(31.8122795225231,31.6435574026667,2.83914271973694));
#20196=CARTESIAN_POINT('Ctrl Pts',(30.9358509939969,34.0001982370698,2.74761639556516));
#20197=CARTESIAN_POINT('Ctrl Pts',(30.9271222988705,35.0035058204319,2.70842344717745));
#20198=CARTESIAN_POINT('Ctrl Pts',(30.9249288558452,35.0033643601501,3.79157655282255));
#20199=CARTESIAN_POINT('Ctrl Pts',(30.9226267326427,35.2639441772806,3.78138322237808));
#20200=CARTESIAN_POINT('Ctrl Pts',(31.0631418150181,36.8598902688347,3.71885651614953));
#20201=CARTESIAN_POINT('Ctrl Pts',(33.1665614759356,39.4326221439007,3.60399643413691));
#20202=CARTESIAN_POINT('Ctrl Pts',(37.6857489237188,38.9744670842276,3.44699630678464));
#20203=CARTESIAN_POINT('Ctrl Pts',(39.7965995458586,34.9523692628263,3.2899961794324));
#20204=CARTESIAN_POINT('Ctrl Pts',(37.6062933383462,30.9729823764193,3.13299605208014));
#20205=CARTESIAN_POINT('Ctrl Pts',(33.078898891504,30.6046608345122,2.97599592472789));
#20206=CARTESIAN_POINT('Ctrl Pts',(31.0458056637607,33.1946781012295,2.86218942497536));
#20207=CARTESIAN_POINT('Ctrl Pts',(30.9221419619551,34.7632600026498,2.80071630100691));
#20208=CARTESIAN_POINT('Ctrl Pts',(30.9241571699662,34.9967917637985,2.79157655282254));
#20209=CARTESIAN_POINT('Origin',(35.,35.,10.2084234471775));
#20210=CARTESIAN_POINT('',(30.9323402673974,34.9986811553562,4.79157655282255));
#20211=CARTESIAN_POINT('',(30.920076562846,34.9997610327988,4.70842344717745));
#20212=CARTESIAN_POINT('',(30.9265,35.0000000000001,10.2084234471775));
#20213=CARTESIAN_POINT('Ctrl Pts',(30.920076562846,34.9997610327988,4.70842344717745));
#20214=CARTESIAN_POINT('Ctrl Pts',(30.9212222576611,36.3199998194329,4.65661686252342));
#20215=CARTESIAN_POINT('Ctrl Pts',(32.3294138679696,38.9760053777146,4.5524769020853));
#20216=CARTESIAN_POINT('Ctrl Pts',(36.833438994737,39.4326232818222,4.39600356586309));
#20217=CARTESIAN_POINT('Ctrl Pts',(39.7085652668935,35.9160026365752,4.23900343851085));
#20218=CARTESIAN_POINT('Ctrl Pts',(38.3614758924016,31.5779936400392,4.08200331115859));
#20219=CARTESIAN_POINT('Ctrl Pts',(34.0001188363665,30.3085305751198,3.92500318380634));
#20220=CARTESIAN_POINT('Ctrl Pts',(31.2520057006646,32.6383841561994,3.80047656247929));
#20221=CARTESIAN_POINT('Ctrl Pts',(30.9285721361126,34.4879553902047,3.72828331693633));
#20222=CARTESIAN_POINT('Ctrl Pts',(30.9312884745882,34.9976733861211,3.70842344717745));
#20223=CARTESIAN_POINT('Ctrl Pts',(30.9323402673974,34.9986811553562,4.79157655282255));
#20224=CARTESIAN_POINT('Ctrl Pts',(30.9345929677557,35.7569895936223,4.76205014374926));
#20225=CARTESIAN_POINT('Ctrl Pts',(31.4994186633631,37.8624608556942,4.68019035889188));
#20226=CARTESIAN_POINT('Ctrl Pts',(34.86678148609,39.7949857907703,4.54599719825042));
#20227=CARTESIAN_POINT('Ctrl Pts',(38.9259070000539,37.7562456562111,4.38899707089817));
#20228=CARTESIAN_POINT('Ctrl Pts',(39.4646340410498,33.2459536025622,4.23199694354592));
#20229=CARTESIAN_POINT('Ctrl Pts',(35.9998809069499,30.3085317794917,4.07499681619366));
#20230=CARTESIAN_POINT('Ctrl Pts',(31.9216887041993,31.4955738644524,3.92819001928588));
#20231=CARTESIAN_POINT('Ctrl Pts',(30.9344460177445,33.9261065033295,3.83371659816217));
#20232=CARTESIAN_POINT('Ctrl Pts',(30.9249288558452,35.0033643601501,3.79157655282255));
#20233=CARTESIAN_POINT('Origin',(35.,35.,10.2084234471775));
#20234=CARTESIAN_POINT('',(30.9207981741727,34.9984838800189,5.79157655282254));
#20235=CARTESIAN_POINT('',(30.93077634299,35.0026290974327,5.70842344717745));
#20236=CARTESIAN_POINT('',(30.9265,35.0000000000001,10.2084234471775));
#20237=CARTESIAN_POINT('Ctrl Pts',(30.93077634299,35.0026290974327,5.70842344717745));
#20238=CARTESIAN_POINT('Ctrl Pts',(30.9278455986019,35.4851531389532,5.68961715967867));
#20239=CARTESIAN_POINT('Ctrl Pts',(31.2287021394076,37.3068916052531,5.61847749639582));
#20240=CARTESIAN_POINT('Ctrl Pts',(33.9071516278456,39.6706883641509,5.49500445732887));
#20241=CARTESIAN_POINT('Ctrl Pts',(38.2928579600589,38.4880846134226,5.33800432997661));
#20242=CARTESIAN_POINT('Ctrl Pts',(39.72582697599,34.1776818622125,5.18100420262437));
#20243=CARTESIAN_POINT('Ctrl Pts',(36.9211016016709,30.6046597061106,5.0240040752721));
#20244=CARTESIAN_POINT('Ctrl Pts',(32.3937059925777,30.9729813426439,4.86700394791986));
#20245=CARTESIAN_POINT('Ctrl Pts',(30.9261522230555,33.6392588729013,4.76181040522164));
#20246=CARTESIAN_POINT('Ctrl Pts',(30.9200649129395,34.986336289844,4.7089502383075));
#20247=CARTESIAN_POINT('Ctrl Pts',(30.920076562846,34.9997610327988,4.70842344717745));
#20248=CARTESIAN_POINT('Ctrl Pts',(30.9207981741727,34.9984838800189,5.79157655282254));
#20249=CARTESIAN_POINT('Ctrl Pts',(30.9268327105953,36.2442078390725,5.74271706512043));
#20250=CARTESIAN_POINT('Ctrl Pts',(32.1969977207135,38.8348891225654,5.64152420163423));
#20251=CARTESIAN_POINT('Ctrl Pts',(36.5844981485848,39.5275823816942,5.48799796236394));
#20252=CARTESIAN_POINT('Ctrl Pts',(39.6504416291735,36.1760224717832,5.33099783501169));
#20253=CARTESIAN_POINT('Ctrl Pts',(38.5462893146292,31.7699121313011,5.17399770765944));
#20254=CARTESIAN_POINT('Ctrl Pts',(34.2621454354683,30.2602524703801,5.01699758030718));
#20255=CARTESIAN_POINT('Ctrl Pts',(31.3209128983978,32.4853713780877,4.88952386202822));
#20256=CARTESIAN_POINT('Ctrl Pts',(30.9306002230203,34.4129439847737,4.81438351953334));
#20257=CARTESIAN_POINT('Ctrl Pts',(30.9323402673974,34.9986811553562,4.79157655282255));
#20258=CARTESIAN_POINT('Origin',(35.,35.,10.2084234471775));
#20259=CARTESIAN_POINT('',(30.9290341434093,35.0032555560525,6.79157655282255));
#20260=CARTESIAN_POINT('',(30.9278854598697,34.9965452008231,6.70842344717745));
#20261=CARTESIAN_POINT('',(30.9265,35.0000000000001,10.2084234471775));
#20262=CARTESIAN_POINT('Ctrl Pts',(30.9278854598697,34.9965452008231,6.70842344717745));
#20263=CARTESIAN_POINT('Ctrl Pts',(30.9361132054557,35.973349573232,6.67028408104985));
#20264=CARTESIAN_POINT('Ctrl Pts',(31.7747973816342,38.3031821914714,6.57981133913817));
#20265=CARTESIAN_POINT('Ctrl Pts',(35.6435863904507,39.7534641813021,6.43700522144238));
#20266=CARTESIAN_POINT('Ctrl Pts',(39.3197971438036,37.085426632005,6.28000509409014));
#20267=CARTESIAN_POINT('Ctrl Pts',(39.122404807981,32.5473627011697,6.12300496673788));
#20268=CARTESIAN_POINT('Ctrl Pts',(35.2284123079944,30.2086043066787,5.96600483938564));
#20269=CARTESIAN_POINT('Ctrl Pts',(31.6205773057362,31.9318281835565,5.82781099953215));
#20270=CARTESIAN_POINT('Ctrl Pts',(30.9360011554815,34.1424047633691,5.74195053546276));
#20271=CARTESIAN_POINT('Ctrl Pts',(30.93077634299,35.0026290974327,5.70842344717745));
#20272=CARTESIAN_POINT('Ctrl Pts',(30.9290341434093,35.0032555560525,6.79157655282255));
#20273=CARTESIAN_POINT('Ctrl Pts',(30.9258712893501,35.4097272653281,6.77571736227569));
#20274=CARTESIAN_POINT('Ctrl Pts',(31.167117385295,37.1538413864501,6.70752479594475));
#20275=CARTESIAN_POINT('Ctrl Pts',(33.6495204900336,39.6027890266495,6.58699885382972));
#20276=CARTESIAN_POINT('Ctrl Pts',(38.0941026784935,38.6655395297167,6.42999872647747));
#20277=CARTESIAN_POINT('Ctrl Pts',(39.7641964207046,34.4413384042963,6.27299859912521));
#20278=CARTESIAN_POINT('Ctrl Pts',(37.1621780526355,30.7181079801836,6.11599847177296));
#20279=CARTESIAN_POINT('Ctrl Pts',(32.6213195789955,30.8344845112897,5.95899834442071));
#20280=CARTESIAN_POINT('Ctrl Pts',(30.9627908371619,33.4874667488915,5.85085770477057));
#20281=CARTESIAN_POINT('Ctrl Pts',(30.9203691212877,34.9099134545334,5.79505044090451));
#20282=CARTESIAN_POINT('Ctrl Pts',(30.9207981741727,34.9984838800189,5.79157655282254));
#20283=CARTESIAN_POINT('Origin',(35.,35.,10.2084234471775));
#20284=CARTESIAN_POINT('',(30.9308749498806,34.995920959377,7.79157655282255));
#20285=CARTESIAN_POINT('',(30.9215901961247,35.0020443570103,7.70842344717745));
#20286=CARTESIAN_POINT('',(30.9265,35.0000000000001,10.2084234471775));
#20287=CARTESIAN_POINT('',(33.9479286229388,31.0647048309474,8.));
#20288=CARTESIAN_POINT('Ctrl Pts',(33.9479286229388,31.0647048309474,8.));
#20289=CARTESIAN_POINT('Ctrl Pts',(32.6539236935135,31.4106472544613,7.94766662421592));
#20290=CARTESIAN_POINT('Ctrl Pts',(31.1943056926496,32.7793278989778,7.87819214182343));
#20291=CARTESIAN_POINT('Ctrl Pts',(30.927873001558,34.5563391849396,7.80871765943095));
#20292=CARTESIAN_POINT('Ctrl Pts',(30.9308749498806,34.995920959377,7.79157655282255));
#20293=CARTESIAN_POINT('',(36.0547204053665,31.0583992220146,8.));
#20294=CARTESIAN_POINT('Origin',(35.,35.,8.));
#20295=CARTESIAN_POINT('Ctrl Pts',(36.0547327596422,31.0583698145405,8.));
#20296=CARTESIAN_POINT('Ctrl Pts',(34.8224437745751,30.7329999802434,7.95000212253756));
#20297=CARTESIAN_POINT('Ctrl Pts',(32.0971699315749,31.3070160119469,7.85280993826337));
#20298=CARTESIAN_POINT('Ctrl Pts',(30.9293418770678,33.7983871843493,7.75561775398919));
#20299=CARTESIAN_POINT('Ctrl Pts',(30.9215901961247,35.0020443570103,7.70842344717745));
#20300=CARTESIAN_POINT('Origin',(-35.,-35.,10.2084234471775));
#20301=CARTESIAN_POINT('',(-39.0787307957508,-34.998051746757,0.791576552822544));
#20302=CARTESIAN_POINT('',(-39.0671620604938,-35.0001591466914,0.708423447177451));
#20303=CARTESIAN_POINT('',(-39.0735,-34.9999999999999,10.2084234471775));
#20304=CARTESIAN_POINT('',(-33.9479286229388,-38.9352951690526,0.));
#20305=CARTESIAN_POINT('Ctrl Pts',(-39.0671620604938,-35.0001591466914,
0.708423447177451));
#20306=CARTESIAN_POINT('Ctrl Pts',(-39.0667166230717,-34.3114421978074,
0.681615801254639));
#20307=CARTESIAN_POINT('Ctrl Pts',(-38.5762703689089,-32.2777626699106,
0.602474779547742));
#20308=CARTESIAN_POINT('Ctrl Pts',(-35.3795268907121,-30.2191428513895,
0.471000382056761));
#20309=CARTESIAN_POINT('Ctrl Pts',(-31.2186995847689,-32.0442153857854,
0.314000254704507));
#20310=CARTESIAN_POINT('Ctrl Pts',(-30.4549379250093,-36.5273603729133,
0.157000127352253));
#20311=CARTESIAN_POINT('Ctrl Pts',(-32.6539236935135,-38.5893527455387,
0.0523333757840845));
#20312=CARTESIAN_POINT('Ctrl Pts',(-33.9479286229388,-38.9352951690526,
0.));
#20313=CARTESIAN_POINT('',(-36.0547200012553,-38.9416007855471,4.26113251110999E-15));
#20314=CARTESIAN_POINT('Origin',(-35.,-35.,0.));
#20315=CARTESIAN_POINT('Ctrl Pts',(-39.0787307957508,-34.9980517467571,
0.791576552822544));
#20316=CARTESIAN_POINT('Ctrl Pts',(-39.0794140710738,-34.8825847789344,
0.787049082480477));
#20317=CARTESIAN_POINT('Ctrl Pts',(-39.0230453421645,-33.4331074898667,
0.730188236354326));
#20318=CARTESIAN_POINT('Ctrl Pts',(-37.2955094371433,-30.7882309135474,
0.620994014444089));
#20319=CARTESIAN_POINT('Ctrl Pts',(-32.7531816644513,-30.7615622313046,
0.463993887091836));
#20320=CARTESIAN_POINT('Ctrl Pts',(-30.2257195673566,-34.5367150123096,
0.306993759739581));
#20321=CARTESIAN_POINT('Ctrl Pts',(-31.9530712365814,-38.6626312798268,
0.152329130708972));
#20322=CARTESIAN_POINT('Ctrl Pts',(-34.8224430395506,-39.2670003060384,
0.0499978774624443));
#20323=CARTESIAN_POINT('Ctrl Pts',(-36.0547323436802,-38.9416301693299,
2.36437388764776E-15));
#20324=CARTESIAN_POINT('Origin',(-35.,-35.,10.2084234471775));
#20325=CARTESIAN_POINT('',(-39.0674338139571,-34.9990828447087,1.79157655282254));
#20326=CARTESIAN_POINT('',(-39.0778200867196,-35.0024921203811,1.70842344717745));
#20327=CARTESIAN_POINT('',(-39.0735,-34.9999999999999,10.2084234471775));
#20328=CARTESIAN_POINT('Ctrl Pts',(-39.0778200867196,-35.0024921203811,
1.70842344717745));
#20329=CARTESIAN_POINT('Ctrl Pts',(-39.0692751810275,-33.8250296994275,
1.66228272262581));
#20330=CARTESIAN_POINT('Ctrl Pts',(-37.9187927175433,-31.297491510544,1.56380862229009));
#20331=CARTESIAN_POINT('Ctrl Pts',(-33.6495202958365,-30.3972103260493,
1.41300114617028));
#20332=CARTESIAN_POINT('Ctrl Pts',(-30.4158791260905,-33.5872717453,1.25600101881803));
#20333=CARTESIAN_POINT('Ctrl Pts',(-31.2929567559004,-38.0442500262742,
1.09900089146578));
#20334=CARTESIAN_POINT('Ctrl Pts',(-35.4939870016774,-39.7711987453336,
0.942000764113521));
#20335=CARTESIAN_POINT('Ctrl Pts',(-38.6106824762136,-37.6557923579424,
0.81180828268408));
#20336=CARTESIAN_POINT('Ctrl Pts',(-39.0675861975231,-35.6559423079101,
0.733949177038723));
#20337=CARTESIAN_POINT('Ctrl Pts',(-39.0671620604938,-35.0001591466914,
0.708423447177451));
#20338=CARTESIAN_POINT('Ctrl Pts',(-39.0674338139571,-34.9990828447087,
1.79157655282254));
#20339=CARTESIAN_POINT('Ctrl Pts',(-39.0686951758822,-34.3862014174905,
1.76771600385165));
#20340=CARTESIAN_POINT('Ctrl Pts',(-38.6530959670617,-32.4307105068614,
1.69152207909667));
#20341=CARTESIAN_POINT('Ctrl Pts',(-35.6435863248602,-30.2465363019221,
1.56299477855761));
#20342=CARTESIAN_POINT('Ctrl Pts',(-31.3902650003177,-31.8409668168855,
1.40599465120536));
#20343=CARTESIAN_POINT('Ctrl Pts',(-30.3738295074692,-36.2681502477922,
1.2489945238531));
#20344=CARTESIAN_POINT('Ctrl Pts',(-33.5057217955833,-39.5581358207848,
1.09199439650085));
#20345=CARTESIAN_POINT('Ctrl Pts',(-37.8485992014502,-38.7838596097918,
0.939521739490664));
#20346=CARTESIAN_POINT('Ctrl Pts',(-39.0715160393823,-36.2172762868091,
0.839382458264562));
#20347=CARTESIAN_POINT('Ctrl Pts',(-39.0787307957508,-34.9980517467571,
0.791576552822544));
#20348=CARTESIAN_POINT('Origin',(-35.,-35.,10.2084234471775));
#20349=CARTESIAN_POINT('',(-39.0758434671966,-35.0032082366984,2.79157655282255));
#20350=CARTESIAN_POINT('',(-39.0728771860086,-34.996494180098,2.70842344717745));
#20351=CARTESIAN_POINT('',(-39.0735,-34.9999999999999,10.2084234471775));
#20352=CARTESIAN_POINT('Ctrl Pts',(-39.0728771860086,-34.996494180098,2.70842344717745));
#20353=CARTESIAN_POINT('Ctrl Pts',(-39.075803701489,-34.6601099750312,2.69528301978107));
#20354=CARTESIAN_POINT('Ctrl Pts',(-38.8850710069041,-32.9873058773963,
2.62980921660061));
#20355=CARTESIAN_POINT('Ctrl Pts',(-36.5844983552314,-30.4724170292356,
2.51200203763606));
#20356=CARTESIAN_POINT('Ctrl Pts',(-32.0977199449364,-31.1807841743797,
2.3550019102838));
#20357=CARTESIAN_POINT('Ctrl Pts',(-30.2134432077683,-35.3138779741053,
2.19800178293155));
#20358=CARTESIAN_POINT('Ctrl Pts',(-32.621319267345,-39.1655160273689,2.04100165557929));
#20359=CARTESIAN_POINT('Ctrl Pts',(-37.1621783376115,-39.2818925846584,
1.88400152822705));
#20360=CARTESIAN_POINT('Ctrl Pts',(-38.9994904706692,-36.6528809760016,
1.77314212542643));
#20361=CARTESIAN_POINT('Ctrl Pts',(-39.0789669178819,-35.1605220209328,
1.7146160984099));
#20362=CARTESIAN_POINT('Ctrl Pts',(-39.0778200867196,-35.0024921203811,
1.70842344717745));
#20363=CARTESIAN_POINT('Ctrl Pts',(-39.0758434671966,-35.0032082366984,
2.79157655282255));
#20364=CARTESIAN_POINT('Ctrl Pts',(-39.0663197739578,-33.8995579722718,
2.74838292522283));
#20365=CARTESIAN_POINT('Ctrl Pts',(-38.037544158487,-31.4430705734335,2.65285592183902));
#20366=CARTESIAN_POINT('Ctrl Pts',(-33.9071517375455,-30.3293121048675,
2.50499554267113));
#20367=CARTESIAN_POINT('Ctrl Pts',(-30.5014133532831,-33.3349589868354,
2.34799541531887));
#20368=CARTESIAN_POINT('Ctrl Pts',(-31.12960079995,-37.8336643815683,2.19099528796663));
#20369=CARTESIAN_POINT('Ctrl Pts',(-35.2284122851668,-39.7913952114128,
2.03399516061437));
#20370=CARTESIAN_POINT('Ctrl Pts',(-38.5306036675732,-37.8080765974554,
1.90085558223301));
#20371=CARTESIAN_POINT('Ctrl Pts',(-39.0659286289889,-35.7304351180991,
1.82004937963574));
#20372=CARTESIAN_POINT('Ctrl Pts',(-39.0674338139571,-34.9990828447087,
1.79157655282254));
#20373=CARTESIAN_POINT('Origin',(-35.,-35.,10.2084234471775));
#20374=CARTESIAN_POINT('',(-39.0750717811968,-34.9966356393236,3.79157655282255));
#20375=CARTESIAN_POINT('',(-39.0687110107696,-35.0023266135852,3.70842344717746));
#20376=CARTESIAN_POINT('',(-39.0735,-34.9999999999999,10.2084234471775));
#20377=CARTESIAN_POINT('Ctrl Pts',(-39.0687110107696,-35.0023266135852,
3.70842344717746));
#20378=CARTESIAN_POINT('Ctrl Pts',(-39.0642694397141,-34.16887057793,3.67594994115225));
#20379=CARTESIAN_POINT('Ctrl Pts',(-38.4124447778773,-31.9858617174929,
3.59114305934296));
#20380=CARTESIAN_POINT('Ctrl Pts',(-34.8667814687478,-30.2050135847982,
3.45400280174957));
#20381=CARTESIAN_POINT('Ctrl Pts',(-30.9271137663599,-32.4659835103585,
3.29700267439732));
#20382=CARTESIAN_POINT('Ctrl Pts',(-30.6396422127733,-36.9992303202149,
3.14000254704507));
#20383=CARTESIAN_POINT('Ctrl Pts',(-34.2621453393335,-39.7397481467912,
2.98300241969281));
#20384=CARTESIAN_POINT('Ctrl Pts',(-38.1877200741971,-38.356442172659,2.83914271973695));
#20385=CARTESIAN_POINT('Ctrl Pts',(-39.0641484919776,-35.9998016365399,
2.74761639556516));
#20386=CARTESIAN_POINT('Ctrl Pts',(-39.0728771860086,-34.996494180098,2.70842344717745));
#20387=CARTESIAN_POINT('Ctrl Pts',(-39.0750717811968,-34.9966356393236,
3.79157655282255));
#20388=CARTESIAN_POINT('Ctrl Pts',(-39.0773739047593,-34.7360557814575,
3.78138322237809));
#20389=CARTESIAN_POINT('Ctrl Pts',(-38.9368588004177,-33.1401094404144,
3.71885651614954));
#20390=CARTESIAN_POINT('Ctrl Pts',(-36.8334388106793,-30.5673771631648,
3.6039964341369));
#20391=CARTESIAN_POINT('Ctrl Pts',(-32.3142506564274,-31.0255322944533,
3.44699630678465));
#20392=CARTESIAN_POINT('Ctrl Pts',(-30.2033997043049,-35.0476307446275,
3.28999617943239));
#20393=CARTESIAN_POINT('Ctrl Pts',(-32.3937062542216,-39.0270182530956,
3.13299605208014));
#20394=CARTESIAN_POINT('Ctrl Pts',(-36.9211014088136,-39.3953398526252,
2.97599592472789));
#20395=CARTESIAN_POINT('Ctrl Pts',(-38.9541949543872,-36.8053221809578,
2.86218942497536));
#20396=CARTESIAN_POINT('Ctrl Pts',(-39.077858675523,-35.2367400343503,2.80071630100691));
#20397=CARTESIAN_POINT('Ctrl Pts',(-39.0758434671966,-35.0032082366984,
2.79157655282255));
#20398=CARTESIAN_POINT('Origin',(-35.,-35.,10.2084234471775));
#20399=CARTESIAN_POINT('',(-39.0676603684793,-35.0013188448613,4.79157655282255));
#20400=CARTESIAN_POINT('',(-39.0799229210932,-35.0002389671693,4.70842344717745));
#20401=CARTESIAN_POINT('',(-39.0735,-34.9999999999999,10.2084234471775));
#20402=CARTESIAN_POINT('Ctrl Pts',(-39.0799229210932,-35.0002389671693,
4.70842344717745));
#20403=CARTESIAN_POINT('Ctrl Pts',(-39.0787772264229,-33.680000347528,4.65661686252342));
#20404=CARTESIAN_POINT('Ctrl Pts',(-37.6705857942339,-31.023995125205,4.5524769020853));
#20405=CARTESIAN_POINT('Ctrl Pts',(-33.1665612371704,-30.5673772788489,
4.39600356586309));
#20406=CARTESIAN_POINT('Ctrl Pts',(-30.291435328683,-34.0839974792893,4.23900343851084));
#20407=CARTESIAN_POINT('Ctrl Pts',(-31.6385245327839,-38.4220059271175,
4.08200331115859));
#20408=CARTESIAN_POINT('Ctrl Pts',(-35.9998810371616,-39.6914688314679,
3.92500318380634));
#20409=CARTESIAN_POINT('Ctrl Pts',(-38.7479938252585,-37.361615545083,3.80047656247929));
#20410=CARTESIAN_POINT('Ctrl Pts',(-39.0714273489013,-35.5120445450279,
3.72828331693633));
#20411=CARTESIAN_POINT('Ctrl Pts',(-39.0687110107696,-35.0023266135852,
3.70842344717746));
#20412=CARTESIAN_POINT('Ctrl Pts',(-39.0676603684793,-35.0013188448613,
4.79157655282255));
#20413=CARTESIAN_POINT('Ctrl Pts',(-39.065407667772,-34.2430102880461,4.76205014374926));
#20414=CARTESIAN_POINT('Ctrl Pts',(-38.5005818838826,-32.1375386968076,
4.68019035889189));
#20415=CARTESIAN_POINT('Ctrl Pts',(-35.1332185347277,-30.2050134596587,
4.54599719825043));
#20416=CARTESIAN_POINT('Ctrl Pts',(-31.0740923862265,-32.2437539129077,
4.38899707089817));
#20417=CARTESIAN_POINT('Ctrl Pts',(-30.535365261007,-36.7540466716456,4.23199694354592));
#20418=CARTESIAN_POINT('Ctrl Pts',(-34.0001189367432,-39.6914689539076,
4.07499681619366));
#20419=CARTESIAN_POINT('Ctrl Pts',(-38.0783117770221,-38.5044266833838,
3.92819001928587));
#20420=CARTESIAN_POINT('Ctrl Pts',(-39.0655546178097,-36.0738936645484,
3.83371659816217));
#20421=CARTESIAN_POINT('Ctrl Pts',(-39.0750717811968,-34.9966356393236,
3.79157655282255));
#20422=CARTESIAN_POINT('Origin',(-35.,-35.,10.2084234471775));
#20423=CARTESIAN_POINT('',(-39.0792024631389,-35.0015161209354,5.79157655282255));
#20424=CARTESIAN_POINT('',(-39.0692231423099,-34.9973709029543,5.70842344717745));
#20425=CARTESIAN_POINT('',(-39.0735,-34.9999999999999,10.2084234471775));
#20426=CARTESIAN_POINT('Ctrl Pts',(-39.0692231423099,-34.9973709029543,
5.70842344717745));
#20427=CARTESIAN_POINT('Ctrl Pts',(-39.072153886322,-34.5148469224124,5.68961715967868));
#20428=CARTESIAN_POINT('Ctrl Pts',(-38.7712973835496,-32.6931086863282,
5.61847749639582));
#20429=CARTESIAN_POINT('Ctrl Pts',(-36.0928482339355,-30.3293122267992,
5.49500445732888));
#20430=CARTESIAN_POINT('Ctrl Pts',(-31.7071424564414,-31.5119158276916,
5.33800432997661));
#20431=CARTESIAN_POINT('Ctrl Pts',(-30.2741736217725,-35.8223180338192,
5.18100420262437));
#20432=CARTESIAN_POINT('Ctrl Pts',(-33.0788986413239,-39.395339737909,5.02400407527211));
#20433=CARTESIAN_POINT('Ctrl Pts',(-37.6062936777584,-39.0270181479993,
4.86700394791986));
#20434=CARTESIAN_POINT('Ctrl Pts',(-39.0738472616523,-36.3607409549812,
4.76181040522164));
#20435=CARTESIAN_POINT('Ctrl Pts',(-39.0799345709982,-35.013663708426,4.7089502383075));
#20436=CARTESIAN_POINT('Ctrl Pts',(-39.0799229210932,-35.0002389671693,
4.70842344717745));
#20437=CARTESIAN_POINT('Ctrl Pts',(-39.0792024631389,-35.0015161209354,
5.79157655282255));
#20438=CARTESIAN_POINT('Ctrl Pts',(-39.0731679256319,-33.7557919674485,
5.74271706512043));
#20439=CARTESIAN_POINT('Ctrl Pts',(-37.8030027181165,-31.1651102767228,
5.64152420163424));
#20440=CARTESIAN_POINT('Ctrl Pts',(-33.4155016033557,-30.4724169111822,
5.48799796236394));
#20441=CARTESIAN_POINT('Ctrl Pts',(-30.3495576440316,-33.8239773440302,
5.3309978350117));
#20442=CARTESIAN_POINT('Ctrl Pts',(-31.4537101308888,-38.230088373826,5.17399770765944));
#20443=CARTESIAN_POINT('Ctrl Pts',(-35.7378546799324,-39.7397482704758,
5.01699758030718));
#20444=CARTESIAN_POINT('Ctrl Pts',(-38.6790876767283,-37.5146290150371,
4.88952386202822));
#20445=CARTESIAN_POINT('Ctrl Pts',(-39.0694004131258,-35.5870561070142,
4.81438351953334));
#20446=CARTESIAN_POINT('Ctrl Pts',(-39.0676603684793,-35.0013188448613,
4.79157655282255));
#20447=CARTESIAN_POINT('Origin',(-35.,-35.,10.2084234471775));
#20448=CARTESIAN_POINT('',(-39.0709664927331,-34.9967444357251,6.79157655282255));
#20449=CARTESIAN_POINT('',(-39.0721140267755,-35.0034548068065,6.70842344717746));
#20450=CARTESIAN_POINT('',(-39.0735,-34.9999999999999,10.2084234471775));
#20451=CARTESIAN_POINT('Ctrl Pts',(-39.0721140267755,-35.0034548068065,
6.70842344717746));
#20452=CARTESIAN_POINT('Ctrl Pts',(-39.0638862819908,-34.0266505561004,
6.67028408104986));
#20453=CARTESIAN_POINT('Ctrl Pts',(-38.2252022081515,-31.6968182141492,
6.57981133913816));
#20454=CARTESIAN_POINT('Ctrl Pts',(-34.3564136921927,-30.2465364275518,
6.4370052214424));
#20455=CARTESIAN_POINT('Ctrl Pts',(-30.6802034020135,-32.9145736277213,
6.28000509409013));
#20456=CARTESIAN_POINT('Ctrl Pts',(-30.8775957137286,-37.4526369907548,
6.12300496673789));
#20457=CARTESIAN_POINT('Ctrl Pts',(-34.7715877207675,-39.7913950861294,
5.96600483938563));
#20458=CARTESIAN_POINT('Ctrl Pts',(-38.3794222668459,-38.0681714287485,
5.82781099953215));
#20459=CARTESIAN_POINT('Ctrl Pts',(-39.0639983304887,-35.8575951283075,
5.74195053546276));
#20460=CARTESIAN_POINT('Ctrl Pts',(-39.0692231423099,-34.9973709029543,
5.70842344717745));
#20461=CARTESIAN_POINT('Ctrl Pts',(-39.0709664927331,-34.9967444357251,
6.79157655282255));
#20462=CARTESIAN_POINT('Ctrl Pts',(-39.074129342561,-34.5902726781194,6.77571736227569));
#20463=CARTESIAN_POINT('Ctrl Pts',(-38.8328831908397,-32.8461583454701,
6.70752479594475));
#20464=CARTESIAN_POINT('Ctrl Pts',(-36.3504797430715,-30.3972101963624,
6.58699885382972));
#20465=CARTESIAN_POINT('Ctrl Pts',(-31.905896825022,-31.3344599279876,6.42999872647746));
#20466=CARTESIAN_POINT('Ctrl Pts',(-30.2358028418083,-35.5586616666892,
6.27299859912522));
#20467=CARTESIAN_POINT('Ctrl Pts',(-32.83782160528,-39.2818926978495,6.11599847177295));
#20468=CARTESIAN_POINT('Ctrl Pts',(-37.3786807951101,-39.1655161353224,
5.95899834442071));
#20469=CARTESIAN_POINT('Ctrl Pts',(-39.0372097938135,-36.5125334877904,
5.85085770477057));
#20470=CARTESIAN_POINT('Ctrl Pts',(-39.0796315161011,-35.090086560245,5.79505044090452));
#20471=CARTESIAN_POINT('Ctrl Pts',(-39.0792024631389,-35.0015161209354,
5.79157655282255));
#20472=CARTESIAN_POINT('Origin',(-35.,-35.,10.2084234471775));
#20473=CARTESIAN_POINT('',(-39.0691247390887,-35.0040754761348,7.79157655282255));
#20474=CARTESIAN_POINT('',(-39.0784093524563,-34.997955826836,7.70842344717746));
#20475=CARTESIAN_POINT('',(-39.0735,-34.9999999999999,10.2084234471775));
#20476=CARTESIAN_POINT('',(-36.0520713770612,-38.9352951690526,8.));
#20477=CARTESIAN_POINT('Ctrl Pts',(-36.0520713770612,-38.9352951690526,
8.));
#20478=CARTESIAN_POINT('Ctrl Pts',(-37.3460763064865,-38.5893527455387,
7.94766662421592));
#20479=CARTESIAN_POINT('Ctrl Pts',(-38.8056934287649,-37.2206664159851,
7.87819214182344));
#20480=CARTESIAN_POINT('Ctrl Pts',(-39.0721265495934,-35.4436566771087,
7.80871765943095));
#20481=CARTESIAN_POINT('Ctrl Pts',(-39.0691247390887,-35.0040754761348,
7.79157655282255));
#20482=CARTESIAN_POINT('',(-33.9452801041878,-38.9416007879337,8.));
#20483=CARTESIAN_POINT('Origin',(-35.,-35.,8.));
#20484=CARTESIAN_POINT('Ctrl Pts',(-33.9452677648582,-38.941630165528,8.));
#20485=CARTESIAN_POINT('Ctrl Pts',(-35.1775571519718,-39.2670003808689,
7.95000212253756));
#20486=CARTESIAN_POINT('Ctrl Pts',(-37.9028288422611,-38.6929823061133,
7.85280993826337));
#20487=CARTESIAN_POINT('Ctrl Pts',(-39.0706575059758,-36.2016126262027,
7.75561775398919));
#20488=CARTESIAN_POINT('Ctrl Pts',(-39.0784093524563,-34.997955826836,7.70842344717745));
#20489=CARTESIAN_POINT('Origin',(35.,-35.,10.2084234471775));
#20490=CARTESIAN_POINT('',(30.9212701195312,-34.9980516557686,0.791576552822542));
#20491=CARTESIAN_POINT('',(30.9328376585755,-35.000159236028,0.708423447177449));
#20492=CARTESIAN_POINT('',(30.9265,-34.9999999999999,10.2084234471775));
#20493=CARTESIAN_POINT('',(36.0520713770612,-38.9352951690526,0.));
#20494=CARTESIAN_POINT('Ctrl Pts',(30.9328376585755,-35.000159236028,0.708423447177449));
#20495=CARTESIAN_POINT('Ctrl Pts',(30.9332830863018,-34.31144230346,0.681615801254637));
#20496=CARTESIAN_POINT('Ctrl Pts',(31.423729341332,-32.2777627653814,0.602474779547741));
#20497=CARTESIAN_POINT('Ctrl Pts',(34.6204730639081,-30.2191415991965,0.471000382056761));
#20498=CARTESIAN_POINT('Ctrl Pts',(38.7813009234074,-32.0442168078902,0.314000254704507));
#20499=CARTESIAN_POINT('Ctrl Pts',(39.5450614875854,-36.5273565705141,0.157000127352254));
#20500=CARTESIAN_POINT('Ctrl Pts',(37.3460763064866,-38.5893527455387,0.0523333757840845));
#20501=CARTESIAN_POINT('Ctrl Pts',(36.0520713770612,-38.9352951690526,0.));
#20502=CARTESIAN_POINT('',(33.9452809380949,-38.9416008127442,2.82508323912273E-15));
#20503=CARTESIAN_POINT('Origin',(35.,-35.,0.));
#20504=CARTESIAN_POINT('Ctrl Pts',(30.9212701195312,-34.9980516557686,0.791576552822542));
#20505=CARTESIAN_POINT('Ctrl Pts',(30.9205868455494,-34.8825847167923,0.787049082480475));
#20506=CARTESIAN_POINT('Ctrl Pts',(30.9769555821544,-33.4331078068366,0.730188236354323));
#20507=CARTESIAN_POINT('Ctrl Pts',(32.704491289799,-30.7882324000235,0.620994014444087));
#20508=CARTESIAN_POINT('Ctrl Pts',(37.2468174060219,-30.7615623188695,0.463993887091833));
#20509=CARTESIAN_POINT('Ctrl Pts',(39.7742801854456,-34.536716632844,0.306993759739581));
#20510=CARTESIAN_POINT('Ctrl Pts',(38.0469263053514,-38.6626279973746,0.152329130708969));
#20511=CARTESIAN_POINT('Ctrl Pts',(35.1775586628442,-39.2670009745688,0.0499978774624438));
#20512=CARTESIAN_POINT('Ctrl Pts',(33.94526862329,-38.9416301412996,2.47469145869816E-15));
#20513=CARTESIAN_POINT('Origin',(35.,-35.,10.2084234471775));
#20514=CARTESIAN_POINT('',(30.9325671258701,-34.9990828432724,1.79157655282254));
#20515=CARTESIAN_POINT('',(30.9221796304986,-35.0024921194124,1.70842344717745));
#20516=CARTESIAN_POINT('',(30.9265,-34.9999999999999,10.2084234471775));
#20517=CARTESIAN_POINT('Ctrl Pts',(30.9221796304986,-35.0024921194124,1.70842344717745));
#20518=CARTESIAN_POINT('Ctrl Pts',(30.9307245358113,-33.8250296189916,1.66228272262581));
#20519=CARTESIAN_POINT('Ctrl Pts',(32.0812070745664,-31.2974912653129,1.56380862229009));
#20520=CARTESIAN_POINT('Ctrl Pts',(36.3504798077544,-30.397209980765,1.41300114617028));
#20521=CARTESIAN_POINT('Ctrl Pts',(39.5841211762074,-33.5872716944053,1.25600101881803));
#20522=CARTESIAN_POINT('Ctrl Pts',(38.7070435276578,-38.0442501505519,1.09900089146578));
#20523=CARTESIAN_POINT('Ctrl Pts',(34.5060129254091,-39.7711992366401,0.942000764113522));
#20524=CARTESIAN_POINT('Ctrl Pts',(31.3893173078737,-37.6557923296961,0.811808282684079));
#20525=CARTESIAN_POINT('Ctrl Pts',(30.9324135307783,-35.6559423817109,0.733949177038721));
#20526=CARTESIAN_POINT('Ctrl Pts',(30.9328376585755,-35.000159236028,0.708423447177449));
#20527=CARTESIAN_POINT('Ctrl Pts',(30.9325671258701,-34.9990828432724,1.79157655282254));
#20528=CARTESIAN_POINT('Ctrl Pts',(30.931305764143,-34.3862015569849,1.76771600385165));
#20529=CARTESIAN_POINT('Ctrl Pts',(31.3469048767902,-32.4307110971121,1.69152207909667));
#20530=CARTESIAN_POINT('Ctrl Pts',(34.3564138261785,-30.2465374145616,1.56299477855761));
#20531=CARTESIAN_POINT('Ctrl Pts',(38.6097341605507,-31.8409675209513,1.40599465120535));
#20532=CARTESIAN_POINT('Ctrl Pts',(39.6261694334752,-36.2681500029269,1.2489945238531));
#20533=CARTESIAN_POINT('Ctrl Pts',(36.4942778376799,-39.5581346787212,1.09199439650085));
#20534=CARTESIAN_POINT('Ctrl Pts',(32.1514014998571,-38.7838588891191,0.939521739490662));
#20535=CARTESIAN_POINT('Ctrl Pts',(30.928484861737,-36.2172758912295,0.839382458264559));
#20536=CARTESIAN_POINT('Ctrl Pts',(30.9212701195312,-34.9980516557686,0.791576552822542));
#20537=CARTESIAN_POINT('Origin',(35.,-35.,10.2084234471775));
#20538=CARTESIAN_POINT('',(30.9241574748343,-35.0032082359637,2.79157655282255));
#20539=CARTESIAN_POINT('',(30.9271225309901,-34.9964941798068,2.70842344717745));
#20540=CARTESIAN_POINT('',(30.9265,-34.9999999999999,10.2084234471775));
#20541=CARTESIAN_POINT('Ctrl Pts',(30.9271225309901,-34.9964941798068,2.70842344717745));
#20542=CARTESIAN_POINT('Ctrl Pts',(30.9241960153079,-34.6601099513618,2.69528301978107));
#20543=CARTESIAN_POINT('Ctrl Pts',(31.1149287231428,-32.9873057374911,2.62980921660061));
#20544=CARTESIAN_POINT('Ctrl Pts',(33.4155015345008,-30.4724167149005,2.51200203763606));
#20545=CARTESIAN_POINT('Ctrl Pts',(37.9022802570419,-31.180783908422,2.3550019102838));
#20546=CARTESIAN_POINT('Ctrl Pts',(39.7865571243079,-35.3138779969793,2.19800178293155));
#20547=CARTESIAN_POINT('Ctrl Pts',(37.3786808989502,-39.1655163148135,2.04100165557929));
#20548=CARTESIAN_POINT('Ctrl Pts',(32.8378215103303,-39.2818928860424,1.88400152822704));
#20549=CARTESIAN_POINT('Ctrl Pts',(31.0005092531499,-36.6528810868796,1.77314212542643));
#20550=CARTESIAN_POINT('Ctrl Pts',(30.9210327993872,-35.1605220306295,1.7146160984099));
#20551=CARTESIAN_POINT('Ctrl Pts',(30.9221796304986,-35.0024921194124,1.70842344717745));
#20552=CARTESIAN_POINT('Ctrl Pts',(30.9241574748343,-35.0032082359637,2.79157655282255));
#20553=CARTESIAN_POINT('Ctrl Pts',(30.9336811658698,-33.8995582265895,2.74838292522282));
#20554=CARTESIAN_POINT('Ctrl Pts',(31.9624565435572,-31.4430713953983,2.65285592183902));
#20555=CARTESIAN_POINT('Ctrl Pts',(36.092848009894,-30.329313184686,2.50499554267113));
#20556=CARTESIAN_POINT('Ctrl Pts',(39.4985856069267,-33.3349593710879,2.34799541531888));
#20557=CARTESIAN_POINT('Ctrl Pts',(38.8703983056154,-37.8336637277424,2.19099528796662));
#20558=CARTESIAN_POINT('Ctrl Pts',(34.7715877673847,-39.7913941019012,2.03399516061437));
#20559=CARTESIAN_POINT('Ctrl Pts',(31.4693971488356,-37.8080759514836,1.90085558223301));
#20560=CARTESIAN_POINT('Ctrl Pts',(30.9340723106019,-35.73043494849,1.82004937963573));
#20561=CARTESIAN_POINT('Ctrl Pts',(30.9325671258701,-34.9990828432724,1.79157655282254));
#20562=CARTESIAN_POINT('Origin',(35.,-35.,10.2084234471775));
#20563=CARTESIAN_POINT('',(30.9249291606556,-34.9966356401017,3.79157655282255));
#20564=CARTESIAN_POINT('',(30.9312887064921,-35.0023266137465,3.70842344717745));
#20565=CARTESIAN_POINT('',(30.9265,-34.9999999999999,10.2084234471775));
#20566=CARTESIAN_POINT('Ctrl Pts',(30.9312887064921,-35.0023266137465,3.70842344717745));
#20567=CARTESIAN_POINT('Ctrl Pts',(30.9357302778565,-34.1688705201733,3.67594994115225));
#20568=CARTESIAN_POINT('Ctrl Pts',(31.5875549849899,-31.9858615080358,3.59114305934295));
#20569=CARTESIAN_POINT('Ctrl Pts',(35.1332185405061,-30.2050132515957,3.45400280174957));
#20570=CARTESIAN_POINT('Ctrl Pts',(39.0728865166754,-32.4659833342563,3.29700267439732));
#20571=CARTESIAN_POINT('Ctrl Pts',(39.3603580902194,-36.9992304591644,3.14000254704507));
#20572=CARTESIAN_POINT('Ctrl Pts',(35.7378547119649,-39.73974847612,2.98300241969282));
#20573=CARTESIAN_POINT('Ctrl Pts',(31.8122797042457,-38.3564424059702,2.83914271973694));
#20574=CARTESIAN_POINT('Ctrl Pts',(30.9358512256228,-35.9998017059771,2.74761639556516));
#20575=CARTESIAN_POINT('Ctrl Pts',(30.9271225309901,-34.9964941798068,2.70842344717745));
#20576=CARTESIAN_POINT('Ctrl Pts',(30.9249291606557,-34.9966356401017,3.79157655282255));
#20577=CARTESIAN_POINT('Ctrl Pts',(30.9226270376253,-34.7360558424623,3.78138322237808));
#20578=CARTESIAN_POINT('Ctrl Pts',(31.0631421094905,-33.1401098702831,3.71885651614953));
#20579=CARTESIAN_POINT('Ctrl Pts',(33.1665616130745,-30.567378187653,3.6039964341369));
#20580=CARTESIAN_POINT('Ctrl Pts',(37.6857487228281,-31.0255332130596,3.44699630678465));
#20581=CARTESIAN_POINT('Ctrl Pts',(39.7965991870786,-35.0476307336073,3.28999617943239));
#20582=CARTESIAN_POINT('Ctrl Pts',(37.606293143399,-39.0270173223719,3.13299605208014));
#20583=CARTESIAN_POINT('Ctrl Pts',(33.0788990351993,-39.3953388367078,2.97599592472789));
#20584=CARTESIAN_POINT('Ctrl Pts',(31.0458059595307,-36.8053217637502,2.86218942497536));
#20585=CARTESIAN_POINT('Ctrl Pts',(30.9221422669741,-35.2367399796465,2.80071630100691));
#20586=CARTESIAN_POINT('Ctrl Pts',(30.9241574748343,-35.0032082359637,2.79157655282255));
#20587=CARTESIAN_POINT('Origin',(35.,-35.,10.2084234471775));
#20588=CARTESIAN_POINT('',(30.9323405716502,-35.0013188445396,4.79157655282255));
#20589=CARTESIAN_POINT('',(30.9200767953891,-35.0002389671868,4.70842344717745));
#20590=CARTESIAN_POINT('',(30.9265,-34.9999999999999,10.2084234471775));
#20591=CARTESIAN_POINT('Ctrl Pts',(30.9200767953891,-35.0002389671868,4.70842344717745));
#20592=CARTESIAN_POINT('Ctrl Pts',(30.9212224901389,-33.6800002558017,4.65661686252342));
#20593=CARTESIAN_POINT('Ctrl Pts',(32.3294140201846,-31.0239948489069,4.5524769020853));
#20594=CARTESIAN_POINT('Ctrl Pts',(36.8334388902368,-30.5673769708228,4.39600356586309));
#20595=CARTESIAN_POINT('Ctrl Pts',(39.7085649985197,-34.0839974156347,4.23900343851085));
#20596=CARTESIAN_POINT('Ctrl Pts',(38.3614757008081,-38.4220061649164,4.08200331115859));
#20597=CARTESIAN_POINT('Ctrl Pts',(34.0001188933562,-39.6914691574817,3.92500318380634));
#20598=CARTESIAN_POINT('Ctrl Pts',(31.2520059142893,-37.3616157091949,3.80047656247929));
#20599=CARTESIAN_POINT('Ctrl Pts',(30.9285723681714,-35.5120445806103,3.72828331693633));
#20600=CARTESIAN_POINT('Ctrl Pts',(30.9312887064921,-35.0023266137465,3.70842344717745));
#20601=CARTESIAN_POINT('Ctrl Pts',(30.9323405716502,-35.0013188445396,4.79157655282255));
#20602=CARTESIAN_POINT('Ctrl Pts',(30.9345932718416,-34.2430104629966,4.76205014374926));
#20603=CARTESIAN_POINT('Ctrl Pts',(31.4994189252081,-32.1375393584237,4.68019035889188));
#20604=CARTESIAN_POINT('Ctrl Pts',(34.8667814960507,-30.2050145678827,4.54599719825042));
#20605=CARTESIAN_POINT('Ctrl Pts',(38.9259067064028,-32.2437545499559,4.38899707089817));
#20606=CARTESIAN_POINT('Ctrl Pts',(39.4646337070995,-36.7540462662356,4.23199694354592));
#20607=CARTESIAN_POINT('Ctrl Pts',(35.9998808321606,-39.6914678695931,4.07499681619366));
#20608=CARTESIAN_POINT('Ctrl Pts',(31.921688934453,-38.5044258734202,3.92819001928587));
#20609=CARTESIAN_POINT('Ctrl Pts',(30.934446321843,-36.0738934163447,3.83371659816217));
#20610=CARTESIAN_POINT('Ctrl Pts',(30.9249291606557,-34.9966356401017,3.79157655282255));
#20611=CARTESIAN_POINT('Origin',(35.,-35.,10.2084234471775));
#20612=CARTESIAN_POINT('',(30.9207984791111,-35.0015161195221,5.79157655282255));
#20613=CARTESIAN_POINT('',(30.93077657492,-34.9973709027416,5.70842344717745));
#20614=CARTESIAN_POINT('',(30.9265,-34.9999999999999,10.2084234471775));
#20615=CARTESIAN_POINT('Ctrl Pts',(30.93077657492,-34.9973709027416,5.70842344717745));
#20616=CARTESIAN_POINT('Ctrl Pts',(30.9278458307013,-34.5148468886989,5.68961715967867));
#20617=CARTESIAN_POINT('Ctrl Pts',(31.2287023543687,-32.6931085261371,5.61847749639581));
#20618=CARTESIAN_POINT('Ctrl Pts',(33.9071516901285,-30.3293119021379,5.49500445732887));
#20619=CARTESIAN_POINT('Ctrl Pts',(38.292857772379,-31.5119155853487,5.33800432997662));
#20620=CARTESIAN_POINT('Ctrl Pts',(39.7258267066312,-35.8223180909381,5.18100420262436));
#20621=CARTESIAN_POINT('Ctrl Pts',(36.9211014921746,-39.3953400433581,5.02400407527211));
#20622=CARTESIAN_POINT('Ctrl Pts',(32.3937061411281,-39.0270184278339,4.86700394791986));
#20623=CARTESIAN_POINT('Ctrl Pts',(30.9261524552523,-36.3607410495406,4.76181040522164));
#20624=CARTESIAN_POINT('Ctrl Pts',(30.9200651454832,-35.0136637093765,4.7089502383075));
#20625=CARTESIAN_POINT('Ctrl Pts',(30.9200767953891,-35.0002389671868,4.70842344717745));
#20626=CARTESIAN_POINT('Ctrl Pts',(30.9207984791111,-35.0015161195221,5.79157655282254));
#20627=CARTESIAN_POINT('Ctrl Pts',(30.9268330150145,-33.7557922534996,5.74271706512043));
#20628=CARTESIAN_POINT('Ctrl Pts',(32.1969979306855,-31.1651111648659,5.64152420163423));
#20629=CARTESIAN_POINT('Ctrl Pts',(36.584498029893,-30.4724179566463,5.48799796236395));
#20630=CARTESIAN_POINT('Ctrl Pts',(39.6504412814188,-33.8239776163473,5.33099783501169));
#20631=CARTESIAN_POINT('Ctrl Pts',(38.5462890493217,-38.2300876270061,5.17399770765944));
#20632=CARTESIAN_POINT('Ctrl Pts',(34.2621454906851,-39.7397471751372,5.01699758030718));
#20633=CARTESIAN_POINT('Ctrl Pts',(31.3209131735827,-37.5146284338107,4.88952386202822));
#20634=CARTESIAN_POINT('Ctrl Pts',(30.9306005274021,-35.5870559713077,4.81438351953334));
#20635=CARTESIAN_POINT('Ctrl Pts',(30.9323405716502,-35.0013188445396,4.79157655282255));
#20636=CARTESIAN_POINT('Origin',(35.,-35.,10.2084234471775));
#20637=CARTESIAN_POINT('',(30.9290344477858,-34.9967444478932,6.79157655282255));
#20638=CARTESIAN_POINT('',(30.9278856911952,-35.003454802609,6.70842344717745));
#20639=CARTESIAN_POINT('',(30.9265,-34.9999999999999,10.2084234471775));
#20640=CARTESIAN_POINT('Ctrl Pts',(30.9278856911952,-35.003454802609,6.70842344717745));
#20641=CARTESIAN_POINT('Ctrl Pts',(30.9361134364198,-34.0266504850423,6.67028408104985));
#20642=CARTESIAN_POINT('Ctrl Pts',(31.7747975664789,-31.6968179913154,6.57981133913816));
#20643=CARTESIAN_POINT('Ctrl Pts',(35.6435863532121,-30.2465360930486,6.43700522144239));
#20644=CARTESIAN_POINT('Ctrl Pts',(39.3197968978512,-32.9145734850341,6.28000509409014));
#20645=CARTESIAN_POINT('Ctrl Pts',(39.1224045728929,-37.4526371600059,6.12300496673789));
#20646=CARTESIAN_POINT('Ctrl Pts',(35.2284122950338,-39.7913954197145,5.96600483938562));
#20647=CARTESIAN_POINT('Ctrl Pts',(31.6205774983358,-38.0681716417432,5.82781099953216));
#20648=CARTESIAN_POINT('Ctrl Pts',(30.9360013871094,-35.857595187819,5.74195053546276));
#20649=CARTESIAN_POINT('Ctrl Pts',(30.93077657492,-34.9973709027416,5.70842344717745));
#20650=CARTESIAN_POINT('Ctrl Pts',(30.9290344477858,-34.9967444478932,6.79157655282255));
#20651=CARTESIAN_POINT('Ctrl Pts',(30.9258715916941,-34.5902727617055,6.77571736227569));
#20652=CARTESIAN_POINT('Ctrl Pts',(31.1671176609215,-32.8461587416485,6.70752479594475));
#20653=CARTESIAN_POINT('Ctrl Pts',(33.6495206016122,-30.3972113452741,6.58699885382972));
#20654=CARTESIAN_POINT('Ctrl Pts',(38.09410244091,-31.3344607296745,6.42999872647747));
#20655=CARTESIAN_POINT('Ctrl Pts',(39.7641960678496,-35.558661561786,6.27299859912521));
#20656=CARTESIAN_POINT('Ctrl Pts',(37.1621778889461,-39.2818916953666,6.11599847177296));
#20657=CARTESIAN_POINT('Ctrl Pts',(32.6213197580022,-39.1655151793351,5.95899834442071));
#20658=CARTESIAN_POINT('Ctrl Pts',(30.962791139069,-36.5125331378606,5.85085770477057));
#20659=CARTESIAN_POINT('Ctrl Pts',(30.920369426263,-35.0900865383931,5.79505044090451));
#20660=CARTESIAN_POINT('Ctrl Pts',(30.9207984791111,-35.0015161195221,5.79157655282254));
#20661=CARTESIAN_POINT('Origin',(35.,-35.,10.2084234471775));
#20662=CARTESIAN_POINT('',(30.9308748007386,-35.0040807474719,7.79157655282254));
#20663=CARTESIAN_POINT('',(30.9215903995924,-34.9979557257256,7.70842344717745));
#20664=CARTESIAN_POINT('',(30.9265,-34.9999999999999,10.2084234471775));
#20665=CARTESIAN_POINT('',(33.9479286229388,-38.9352951690526,8.));
#20666=CARTESIAN_POINT('Ctrl Pts',(33.9479286229388,-38.9352951690526,8.));
#20667=CARTESIAN_POINT('Ctrl Pts',(32.6539236935135,-38.5893527455387,7.94766662421592));
#20668=CARTESIAN_POINT('Ctrl Pts',(31.1943052713303,-37.2206748258175,7.87819214182343));
#20669=CARTESIAN_POINT('Ctrl Pts',(30.9278727863252,-35.4436627970733,7.80871765943094));
#20670=CARTESIAN_POINT('Ctrl Pts',(30.9308748007386,-35.0040807474719,7.79157655282254));
#20671=CARTESIAN_POINT('',(36.0547201762178,-38.9416007819636,8.));
#20672=CARTESIAN_POINT('Origin',(35.,-35.,8.));
#20673=CARTESIAN_POINT('Ctrl Pts',(36.0547325237759,-38.9416301760088,8.));
#20674=CARTESIAN_POINT('Ctrl Pts',(34.822443357586,-39.2670001819919,7.95000212253756));
#20675=CARTESIAN_POINT('Ctrl Pts',(32.0971704836176,-38.6929832307492,7.85280993826338));
#20676=CARTESIAN_POINT('Ctrl Pts',(30.9293421550372,-36.2016127302822,7.75561775398919));
#20677=CARTESIAN_POINT('Ctrl Pts',(30.9215903995924,-34.9979557257256,7.70842344717745));
#20678=CARTESIAN_POINT('Origin',(35.,-35.,10.2084234471775));
#20679=CARTESIAN_POINT('Ctrl Pts',(30.9215903995924,-34.9979557257256,7.70842344717745));
#20680=CARTESIAN_POINT('Ctrl Pts',(30.9207462976534,-34.8668874511107,7.70328437820511));
#20681=CARTESIAN_POINT('Ctrl Pts',(30.9854756915705,-33.4019022214529,7.64581193344868));
#20682=CARTESIAN_POINT('Ctrl Pts',(32.753181490405,-30.7615622140283,7.53600611290817));
#20683=CARTESIAN_POINT('Ctrl Pts',(37.2955095733766,-30.7882306349807,7.3790059855559));
#20684=CARTESIAN_POINT('Ctrl Pts',(39.7793714317054,-34.5910508431566,7.22200585820367));
#20685=CARTESIAN_POINT('Ctrl Pts',(37.9775552386376,-38.7608686529102,7.0650057308514));
#20686=CARTESIAN_POINT('Ctrl Pts',(33.5057217267653,-39.5581360350982,6.90800560349915));
#20687=CARTESIAN_POINT('Ctrl Pts',(31.1346464724166,-37.067372389099,6.7891448422745));
#20688=CARTESIAN_POINT('Ctrl Pts',(30.9248236399074,-35.3669839150134,6.72261745683393));
#20689=CARTESIAN_POINT('Ctrl Pts',(30.9278856911952,-35.003454802609,6.70842344717745));
#20690=CARTESIAN_POINT('Ctrl Pts',(30.9308748007386,-35.0040807474719,7.79157655282254));
#20691=CARTESIAN_POINT('Ctrl Pts',(30.9370382125719,-34.10157834971,7.75638428364686));
#20692=CARTESIAN_POINT('Ctrl Pts',(31.6729756008745,-31.8449525580975,7.66885863868709));
#20693=CARTESIAN_POINT('Ctrl Pts',(35.3795267558193,-30.2191465582126,7.52899961794324));
#20694=CARTESIAN_POINT('Ctrl Pts',(39.1969165266342,-32.6774422642514,7.37199949059099));
#20695=CARTESIAN_POINT('Ctrl Pts',(39.2524336251343,-37.2202141105436,7.21499936323873));
#20696=CARTESIAN_POINT('Ctrl Pts',(35.4939867861423,-39.7711972931265,7.05799923588648));
#20697=CARTESIAN_POINT('Ctrl Pts',(31.7173198121032,-38.2186953257486,6.91685829908109));
#20698=CARTESIAN_POINT('Ctrl Pts',(30.9363086272988,-35.9315792701304,6.82805073805977));
#20699=CARTESIAN_POINT('Ctrl Pts',(30.9290344477858,-34.9967444478932,6.79157655282255));
#20700=CARTESIAN_POINT('Ctrl Pts',(37.6735319337713,-32.7141668369925,8.));
#20701=CARTESIAN_POINT('Ctrl Pts',(38.4251602751564,-33.5932784036374,7.94766662421592));
#20702=CARTESIAN_POINT('Ctrl Pts',(38.9814215765655,-36.1362159265307,7.84299987264775));
#20703=CARTESIAN_POINT('Ctrl Pts',(36.2450915261219,-38.9529260673994,7.6859997452955));
#20704=CARTESIAN_POINT('Ctrl Pts',(32.3914756047223,-38.2165112413961,7.52899961794324));
#20705=CARTESIAN_POINT('Ctrl Pts',(30.8773704214612,-34.5999494268526,7.37199949059098));
#20706=CARTESIAN_POINT('Ctrl Pts',(33.0598541530624,-31.3400748957517,7.21499936323873));
#20707=CARTESIAN_POINT('Ctrl Pts',(36.9821909719779,-31.3631032916521,7.05799923588648));
#20708=CARTESIAN_POINT('Ctrl Pts',(39.127025656321,-34.6468691152089,6.90099910853422));
#20709=CARTESIAN_POINT('Ctrl Pts',(37.5711428874206,-38.2475403183041,6.74399898118197));
#20710=CARTESIAN_POINT('Ctrl Pts',(33.7096786974094,-38.9359871126692,6.58699885382972));
#20711=CARTESIAN_POINT('Ctrl Pts',(31.005264414648,-36.0950579743517,6.42999872647747));
#20712=CARTESIAN_POINT('Ctrl Pts',(31.8829646703068,-32.272149334312,6.27299859912521));
#20713=CARTESIAN_POINT('Ctrl Pts',(35.5557419902844,-30.8953456995945,6.11599847177296));
#20714=CARTESIAN_POINT('Ctrl Pts',(38.7301793514647,-33.1992174379789,5.9589983444207));
#20715=CARTESIAN_POINT('Ctrl Pts',(38.5597294918745,-37.1178719063019,5.80199821706845));
#20716=CARTESIAN_POINT('Ctrl Pts',(35.1972358531438,-39.137408466637,5.6449980897162));
#20717=CARTESIAN_POINT('Ctrl Pts',(31.6578790286353,-37.4468920814909,5.48799796236395));
#20718=CARTESIAN_POINT('Ctrl Pts',(31.115434094392,-33.5622236362915,5.33099783501169));
#20719=CARTESIAN_POINT('Ctrl Pts',(34.0563166981778,-30.9668232762417,5.17399770765944));
#20720=CARTESIAN_POINT('Ctrl Pts',(37.8434091602659,-31.9880110645548,5.01699758030718));
#20721=CARTESIAN_POINT('Ctrl Pts',(39.0807893557322,-35.7100782827727,4.85999745295493));
#20722=CARTESIAN_POINT('Ctrl Pts',(36.6588865837055,-38.7954114649594,4.70299732560268));
#20723=CARTESIAN_POINT('Ctrl Pts',(32.7494442988629,-38.4773627887335,4.54599719825042));
#20724=CARTESIAN_POINT('Ctrl Pts',(30.8580969013801,-35.0411295327127,4.38899707089817));
#20725=CARTESIAN_POINT('Ctrl Pts',(32.6808337483856,-31.5680150335338,4.23199694354591));
#20726=CARTESIAN_POINT('Ctrl Pts',(36.5831892221451,-31.1723943770392,4.07499681619367));
#20727=CARTESIAN_POINT('Ctrl Pts',(39.0658837319978,-34.2090244039511,3.91799668884141));
#20728=CARTESIAN_POINT('Ctrl Pts',(37.9026612931367,-37.9549298355453,3.76099656148916));
#20729=CARTESIAN_POINT('Ctrl Pts',(34.1365946255998,-39.0511213358148,3.6039964341369));
#20730=CARTESIAN_POINT('Ctrl Pts',(31.144751840957,-36.5146334688211,3.44699630678465));
#20731=CARTESIAN_POINT('Ctrl Pts',(31.6099470650134,-32.6199592409358,3.2899961794324));
#20732=CARTESIAN_POINT('Ctrl Pts',(35.1150352807734,-30.8594903921659,3.13299605208014));
#20733=CARTESIAN_POINT('Ctrl Pts',(38.5169702522169,-32.811856236221,2.97599592472789));
#20734=CARTESIAN_POINT('Ctrl Pts',(38.7652042671773,-36.72635157484,2.81899579737563));
#20735=CARTESIAN_POINT('Ctrl Pts',(35.6371434759633,-39.0928109156136,2.66199567002339));
#20736=CARTESIAN_POINT('Ctrl Pts',(31.9377500537671,-37.7892074010372,2.50499554267113));
#20737=CARTESIAN_POINT('Ctrl Pts',(30.9843054629328,-33.9844949374723,2.34799541531888));
#20738=CARTESIAN_POINT('Ctrl Pts',(33.6317728360394,-31.0903954325918,2.19099528796662));
#20739=CARTESIAN_POINT('Ctrl Pts',(37.5061423356192,-31.7020761993063,2.03399516061437));
#20740=CARTESIAN_POINT('Ctrl Pts',(39.1332305596546,-35.2710361738983,1.87699503326212));
#20741=CARTESIAN_POINT('Ctrl Pts',(37.054010080289,-38.5969568276314,1.71999490590986));
#20742=CARTESIAN_POINT('Ctrl Pts',(33.1329414907541,-38.6974489325283,1.56299477855761));
#20743=CARTESIAN_POINT('Ctrl Pts',(30.8860772740811,-35.4824088577318,1.40599465120536));
#20744=CARTESIAN_POINT('Ctrl Pts',(32.3282169135405,-31.8347765477019,1.2489945238531));
#20745=CARTESIAN_POINT('Ctrl Pts',(36.1661501715419,-31.025453813021,1.09199439650085));
#20746=CARTESIAN_POINT('Ctrl Pts',(38.9584254909315,-33.7800977501094,0.934994269148596));
#20747=CARTESIAN_POINT('Ctrl Pts',(38.201061889907,-37.6287344800703,0.777994141796343));
#20748=CARTESIAN_POINT('Ctrl Pts',(34.5734381895487,-39.1199689001796,0.620994014444089));
#20749=CARTESIAN_POINT('Ctrl Pts',(31.3279885395076,-36.9171722692834,0.463993887091836));
#20750=CARTESIAN_POINT('Ctrl Pts',(31.3759276866332,-32.994453947074,0.306993759739581));
#20751=CARTESIAN_POINT('Ctrl Pts',(34.6722754393756,-30.8716903339078,0.149993632387328));
#20752=CARTESIAN_POINT('Ctrl Pts',(38.2651837481491,-32.4476574497985,-0.00700649496492499));
#20753=CARTESIAN_POINT('Ctrl Pts',(38.9246971357756,-36.3188846782332,-0.164006622317179));
#20754=CARTESIAN_POINT('Ctrl Pts',(37.0258557525633,-38.0994349533404,-0.268673373885348));
#20755=CARTESIAN_POINT('Ctrl Pts',(35.9084720925035,-38.3981590173419,-0.321006749669432));
#20756=CARTESIAN_POINT('Ctrl Pts',(37.8143974874483,-32.5937287191406,8.10700224988981));
#20757=CARTESIAN_POINT('Ctrl Pts',(38.6056283266121,-33.5191597390956,8.05466887410573));
#20758=CARTESIAN_POINT('Ctrl Pts',(39.1911984442813,-36.1960819350737,7.95000212253756));
#20759=CARTESIAN_POINT('Ctrl Pts',(36.3106940741934,-39.1612015370487,7.7930019951853));
#20760=CARTESIAN_POINT('Ctrl Pts',(32.2540352290981,-38.3859857972091,7.63600186783306));
#20761=CARTESIAN_POINT('Ctrl Pts',(30.6601534543285,-34.5788711876989,7.47900174048079));
#20762=CARTESIAN_POINT('Ctrl Pts',(32.9576299321766,-31.1472373351772,7.32200161312855));
#20763=CARTESIAN_POINT('Ctrl Pts',(37.0866305057775,-31.1714790727616,7.16500148577629));
#20764=CARTESIAN_POINT('Ctrl Pts',(39.3444742481158,-34.6282630245248,7.00800135842403));
#20765=CARTESIAN_POINT('Ctrl Pts',(37.7066136711597,-38.4186497631728,6.85100123107179));
#20766=CARTESIAN_POINT('Ctrl Pts',(33.641693040528,-39.1433700868122,6.69400110371952));
#20767=CARTESIAN_POINT('Ctrl Pts',(30.7947860459719,-36.1527554141754,6.53700097636728));
#20768=CARTESIAN_POINT('Ctrl Pts',(31.718731394466,-32.1284217844307,6.38000084901502));
#20769=CARTESIAN_POINT('Ctrl Pts',(35.5850234445937,-30.6790758307459,6.22300072166277));
#20770=CARTESIAN_POINT('Ctrl Pts',(38.9267185335935,-33.1043361203307,6.06600059431051));
#20771=CARTESIAN_POINT('Ctrl Pts',(38.747287852214,-37.2294603242033,5.90900046695826));
#20772=CARTESIAN_POINT('Ctrl Pts',(35.2076280004405,-39.3554041176628,5.75200033960601));
#20773=CARTESIAN_POINT('Ctrl Pts',(31.481786229765,-37.5758162224347,5.59500021225375));
#20774=CARTESIAN_POINT('Ctrl Pts',(30.9107604489508,-33.4864687290921,5.4380000849015));
#20775=CARTESIAN_POINT('Ctrl Pts',(34.0065950288281,-30.7543194848738,5.28099995754925));
#20776=CARTESIAN_POINT('Ctrl Pts',(37.9932253643036,-31.8293125714861,5.123999830197));
#20777=CARTESIAN_POINT('Ctrl Pts',(39.2958018060318,-35.7474915521612,4.96699970284474));
#20778=CARTESIAN_POINT('Ctrl Pts',(36.7462915531952,-38.995387657759,4.80999957549249));
#20779=CARTESIAN_POINT('Ctrl Pts',(32.6308649129514,-38.6605813351003,4.65299944814023));
#20780=CARTESIAN_POINT('Ctrl Pts',(30.6398644329761,-35.0432966040406,4.49599932078798));
#20781=CARTESIAN_POINT('Ctrl Pts',(32.5586393455524,-31.3871873963525,4.33899919343573));
#20782=CARTESIAN_POINT('Ctrl Pts',(36.6666057781757,-30.9707219083004,4.18199906608348));
#20783=CARTESIAN_POINT('Ctrl Pts',(39.2801108208385,-34.167348741179,4.02499893873122));
#20784=CARTESIAN_POINT('Ctrl Pts',(38.0555994290271,-38.1106219453356,3.86799881137897));
#20785=CARTESIAN_POINT('Ctrl Pts',(34.0911027148519,-39.2645706097038,3.71099868402672));
#20786=CARTESIAN_POINT('Ctrl Pts',(30.9416229163962,-36.5944378951337,3.55399855667446));
#20787=CARTESIAN_POINT('Ctrl Pts',(31.4313287819664,-32.494557425059,3.39699842932221));
#20788=CARTESIAN_POINT('Ctrl Pts',(35.1210963673509,-30.6413313453092,3.23999830196996));
#20789=CARTESIAN_POINT('Ctrl Pts',(38.7022756737031,-32.6965652688994,3.0829981746177));
#20790=CARTESIAN_POINT('Ctrl Pts',(38.963588874858,-36.8173112029482,2.92599804726545));
#20791=CARTESIAN_POINT('Ctrl Pts',(35.6707138879638,-39.3084567691156,2.76899791991319));
#20792=CARTESIAN_POINT('Ctrl Pts',(31.7764033615041,-37.9361677720372,2.61199779256094));
#20793=CARTESIAN_POINT('Ctrl Pts',(30.7727227893853,-33.9309890559499,2.45499766520869));
#20794=CARTESIAN_POINT('Ctrl Pts',(33.5596824021932,-30.8844025266947,2.29799753785643));
#20795=CARTESIAN_POINT('Ctrl Pts',(37.6381883094267,-31.5283121023449,2.14099741050418));
#20796=CARTESIAN_POINT('Ctrl Pts',(39.3510060812057,-35.2853167815919,1.98399728315193));
#20797=CARTESIAN_POINT('Ctrl Pts',(37.1622336865094,-38.7864766566921,1.82699715579967));
#20798=CARTESIAN_POINT('Ctrl Pts',(33.0345681639462,-38.8922635836996,1.66999702844742));
#20799=CARTESIAN_POINT('Ctrl Pts',(30.6693190617512,-35.5078264672934,1.51299690109517));
#20800=CARTESIAN_POINT('Ctrl Pts',(32.187443504768,-31.6680042909403,1.35599677374291));
#20801=CARTESIAN_POINT('Ctrl Pts',(36.2275933836127,-30.8160392022689,1.19899664639066));
#20802=CARTESIAN_POINT('Ctrl Pts',(39.1669907193568,-33.715822398208,1.04199651903841));
#20803=CARTESIAN_POINT('Ctrl Pts',(38.3697224358239,-37.7672397035641,0.884996391686155));
#20804=CARTESIAN_POINT('Ctrl Pts',(34.5509631015021,-39.3370456789998,0.7279962643339));
#20805=CARTESIAN_POINT('Ctrl Pts',(31.1345141616793,-37.0181860368003,0.570996136981647));
#20806=CARTESIAN_POINT('Ctrl Pts',(31.1849791714726,-32.8887838589028,0.413996009629392));
#20807=CARTESIAN_POINT('Ctrl Pts',(34.6550079808865,-30.6541740890041,0.256995882277139));
#20808=CARTESIAN_POINT('Ctrl Pts',(38.4372228065685,-32.313177235829,0.0999957549248859));
#20809=CARTESIAN_POINT('Ctrl Pts',(39.1314852530455,-36.3883753089936,-0.0570043724273679));
#20810=CARTESIAN_POINT('Ctrl Pts',(37.1325959372044,-38.2627408840732,-0.161671123995537));
#20811=CARTESIAN_POINT('Ctrl Pts',(35.9563385206894,-38.5772044012455,-0.214004499779622));
#20812=CARTESIAN_POINT('Ctrl Pts',(37.9552630411254,-32.4732906012887,8.21400449977962));
#20813=CARTESIAN_POINT('Ctrl Pts',(38.7860963780679,-33.4450410745538,8.16167112399554));
#20814=CARTESIAN_POINT('Ctrl Pts',(39.400975311997,-36.2559479436168,8.05700437242737));
#20815=CARTESIAN_POINT('Ctrl Pts',(36.3762966222648,-39.369477006698,7.90000424507512));
#20816=CARTESIAN_POINT('Ctrl Pts',(32.1165948534739,-38.5554603530221,7.74300411772285));
#20817=CARTESIAN_POINT('Ctrl Pts',(30.4429364871958,-34.5577929485451,7.58600399037062));
#20818=CARTESIAN_POINT('Ctrl Pts',(32.8554057112908,-30.9543997746027,7.42900386301835));
#20819=CARTESIAN_POINT('Ctrl Pts',(37.191070039577,-30.9798548538712,7.2720037356661));
#20820=CARTESIAN_POINT('Ctrl Pts',(39.5619228399106,-34.6096569338406,7.11500360831384));
#20821=CARTESIAN_POINT('Ctrl Pts',(37.8420844548986,-38.5897592080416,6.9580034809616));
#20822=CARTESIAN_POINT('Ctrl Pts',(33.5737073836467,-39.3507530609551,6.80100335360933));
#20823=CARTESIAN_POINT('Ctrl Pts',(30.5843076772956,-36.2104528539991,6.64400322625709));
#20824=CARTESIAN_POINT('Ctrl Pts',(31.5544981186253,-31.9846942345494,6.48700309890483));
#20825=CARTESIAN_POINT('Ctrl Pts',(35.6143048989029,-30.4628059618972,6.33000297155259));
#20826=CARTESIAN_POINT('Ctrl Pts',(39.1232577157224,-33.0094548026823,6.17300284420032));
#20827=CARTESIAN_POINT('Ctrl Pts',(38.9348462125535,-37.3410487421046,6.01600271684808));
#20828=CARTESIAN_POINT('Ctrl Pts',(35.2180201477371,-39.5733997686886,5.85900258949581));
#20829=CARTESIAN_POINT('Ctrl Pts',(31.3056934308947,-37.7047403633785,5.70200246214358));
#20830=CARTESIAN_POINT('Ctrl Pts',(30.7060868035096,-33.4107138218927,5.54500233479131));
#20831=CARTESIAN_POINT('Ctrl Pts',(33.9568733594783,-30.5418156935059,5.38800220743906));
#20832=CARTESIAN_POINT('Ctrl Pts',(38.1430415683413,-31.6706140784174,5.2310020800868));
#20833=CARTESIAN_POINT('Ctrl Pts',(39.5108142563315,-35.7849048215497,5.07400195273456));
#20834=CARTESIAN_POINT('Ctrl Pts',(36.8336965226849,-39.1953638505585,4.9170018253823));
#20835=CARTESIAN_POINT('Ctrl Pts',(32.5122855270398,-38.8437998814671,4.76000169803005));
#20836=CARTESIAN_POINT('Ctrl Pts',(30.4216319645722,-35.0454636753686,4.60300157067779));
#20837=CARTESIAN_POINT('Ctrl Pts',(32.4364449427192,-31.2063597591713,4.44600144332554));
#20838=CARTESIAN_POINT('Ctrl Pts',(36.7500223342062,-30.7690494395616,4.28900131597329));
#20839=CARTESIAN_POINT('Ctrl Pts',(39.4943379096791,-34.1256730784068,4.13200118862103));
#20840=CARTESIAN_POINT('Ctrl Pts',(38.2085375649176,-38.266314055126,3.97500106126878));
#20841=CARTESIAN_POINT('Ctrl Pts',(34.0456108041041,-39.4780198835927,3.81800093391653));
#20842=CARTESIAN_POINT('Ctrl Pts',(30.7384939918355,-36.6742423214464,3.66100080656427));
#20843=CARTESIAN_POINT('Ctrl Pts',(31.2527104989195,-32.3691556091822,3.50400067921202));
#20844=CARTESIAN_POINT('Ctrl Pts',(35.1271574539286,-30.4231722984524,3.34700055185977));
#20845=CARTESIAN_POINT('Ctrl Pts',(38.8875810951892,-32.5812743015779,3.19000042450751));
#20846=CARTESIAN_POINT('Ctrl Pts',(39.1619734825387,-36.9082708310562,3.03300029715526));
#20847=CARTESIAN_POINT('Ctrl Pts',(35.7042842999643,-39.5241026226178,2.876000169803));
#20848=CARTESIAN_POINT('Ctrl Pts',(31.6150566692411,-38.083128143037,2.71900004245075));
#20849=CARTESIAN_POINT('Ctrl Pts',(30.5611401158378,-33.8774831744275,2.5619999150985));
#20850=CARTESIAN_POINT('Ctrl Pts',(33.487591968347,-30.6784096207976,2.40499978774624));
#20851=CARTESIAN_POINT('Ctrl Pts',(37.7702342832343,-31.3545480053834,2.24799966039399));
#20852=CARTESIAN_POINT('Ctrl Pts',(39.5687816027568,-35.2995973892856,2.09099953304174));
#20853=CARTESIAN_POINT('Ctrl Pts',(37.2704572927298,-38.9759964857528,1.93399940568948));
#20854=CARTESIAN_POINT('Ctrl Pts',(32.9361948371383,-39.087078234871,1.77699927833723));
#20855=CARTESIAN_POINT('Ctrl Pts',(30.4525608494213,-35.533244076855,1.61999915098498));
#20856=CARTESIAN_POINT('Ctrl Pts',(32.0466700959956,-31.5012320341786,1.46299902363273));
#20857=CARTESIAN_POINT('Ctrl Pts',(36.2890365956835,-30.606624591517,1.30599889628047));
#20858=CARTESIAN_POINT('Ctrl Pts',(39.3755559477821,-33.6515470463066,1.14899876892822));
#20859=CARTESIAN_POINT('Ctrl Pts',(38.5383829817409,-37.905744927058,0.991998641575965));
#20860=CARTESIAN_POINT('Ctrl Pts',(34.5284880134556,-39.55412245782,0.83499851422371));
#20861=CARTESIAN_POINT('Ctrl Pts',(30.9410397838509,-37.1191998043172,0.677998386871458));
#20862=CARTESIAN_POINT('Ctrl Pts',(30.9940306563121,-32.7831137707316,0.520998259519202));
#20863=CARTESIAN_POINT('Ctrl Pts',(34.6377405223973,-30.4366578441002,0.36399813216695));
#20864=CARTESIAN_POINT('Ctrl Pts',(38.6092618649879,-32.1786970218597,0.206998004814696));
#20865=CARTESIAN_POINT('Ctrl Pts',(39.3382733703155,-36.4578659397538,0.0499978774624431));
#20866=CARTESIAN_POINT('Ctrl Pts',(37.2393361218455,-38.4260468148059,-0.0546688741057264));
#20867=CARTESIAN_POINT('Ctrl Pts',(36.0042049488753,-38.756249785149,-0.107002249889811));
#20868=CARTESIAN_POINT('Ctrl Pts',(38.0961285948024,-32.3528524834367,8.32100674966943));
#20869=CARTESIAN_POINT('Ctrl Pts',(38.9665644295237,-33.3709224100119,8.26867337388535));
#20870=CARTESIAN_POINT('Ctrl Pts',(39.6107521797128,-36.3158139521599,8.16400662231718));
#20871=CARTESIAN_POINT('Ctrl Pts',(36.4418991703362,-39.5777524763472,8.00700649496493));
#20872=CARTESIAN_POINT('Ctrl Pts',(31.9791544778497,-38.724934908835,7.85000636761268));
#20873=CARTESIAN_POINT('Ctrl Pts',(30.2257195200631,-34.5367147093914,7.69300624026041));
#20874=CARTESIAN_POINT('Ctrl Pts',(32.753181490405,-30.7615622140283,7.53600611290817));
#20875=CARTESIAN_POINT('Ctrl Pts',(37.2955095733766,-30.7882306349807,7.3790059855559));
#20876=CARTESIAN_POINT('Ctrl Pts',(39.7793714317054,-34.5910508431566,7.22200585820367));
#20877=CARTESIAN_POINT('Ctrl Pts',(37.9775552386376,-38.7608686529102,7.0650057308514));
#20878=CARTESIAN_POINT('Ctrl Pts',(33.5057217267653,-39.5581360350982,6.90800560349915));
#20879=CARTESIAN_POINT('Ctrl Pts',(30.3738293086194,-36.2681502938228,6.7510054761469));
#20880=CARTESIAN_POINT('Ctrl Pts',(31.3902648427845,-31.8409666846681,6.59400534879465));
#20881=CARTESIAN_POINT('Ctrl Pts',(35.6435863532121,-30.2465360930486,6.43700522144239));
#20882=CARTESIAN_POINT('Ctrl Pts',(39.3197968978512,-32.9145734850341,6.28000509409014));
#20883=CARTESIAN_POINT('Ctrl Pts',(39.1224045728929,-37.4526371600059,6.12300496673789));
#20884=CARTESIAN_POINT('Ctrl Pts',(35.2284122950338,-39.7913954197145,5.96600483938562));
#20885=CARTESIAN_POINT('Ctrl Pts',(31.1296006320244,-37.8336645043222,5.80900471203338));
#20886=CARTESIAN_POINT('Ctrl Pts',(30.5014131580684,-33.3349589146933,5.65200458468112));
#20887=CARTESIAN_POINT('Ctrl Pts',(33.9071516901285,-30.3293119021379,5.49500445732887));
#20888=CARTESIAN_POINT('Ctrl Pts',(38.292857772379,-31.5119155853487,5.33800432997662));
#20889=CARTESIAN_POINT('Ctrl Pts',(39.7258267066312,-35.8223180909381,5.18100420262436));
#20890=CARTESIAN_POINT('Ctrl Pts',(36.9211014921746,-39.3953400433581,5.02400407527211));
#20891=CARTESIAN_POINT('Ctrl Pts',(32.3937061411281,-39.0270184278339,4.86700394791986));
#20892=CARTESIAN_POINT('Ctrl Pts',(30.2033994961682,-35.0476307466965,4.7100038205676));
#20893=CARTESIAN_POINT('Ctrl Pts',(32.314250539886,-31.02553212199,4.55300369321535));
#20894=CARTESIAN_POINT('Ctrl Pts',(36.8334388902368,-30.5673769708228,4.39600356586309));
#20895=CARTESIAN_POINT('Ctrl Pts',(39.7085649985197,-34.0839974156347,4.23900343851085));
#20896=CARTESIAN_POINT('Ctrl Pts',(38.3614757008081,-38.4220061649164,4.08200331115859));
#20897=CARTESIAN_POINT('Ctrl Pts',(34.0001188933562,-39.6914691574817,3.92500318380634));
#20898=CARTESIAN_POINT('Ctrl Pts',(30.5353650672746,-36.754046747759,3.76800305645408));
#20899=CARTESIAN_POINT('Ctrl Pts',(31.0740922158726,-32.2437537933055,3.61100292910183));
#20900=CARTESIAN_POINT('Ctrl Pts',(35.1332185405061,-30.2050132515957,3.45400280174957));
#20901=CARTESIAN_POINT('Ctrl Pts',(39.0728865166754,-32.4659833342563,3.29700267439732));
#20902=CARTESIAN_POINT('Ctrl Pts',(39.3603580902194,-36.9992304591644,3.14000254704507));
#20903=CARTESIAN_POINT('Ctrl Pts',(35.7378547119649,-39.73974847612,2.98300241969282));
#20904=CARTESIAN_POINT('Ctrl Pts',(31.453709976978,-38.2300885140369,2.82600229234056));
#20905=CARTESIAN_POINT('Ctrl Pts',(30.3495574422904,-33.8239772929051,2.66900216498831));
#20906=CARTESIAN_POINT('Ctrl Pts',(33.4155015345008,-30.4724167149005,2.51200203763606));
#20907=CARTESIAN_POINT('Ctrl Pts',(37.9022802570419,-31.180783908422,2.3550019102838));
#20908=CARTESIAN_POINT('Ctrl Pts',(39.7865571243079,-35.3138779969793,2.19800178293155));
#20909=CARTESIAN_POINT('Ctrl Pts',(37.3786808989502,-39.1655163148135,2.04100165557929));
#20910=CARTESIAN_POINT('Ctrl Pts',(32.8378215103303,-39.2818928860424,1.88400152822704));
#20911=CARTESIAN_POINT('Ctrl Pts',(30.2358026370915,-35.5586616864166,1.72700140087479));
#20912=CARTESIAN_POINT('Ctrl Pts',(31.9058966872231,-31.3344597774169,1.57000127352254));
#20913=CARTESIAN_POINT('Ctrl Pts',(36.3504798077544,-30.397209980765,1.41300114617028));
#20914=CARTESIAN_POINT('Ctrl Pts',(39.5841211762074,-33.5872716944053,1.25600101881803));
#20915=CARTESIAN_POINT('Ctrl Pts',(38.7070435276578,-38.0442501505519,1.09900089146578));
#20916=CARTESIAN_POINT('Ctrl Pts',(34.5060129254091,-39.7711992366401,0.942000764113522));
#20917=CARTESIAN_POINT('Ctrl Pts',(30.7475654060226,-37.220213571834,0.785000636761267));
#20918=CARTESIAN_POINT('Ctrl Pts',(30.8030821411515,-32.6774436825603,0.628000509409014));
#20919=CARTESIAN_POINT('Ctrl Pts',(34.6204730639081,-30.2191415991965,0.471000382056761));
#20920=CARTESIAN_POINT('Ctrl Pts',(38.7813009234074,-32.0442168078902,0.314000254704507));
#20921=CARTESIAN_POINT('Ctrl Pts',(39.5450614875854,-36.5273565705141,0.157000127352254));
#20922=CARTESIAN_POINT('Ctrl Pts',(37.3460763064866,-38.5893527455387,0.0523333757840845));
#20923=CARTESIAN_POINT('Ctrl Pts',(36.0520713770612,-38.9352951690526,0.));
#20924=CARTESIAN_POINT('Ctrl Pts',(36.0520713770612,-38.9352951690526,0.));
#20925=CARTESIAN_POINT('Ctrl Pts',(36.1681792863691,-38.8956805730896,-1.36202072051053E-17));
#20926=CARTESIAN_POINT('Ctrl Pts',(36.2820221354364,-38.8505155517789,2.68655360649277E-15));
#20927=CARTESIAN_POINT('Ctrl Pts',(36.3933740322884,-38.80015771728,1.94289029309402E-15));
#20928=CARTESIAN_POINT('Ctrl Pts',(36.5072231634749,-38.7486705323445,1.18254920758684E-15));
#20929=CARTESIAN_POINT('Ctrl Pts',(36.6184689861953,-38.6917545108625,4.54098351417643E-16));
#20930=CARTESIAN_POINT('Ctrl Pts',(36.7268457946485,-38.6297432931302,1.66533453693773E-16));
#20931=CARTESIAN_POINT('Ctrl Pts',(36.8407841942848,-38.56454983515,-1.35788460984399E-16));
#20932=CARTESIAN_POINT('Ctrl Pts',(36.9515525365026,-38.4937243961273,-1.82271800722416E-15));
#20933=CARTESIAN_POINT('Ctrl Pts',(37.0588029145039,-38.4176084656939,-1.99840144432528E-15));
#20934=CARTESIAN_POINT('Ctrl Pts',(37.1526469952551,-38.3510070265646,-2.15212445178876E-15));
#20935=CARTESIAN_POINT('Ctrl Pts',(37.2437973301633,-38.2803539972376,-9.7785017405382E-16));
#20936=CARTESIAN_POINT('Ctrl Pts',(37.3319893511255,-38.2058560072044,-8.88178419700125E-16));
#20937=CARTESIAN_POINT('Ctrl Pts',(37.3493647837374,-38.1911785478217,-8.70511452689226E-16));
#20938=CARTESIAN_POINT('Ctrl Pts',(37.3666252839799,-38.1763517900465,-1.48427532953915E-15));
#20939=CARTESIAN_POINT('Ctrl Pts',(37.3837686739948,-38.1613772431262,-1.55431223447522E-15));
#20940=CARTESIAN_POINT('Ctrl Pts',(37.3963029962073,-38.1504286620158,-1.60551944217877E-15));
#20941=CARTESIAN_POINT('Ctrl Pts',(37.4087735029071,-38.139402069251,-1.97641509759958E-15));
#20942=CARTESIAN_POINT('Ctrl Pts',(37.4211705433933,-38.1283061781123,-1.88737914186277E-15));
#20943=CARTESIAN_POINT('Ctrl Pts',(37.5137497678178,-38.0454437403337,-1.22247208301798E-15));
#20944=CARTESIAN_POINT('Ctrl Pts',(37.6023731431382,-37.9585995914834,-1.41571360075421E-15));
#20945=CARTESIAN_POINT('Ctrl Pts',(37.6867792446409,-37.8680946551148,-1.63757896132211E-15));
#20946=CARTESIAN_POINT('Ctrl Pts',(37.7709936181979,-37.7777953001582,-1.85894035607411E-15));
#20947=CARTESIAN_POINT('Ctrl Pts',(37.8510103725839,-37.6838510649778,4.27670315709133E-16));
#20948=CARTESIAN_POINT('Ctrl Pts',(37.9265294316329,-37.5865486541875,7.49400541621981E-16));
#20949=CARTESIAN_POINT('Ctrl Pts',(38.0010161819357,-37.4905763199493,1.06673287208574E-15));
#20950=CARTESIAN_POINT('Ctrl Pts',(38.0711277582919,-37.3913363066692,-2.10142620498032E-15));
#20951=CARTESIAN_POINT('Ctrl Pts',(38.1365301844556,-37.2890828938187,-2.44249065417534E-15));
#20952=CARTESIAN_POINT('Ctrl Pts',(38.1898358473465,-37.2057421635956,-2.72047218512562E-15));
#20953=CARTESIAN_POINT('Ctrl Pts',(38.2400125268915,-37.1203991308186,-6.32482117348439E-16));
#20954=CARTESIAN_POINT('Ctrl Pts',(38.2868534572638,-37.0331856293588,-5.55111512312578E-16));
#20955=CARTESIAN_POINT('Ctrl Pts',(38.2987532893997,-37.0110292370944,-5.35455685563087E-16));
#20956=CARTESIAN_POINT('Ctrl Pts',(38.3104377056016,-36.9887521084602,-5.70989169773688E-17));
#20957=CARTESIAN_POINT('Ctrl Pts',(38.3219030525931,-36.9663563797929,-2.77555756156289E-17));
#20958=CARTESIAN_POINT('Ctrl Pts',(38.3300600637675,-36.9504229580542,-6.87928085047562E-18));
#20959=CARTESIAN_POINT('Ctrl Pts',(38.3381024804697,-36.9344366850298,-1.37102362174578E-15));
#20960=CARTESIAN_POINT('Ctrl Pts',(38.3460266349626,-36.9184039879293,-1.33226762955019E-15));
#20961=CARTESIAN_POINT('Ctrl Pts',(38.3989875306322,-36.8112498430667,-1.07324288929609E-15));
#20962=CARTESIAN_POINT('Ctrl Pts',(38.4467095755205,-36.7019458397232,2.38645293041498E-15));
#20963=CARTESIAN_POINT('Ctrl Pts',(38.4889139708526,-36.5907545955107,1.9151347174784E-15));
#20964=CARTESIAN_POINT('Ctrl Pts',(38.5302822088046,-36.4817662825029,1.45315430452751E-15));
#20965=CARTESIAN_POINT('Ctrl Pts',(38.5663495354543,-36.3709641352684,1.27266374069395E-15));
#20966=CARTESIAN_POINT('Ctrl Pts',(38.5968051838807,-36.2585816849604,1.52655665885959E-15));
#20967=CARTESIAN_POINT('Ctrl Pts',(38.6012594551821,-36.2421452618648,1.56368960455097E-15));
#20968=CARTESIAN_POINT('Ctrl Pts',(38.6055936009628,-36.2256750205659,1.48568813827467E-15));
#20969=CARTESIAN_POINT('Ctrl Pts',(38.6098065549286,-36.2091716785531,1.47104550762833E-15));
#20970=CARTESIAN_POINT('Ctrl Pts',(38.6394751128162,-36.092951477284,1.34152120378576E-15));
#20971=CARTESIAN_POINT('Ctrl Pts',(38.6631376928158,-35.9750893748381,9.72065328759131E-16));
#20972=CARTESIAN_POINT('Ctrl Pts',(38.6808851493713,-35.856021209443,1.41553435639707E-15));
#20973=CARTESIAN_POINT('Ctrl Pts',(38.6908686963668,-35.7890413229915,1.66500074413739E-15));
#20974=CARTESIAN_POINT('Ctrl Pts',(38.6989794822973,-35.7216798344703,1.48644827793188E-15));
#20975=CARTESIAN_POINT('Ctrl Pts',(38.7052266318381,-35.6540157826807,1.55431223447522E-15));
#20976=CARTESIAN_POINT('Ctrl Pts',(38.7081091139172,-35.6227950770761,1.58562517764618E-15));
#20977=CARTESIAN_POINT('Ctrl Pts',(38.7105947647117,-35.591509978624,7.00070747597251E-16));
#20978=CARTESIAN_POINT('Ctrl Pts',(38.7126841330784,-35.5601683863959,6.66133814775094E-16));
#20979=CARTESIAN_POINT('Ctrl Pts',(38.7138852254902,-35.5421513870013,6.46624860231182E-16));
#20980=CARTESIAN_POINT('Ctrl Pts',(38.7149548469422,-35.5241227721236,2.63074882680395E-16));
#20981=CARTESIAN_POINT('Ctrl Pts',(38.7158930667035,-35.5060923822785,2.77555756156289E-16));
#20982=CARTESIAN_POINT('Ctrl Pts',(38.7222040106739,-35.3848107969113,3.74961486578641E-16));
#20983=CARTESIAN_POINT('Ctrl Pts',(38.7225824292358,-35.263331928612,-1.41858650592555E-15));
#20984=CARTESIAN_POINT('Ctrl Pts',(38.717186529709,-35.1421030264707,-9.99200722162641E-16));
#20985=CARTESIAN_POINT('Ctrl Pts',(38.7119025633842,-35.0233889115555,-5.88514728574682E-16));
#20986=CARTESIAN_POINT('Ctrl Pts',(38.7010808603444,-34.9049135759813,2.80055440532142E-15));
#20987=CARTESIAN_POINT('Ctrl Pts',(38.6848166129475,-34.7871029976449,2.56739074444567E-15));
#20988=CARTESIAN_POINT('Ctrl Pts',(38.6687112711112,-34.6704434566446,2.3365051479245E-15));
#20989=CARTESIAN_POINT('Ctrl Pts',(38.6472688652681,-34.5544349100609,2.77413847088875E-15));
#20990=CARTESIAN_POINT('Ctrl Pts',(38.6205350417295,-34.4395098718885,3.02535774210355E-15));
#20991=CARTESIAN_POINT('Ctrl Pts',(38.6031281553353,-34.3646800563773,3.18893125068641E-15));
#20992=CARTESIAN_POINT('Ctrl Pts',(38.583477007896,-34.2903100135713,5.83132516188889E-16));
#20993=CARTESIAN_POINT('Ctrl Pts',(38.5615843988617,-34.2165260396906,2.91433543964104E-16));
#20994=CARTESIAN_POINT('Ctrl Pts',(38.5541960449916,-34.1916253022719,1.92990492842735E-16));
#20995=CARTESIAN_POINT('Ctrl Pts',(38.5465523399986,-34.1667913689833,-1.55624678416612E-15));
#20996=CARTESIAN_POINT('Ctrl Pts',(38.5386532038413,-34.1420292711584,-1.62370117351429E-15));
#20997=CARTESIAN_POINT('Ctrl Pts',(38.5335667843701,-34.1260844369365,-1.66713646980058E-15));
#20998=CARTESIAN_POINT('Ctrl Pts',(38.5283752457655,-34.1101719998602,9.92420310992954E-16));
#20999=CARTESIAN_POINT('Ctrl Pts',(38.5230814471938,-34.0943013261403,9.71445146547012E-16));
#21000=CARTESIAN_POINT('Ctrl Pts',(38.4861837828756,-33.9836830652666,8.25248693044116E-16));
#21001=CARTESIAN_POINT('Ctrl Pts',(38.4442854059965,-33.8749762815042,4.28212832527473E-15));
#21002=CARTESIAN_POINT('Ctrl Pts',(38.3974511090383,-33.7686001708186,3.23352455922077E-15));
#21003=CARTESIAN_POINT('Ctrl Pts',(38.359337050901,-33.6820305940251,2.38016393467622E-15));
#21004=CARTESIAN_POINT('Ctrl Pts',(38.3179530879923,-33.5970047635678,1.69064823388315E-15));
#21005=CARTESIAN_POINT('Ctrl Pts',(38.2733131581435,-33.5137642691618,1.70696790036118E-15));
#21006=CARTESIAN_POINT('Ctrl Pts',(38.251698175988,-33.473458609917,1.71487000282641E-15));
#21007=CARTESIAN_POINT('Ctrl Pts',(38.2293195396252,-33.4335717773559,1.04902033086069E-15));
#21008=CARTESIAN_POINT('Ctrl Pts',(38.2061773582038,-33.3941327240688,1.01307850997046E-15));
#21009=CARTESIAN_POINT('Ctrl Pts',(38.1925909929398,-33.3709787536688,9.91977702834968E-16));
#21010=CARTESIAN_POINT('Ctrl Pts',(38.1787393972074,-33.347976051224,-1.47665884113671E-16));
#21011=CARTESIAN_POINT('Ctrl Pts',(38.1646366459175,-33.3251529677485,-1.38777878078145E-17));
#21012=CARTESIAN_POINT('Ctrl Pts',(38.1062051944783,-33.230590859521,5.40441897174675E-16));
#21013=CARTESIAN_POINT('Ctrl Pts',(38.0434224756675,-33.1390339550006,1.08623518571526E-16));
#21014=CARTESIAN_POINT('Ctrl Pts',(37.9763225348264,-33.0508729636923,6.24500451351651E-16));
#21015=CARTESIAN_POINT('Ctrl Pts',(37.9162918094667,-32.9720000438309,1.08602792936337E-15));
#21016=CARTESIAN_POINT('Ctrl Pts',(37.8528049873413,-32.8958452375375,9.00746847309969E-16));
#21017=CARTESIAN_POINT('Ctrl Pts',(37.7858629582169,-32.8227148526165,3.72098185597025E-16));
#21018=CARTESIAN_POINT('Ctrl Pts',(37.7510080319419,-32.784637814794,1.2084137301326E-16));
#21019=CARTESIAN_POINT('Ctrl Pts',(37.7152160018646,-32.7473811866193,3.2434591796547E-16));
#21020=CARTESIAN_POINT('Ctrl Pts',(37.6785242770714,-32.7109603660126,2.77555756156289E-16));
#21021=CARTESIAN_POINT('Ctrl Pts',(37.6735319337713,-32.7141668369925,8.));
#21022=CARTESIAN_POINT('Ctrl Pts',(37.7506744257016,-32.7912795331857,8.));
#21023=CARTESIAN_POINT('Ctrl Pts',(37.8237045554225,-32.8720144016735,8.));
#21024=CARTESIAN_POINT('Ctrl Pts',(37.8926300182219,-32.9559529391151,8.));
#21025=CARTESIAN_POINT('Ctrl Pts',(37.9633153902931,-33.0420347223805,8.));
#21026=CARTESIAN_POINT('Ctrl Pts',(38.0296841818896,-33.1314863178634,8.));
#21027=CARTESIAN_POINT('Ctrl Pts',(38.0917148195566,-33.2239024768849,8.));
#21028=CARTESIAN_POINT('Ctrl Pts',(38.1550365108844,-33.3182421083212,8.));
#21029=CARTESIAN_POINT('Ctrl Pts',(38.2138380035849,-33.4156715766502,8.));
#21030=CARTESIAN_POINT('Ctrl Pts',(38.268059557232,-33.515799249106,8.));
#21031=CARTESIAN_POINT('Ctrl Pts',(38.3198487844224,-33.6114352910132,8.));
#21032=CARTESIAN_POINT('Ctrl Pts',(38.3674597504585,-33.7095337219438,8.));
#21033=CARTESIAN_POINT('Ctrl Pts',(38.410804885236,-33.8097778917925,8.));
#21034=CARTESIAN_POINT('Ctrl Pts',(38.4178421610283,-33.8260529794907,8.));
#21035=CARTESIAN_POINT('Ctrl Pts',(38.4247669147912,-33.8423846664997,8.));
#21036=CARTESIAN_POINT('Ctrl Pts',(38.4315786781863,-33.8587716403974,8.));
#21037=CARTESIAN_POINT('Ctrl Pts',(38.4380889335058,-33.8744332800934,8.));
#21038=CARTESIAN_POINT('Ctrl Pts',(38.4444929624372,-33.8901382301107,8.));
#21039=CARTESIAN_POINT('Ctrl Pts',(38.4507885504088,-33.9058798359799,8.));
#21040=CARTESIAN_POINT('Ctrl Pts',(38.4941738374283,-34.014361218793,8.));
#21041=CARTESIAN_POINT('Ctrl Pts',(38.5324452713943,-34.124659589853,8.));
#21042=CARTESIAN_POINT('Ctrl Pts',(38.5655742382515,-34.2363431431182,8.));
#21043=CARTESIAN_POINT('Ctrl Pts',(38.5991377517882,-34.3494916293961,8.));
#21044=CARTESIAN_POINT('Ctrl Pts',(38.6274234029538,-34.4640626260336,8.));
#21045=CARTESIAN_POINT('Ctrl Pts',(38.6503587972893,-34.5796396359417,8.));
#21046=CARTESIAN_POINT('Ctrl Pts',(38.6743337296149,-34.7004551296896,8.));
#21047=CARTESIAN_POINT('Ctrl Pts',(38.692463198861,-34.8223707151795,8.));
#21048=CARTESIAN_POINT('Ctrl Pts',(38.7046087858744,-34.9449340325394,8.));
#21049=CARTESIAN_POINT('Ctrl Pts',(38.7137179761345,-35.0368565205594,8.));
#21050=CARTESIAN_POINT('Ctrl Pts',(38.7194601094409,-35.1291439544571,8.));
#21051=CARTESIAN_POINT('Ctrl Pts',(38.721753661108,-35.2216089483748,8.));
#21052=CARTESIAN_POINT('Ctrl Pts',(38.7223012285573,-35.2436842395473,8.));
#21053=CARTESIAN_POINT('Ctrl Pts',(38.7226520798176,-35.2657741780712,8.));
#21054=CARTESIAN_POINT('Ctrl Pts',(38.7228050031224,-35.2878471504668,8.));
#21055=CARTESIAN_POINT('Ctrl Pts',(38.723639797835,-35.4083415425535,8.));
#21056=CARTESIAN_POINT('Ctrl Pts',(38.7185864406144,-35.528481112922,8.));
#21057=CARTESIAN_POINT('Ctrl Pts',(38.7075759731584,-35.6478398239672,8.));
#21058=CARTESIAN_POINT('Ctrl Pts',(38.6966361565965,-35.766432645673,8.));
#21059=CARTESIAN_POINT('Ctrl Pts',(38.6798156826268,-35.8842554734363,8.));
#21060=CARTESIAN_POINT('Ctrl Pts',(38.6569974768235,-36.0009032638125,8.));
#21061=CARTESIAN_POINT('Ctrl Pts',(38.6541238330716,-36.0155934720123,8.));
#21062=CARTESIAN_POINT('Ctrl Pts',(38.6511549977698,-36.0302650508608,8.));
#21063=CARTESIAN_POINT('Ctrl Pts',(38.6480906778903,-36.0449171950576,8.));
#21064=CARTESIAN_POINT('Ctrl Pts',(38.6241801879288,-36.1592459728997,8.));
#21065=CARTESIAN_POINT('Ctrl Pts',(38.5944604969197,-36.2723920187216,8.));
#21066=CARTESIAN_POINT('Ctrl Pts',(38.5592377490131,-36.3840888412668,8.));
#21067=CARTESIAN_POINT('Ctrl Pts',(38.5372725083531,-36.4537440423509,8.));
#21068=CARTESIAN_POINT('Ctrl Pts',(38.5131661119788,-36.5228355678477,8.));
#21069=CARTESIAN_POINT('Ctrl Pts',(38.4869829521143,-36.5912966040202,8.));
#21070=CARTESIAN_POINT('Ctrl Pts',(38.4780335436947,-36.614696597631,8.));
#21071=CARTESIAN_POINT('Ctrl Pts',(38.4688414510417,-36.6380229129432,8.));
#21072=CARTESIAN_POINT('Ctrl Pts',(38.4594090583389,-36.6612728133014,8.));
#21073=CARTESIAN_POINT('Ctrl Pts',(38.4526597990907,-36.677909059263,8.));
#21074=CARTESIAN_POINT('Ctrl Pts',(38.4457869585498,-36.6945073015523,8.));
#21075=CARTESIAN_POINT('Ctrl Pts',(38.4387984803451,-36.7110502346119,8.));
#21076=CARTESIAN_POINT('Ctrl Pts',(38.3928771569434,-36.8197539261443,8.));
#21077=CARTESIAN_POINT('Ctrl Pts',(38.3419028069428,-36.9262312105814,8.));
#21078=CARTESIAN_POINT('Ctrl Pts',(38.286233868877,-37.0302277419135,8.));
#21079=CARTESIAN_POINT('Ctrl Pts',(38.2286497374683,-37.1378020936858,8.));
#21080=CARTESIAN_POINT('Ctrl Pts',(38.1660422723199,-37.2427227531059,8.));
#21081=CARTESIAN_POINT('Ctrl Pts',(38.0987528117336,-37.3447008755076,8.));
#21082=CARTESIAN_POINT('Ctrl Pts',(38.0308301924039,-37.447638558876,8.));
#21083=CARTESIAN_POINT('Ctrl Pts',(37.9581366181552,-37.5475788135467,8.));
#21084=CARTESIAN_POINT('Ctrl Pts',(37.8809726402855,-37.6442062900679,8.));
#21085=CARTESIAN_POINT('Ctrl Pts',(37.8265596140724,-37.7123442160536,8.));
#21086=CARTESIAN_POINT('Ctrl Pts',(37.7699226008246,-37.7788344950898,8.));
#21087=CARTESIAN_POINT('Ctrl Pts',(37.7111539331996,-37.8435580680838,8.));
#21088=CARTESIAN_POINT('Ctrl Pts',(37.6849210722466,-37.8724490496109,8.));
#21089=CARTESIAN_POINT('Ctrl Pts',(37.6582633448569,-37.9009879055023,8.));
#21090=CARTESIAN_POINT('Ctrl Pts',(37.6311883528209,-37.9291634733987,8.));
#21091=CARTESIAN_POINT('Ctrl Pts',(37.6195660136439,-37.9412582509764,8.));
#21092=CARTESIAN_POINT('Ctrl Pts',(37.6078682053827,-37.9532845462101,8.));
#21093=CARTESIAN_POINT('Ctrl Pts',(37.5961020337617,-37.9652350938879,8.));
#21094=CARTESIAN_POINT('Ctrl Pts',(37.507659771091,-38.055063247923,8.));
#21095=CARTESIAN_POINT('Ctrl Pts',(37.415258178228,-38.1407187695167,8.));
#21096=CARTESIAN_POINT('Ctrl Pts',(37.3192259922681,-38.2218835091588,8.));
#21097=CARTESIAN_POINT('Ctrl Pts',(37.2371862486548,-38.2912220789739,8.));
#21098=CARTESIAN_POINT('Ctrl Pts',(37.152495821289,-38.3572831262055,8.));
#21099=CARTESIAN_POINT('Ctrl Pts',(37.0653354498859,-38.4198507239943,8.));
#21100=CARTESIAN_POINT('Ctrl Pts',(37.0262246732672,-38.4479261819266,8.));
#21101=CARTESIAN_POINT('Ctrl Pts',(36.9866162962358,-38.4752979774627,8.));
#21102=CARTESIAN_POINT('Ctrl Pts',(36.9465254062051,-38.5019452444609,8.));
#21103=CARTESIAN_POINT('Ctrl Pts',(36.9192921690604,-38.5200463976374,8.));
#21104=CARTESIAN_POINT('Ctrl Pts',(36.8918306415648,-38.5378166037371,8.));
#21105=CARTESIAN_POINT('Ctrl Pts',(36.8641755127457,-38.555230549143,8.));
#21106=CARTESIAN_POINT('Ctrl Pts',(36.7573712570443,-38.6224832996203,8.));
#21107=CARTESIAN_POINT('Ctrl Pts',(36.6476202687202,-38.6844692470865,8.));
#21108=CARTESIAN_POINT('Ctrl Pts',(36.5352245224892,-38.7408547353335,8.));
#21109=CARTESIAN_POINT('Ctrl Pts',(36.4331307539574,-38.7920720382892,8.));
#21110=CARTESIAN_POINT('Ctrl Pts',(36.3288540451722,-38.8386685245707,8.));
#21111=CARTESIAN_POINT('Ctrl Pts',(36.2225973607791,-38.8803650263204,8.));
#21112=CARTESIAN_POINT('Ctrl Pts',(36.1671668634624,-38.9021166727374,8.));
#21113=CARTESIAN_POINT('Ctrl Pts',(36.1111972101676,-38.9225343520043,8.));
#21114=CARTESIAN_POINT('Ctrl Pts',(36.054732523776,-38.9416301760088,8.));
#21115=CARTESIAN_POINT('Ctrl Pts',(31.4836965554877,-35.0029832498286,6.38741669750802));
#21116=CARTESIAN_POINT('Ctrl Pts',(31.4810524495825,-35.31689356108,6.4016107071645));
#21117=CARTESIAN_POINT('Ctrl Pts',(31.519709060091,-35.6301638289998,6.41580471682099));
#21118=CARTESIAN_POINT('Ctrl Pts',(31.6022835043847,-35.9313947240647,6.42999872647747));
#21119=CARTESIAN_POINT('Ctrl Pts',(31.9067358422351,-37.0420343537909,6.48233210226155));
#21120=CARTESIAN_POINT('Ctrl Pts',(32.8082072698223,-37.98901073323,6.53466547804564));
#21121=CARTESIAN_POINT('Ctrl Pts',(33.9025203486177,-38.3477577905554,6.58699885382972));
#21122=CARTESIAN_POINT('Ctrl Pts',(34.9968334274131,-38.7065048478808,6.6393322296138));
#21123=CARTESIAN_POINT('Ctrl Pts',(36.2839881574169,-38.4770225830925,6.69166560539789));
#21124=CARTESIAN_POINT('Ctrl Pts',(37.1868793172355,-37.7621695835158,6.74399898118197));
#21125=CARTESIAN_POINT('Ctrl Pts',(38.0897704770541,-37.0473165839391,6.79633235696606));
#21126=CARTESIAN_POINT('Ctrl Pts',(38.6083980666875,-35.847092849574,6.84866573275014));
#21127=CARTESIAN_POINT('Ctrl Pts',(38.5102394141138,-34.6996866784653,6.90099910853423));
#21128=CARTESIAN_POINT('Ctrl Pts',(38.41208076154,-33.5522805073566,6.95333248431831));
#21129=CARTESIAN_POINT('Ctrl Pts',(37.697135866759,-32.4576918995043,7.0056658601024));
#21130=CARTESIAN_POINT('Ctrl Pts',(36.6859406162159,-31.9065595295948,7.05799923588648));
#21131=CARTESIAN_POINT('Ctrl Pts',(35.6747453656728,-31.3554271596853,7.11033261167057));
#21132=CARTESIAN_POINT('Ctrl Pts',(34.3672997593676,-31.3477510277185,7.16266598745465));
#21133=CARTESIAN_POINT('Ctrl Pts',(33.3498296676148,-31.8872253835852,7.21499936323873));
#21134=CARTESIAN_POINT('Ctrl Pts',(32.332359575862,-32.426699739452,7.26733273902282));
#21135=CARTESIAN_POINT('Ctrl Pts',(31.6048649986616,-33.5133245831523,7.3196661148069));
#21136=CARTESIAN_POINT('Ctrl Pts',(31.4934685739382,-34.6593973074264,7.37199949059099));
#21137=CARTESIAN_POINT('Ctrl Pts',(31.4825295909021,-34.7719401481876,7.37713855956333));
#21138=CARTESIAN_POINT('Ctrl Pts',(31.4775316317653,-34.8850562438399,7.38227762853568));
#21139=CARTESIAN_POINT('Ctrl Pts',(31.478260520576,-34.9982347527286,7.38741669750802));
#21140=CARTESIAN_POINT('Ctrl Pts',(33.9479286229388,-38.9352951690526,8.));
#21141=CARTESIAN_POINT('Ctrl Pts',(32.6539236935135,-38.5893527455387,7.94766662421592));
#21142=CARTESIAN_POINT('Ctrl Pts',(30.4549361873396,-36.5273716142364,7.84299987264774));
#21143=CARTESIAN_POINT('Ctrl Pts',(31.2187010881653,-32.044211167377,7.68599974529549));
#21144=CARTESIAN_POINT('Ctrl Pts',(35.3795267558193,-30.2191465582126,7.52899961794324));
#21145=CARTESIAN_POINT('Ctrl Pts',(39.1969165266342,-32.6774422642514,7.37199949059099));
#21146=CARTESIAN_POINT('Ctrl Pts',(39.2524336251343,-37.2202141105436,7.21499936323873));
#21147=CARTESIAN_POINT('Ctrl Pts',(35.4939867861423,-39.7711972931265,7.05799923588648));
#21148=CARTESIAN_POINT('Ctrl Pts',(31.292957592828,-38.0442496611363,6.90099910853423));
#21149=CARTESIAN_POINT('Ctrl Pts',(30.4158800177777,-33.5872718945856,6.74399898118197));
#21150=CARTESIAN_POINT('Ctrl Pts',(33.6495206016122,-30.3972113452741,6.58699885382972));
#21151=CARTESIAN_POINT('Ctrl Pts',(38.09410244091,-31.3344607296745,6.42999872647747));
#21152=CARTESIAN_POINT('Ctrl Pts',(39.7641960678496,-35.558661561786,6.27299859912521));
#21153=CARTESIAN_POINT('Ctrl Pts',(37.1621778889461,-39.2818916953666,6.11599847177296));
#21154=CARTESIAN_POINT('Ctrl Pts',(32.6213197580022,-39.1655151793351,5.95899834442071));
#21155=CARTESIAN_POINT('Ctrl Pts',(30.2134441875202,-35.3138779065921,5.80199821706845));
#21156=CARTESIAN_POINT('Ctrl Pts',(32.0977205408613,-31.1807849590781,5.6449980897162));
#21157=CARTESIAN_POINT('Ctrl Pts',(36.584498029893,-30.4724179566463,5.48799796236395));
#21158=CARTESIAN_POINT('Ctrl Pts',(39.6504412814188,-33.8239776163473,5.33099783501169));
#21159=CARTESIAN_POINT('Ctrl Pts',(38.5462890493217,-38.2300876270061,5.17399770765944));
#21160=CARTESIAN_POINT('Ctrl Pts',(34.2621454906851,-39.7397471751372,5.01699758030718));
#21161=CARTESIAN_POINT('Ctrl Pts',(30.6396431067263,-36.9992299102556,4.85999745295493));
#21162=CARTESIAN_POINT('Ctrl Pts',(30.9271146014312,-32.4659840299328,4.70299732560268));
#21163=CARTESIAN_POINT('Ctrl Pts',(34.8667814960507,-30.2050145678827,4.54599719825042));
#21164=CARTESIAN_POINT('Ctrl Pts',(38.9259067064028,-32.2437545499559,4.38899707089817));
#21165=CARTESIAN_POINT('Ctrl Pts',(39.4646337070995,-36.7540462662356,4.23199694354592));
#21166=CARTESIAN_POINT('Ctrl Pts',(35.9998808321606,-39.6914678695931,4.07499681619366));
#21167=CARTESIAN_POINT('Ctrl Pts',(31.6385252219761,-38.4220052255121,3.91799668884141));
#21168=CARTESIAN_POINT('Ctrl Pts',(30.291436294066,-34.0839976670965,3.76099656148916));
#21169=CARTESIAN_POINT('Ctrl Pts',(33.1665616130745,-30.567378187653,3.6039964341369));
#21170=CARTESIAN_POINT('Ctrl Pts',(37.6857487228281,-31.0255332130596,3.44699630678465));
#21171=CARTESIAN_POINT('Ctrl Pts',(39.7965991870786,-35.0476307336073,3.28999617943239));
#21172=CARTESIAN_POINT('Ctrl Pts',(37.606293143399,-39.0270173223719,3.13299605208014));
#21173=CARTESIAN_POINT('Ctrl Pts',(33.0788990351993,-39.3953388367078,2.97599592472789));
#21174=CARTESIAN_POINT('Ctrl Pts',(30.2741745906988,-35.8223178652953,2.81899579737564));
#21175=CARTESIAN_POINT('Ctrl Pts',(31.7071431315558,-31.5119165427019,2.66199567002338));
#21176=CARTESIAN_POINT('Ctrl Pts',(36.092848009894,-30.329313184686,2.50499554267113));
#21177=CARTESIAN_POINT('Ctrl Pts',(39.4985856069267,-33.3349593710879,2.34799541531888));
#21178=CARTESIAN_POINT('Ctrl Pts',(38.8703983056154,-37.8336637277424,2.19099528796662));
#21179=CARTESIAN_POINT('Ctrl Pts',(34.7715877673847,-39.7913941019012,2.03399516061437));
#21180=CARTESIAN_POINT('Ctrl Pts',(30.8775965593863,-37.4526364914204,1.87699503326212));
#21181=CARTESIAN_POINT('Ctrl Pts',(30.6802042867265,-32.914574048659,1.71999490590986));
#21182=CARTESIAN_POINT('Ctrl Pts',(34.3564138261785,-30.2465374145616,1.56299477855761));
#21183=CARTESIAN_POINT('Ctrl Pts',(38.6097341605507,-31.8409675209513,1.40599465120535));
#21184=CARTESIAN_POINT('Ctrl Pts',(39.6261694334752,-36.2681500029269,1.2489945238531));
#21185=CARTESIAN_POINT('Ctrl Pts',(36.4942778376799,-39.5581346787212,1.09199439650085));
#21186=CARTESIAN_POINT('Ctrl Pts',(32.0224456319375,-38.7608678116187,0.934994269148595));
#21187=CARTESIAN_POINT('Ctrl Pts',(30.2206297689144,-34.5910506117954,0.777994141796339));
#21188=CARTESIAN_POINT('Ctrl Pts',(32.704491289799,-30.7882324000235,0.620994014444087));
#21189=CARTESIAN_POINT('Ctrl Pts',(37.2468174060219,-30.7615623188695,0.463993887091833));
#21190=CARTESIAN_POINT('Ctrl Pts',(39.7742801854456,-34.536716632844,0.306993759739581));
#21191=CARTESIAN_POINT('Ctrl Pts',(38.0208425645948,-38.7249309242138,0.149993632387326));
#21192=CARTESIAN_POINT('Ctrl Pts',(33.5581056824257,-39.5777559852671,-0.00700649496492666));
#21193=CARTESIAN_POINT('Ctrl Pts',(30.3892373827997,-36.3158028716181,-0.16400662231718));
#21194=CARTESIAN_POINT('Ctrl Pts',(31.0334355704763,-33.370922410012,-0.26867337388535));
#21195=CARTESIAN_POINT('Ctrl Pts',(31.9038714051976,-32.3528524834368,-0.321006749669435));
#21196=CARTESIAN_POINT('Ctrl Pts',(33.9957950511247,-38.756249785149,8.10700224988981));
#21197=CARTESIAN_POINT('Ctrl Pts',(32.7606638781546,-38.426046814806,8.05466887410573));
#21198=CARTESIAN_POINT('Ctrl Pts',(30.6617244103942,-36.4578802990271,7.95000212253756));
#21199=CARTESIAN_POINT('Ctrl Pts',(31.3907400550635,-32.1786916379746,7.79300199518531));
#21200=CARTESIAN_POINT('Ctrl Pts',(35.3622593055321,-30.4366625774945,7.63600186783305));
#21201=CARTESIAN_POINT('Ctrl Pts',(39.0059680720859,-32.7831124169518,7.4790017404808));
#21202=CARTESIAN_POINT('Ctrl Pts',(39.0589592913856,-37.1192003185169,7.32200161312853));
#21203=CARTESIAN_POINT('Ctrl Pts',(35.4715117112195,-39.554120602731,7.16500148577629));
#21204=CARTESIAN_POINT('Ctrl Pts',(31.4616180877658,-37.9057444599095,7.00800135842404));
#21205=CARTESIAN_POINT('Ctrl Pts',(30.6244451918799,-33.6515472373793,6.85100123107178));
#21206=CARTESIAN_POINT('Ctrl Pts',(33.7109637950579,-30.6066258939446,6.69400110371953));
#21207=CARTESIAN_POINT('Ctrl Pts',(37.9533290718052,-31.5012329431111,6.53700097636728));
#21208=CARTESIAN_POINT('Ctrl Pts',(39.5474379144414,-35.5332439578948,6.38000084901502));
#21209=CARTESIAN_POINT('Ctrl Pts',(37.0638045894695,-39.0870770983678,6.22300072166277));
#21210=CARTESIAN_POINT('Ctrl Pts',(32.729543334333,-38.9759954019356,6.06600059431052));
#21211=CARTESIAN_POINT('Ctrl Pts',(30.4312196493866,-35.2995973030108,5.90900046695826));
#21212=CARTESIAN_POINT('Ctrl Pts',(32.2297664783665,-31.3545490082375,5.752000339606));
#21213=CARTESIAN_POINT('Ctrl Pts',(36.5124076158656,-30.6784108060473,5.59500021225375));
#21214=CARTESIAN_POINT('Ctrl Pts',(39.4388586659392,-33.8774834831539,5.4380000849015));
#21215=CARTESIAN_POINT('Ctrl Pts',(38.3849424013594,-38.0831272963638,5.28099995754925));
#21216=CARTESIAN_POINT('Ctrl Pts',(34.2957158934656,-39.5241013808263,5.123999830197));
#21217=CARTESIAN_POINT('Ctrl Pts',(30.8380276599492,-36.9082703071214,4.96699970284474));
#21218=CARTESIAN_POINT('Ctrl Pts',(31.1124199720466,-32.581274965603,4.80999957549249));
#21219=CARTESIAN_POINT('Ctrl Pts',(34.8728425809651,-30.4231735548519,4.65299944814024));
#21220=CARTESIAN_POINT('Ctrl Pts',(38.7472884723895,-32.3691563314071,4.49599932078798));
#21221=CARTESIAN_POINT('Ctrl Pts',(39.2615048383014,-36.674241861831,4.33899919343573));
#21222=CARTESIAN_POINT('Ctrl Pts',(35.954388933901,-39.4780186542996,4.18199906608348));
#21223=CARTESIAN_POINT('Ctrl Pts',(31.7914633158823,-38.2663131584621,4.02499893873122));
#21224=CARTESIAN_POINT('Ctrl Pts',(30.5056633240975,-34.1256733184278,3.86799881137897));
#21225=CARTESIAN_POINT('Ctrl Pts',(33.2499781462058,-30.7690506010293,3.71099868402671));
#21226=CARTESIAN_POINT('Ctrl Pts',(37.5635543535394,-31.2063608006002,3.55399855667446));
#21227=CARTESIAN_POINT('Ctrl Pts',(39.5783667785835,-35.0454636628748,3.39699842932221));
#21228=CARTESIAN_POINT('Ctrl Pts',(37.4877137900394,-38.8437988263006,3.23999830196995));
#21229=CARTESIAN_POINT('Ctrl Pts',(33.1663039806949,-39.1953626988076,3.0829981746177));
#21230=CARTESIAN_POINT('Ctrl Pts',(30.4891869819735,-35.784904606173,2.92599804726545));
#21231=CARTESIAN_POINT('Ctrl Pts',(31.856959294467,-31.6706149922136,2.76899791991319));
#21232=CARTESIAN_POINT('Ctrl Pts',(36.0431263541924,-30.5418169177014,2.61199779256094));
#21233=CARTESIAN_POINT('Ctrl Pts',(39.2939120176749,-33.4107142575226,2.45499766520869));
#21234=CARTESIAN_POINT('Ctrl Pts',(38.6943055550796,-37.704739622131,2.29799753785643));
#21235=CARTESIAN_POINT('Ctrl Pts',(34.7819799118415,-39.5733985108324,2.14099741050418));
#21236=CARTESIAN_POINT('Ctrl Pts',(31.0651548682101,-37.3410481039379,1.98399728315193));
#21237=CARTESIAN_POINT('Ctrl Pts',(30.8767434149602,-33.0094553406639,1.82699715579967));
#21238=CARTESIAN_POINT('Ctrl Pts',(34.3856952723259,-30.4628072232849,1.66999702844742));
#21239=CARTESIAN_POINT('Ctrl Pts',(38.4455009300555,-31.9846950327841,1.51299690109516));
#21240=CARTESIAN_POINT('Ctrl Pts',(39.4156911220303,-36.2104525763381,1.35599677374291));
#21241=CARTESIAN_POINT('Ctrl Pts',(36.4262922006151,-39.3507517662898,1.19899664639066));
#21242=CARTESIAN_POINT('Ctrl Pts',(32.1579163760677,-38.5897584050265,1.04199651903841));
#21243=CARTESIAN_POINT('Ctrl Pts',(30.4380783060842,-34.6096567130058,0.884996391686151));
#21244=CARTESIAN_POINT('Ctrl Pts',(32.8089307843264,-30.9798565386092,0.727996264333898));
#21245=CARTESIAN_POINT('Ctrl Pts',(37.1445932353457,-30.9543998746739,0.570996136981644));
#21246=CARTESIAN_POINT('Ctrl Pts',(39.5570632317115,-34.5577947844858,0.413996009629391));
#21247=CARTESIAN_POINT('Ctrl Pts',(37.8834023235315,-38.5554565496905,0.256995882277137));
#21248=CARTESIAN_POINT('Ctrl Pts',(33.6237080097094,-39.3694803559713,0.0999957549248841));
#21249=CARTESIAN_POINT('Ctrl Pts',(30.5990147253931,-36.25593736721,-0.0570043724273687));
#21250=CARTESIAN_POINT('Ctrl Pts',(31.2139036219321,-33.4450410745538,-0.161671123995539));
#21251=CARTESIAN_POINT('Ctrl Pts',(32.0447369588746,-32.4732906012887,-0.214004499779624));
#21252=CARTESIAN_POINT('Ctrl Pts',(34.0436614793107,-38.5772044012455,8.21400449977962));
#21253=CARTESIAN_POINT('Ctrl Pts',(32.8674040627957,-38.2627408840732,8.16167112399554));
#21254=CARTESIAN_POINT('Ctrl Pts',(30.8685126334489,-36.3883889838178,8.05700437242737));
#21255=CARTESIAN_POINT('Ctrl Pts',(31.5627790219617,-32.3131721085722,7.90000424507511));
#21256=CARTESIAN_POINT('Ctrl Pts',(35.3449918552448,-30.6541785967763,7.74300411772285));
#21257=CARTESIAN_POINT('Ctrl Pts',(38.8150196175374,-32.8887825696523,7.58600399037061));
#21258=CARTESIAN_POINT('Ctrl Pts',(38.8654849576371,-37.0181865264902,7.42900386301835));
#21259=CARTESIAN_POINT('Ctrl Pts',(35.4490366362965,-39.3370439123355,7.2720037356661));
#21260=CARTESIAN_POINT('Ctrl Pts',(31.6302785827036,-37.7672392586828,7.11500360831385));
#21261=CARTESIAN_POINT('Ctrl Pts',(30.833010365982,-33.715822580173,6.95800348096159));
#21262=CARTESIAN_POINT('Ctrl Pts',(33.7724069885036,-30.8160404426151,6.80100335360934));
#21263=CARTESIAN_POINT('Ctrl Pts',(37.8125557027003,-31.6680051565476,6.64400322625708));
#21264=CARTESIAN_POINT('Ctrl Pts',(39.3306797610333,-35.5078263540035,6.48700309890484));
#21265=CARTESIAN_POINT('Ctrl Pts',(36.9654312899929,-38.892262501369,6.33000297155257));
#21266=CARTESIAN_POINT('Ctrl Pts',(32.8377669106638,-38.7864756245362,6.17300284420034));
#21267=CARTESIAN_POINT('Ctrl Pts',(30.6489951112531,-35.2853166994296,6.01600271684807));
#21268=CARTESIAN_POINT('Ctrl Pts',(32.3618124158715,-31.5283130573969,5.85900258949582));
#21269=CARTESIAN_POINT('Ctrl Pts',(36.4403172018384,-30.8844036554483,5.70200246214356));
#21270=CARTESIAN_POINT('Ctrl Pts',(39.2272760504595,-33.9309893499606,5.54500233479132));
#21271=CARTESIAN_POINT('Ctrl Pts',(38.2235957533972,-37.9361669657214,5.38800220743906));
#21272=CARTESIAN_POINT('Ctrl Pts',(34.3292862962461,-39.3084555865154,5.23100208008681));
#21273=CARTESIAN_POINT('Ctrl Pts',(31.0364122131721,-36.8173107039871,5.07400195273455));
#21274=CARTESIAN_POINT('Ctrl Pts',(31.2977253426618,-32.6965659012732,4.9170018253823));
#21275=CARTESIAN_POINT('Ctrl Pts',(34.8789036658794,-30.6413325418211,4.76000169803005));
#21276=CARTESIAN_POINT('Ctrl Pts',(38.5686702383762,-32.4945581128583,4.60300157067779));
#21277=CARTESIAN_POINT('Ctrl Pts',(39.0583759695033,-36.5944374574263,4.44600144332554));
#21278=CARTESIAN_POINT('Ctrl Pts',(35.9088970356414,-39.2645694390062,4.28900131597328));
#21279=CARTESIAN_POINT('Ctrl Pts',(31.9444014097886,-38.1106210914121,4.13200118862103));
#21280=CARTESIAN_POINT('Ctrl Pts',(30.7198903541289,-34.1673489697591,3.97500106126878));
#21281=CARTESIAN_POINT('Ctrl Pts',(33.333394679337,-30.9707230144056,3.81800093391652));
#21282=CARTESIAN_POINT('Ctrl Pts',(37.4413599842507,-31.3871883881407,3.66100080656427));
#21283=CARTESIAN_POINT('Ctrl Pts',(39.3601343700882,-35.0432965921423,3.50400067921202));
#21284=CARTESIAN_POINT('Ctrl Pts',(37.36913443668,-38.6605803302294,3.34700055185977));
#21285=CARTESIAN_POINT('Ctrl Pts',(33.2537089261905,-38.9953865609073,3.19000042450751));
#21286=CARTESIAN_POINT('Ctrl Pts',(30.7041993732481,-35.7474913470507,3.03300029715526));
#21287=CARTESIAN_POINT('Ctrl Pts',(32.006775457378,-31.8293134417253,2.876000169803));
#21288=CARTESIAN_POINT('Ctrl Pts',(35.9934046984909,-30.7543206507168,2.71900004245075));
#21289=CARTESIAN_POINT('Ctrl Pts',(39.0892384284232,-33.4864691439573,2.5619999150985));
#21290=CARTESIAN_POINT('Ctrl Pts',(38.5182128045439,-37.5758155165195,2.40499978774624));
#21291=CARTESIAN_POINT('Ctrl Pts',(34.7923720562983,-39.3554029197635,2.24799966039399));
#21292=CARTESIAN_POINT('Ctrl Pts',(31.2527131770338,-37.2294597164554,2.09099953304174));
#21293=CARTESIAN_POINT('Ctrl Pts',(31.073282543194,-33.1043366326688,1.93399940568948));
#21294=CARTESIAN_POINT('Ctrl Pts',(34.4149767184733,-30.6790770320082,1.77699927833723));
#21295=CARTESIAN_POINT('Ctrl Pts',(38.2812676995604,-32.1284225446167,1.61999915098497));
#21296=CARTESIAN_POINT('Ctrl Pts',(39.2052128105854,-36.1527551497494,1.46299902363272));
#21297=CARTESIAN_POINT('Ctrl Pts',(36.3583065635504,-39.1433688538583,1.30599889628047));
#21298=CARTESIAN_POINT('Ctrl Pts',(32.2933871201978,-38.4186489984343,1.14899876892821));
#21299=CARTESIAN_POINT('Ctrl Pts',(30.655526843254,-34.6282628142162,0.991998641575962));
#21300=CARTESIAN_POINT('Ctrl Pts',(32.9133702788538,-31.1714806771949,0.834998514223709));
#21301=CARTESIAN_POINT('Ctrl Pts',(37.0423690646695,-31.1472374304784,0.677998386871454));
#21302=CARTESIAN_POINT('Ctrl Pts',(39.3398462779774,-34.5788729361276,0.520998259519202));
#21303=CARTESIAN_POINT('Ctrl Pts',(37.7459620824681,-38.385982175167,0.363998132166948));
#21304=CARTESIAN_POINT('Ctrl Pts',(33.6893103369932,-39.1612047266757,0.206998004814695));
#21305=CARTESIAN_POINT('Ctrl Pts',(30.8087920679866,-36.1960718628018,0.0499978774624421));
#21306=CARTESIAN_POINT('Ctrl Pts',(31.3943716733879,-33.5191597390956,-0.0546688741057282));
#21307=CARTESIAN_POINT('Ctrl Pts',(32.1856025125517,-32.5937287191406,-0.107002249889813));
#21308=CARTESIAN_POINT('Ctrl Pts',(34.0915279074966,-38.398159017342,8.32100674966943));
#21309=CARTESIAN_POINT('Ctrl Pts',(32.9741442474368,-38.0994349533405,8.26867337388535));
#21310=CARTESIAN_POINT('Ctrl Pts',(31.0753008565035,-36.3188976686085,8.16400662231718));
#21311=CARTESIAN_POINT('Ctrl Pts',(31.73481798886,-32.4476525791699,8.00700649496493));
#21312=CARTESIAN_POINT('Ctrl Pts',(35.3277244049576,-30.8716946160581,7.85000636761267));
#21313=CARTESIAN_POINT('Ctrl Pts',(38.6240711629891,-32.9944527223528,7.69300624026043));
#21314=CARTESIAN_POINT('Ctrl Pts',(38.6720106238885,-36.9171727344635,7.53600611290815));
#21315=CARTESIAN_POINT('Ctrl Pts',(35.4265615613737,-39.1199672219399,7.37900598555592));
#21316=CARTESIAN_POINT('Ctrl Pts',(31.7989390776415,-37.628734057456,7.22200585820365));
#21317=CARTESIAN_POINT('Ctrl Pts',(31.0415755400842,-33.7800979229667,7.06500573085141));
#21318=CARTESIAN_POINT('Ctrl Pts',(33.8338501819494,-31.0254549912856,6.90800560349915));
#21319=CARTESIAN_POINT('Ctrl Pts',(37.6717823335954,-31.8347773699841,6.75100547614689));
#21320=CARTESIAN_POINT('Ctrl Pts',(39.1139216076251,-35.4824087501123,6.59400534879465));
#21321=CARTESIAN_POINT('Ctrl Pts',(36.8670579905162,-38.6974479043702,6.43700522144239));
#21322=CARTESIAN_POINT('Ctrl Pts',(32.9459904869947,-38.5969558471367,6.28000509409014));
#21323=CARTESIAN_POINT('Ctrl Pts',(30.8667705731195,-35.2710360958482,6.12300496673788));
#21324=CARTESIAN_POINT('Ctrl Pts',(32.4938583533767,-31.7020771065563,5.96600483938563));
#21325=CARTESIAN_POINT('Ctrl Pts',(36.3682267878111,-31.0903965048492,5.80900471203338));
#21326=CARTESIAN_POINT('Ctrl Pts',(39.0156934349799,-33.9844952167673,5.65200458468112));
#21327=CARTESIAN_POINT('Ctrl Pts',(38.0622491054349,-37.789206635079,5.49500445732887));
#21328=CARTESIAN_POINT('Ctrl Pts',(34.3628566990267,-39.0928097922045,5.33800432997662));
#21329=CARTESIAN_POINT('Ctrl Pts',(31.234796766395,-36.7263511008529,5.18100420262436));
#21330=CARTESIAN_POINT('Ctrl Pts',(31.4830307132771,-32.8118568369433,5.02400407527211));
#21331=CARTESIAN_POINT('Ctrl Pts',(34.8849647507938,-30.8594915287904,4.86700394791986));
#21332=CARTESIAN_POINT('Ctrl Pts',(38.3900520043628,-32.6199598943095,4.7100038205676));
#21333=CARTESIAN_POINT('Ctrl Pts',(38.8552471007052,-36.5146330530217,4.55300369321535));
#21334=CARTESIAN_POINT('Ctrl Pts',(35.8634051373818,-39.0511202237127,4.39600356586309));
#21335=CARTESIAN_POINT('Ctrl Pts',(32.0973395036949,-37.9549290243621,4.23900343851084));
#21336=CARTESIAN_POINT('Ctrl Pts',(30.9341173841603,-34.2090246210904,4.08200331115859));
#21337=CARTESIAN_POINT('Ctrl Pts',(33.4168112124683,-31.1723954277819,3.92500318380634));
#21338=CARTESIAN_POINT('Ctrl Pts',(37.319165614962,-31.5680159756812,3.76800305645408));
#21339=CARTESIAN_POINT('Ctrl Pts',(39.141901961593,-35.0411295214099,3.61100292910183));
#21340=CARTESIAN_POINT('Ctrl Pts',(37.2505550833205,-38.4773618341581,3.45400280174957));
#21341=CARTESIAN_POINT('Ctrl Pts',(33.3411138716861,-38.7954104230071,3.29700267439732));
#21342=CARTESIAN_POINT('Ctrl Pts',(30.9192117645227,-35.7100780879284,3.14000254704507));
#21343=CARTESIAN_POINT('Ctrl Pts',(32.1565916202891,-31.988011891237,2.98300241969282));
#21344=CARTESIAN_POINT('Ctrl Pts',(35.9436830427893,-30.9668243837322,2.82600229234056));
#21345=CARTESIAN_POINT('Ctrl Pts',(38.8845648391714,-33.5622240303919,2.66900216498831));
#21346=CARTESIAN_POINT('Ctrl Pts',(38.3421200540082,-37.4468914109081,2.51200203763606));
#21347=CARTESIAN_POINT('Ctrl Pts',(34.802764200755,-39.1374073286946,2.3550019102838));
#21348=CARTESIAN_POINT('Ctrl Pts',(31.4402714858577,-37.1178713289729,2.19800178293155));
#21349=CARTESIAN_POINT('Ctrl Pts',(31.2698216714276,-33.1992179246737,2.04100165557929));
#21350=CARTESIAN_POINT('Ctrl Pts',(34.4442581646208,-30.8953468407316,1.88400152822704));
#21351=CARTESIAN_POINT('Ctrl Pts',(38.1170344690652,-32.2721500564494,1.72700140087478));
#21352=CARTESIAN_POINT('Ctrl Pts',(38.9947344991405,-36.0950577231607,1.57000127352253));
#21353=CARTESIAN_POINT('Ctrl Pts',(36.2903209264856,-38.9359859414268,1.41300114617028));
#21354=CARTESIAN_POINT('Ctrl Pts',(32.428857864328,-38.247539591842,1.25600101881803));
#21355=CARTESIAN_POINT('Ctrl Pts',(30.8729753804238,-34.6468689154266,1.09900089146577));
#21356=CARTESIAN_POINT('Ctrl Pts',(33.0178097733811,-31.3631048157807,0.942000764113519));
#21357=CARTESIAN_POINT('Ctrl Pts',(36.9401448939934,-31.3400749862829,0.785000636761266));
#21358=CARTESIAN_POINT('Ctrl Pts',(39.1226293242432,-34.5999510877694,0.628000509409013));
#21359=CARTESIAN_POINT('Ctrl Pts',(37.6085218414048,-38.2165078006437,0.471000382056759));
#21360=CARTESIAN_POINT('Ctrl Pts',(33.754912664277,-38.9529290973799,0.314000254704506));
#21361=CARTESIAN_POINT('Ctrl Pts',(31.0185694105801,-36.1362063583937,0.157000127352253));
#21362=CARTESIAN_POINT('Ctrl Pts',(31.5748397248436,-33.5932784036374,0.0523333757840826));
#21363=CARTESIAN_POINT('Ctrl Pts',(32.3264680662287,-32.7141668369925,-2.22044604925031E-15));
#21364=CARTESIAN_POINT('Ctrl Pts',(32.3264680662287,-32.7141668369925,-2.27595720048157E-15));
#21365=CARTESIAN_POINT('Ctrl Pts',(32.2493253090815,-32.7912797983002,-2.16394166852401E-15));
#21366=CARTESIAN_POINT('Ctrl Pts',(32.1762949026186,-32.8720149145437,3.46363794187806E-16));
#21367=CARTESIAN_POINT('Ctrl Pts',(32.1073691591848,-32.9559536860909,1.66533453693773E-16));
#21368=CARTESIAN_POINT('Ctrl Pts',(32.0366835341849,-33.0420356669728,-1.78884963425382E-17));
#21369=CARTESIAN_POINT('Ctrl Pts',(31.9703144812951,-33.1314874423946,-2.24888209125886E-15));
#21370=CARTESIAN_POINT('Ctrl Pts',(31.9082835820817,-33.2239037683368,-2.33146835171283E-15));
#21371=CARTESIAN_POINT('Ctrl Pts',(31.8449616802408,-33.3182434860262,-2.41577341812641E-15));
#21372=CARTESIAN_POINT('Ctrl Pts',(31.7861599686898,-33.4156730215343,-2.34515801197777E-15));
#21373=CARTESIAN_POINT('Ctrl Pts',(31.7319381963941,-33.5158007480848,-2.77555756156289E-15));
#21374=CARTESIAN_POINT('Ctrl Pts',(31.6801489223982,-33.611436542441,-3.18664851741706E-15));
#21375=CARTESIAN_POINT('Ctrl Pts',(31.6325378836028,-33.7095346984804,-3.69832300465041E-15));
#21376=CARTESIAN_POINT('Ctrl Pts',(31.5891926568309,-33.8097785742014,-3.99680288865056E-15));
#21377=CARTESIAN_POINT('Ctrl Pts',(31.5821541452564,-33.8260564375806,-4.04527083482939E-15));
#21378=CARTESIAN_POINT('Ctrl Pts',(31.5752281942475,-33.8423909194022,-5.19848407519141E-15));
#21379=CARTESIAN_POINT('Ctrl Pts',(31.568415272417,-33.8587807065962,-5.21804821573824E-15));
#21380=CARTESIAN_POINT('Ctrl Pts',(31.561906348996,-33.8744391674425,-5.23673938757109E-15));
#21381=CARTESIAN_POINT('Ctrl Pts',(31.5555036120846,-33.8901409126424,-5.57046258471252E-15));
#21382=CARTESIAN_POINT('Ctrl Pts',(31.5492092706946,-33.9058793019477,-5.49560397189452E-15));
#21383=CARTESIAN_POINT('Ctrl Pts',(31.5058237133564,-34.0143606742329,-4.97961946494936E-15));
#21384=CARTESIAN_POINT('Ctrl Pts',(31.4675520206245,-34.1246590298884,-6.38605598306829E-15));
#21385=CARTESIAN_POINT('Ctrl Pts',(31.4344228151864,-34.2363425690307,-5.19029264012261E-15));
#21386=CARTESIAN_POINT('Ctrl Pts',(31.4008590997118,-34.3494909069217,-3.9788461207494E-15));
#21387=CARTESIAN_POINT('Ctrl Pts',(31.3725732548101,-34.4640617531158,-1.67269218670119E-15));
#21388=CARTESIAN_POINT('Ctrl Pts',(31.3496376837557,-34.5796386183165,-1.85962356624714E-15));
#21389=CARTESIAN_POINT('Ctrl Pts',(31.3256626239872,-34.7004536721242,-2.05502707229468E-15));
#21390=CARTESIAN_POINT('Ctrl Pts',(31.3075330179638,-34.8223688186784,-6.90474885500916E-16));
#21391=CARTESIAN_POINT('Ctrl Pts',(31.2953872940185,-34.9449317101526,1.11022302462516E-16));
#21392=CARTESIAN_POINT('Ctrl Pts',(31.2862780010595,-35.0368538787582,7.12145193435089E-16));
#21393=CARTESIAN_POINT('Ctrl Pts',(31.2805357649583,-35.1291410005731,-7.33619512718545E-16));
#21394=CARTESIAN_POINT('Ctrl Pts',(31.2782421142109,-35.2216056948398,-3.88578058618805E-16));
#21395=CARTESIAN_POINT('Ctrl Pts',(31.2776945327762,-35.2436805246709,-3.0620357564075E-16));
#21396=CARTESIAN_POINT('Ctrl Pts',(31.2773436607928,-35.2657700018002,-4.90649572448904E-16));
#21397=CARTESIAN_POINT('Ctrl Pts',(31.2771907100455,-35.287842514156,-5.27355936696949E-16));
#21398=CARTESIAN_POINT('Ctrl Pts',(31.2763557493203,-35.4083367336975,-7.27736602069211E-16));
#21399=CARTESIAN_POINT('Ctrl Pts',(31.2814089690861,-35.5284761575602,-1.32546033095374E-15));
#21400=CARTESIAN_POINT('Ctrl Pts',(31.2924193361456,-35.6478347566642,-1.0547118733939E-15));
#21401=CARTESIAN_POINT('Ctrl Pts',(31.3033590399359,-35.7664273260093,-7.85701048289603E-16));
#21402=CARTESIAN_POINT('Ctrl Pts',(31.3201794237171,-35.8842499373544,-3.19095490877261E-16));
#21403=CARTESIAN_POINT('Ctrl Pts',(31.3429975699143,-36.0008975571309,1.94289029309402E-16));
#21404=CARTESIAN_POINT('Ctrl Pts',(31.3458712257766,-36.0155878441288,2.58943292776536E-16));
#21405=CARTESIAN_POINT('Ctrl Pts',(31.3488400749734,-36.030259502248,-2.41414676176044E-15));
#21406=CARTESIAN_POINT('Ctrl Pts',(31.3519044105546,-36.0449117261916,-2.44249065417534E-15));
#21407=CARTESIAN_POINT('Ctrl Pts',(31.375814852164,-36.1592403092631,-2.71916393553799E-15));
#21408=CARTESIAN_POINT('Ctrl Pts',(31.4055345217229,-36.272386206175,5.65793814005205E-16));
#21409=CARTESIAN_POINT('Ctrl Pts',(31.4407572695548,-36.384082920097,4.44089209850063E-16));
#21410=CARTESIAN_POINT('Ctrl Pts',(31.4627225424769,-36.453738155898,3.68192949317207E-16));
#21411=CARTESIAN_POINT('Ctrl Pts',(31.4868289857256,-36.52282973013,-1.13814971295829E-15));
#21412=CARTESIAN_POINT('Ctrl Pts',(31.513012205469,-36.5912908274846,-1.69309011255336E-15));
#21413=CARTESIAN_POINT('Ctrl Pts',(31.5219624105717,-36.6146928715758,-1.88278528544959E-15));
#21414=CARTESIAN_POINT('Ctrl Pts',(31.531155343526,-36.6380212260425,4.03667916851762E-15));
#21415=CARTESIAN_POINT('Ctrl Pts',(31.5405886194687,-36.6612731534534,4.32986979603811E-15));
#21416=CARTESIAN_POINT('Ctrl Pts',(31.5473370498667,-36.6779072490427,4.53961416853196E-15));
#21417=CARTESIAN_POINT('Ctrl Pts',(31.5542090296369,-36.6945033501966,3.07759665647771E-15));
#21418=CARTESIAN_POINT('Ctrl Pts',(31.561196617679,-36.7110441569158,2.94209101525666E-15));
#21419=CARTESIAN_POINT('Ctrl Pts',(31.6071179522689,-36.8197477489354,2.0515691568155E-15));
#21420=CARTESIAN_POINT('Ctrl Pts',(31.6580923235038,-36.9262249725842,4.21341387307547E-15));
#21421=CARTESIAN_POINT('Ctrl Pts',(31.7137612878297,-37.0302214764794,3.42781358853017E-15));
#21422=CARTESIAN_POINT('Ctrl Pts',(31.7713455134326,-37.1377959250922,2.61518514166327E-15));
#21423=CARTESIAN_POINT('Ctrl Pts',(31.8339530898433,-37.2427167108642,9.07249106506457E-16));
#21424=CARTESIAN_POINT('Ctrl Pts',(31.9012426720394,-37.3446949826671,6.80011602582908E-16));
#21425=CARTESIAN_POINT('Ctrl Pts',(31.9691654564611,-37.4476328810058,4.50635769240332E-16));
#21426=CARTESIAN_POINT('Ctrl Pts',(32.0418592122967,-37.5475733704053,-1.57902851375934E-15));
#21427=CARTESIAN_POINT('Ctrl Pts',(32.1190233809196,-37.6442010945393,-1.81799020282369E-15));
#21428=CARTESIAN_POINT('Ctrl Pts',(32.1734366012044,-37.712339269715,-1.98649684598102E-15));
#21429=CARTESIAN_POINT('Ctrl Pts',(32.2300738179544,-37.7788298007494,1.23701449661782E-16));
#21430=CARTESIAN_POINT('Ctrl Pts',(32.2888426956766,-37.8435536257978,-3.88578058618805E-16));
#21431=CARTESIAN_POINT('Ctrl Pts',(32.3150744390812,-37.8724433857632,-6.17236238483284E-16));
#21432=CARTESIAN_POINT('Ctrl Pts',(32.3417310110036,-37.9009810526196,1.30430196317008E-16));
#21433=CARTESIAN_POINT('Ctrl Pts',(32.3688048104485,-37.9291554653168,-2.77555756156289E-17));
#21434=CARTESIAN_POINT('Ctrl Pts',(32.3804263297313,-37.9412494265322,-9.56573491554205E-17));
#21435=CARTESIAN_POINT('Ctrl Pts',(32.392123309834,-37.9532749179279,-6.28475541027777E-16));
#21436=CARTESIAN_POINT('Ctrl Pts',(32.4038886430803,-37.9652246721857,-5.96744875736022E-16));
#21437=CARTESIAN_POINT('Ctrl Pts',(32.4923309120516,-38.05505326931,-3.5821937240873E-16));
#21438=CARTESIAN_POINT('Ctrl Pts',(32.5847325176906,-38.1407092470896,2.11600168392725E-15));
#21439=CARTESIAN_POINT('Ctrl Pts',(32.6807647145451,-38.221874449736,1.96370697480575E-15));
#21440=CARTESIAN_POINT('Ctrl Pts',(32.7628051861864,-38.2912140225467,1.8336013417573E-15));
#21441=CARTESIAN_POINT('Ctrl Pts',(32.8474963866317,-38.3572760203649,1.20960812321559E-15));
#21442=CARTESIAN_POINT('Ctrl Pts',(32.9346575664231,-38.4198445069104,5.62050406216485E-16));
#21443=CARTESIAN_POINT('Ctrl Pts',(32.973768957553,-38.4479205443796,2.71475138541893E-16));
#21444=CARTESIAN_POINT('Ctrl Pts',(33.0133779626213,-38.4752928979382,3.47992543175087E-15));
#21445=CARTESIAN_POINT('Ctrl Pts',(33.0534694930906,-38.5019407001488,3.78169717762944E-15));
#21446=CARTESIAN_POINT('Ctrl Pts',(33.0807047104967,-38.5200432439556,3.98669855846499E-15));
#21447=CARTESIAN_POINT('Ctrl Pts',(33.108168250427,-38.5378147929466,1.27528005472796E-15));
#21448=CARTESIAN_POINT('Ctrl Pts',(33.1358254185318,-38.5552300293176,1.47104550762833E-15));
#21449=CARTESIAN_POINT('Ctrl Pts',(33.2426299049644,-38.6224829515854,2.22703862229035E-15));
#21450=CARTESIAN_POINT('Ctrl Pts',(33.3523811032195,-38.6844690524263,5.56024339803508E-15));
#21451=CARTESIAN_POINT('Ctrl Pts',(33.4647770313827,-38.7408546683214,3.76781938982163E-15));
#21452=CARTESIAN_POINT('Ctrl Pts',(33.5668706528472,-38.7920719305417,2.13969049592827E-15));
#21453=CARTESIAN_POINT('Ctrl Pts',(33.6711471781243,-38.8386683831236,1.86420798495096E-15));
#21454=CARTESIAN_POINT('Ctrl Pts',(33.7774036389012,-38.880364855251,2.14498557804532E-15));
#21455=CARTESIAN_POINT('Ctrl Pts',(33.8328341927383,-38.9021165541705,2.26717202503918E-15));
#21456=CARTESIAN_POINT('Ctrl Pts',(33.8888038950002,-38.9225342787199,1.50877474080585E-16));
#21457=CARTESIAN_POINT('Ctrl Pts',(33.94526862329,-38.9416301412996,1.94289029309402E-16));
#21458=CARTESIAN_POINT('Ctrl Pts',(31.4846885160394,-34.9971888045819,7.11258330249198));
#21459=CARTESIAN_POINT('Ctrl Pts',(31.4819573643756,-34.6461972356202,7.09672411194512));
#21460=CARTESIAN_POINT('Ctrl Pts',(31.5304047798457,-34.2959415119622,7.08086492139826));
#21461=CARTESIAN_POINT('Ctrl Pts',(31.6331819033213,-33.9624301234347,7.0650057308514));
#21462=CARTESIAN_POINT('Ctrl Pts',(31.9723337540393,-32.8618836124063,7.01267235506732));
#21463=CARTESIAN_POINT('Ctrl Pts',(32.9030919679943,-31.943669301846,6.96033897928324));
#21464=CARTESIAN_POINT('Ctrl Pts',(34.0081264335795,-31.6194492096822,6.90800560349915));
#21465=CARTESIAN_POINT('Ctrl Pts',(35.1131608991647,-31.2952291175184,6.85567222771506));
#21466=CARTESIAN_POINT('Ctrl Pts',(36.3924716163801,-31.5650032437512,6.80333885193098));
#21467=CARTESIAN_POINT('Ctrl Pts',(37.2724835206594,-32.3078288702224,6.75100547614689));
#21468=CARTESIAN_POINT('Ctrl Pts',(38.1524954249387,-33.0506544966935,6.69867210036281));
#21469=CARTESIAN_POINT('Ctrl Pts',(38.6332085162819,-34.2665316234029,6.64633872457873));
#21470=CARTESIAN_POINT('Ctrl Pts',(38.4990877924354,-35.4103100458006,6.59400534879464));
#21471=CARTESIAN_POINT('Ctrl Pts',(38.3649670685888,-36.5540884681983,6.54167197301056));
#21472=CARTESIAN_POINT('Ctrl Pts',(37.6160125295525,-37.6257681862843,6.48933859722647));
#21473=CARTESIAN_POINT('Ctrl Pts',(36.5880240094475,-38.1448593691216,6.43700522144239));
#21474=CARTESIAN_POINT('Ctrl Pts',(35.5600354893424,-38.663950551959,6.3846718456583));
#21475=CARTESIAN_POINT('Ctrl Pts',(34.2530129881685,-38.6304531995479,6.33233846987422));
#21476=CARTESIAN_POINT('Ctrl Pts',(33.2529650852691,-38.0593845647942,6.28000509409014));
#21477=CARTESIAN_POINT('Ctrl Pts',(32.2529171823696,-37.4883159300405,6.22767171830605));
#21478=CARTESIAN_POINT('Ctrl Pts',(31.5598438777445,-36.3796760129444,6.17533834252196));
#21479=CARTESIAN_POINT('Ctrl Pts',(31.4844885221415,-35.230529556181,6.12300496673788));
#21480=CARTESIAN_POINT('Ctrl Pts',(31.4794864356562,-35.1542492451791,6.11953107865591));
#21481=CARTESIAN_POINT('Ctrl Pts',(31.4772062002897,-35.0777904501775,6.11605719057394));
#21482=CARTESIAN_POINT('Ctrl Pts',(31.4775766908735,-35.0013091813966,6.11258330249198));
#21483=CARTESIAN_POINT('Ctrl Pts',(33.9479286229388,-38.9352951690526,8.));
#21484=CARTESIAN_POINT('Ctrl Pts',(33.8318204065611,-38.8956804683211,8.));
#21485=CARTESIAN_POINT('Ctrl Pts',(33.7179772526967,-38.8505153756638,8.));
#21486=CARTESIAN_POINT('Ctrl Pts',(33.6066250571068,-38.8001574942087,8.));
#21487=CARTESIAN_POINT('Ctrl Pts',(33.4927757454994,-38.7486703178014,8.));
#21488=CARTESIAN_POINT('Ctrl Pts',(33.3815297429693,-38.6917543422691,8.));
#21489=CARTESIAN_POINT('Ctrl Pts',(33.2731527586738,-38.6297431972011,8.));
#21490=CARTESIAN_POINT('Ctrl Pts',(33.1592144063828,-38.5645499484809,8.));
#21491=CARTESIAN_POINT('Ctrl Pts',(33.0484461029789,-38.4937247712042,8.));
#21492=CARTESIAN_POINT('Ctrl Pts',(32.9411957572322,-38.4176091405434,8.));
#21493=CARTESIAN_POINT('Ctrl Pts',(32.8473517047039,-38.3510079637152,8.));
#21494=CARTESIAN_POINT('Ctrl Pts',(32.7562013929947,-38.2803552258207,8.));
#21495=CARTESIAN_POINT('Ctrl Pts',(32.668009391503,-38.2058575466902,8.));
#21496=CARTESIAN_POINT('Ctrl Pts',(32.6506323829748,-38.1911788141103,8.));
#21497=CARTESIAN_POINT('Ctrl Pts',(32.6333703275703,-38.1763507567444,8.));
#21498=CARTESIAN_POINT('Ctrl Pts',(32.6162254037543,-38.1613748841763,8.));
#21499=CARTESIAN_POINT('Ctrl Pts',(32.603691142847,-38.1504263669302,8.));
#21500=CARTESIAN_POINT('Ctrl Pts',(32.5912206997708,-38.139399841404,8.));
#21501=CARTESIAN_POINT('Ctrl Pts',(32.5788237219142,-38.1283040179759,8.));
#21502=CARTESIAN_POINT('Ctrl Pts',(32.4862445714949,-38.0454417334689,8.));
#21503=CARTESIAN_POINT('Ctrl Pts',(32.3976212761744,-37.9585977539474,8.));
#21504=CARTESIAN_POINT('Ctrl Pts',(32.3132152636303,-37.8680929905958,8.));
#21505=CARTESIAN_POINT('Ctrl Pts',(32.2290010683149,-37.7777939042141,8.));
#21506=CARTESIAN_POINT('Ctrl Pts',(32.1489844921721,-37.6838499490402,8.));
#21507=CARTESIAN_POINT('Ctrl Pts',(32.0734656135458,-37.5865478166696,8.));
#21508=CARTESIAN_POINT('Ctrl Pts',(31.9989790801238,-37.4905758071975,8.));
#21509=CARTESIAN_POINT('Ctrl Pts',(31.9288677181994,-37.3913361205739,8.));
#21510=CARTESIAN_POINT('Ctrl Pts',(31.8634655056288,-37.2890830233624,8.));
#21511=CARTESIAN_POINT('Ctrl Pts',(31.8101602412414,-37.2057429012617,8.));
#21512=CARTESIAN_POINT('Ctrl Pts',(31.7599839333137,-37.1204004861509,8.));
#21513=CARTESIAN_POINT('Ctrl Pts',(31.7131433458597,-37.0331876031136,8.));
#21514=CARTESIAN_POINT('Ctrl Pts',(31.7012416847729,-37.011027800414,8.));
#21515=CARTESIAN_POINT('Ctrl Pts',(31.6895555071392,-36.9887472225083,8.));
#21516=CARTESIAN_POINT('Ctrl Pts',(31.6780884679743,-36.9663480066189,8.));
#21517=CARTESIAN_POINT('Ctrl Pts',(31.6699335871488,-36.9504186168665,8.));
#21518=CARTESIAN_POINT('Ctrl Pts',(31.6618932487394,-36.9344364128785,8.));
#21519=CARTESIAN_POINT('Ctrl Pts',(31.6539711105215,-36.918407803011,8.));
#21520=CARTESIAN_POINT('Ctrl Pts',(31.6010103294039,-36.8112539418358,8.));
#21521=CARTESIAN_POINT('Ctrl Pts',(31.553288398372,-36.7019501913722,8.));
#21522=CARTESIAN_POINT('Ctrl Pts',(31.5110841176717,-36.5907591572156,8.));
#21523=CARTESIAN_POINT('Ctrl Pts',(31.4697159940302,-36.4817710552385,8.));
#21524=CARTESIAN_POINT('Ctrl Pts',(31.433648781936,-36.3709690780795,8.));
#21525=CARTESIAN_POINT('Ctrl Pts',(31.4031932495943,-36.2585867452464,8.));
#21526=CARTESIAN_POINT('Ctrl Pts',(31.3987391935523,-36.2421510709998,8.));
#21527=CARTESIAN_POINT('Ctrl Pts',(31.3944052523692,-36.2256815804349,8.));
#21528=CARTESIAN_POINT('Ctrl Pts',(31.3901924922002,-36.2091789909079,8.));
#21529=CARTESIAN_POINT('Ctrl Pts',(31.3605239499998,-36.0929588041061,8.));
#21530=CARTESIAN_POINT('Ctrl Pts',(31.3368613966103,-35.9750966537399,8.));
#21531=CARTESIAN_POINT('Ctrl Pts',(31.319113975657,-35.8560283881328,8.));
#21532=CARTESIAN_POINT('Ctrl Pts',(31.3091304483948,-35.7890484433355,8.));
#21533=CARTESIAN_POINT('Ctrl Pts',(31.3010196851544,-35.7216868798927,8.));
#21534=CARTESIAN_POINT('Ctrl Pts',(31.2947725609189,-35.6540227383851,8.));
#21535=CARTESIAN_POINT('Ctrl Pts',(31.2918900964785,-35.6228020559662,8.));
#21536=CARTESIAN_POINT('Ctrl Pts',(31.2894044622378,-35.591516977816,8.));
#21537=CARTESIAN_POINT('Ctrl Pts',(31.2873151093096,-35.5601754031315,8.));
#21538=CARTESIAN_POINT('Ctrl Pts',(31.2861140199798,-35.542158326923,8.));
#21539=CARTESIAN_POINT('Ctrl Pts',(31.2850444024964,-35.5241296340464,8.));
#21540=CARTESIAN_POINT('Ctrl Pts',(31.2841061875917,-35.5060991653233,8.));
#21541=CARTESIAN_POINT('Ctrl Pts',(31.2777952935748,-35.3848173815625,8.));
#21542=CARTESIAN_POINT('Ctrl Pts',(31.2774169324427,-35.2633382728991,8.));
#21543=CARTESIAN_POINT('Ctrl Pts',(31.2828128947659,-35.142109099441,8.));
#21544=CARTESIAN_POINT('Ctrl Pts',(31.2880969228261,-35.0233947134034,8.));
#21545=CARTESIAN_POINT('Ctrl Pts',(31.2989186932579,-34.9049190770275,8.));
#21546=CARTESIAN_POINT('Ctrl Pts',(31.3151830117592,-34.7871081783408,8.));
#21547=CARTESIAN_POINT('Ctrl Pts',(31.3312884180702,-34.67044836311,8.));
#21548=CARTESIAN_POINT('Ctrl Pts',(31.3527308881008,-34.5544395226326,8.));
#21549=CARTESIAN_POINT('Ctrl Pts',(31.3794647737014,-34.4395141802506,8.));
#21550=CARTESIAN_POINT('Ctrl Pts',(31.396871707047,-34.3646841385402,8.));
#21551=CARTESIAN_POINT('Ctrl Pts',(31.416522902222,-34.2903138655065,8.));
#21552=CARTESIAN_POINT('Ctrl Pts',(31.4384155592443,-34.2165296601315,8.));
#21553=CARTESIAN_POINT('Ctrl Pts',(31.4458038981696,-34.1916289495378,8.));
#21554=CARTESIAN_POINT('Ctrl Pts',(31.4534475860939,-34.1667950423673,8.));
#21555=CARTESIAN_POINT('Ctrl Pts',(31.461346703037,-34.1420329699976,8.));
#21556=CARTESIAN_POINT('Ctrl Pts',(31.46643308557,-34.1260882291753,8.));
#21557=CARTESIAN_POINT('Ctrl Pts',(31.471624585416,-34.1101758846519,8.));
#21558=CARTESIAN_POINT('Ctrl Pts',(31.476918343353,-34.0943053028287,8.));
#21559=CARTESIAN_POINT('Ctrl Pts',(31.513816049212,-33.9836867088362,8.));
#21560=CARTESIAN_POINT('Ctrl Pts',(31.5557144650388,-33.8749795921173,8.));
#21561=CARTESIAN_POINT('Ctrl Pts',(31.6025487964097,-33.7686031580514,8.));
#21562=CARTESIAN_POINT('Ctrl Pts',(31.6406629208299,-33.6820332311479,8.));
#21563=CARTESIAN_POINT('Ctrl Pts',(31.682046953583,-33.5970070600165,8.));
#21564=CARTESIAN_POINT('Ctrl Pts',(31.7266869557237,-33.5137662402706,8.));
#21565=CARTESIAN_POINT('Ctrl Pts',(31.7483019580961,-33.4734604510681,8.));
#21566=CARTESIAN_POINT('Ctrl Pts',(31.7706806142055,-33.4335734915742,8.));
#21567=CARTESIAN_POINT('Ctrl Pts',(31.7938228147784,-33.3941343150086,8.));
#21568=CARTESIAN_POINT('Ctrl Pts',(31.8074092885987,-33.3709801063925,8.));
#21569=CARTESIAN_POINT('Ctrl Pts',(31.8212609965416,-33.347977169053,8.));
#21570=CARTESIAN_POINT('Ctrl Pts',(31.8353638634359,-33.3251538546887,8.));
#21571=CARTESIAN_POINT('Ctrl Pts',(31.8937952976074,-33.2305915929272,8.));
#21572=CARTESIAN_POINT('Ctrl Pts',(31.9565779834776,-33.1390345522359,8.));
#21573=CARTESIAN_POINT('Ctrl Pts',(32.0236778740976,-33.0508734495428,8.));
#21574=CARTESIAN_POINT('Ctrl Pts',(32.0837087245751,-32.972000206609,8.));
#21575=CARTESIAN_POINT('Ctrl Pts',(32.1471956775548,-32.8958451124639,8.));
#21576=CARTESIAN_POINT('Ctrl Pts',(32.2141378419758,-32.8227144830143,8.));
#21577=CARTESIAN_POINT('Ctrl Pts',(32.2489927811285,-32.7846373807617,8.));
#21578=CARTESIAN_POINT('Ctrl Pts',(32.2847848221939,-32.7473806972021,8.));
#21579=CARTESIAN_POINT('Ctrl Pts',(32.3214765561793,-32.7109598296518,8.));
#21580=CARTESIAN_POINT('Origin',(0.,0.,8.));
#21581=CARTESIAN_POINT('',(-50.,50.,8.));
#21582=CARTESIAN_POINT('',(-50.,-50.,8.));
#21583=CARTESIAN_POINT('',(-50.,50.,8.));
#21584=CARTESIAN_POINT('',(50.,-50.,8.));
#21585=CARTESIAN_POINT('',(-50.,-50.,8.));
#21586=CARTESIAN_POINT('',(50.,50.,8.));
#21587=CARTESIAN_POINT('',(50.,-50.,8.));
#21588=CARTESIAN_POINT('',(50.,50.,8.));
#21589=CARTESIAN_POINT('Ctrl Pts',(-32.3264680662287,-32.7141668369925,
8.));
#21590=CARTESIAN_POINT('Ctrl Pts',(-32.2493255072635,-32.7912796001948,
8.));
#21591=CARTESIAN_POINT('Ctrl Pts',(-32.1762953075955,-32.8720145313034,
8.));
#21592=CARTESIAN_POINT('Ctrl Pts',(-32.1073697738656,-32.9559531279149,
8.));
#21593=CARTESIAN_POINT('Ctrl Pts',(-32.0366843378685,-33.0420349611253,
8.));
#21594=CARTESIAN_POINT('Ctrl Pts',(-31.9703154802321,-33.1314866020839,
8.));
#21595=CARTESIAN_POINT('Ctrl Pts',(-31.9082847764611,-33.2239028032894,
8.));
#21596=CARTESIAN_POINT('Ctrl Pts',(-31.8449630319238,-33.3182424565268,
8.));
#21597=CARTESIAN_POINT('Ctrl Pts',(-31.786161483907,-33.415671941835,8.));
#21598=CARTESIAN_POINT('Ctrl Pts',(-31.7319398749946,-33.5157996279616,
8.));
#21599=CARTESIAN_POINT('Ctrl Pts',(-31.6801506359753,-33.6114356072929,
8.));
#21600=CARTESIAN_POINT('Ctrl Pts',(-31.6325396515499,-33.709533968736,8.));
#21601=CARTESIAN_POINT('Ctrl Pts',(-31.5891944935205,-33.8097780642334,
8.));
#21602=CARTESIAN_POINT('Ctrl Pts',(-31.582156905406,-33.8260538534356,8.));
#21603=CARTESIAN_POINT('Ctrl Pts',(-31.5752318490596,-33.8423862467834,
8.));
#21604=CARTESIAN_POINT('Ctrl Pts',(-31.568419792889,-33.8587739316911,8.));
#21605=CARTESIAN_POINT('Ctrl Pts',(-31.5619098742369,-33.8744347678579,
8.));
#21606=CARTESIAN_POINT('Ctrl Pts',(-31.5555061718916,-33.8901389077819,
8.));
#21607=CARTESIAN_POINT('Ctrl Pts',(-31.5492108990198,-33.9058797005882,
8.));
#21608=CARTESIAN_POINT('Ctrl Pts',(-31.5058255436634,-34.0143610807278,
8.));
#21609=CARTESIAN_POINT('Ctrl Pts',(-31.4675540442795,-34.1246594478804,
8.));
#21610=CARTESIAN_POINT('Ctrl Pts',(-31.434425017105,-34.2363429975606,8.));
#21611=CARTESIAN_POINT('Ctrl Pts',(-31.4008614525105,-34.3494914463237,
8.));
#21612=CARTESIAN_POINT('Ctrl Pts',(-31.3725757523594,-34.4640624049253,
8.));
#21613=CARTESIAN_POINT('Ctrl Pts',(-31.3496403133382,-34.5796393782454,
8.));
#21614=CARTESIAN_POINT('Ctrl Pts',(-31.3256653487767,-34.7004547608028,
8.));
#21615=CARTESIAN_POINT('Ctrl Pts',(-31.307535844936,-34.8223702353544,8.));
#21616=CARTESIAN_POINT('Ctrl Pts',(-31.2953902232888,-34.9449334450722,
8.));
#21617=CARTESIAN_POINT('Ctrl Pts',(-31.2862810070535,-35.0368558523606,
8.));
#21618=CARTESIAN_POINT('Ctrl Pts',(-31.2805388477475,-35.1291432073786,
8.));
#21619=CARTESIAN_POINT('Ctrl Pts',(-31.2782452710195,-35.2216081255571,
8.));
#21620=CARTESIAN_POINT('Ctrl Pts',(-31.2776977000309,-35.243683300125,8.));
#21621=CARTESIAN_POINT('Ctrl Pts',(-31.2773468435284,-35.2657731220308,
8.));
#21622=CARTESIAN_POINT('Ctrl Pts',(-31.277193913283,-35.2878459781507,8.));
#21623=CARTESIAN_POINT('Ctrl Pts',(-31.2763590765867,-35.4083403266138,
8.));
#21624=CARTESIAN_POINT('Ctrl Pts',(-31.2814123990406,-35.5284798599375,
8.));
#21625=CARTESIAN_POINT('Ctrl Pts',(-31.2924228410947,-35.6478385426709,
8.));
#21626=CARTESIAN_POINT('Ctrl Pts',(-31.303362629127,-35.7664313005734,8.));
#21627=CARTESIAN_POINT('Ctrl Pts',(-31.3201830802735,-35.8842540736147,
8.));
#21628=CARTESIAN_POINT('Ctrl Pts',(-31.3430012709811,-36.000901820846,8.));
#21629=CARTESIAN_POINT('Ctrl Pts',(-31.3458749177941,-36.0155920489787,
8.));
#21630=CARTESIAN_POINT('Ctrl Pts',(-31.3488437566082,-36.0302636478795,
8.));
#21631=CARTESIAN_POINT('Ctrl Pts',(-31.3519080804568,-36.0449158122488,
8.));
#21632=CARTESIAN_POINT('Ctrl Pts',(-31.3758185581684,-36.1592445408324,
8.));
#21633=CARTESIAN_POINT('Ctrl Pts',(-31.4055382437248,-36.2723905489836,
8.));
#21634=CARTESIAN_POINT('Ctrl Pts',(-31.4407609915798,-36.3840873440382,
8.));
#21635=CARTESIAN_POINT('Ctrl Pts',(-31.4627262403709,-36.4537425538657,
8.));
#21636=CARTESIAN_POINT('Ctrl Pts',(-31.4868326485685,-36.5228340916482,
8.));
#21637=CARTESIAN_POINT('Ctrl Pts',(-31.5130158235422,-36.5912951432516,
8.));
#21638=CARTESIAN_POINT('Ctrl Pts',(-31.5219654331702,-36.6146956547323,
8.));
#21639=CARTESIAN_POINT('Ctrl Pts',(-31.5311577380477,-36.638022485054,8.));
#21640=CARTESIAN_POINT('Ctrl Pts',(-31.5405903538195,-36.6612728973655,
8.));
#21641=CARTESIAN_POINT('Ctrl Pts',(-31.5473394036631,-36.677908600056,8.));
#21642=CARTESIAN_POINT('Ctrl Pts',(-31.5542120267349,-36.6945063014083,
8.));
#21643=CARTESIAN_POINT('Ctrl Pts',(-31.5612002800447,-36.7110486972688,
8.));
#21644=CARTESIAN_POINT('Ctrl Pts',(-31.6071216062265,-36.8197523636167,
8.));
#21645=CARTESIAN_POINT('Ctrl Pts',(-31.6580959615467,-36.9262296326556,
8.));
#21646=CARTESIAN_POINT('Ctrl Pts',(-31.7137649062032,-37.0302261570189,
8.));
#21647=CARTESIAN_POINT('Ctrl Pts',(-31.7713490613653,-37.1378005332208,
8.));
#21648=CARTESIAN_POINT('Ctrl Pts',(-31.833956554581,-37.2427212245297,8.));
#21649=CARTESIAN_POINT('Ctrl Pts',(-31.9012460458509,-37.3446993846474,
8.));
#21650=CARTESIAN_POINT('Ctrl Pts',(-31.9691687068521,-37.4476371223012,
8.));
#21651=CARTESIAN_POINT('Ctrl Pts',(-32.0418623269422,-37.547577436253,8.));
#21652=CARTESIAN_POINT('Ctrl Pts',(-32.1190263529718,-37.6442049753141,
8.));
#21653=CARTESIAN_POINT('Ctrl Pts',(-32.1734394282079,-37.7123429642625,
8.));
#21654=CARTESIAN_POINT('Ctrl Pts',(-32.230076492864,-37.7788333069719,8.));
#21655=CARTESIAN_POINT('Ctrl Pts',(-32.288845213566,-37.8435569436544,8.));
#21656=CARTESIAN_POINT('Ctrl Pts',(-32.3150777918285,-37.8724476161826,
8.));
#21657=CARTESIAN_POINT('Ctrl Pts',(-32.3417352269367,-37.9009861713024,
8.));
#21658=CARTESIAN_POINT('Ctrl Pts',(-32.3688099173017,-37.9291614469859,
8.));
#21659=CARTESIAN_POINT('Ctrl Pts',(-32.3804320487223,-37.941256017686,8.));
#21660=CARTESIAN_POINT('Ctrl Pts',(-32.3921296471323,-37.9532821092146,
8.));
#21661=CARTESIAN_POINT('Ctrl Pts',(-32.4038956063136,-37.9652324558272,
8.));
#21662=CARTESIAN_POINT('Ctrl Pts',(-32.4923378704609,-38.0550607218847,
8.));
#21663=CARTESIAN_POINT('Ctrl Pts',(-32.5847394664431,-38.1407163588179,
8.));
#21664=CARTESIAN_POINT('Ctrl Pts',(-32.6807716550536,-38.2218812155311,
8.));
#21665=CARTESIAN_POINT('Ctrl Pts',(-32.7628115828128,-38.2912200390828,
8.));
#21666=CARTESIAN_POINT('Ctrl Pts',(-32.8475022057307,-38.3572813267927,
8.));
#21667=CARTESIAN_POINT('Ctrl Pts',(-32.9346627816287,-38.4198491494197,
8.));
#21668=CARTESIAN_POINT('Ctrl Pts',(-32.9737737137373,-38.447924753989,8.));
#21669=CARTESIAN_POINT('Ctrl Pts',(-33.0133822496832,-38.4752966907185,
8.));
#21670=CARTESIAN_POINT('Ctrl Pts',(-33.0534733017689,-38.5019440931387,
8.));
#21671=CARTESIAN_POINT('Ctrl Pts',(-33.0807070399686,-38.5200455981744,
8.));
#21672=CARTESIAN_POINT('Ctrl Pts',(-33.1081690766608,-38.5378161440549,
8.));
#21673=CARTESIAN_POINT('Ctrl Pts',(-33.1358247214715,-38.5552304161034,
8.));
#21674=CARTESIAN_POINT('Ctrl Pts',(-33.2426290354803,-38.6224832099845,
8.));
#21675=CARTESIAN_POINT('Ctrl Pts',(-33.3523800768607,-38.684469196206,8.));
#21676=CARTESIAN_POINT('Ctrl Pts',(-33.4647758690787,-38.7408547167133,
8.));
#21677=CARTESIAN_POINT('Ctrl Pts',(-33.5668696003918,-38.7920720093452,
8.));
#21678=CARTESIAN_POINT('Ctrl Pts',(-33.6711462627517,-38.8386684870918,
8.));
#21679=CARTESIAN_POINT('Ctrl Pts',(-33.777402890587,-38.880364981349,8.));
#21680=CARTESIAN_POINT('Ctrl Pts',(-33.8328334021929,-38.9021166410425,
8.));
#21681=CARTESIAN_POINT('Ctrl Pts',(-33.8888030678697,-38.9225343317631,
8.));
#21682=CARTESIAN_POINT('Ctrl Pts',(-33.9452677648582,-38.941630165528,8.));
#21683=CARTESIAN_POINT('Ctrl Pts',(-36.0520713770612,-38.9352951690526,
8.));
#21684=CARTESIAN_POINT('Ctrl Pts',(-36.1681793348248,-38.8956805565571,
8.));
#21685=CARTESIAN_POINT('Ctrl Pts',(-36.2820222319885,-38.8505155239877,
8.));
#21686=CARTESIAN_POINT('Ctrl Pts',(-36.39337417598,-38.8001576820793,8.));
#21687=CARTESIAN_POINT('Ctrl Pts',(-36.507223335641,-38.7486704984873,8.));
#21688=CARTESIAN_POINT('Ctrl Pts',(-36.6184691867386,-38.6917544842536,
8.));
#21689=CARTESIAN_POINT('Ctrl Pts',(-36.726846022942,-38.6297432779853,8.));
#21690=CARTESIAN_POINT('Ctrl Pts',(-36.8407844151035,-38.5645498530274,
8.));
#21691=CARTESIAN_POINT('Ctrl Pts',(-36.9515527511922,-38.4937244553102,
8.));
#21692=CARTESIAN_POINT('Ctrl Pts',(-37.0588031240991,-38.417608572184,8.));
#21693=CARTESIAN_POINT('Ctrl Pts',(-37.1526472003926,-38.3510071744486,
8.));
#21694=CARTESIAN_POINT('Ctrl Pts',(-37.2437975316357,-38.2803541911134,
8.));
#21695=CARTESIAN_POINT('Ctrl Pts',(-37.3319895495211,-38.2058562501456,
8.));
#21696=CARTESIAN_POINT('Ctrl Pts',(-37.3493652308069,-38.1911785898568,
8.));
#21697=CARTESIAN_POINT('Ctrl Pts',(-37.3666259764485,-38.1763516270108,
8.));
#21698=CARTESIAN_POINT('Ctrl Pts',(-37.3837696084918,-38.1613768709081,
8.));
#21699=CARTESIAN_POINT('Ctrl Pts',(-37.3963039208792,-38.1504283000079,
8.));
#21700=CARTESIAN_POINT('Ctrl Pts',(-37.4087744173897,-38.1394017179875,
8.));
#21701=CARTESIAN_POINT('Ctrl Pts',(-37.421171447845,-38.1283058376695,8.));
#21702=CARTESIAN_POINT('Ctrl Pts',(-37.5137506606012,-38.0454434240953,
8.));
#21703=CARTESIAN_POINT('Ctrl Pts',(-37.6023740233075,-37.9585993019841,
8.));
#21704=CARTESIAN_POINT('Ctrl Pts',(-37.686780110783,-37.8680943929378,8.));
#21705=CARTESIAN_POINT('Ctrl Pts',(-37.7709944562299,-37.7777950803761,
8.));
#21706=CARTESIAN_POINT('Ctrl Pts',(-37.8510111825053,-37.6838508893952,
8.));
#21707=CARTESIAN_POINT('Ctrl Pts',(-37.9265302130999,-37.5865485225552,
8.));
#21708=CARTESIAN_POINT('Ctrl Pts',(-38.0010169291866,-37.4905762395914,
8.));
#21709=CARTESIAN_POINT('Ctrl Pts',(-38.0711284717142,-37.3913362778857,
8.));
#21710=CARTESIAN_POINT('Ctrl Pts',(-38.1365308641829,-37.2890829148734,
8.));
#21711=CARTESIAN_POINT('Ctrl Pts',(-38.1898364642257,-37.2057422805937,
8.));
#21712=CARTESIAN_POINT('Ctrl Pts',(-38.2400130851628,-37.1203993452656,
8.));
#21713=CARTESIAN_POINT('Ctrl Pts',(-38.2868539614533,-37.0331859413737,
8.));
#21714=CARTESIAN_POINT('Ctrl Pts',(-38.2987540819478,-37.0110290114177,
8.));
#21715=CARTESIAN_POINT('Ctrl Pts',(-38.3104387758635,-36.9887513389692,
8.));
#21716=CARTESIAN_POINT('Ctrl Pts',(-38.3219043896502,-36.9663550605045,
8.));
#21717=CARTESIAN_POINT('Ctrl Pts',(-38.3300610648434,-36.9504222746659,
8.));
#21718=CARTESIAN_POINT('Ctrl Pts',(-38.3381031537755,-36.9344366433847,
8.));
#21719=CARTESIAN_POINT('Ctrl Pts',(-38.3460269902799,-36.918404590898,8.));
#21720=CARTESIAN_POINT('Ctrl Pts',(-38.3989878678949,-36.8112504908368,
8.));
#21721=CARTESIAN_POINT('Ctrl Pts',(-38.4467098948397,-36.7019465274356,
8.));
#21722=CARTESIAN_POINT('Ctrl Pts',(-38.4889142721076,-36.5907553164102,
8.));
#21723=CARTESIAN_POINT('Ctrl Pts',(-38.5302824920512,-36.4817670367281,
8.));
#21724=CARTESIAN_POINT('Ctrl Pts',(-38.566349800654,-36.3709649163585,8.));
#21725=CARTESIAN_POINT('Ctrl Pts',(-38.5968054307926,-36.2585824846173,
8.));
#21726=CARTESIAN_POINT('Ctrl Pts',(-38.6012596681997,-36.2421461794391,
8.));
#21727=CARTESIAN_POINT('Ctrl Pts',(-38.6055937817646,-36.225676056354,8.));
#21728=CARTESIAN_POINT('Ctrl Pts',(-38.6098067052154,-36.2091728328306,
8.));
#21729=CARTESIAN_POINT('Ctrl Pts',(-38.6394752606328,-36.0929526338671,
8.));
#21730=CARTESIAN_POINT('Ctrl Pts',(-38.6631378364378,-35.9750905238851,
8.));
#21731=CARTESIAN_POINT('Ctrl Pts',(-38.6808852873793,-35.8560223427045,
8.));
#21732=CARTESIAN_POINT('Ctrl Pts',(-38.6908688312617,-35.7890424470708,
8.));
#21733=CARTESIAN_POINT('Ctrl Pts',(-38.6989796136129,-35.7216809467524,
8.));
#21734=CARTESIAN_POINT('Ctrl Pts',(-38.705226759162,-35.6540168808315,8.));
#21735=CARTESIAN_POINT('Ctrl Pts',(-38.7081092384591,-35.6227961788899,
8.));
#21736=CARTESIAN_POINT('Ctrl Pts',(-38.7105948866426,-35.5915110836458,
8.));
#21737=CARTESIAN_POINT('Ctrl Pts',(-38.7126842525742,-35.5601694941906,
8.));
#21738=CARTESIAN_POINT('Ctrl Pts',(-38.713885344499,-35.542152482698,8.));
#21739=CARTESIAN_POINT('Ctrl Pts',(-38.7149549653242,-35.5241238555354,
8.));
#21740=CARTESIAN_POINT('Ctrl Pts',(-38.7158931843189,-35.5060934532667,
8.));
#21741=CARTESIAN_POINT('Ctrl Pts',(-38.7222041204107,-35.3848118366399,
8.));
#21742=CARTESIAN_POINT('Ctrl Pts',(-38.7225825299149,-35.2633329304591,
8.));
#21743=CARTESIAN_POINT('Ctrl Pts',(-38.717186620484,-35.142103985552,8.));
#21744=CARTESIAN_POINT('Ctrl Pts',(-38.7119026444224,-35.0233898278976,
8.));
#21745=CARTESIAN_POINT('Ctrl Pts',(-38.7010809307532,-34.9049144449008,
8.));
#21746=CARTESIAN_POINT('Ctrl Pts',(-38.684816672141,-34.7871038160559,8.));
#21747=CARTESIAN_POINT('Ctrl Pts',(-38.668711320133,-34.6704442318052,8.));
#21748=CARTESIAN_POINT('Ctrl Pts',(-38.6472689041617,-34.5544356388673,
8.));
#21749=CARTESIAN_POINT('Ctrl Pts',(-38.6205350708283,-34.439510552711,8.));
#21750=CARTESIAN_POINT('Ctrl Pts',(-38.6031281770284,-34.364680701536,8.));
#21751=CARTESIAN_POINT('Ctrl Pts',(-38.5834770220596,-34.2903106224296,
8.));
#21752=CARTESIAN_POINT('Ctrl Pts',(-38.5615844054563,-34.2165266120474,
8.));
#21753=CARTESIAN_POINT('Ctrl Pts',(-38.5541960539989,-34.1916258790507,
8.));
#21754=CARTESIAN_POINT('Ctrl Pts',(-38.5465523517576,-34.1667919500715,
8.));
#21755=CARTESIAN_POINT('Ctrl Pts',(-38.5386532186941,-34.1420298564502,
8.));
#21756=CARTESIAN_POINT('Ctrl Pts',(-38.5335668050111,-34.1260850368347,
8.));
#21757=CARTESIAN_POINT('Ctrl Pts',(-38.5283752724802,-34.1101726142316,
8.));
#21758=CARTESIAN_POINT('Ctrl Pts',(-38.5230814802764,-34.094301954882,8.));
#21759=CARTESIAN_POINT('Ctrl Pts',(-38.4861838094094,-33.9836836414723,
8.));
#21760=CARTESIAN_POINT('Ctrl Pts',(-38.4442854263901,-33.8749768051962,
8.));
#21761=CARTESIAN_POINT('Ctrl Pts',(-38.3974511240065,-33.7686006435033,
8.));
#21762=CARTESIAN_POINT('Ctrl Pts',(-38.3593370554135,-33.6820310114798,
8.));
#21763=CARTESIAN_POINT('Ctrl Pts',(-38.3179530814865,-33.5970051272784,
8.));
#21764=CARTESIAN_POINT('Ctrl Pts',(-38.2733131402326,-33.5137645815446,
8.));
#21765=CARTESIAN_POINT('Ctrl Pts',(-38.2516981548861,-33.4734589017939,
8.));
#21766=CARTESIAN_POINT('Ctrl Pts',(-38.2293195154062,-33.4335720492035,
8.));
#21767=CARTESIAN_POINT('Ctrl Pts',(-38.2061773309613,-33.3941329764629,
8.));
#21768=CARTESIAN_POINT('Ctrl Pts',(-38.1925909485316,-33.3709789684133,
8.));
#21769=CARTESIAN_POINT('Ctrl Pts',(-38.1787393350554,-33.3479762288434,
8.));
#21770=CARTESIAN_POINT('Ctrl Pts',(-38.1646365654847,-33.3251531088758,
8.));
#21771=CARTESIAN_POINT('Ctrl Pts',(-38.1062051167558,-33.2305909764135,
8.));
#21772=CARTESIAN_POINT('Ctrl Pts',(-38.0434224031259,-33.139034050394,8.));
#21773=CARTESIAN_POINT('Ctrl Pts',(-37.9763224701899,-33.050873041493,8.));
#21774=CARTESIAN_POINT('Ctrl Pts',(-37.9162917251371,-32.972000070726,8.));
#21775=CARTESIAN_POINT('Ctrl Pts',(-37.8528048824192,-32.8958452190746,
8.));
#21776=CARTESIAN_POINT('Ctrl Pts',(-37.7858628320068,-32.8227147956203,
8.));
#21777=CARTESIAN_POINT('Ctrl Pts',(-37.7510079037,-32.7846377476237,8.));
#21778=CARTESIAN_POINT('Ctrl Pts',(-37.7152158718889,-32.7473811107005,
8.));
#21779=CARTESIAN_POINT('Ctrl Pts',(-37.6785241456451,-32.7109602826758,
8.));
#21780=CARTESIAN_POINT('Ctrl Pts',(-32.3264680662287,37.2858331630075,8.));
#21781=CARTESIAN_POINT('Ctrl Pts',(-32.2493254281347,37.208720320707,8.));
#21782=CARTESIAN_POINT('Ctrl Pts',(-32.1762951458997,37.1279853156793,8.));
#21783=CARTESIAN_POINT('Ctrl Pts',(-32.1073695284417,37.0440466492215,8.));
#21784=CARTESIAN_POINT('Ctrl Pts',(-32.036684016981,36.9579647570495,8.));
#21785=CARTESIAN_POINT('Ctrl Pts',(-31.9703150813857,36.8685130624034,8.));
#21786=CARTESIAN_POINT('Ctrl Pts',(-31.9082842995806,36.7760968113946,8.));
#21787=CARTESIAN_POINT('Ctrl Pts',(-31.8449624922372,36.6817571324243,8.));
#21788=CARTESIAN_POINT('Ctrl Pts',(-31.7861608789268,36.5843276270745,8.));
#21789=CARTESIAN_POINT('Ctrl Pts',(-31.7319392047808,36.4841999248104,8.));
#21790=CARTESIAN_POINT('Ctrl Pts',(-31.680149951798,36.3885640193387,8.));
#21791=CARTESIAN_POINT('Ctrl Pts',(-31.6325389456654,36.2904657399127,8.));
#21792=CARTESIAN_POINT('Ctrl Pts',(-31.5891937601898,36.1902217321721,8.));
#21793=CARTESIAN_POINT('Ctrl Pts',(-31.5821558034642,36.1739451150407,8.));
#21794=CARTESIAN_POINT('Ctrl Pts',(-31.575230390001,36.1576118880571,8.));
#21795=CARTESIAN_POINT('Ctrl Pts',(-31.56841798829,36.1412233640005,8.));
#21796=CARTESIAN_POINT('Ctrl Pts',(-31.5619084669515,36.125563476111,8.));
#21797=CARTESIAN_POINT('Ctrl Pts',(-31.5555051500235,36.1098602922108,8.));
#21798=CARTESIAN_POINT('Ctrl Pts',(-31.5492102490141,36.0941204589327,8.));
#21799=CARTESIAN_POINT('Ctrl Pts',(-31.5058248130015,35.9856390819387,8.));
#21800=CARTESIAN_POINT('Ctrl Pts',(-31.467553236408,35.8753407193868,8.));
#21801=CARTESIAN_POINT('Ctrl Pts',(-31.4344241380457,35.7636571739254,8.));
#21802=CARTESIAN_POINT('Ctrl Pts',(-31.4008605131946,35.650508769435,8.));
#21803=CARTESIAN_POINT('Ctrl Pts',(-31.3725747552338,35.5359378557202,8.));
#21804=CARTESIAN_POINT('Ctrl Pts',(-31.3496392634799,35.4203609255757,8.));
#21805=CARTESIAN_POINT('Ctrl Pts',(-31.3256642608852,35.2995456742689,8.));
#21806=CARTESIAN_POINT('Ctrl Pts',(-31.3075347162269,35.1776303306686,8.));
#21807=CARTESIAN_POINT('Ctrl Pts',(-31.2953890537165,35.0550672480091,8.));
#21808=CARTESIAN_POINT('Ctrl Pts',(-31.2862798068337,34.9631449360145,8.));
#21809=CARTESIAN_POINT('Ctrl Pts',(-31.2805376168519,34.8708576741034,8.));
#21810=CARTESIAN_POINT('Ctrl Pts',(-31.2782440105566,34.778392845323,8.));
#21811=CARTESIAN_POINT('Ctrl Pts',(-31.2776964353943,34.7563178084142,8.));
#21812=CARTESIAN_POINT('Ctrl Pts',(-31.2773455727076,34.7342281241833,8.));
#21813=CARTESIAN_POINT('Ctrl Pts',(-31.2771926342729,34.7121554053342,8.));
#21814=CARTESIAN_POINT('Ctrl Pts',(-31.2763577480363,34.5916611083402,8.));
#21815=CARTESIAN_POINT('Ctrl Pts',(-31.2814110294711,34.4715216187175,8.));
#21816=CARTESIAN_POINT('Ctrl Pts',(-31.2924214415633,34.3521629693739,8.));
#21817=CARTESIAN_POINT('Ctrl Pts',(-31.3033611959409,34.2335702867641,8.));
#21818=CARTESIAN_POINT('Ctrl Pts',(-31.3201816201703,34.115747578293,8.));
#21819=CARTESIAN_POINT('Ctrl Pts',(-31.3429997930851,33.999099881963,8.));
#21820=CARTESIAN_POINT('Ctrl Pts',(-31.345873443513,33.984409630306,8.));
#21821=CARTESIAN_POINT('Ctrl Pts',(-31.3488422864746,33.96973800774,8.));
#21822=CARTESIAN_POINT('Ctrl Pts',(-31.35190661501,33.9550858195635,8.));
#21823=CARTESIAN_POINT('Ctrl Pts',(-31.3758170782861,33.8407571491025,8.));
#21824=CARTESIAN_POINT('Ctrl Pts',(-31.4055367574321,33.7276111853924,8.));
#21825=CARTESIAN_POINT('Ctrl Pts',(-31.4407595052535,33.6159144227599,8.));
#21826=CARTESIAN_POINT('Ctrl Pts',(-31.4627247636627,33.5462592025841,8.));
#21827=CARTESIAN_POINT('Ctrl Pts',(-31.4868311858377,33.4771676502711,8.));
#21828=CARTESIAN_POINT('Ctrl Pts',(-31.5130143786684,33.4087065804238,8.));
#21829=CARTESIAN_POINT('Ctrl Pts',(-31.5219642258836,33.3853054574484,8.));
#21830=CARTESIAN_POINT('Ctrl Pts',(-31.5311567813561,33.3619780190094,8.));
#21831=CARTESIAN_POINT('Ctrl Pts',(-31.5405896605283,33.3387270021894,8.));
#21832=CARTESIAN_POINT('Ctrl Pts',(-31.5473384631411,33.3220919409105,8.));
#21833=CARTESIAN_POINT('Ctrl Pts',(-31.5542108294608,33.3054948782145,8.));
#21834=CARTESIAN_POINT('Ctrl Pts',(-31.5611988172515,33.288953116597,8.));
#21835=CARTESIAN_POINT('Ctrl Pts',(-31.6071201467481,33.1802494799514,8.));
#21836=CARTESIAN_POINT('Ctrl Pts',(-31.6580945083799,33.0737722290612,8.));
#21837=CARTESIAN_POINT('Ctrl Pts',(-31.7137634608477,32.9697757128959,8.));
#21838=CARTESIAN_POINT('Ctrl Pts',(-31.7713476440883,32.8622013078145,8.));
#21839=CARTESIAN_POINT('Ctrl Pts',(-31.8339551704749,32.7572805788209,8.));
#21840=CARTESIAN_POINT('Ctrl Pts',(-31.9012446980031,32.6553023741411,8.));
#21841=CARTESIAN_POINT('Ctrl Pts',(-31.9691674082359,32.552364572362,8.));
#21842=CARTESIAN_POINT('Ctrl Pts',(-32.0418610824791,32.4524241883893,8.));
#21843=CARTESIAN_POINT('Ctrl Pts',(-32.1190251653974,32.3557965754622,8.));
#21844=CARTESIAN_POINT('Ctrl Pts',(-32.1734382985285,32.2876585121627,8.));
#21845=CARTESIAN_POINT('Ctrl Pts',(-32.2300754238941,32.2211680942644,8.));
#21846=CARTESIAN_POINT('Ctrl Pts',(-32.2888442072745,32.1564443823762,8.));
#21847=CARTESIAN_POINT('Ctrl Pts',(-32.3150764518969,32.1275540745384,8.));
#21848=CARTESIAN_POINT('Ctrl Pts',(-32.341733542045,32.0990158743987,8.));
#21849=CARTESIAN_POINT('Ctrl Pts',(-32.3688078763672,32.0708409435943,8.));
#21850=CARTESIAN_POINT('Ctrl Pts',(-32.3804297629888,32.0587466166393,8.));
#21851=CARTESIAN_POINT('Ctrl Pts',(-32.3921271141324,32.0467207651166,8.));
#21852=CARTESIAN_POINT('Ctrl Pts',(-32.4038928229971,32.0347706553995,8.));
#21853=CARTESIAN_POINT('Ctrl Pts',(-32.4923350889694,31.9449422571145,8.));
#21854=CARTESIAN_POINT('Ctrl Pts',(-32.5847366887113,31.8592864840437,8.));
#21855=CARTESIAN_POINT('Ctrl Pts',(-32.6807688805232,31.7781214891551,8.));
#21856=CARTESIAN_POINT('Ctrl Pts',(-32.7628090255767,31.7087823662183,8.));
#21857=CARTESIAN_POINT('Ctrl Pts',(-32.8474998792406,31.6427207947673,8.));
#21858=CARTESIAN_POINT('Ctrl Pts',(-32.9346606964287,31.5801527068548,8.));
#21859=CARTESIAN_POINT('Ctrl Pts',(-32.9737718119822,31.5520769292834,8.));
#21860=CARTESIAN_POINT('Ctrl Pts',(-33.0133805354119,31.5247048259746,8.));
#21861=CARTESIAN_POINT('Ctrl Pts',(-33.0534717786847,31.4980572637843,8.));
#21862=CARTESIAN_POINT('Ctrl Pts',(-33.0807061080661,31.4799553435978,8.));
#21863=CARTESIAN_POINT('Ctrl Pts',(-33.1081687455454,31.4621843968183,8.));
#21864=CARTESIAN_POINT('Ctrl Pts',(-33.1358249991596,31.4447697393726,8.));
#21865=CARTESIAN_POINT('Ctrl Pts',(-33.2426293820058,31.3775168942506,8.));
#21866=CARTESIAN_POINT('Ctrl Pts',(-33.3523804860194,31.3155308622806,8.));
#21867=CARTESIAN_POINT('Ctrl Pts',(-33.464776332519,31.2591453036981,8.));
#21868=CARTESIAN_POINT('Ctrl Pts',(-33.5668700198747,31.2079280232686,8.));
#21869=CARTESIAN_POINT('Ctrl Pts',(-33.671146627403,31.161331555616,8.));
#21870=CARTESIAN_POINT('Ctrl Pts',(-33.7774031884393,31.1196350702262,8.));
#21871=CARTESIAN_POINT('Ctrl Pts',(-33.8328337169093,31.0978833948665,8.));
#21872=CARTESIAN_POINT('Ctrl Pts',(-33.8888033971972,31.0774656906331,8.));
#21873=CARTESIAN_POINT('Ctrl Pts',(-33.9452681066883,31.058369845356,8.));
#21874=CARTESIAN_POINT('Ctrl Pts',(-36.0520713770612,31.0647048309474,8.));
#21875=CARTESIAN_POINT('Ctrl Pts',(-36.168179415234,31.1043194708775,8.));
#21876=CARTESIAN_POINT('Ctrl Pts',(-36.2820223922111,31.1494845221288,8.));
#21877=CARTESIAN_POINT('Ctrl Pts',(-36.3933744144291,31.1998423763314,8.));
#21878=CARTESIAN_POINT('Ctrl Pts',(-36.5072236213378,31.25132955769,8.));
#21879=CARTESIAN_POINT('Ctrl Pts',(-36.6184695195224,31.3082455598905,8.));
#21880=CARTESIAN_POINT('Ctrl Pts',(-36.7268464017735,31.3702567471293,8.));
#21881=CARTESIAN_POINT('Ctrl Pts',(-36.8407847815347,31.4354501172862,8.));
#21882=CARTESIAN_POINT('Ctrl Pts',(-36.9515531074568,31.5062754464572,8.));
#21883=CARTESIAN_POINT('Ctrl Pts',(-37.0588034719145,31.5823912510781,8.));
#21884=CARTESIAN_POINT('Ctrl Pts',(-37.152647540815,31.6489925801213,8.));
#21885=CARTESIAN_POINT('Ctrl Pts',(-37.2437978659804,31.7196454871349,8.));
#21886=CARTESIAN_POINT('Ctrl Pts',(-37.3319898787643,31.7941433466814,8.));
#21887=CARTESIAN_POINT('Ctrl Pts',(-37.3493659727369,31.8088213403836,8.));
#21888=CARTESIAN_POINT('Ctrl Pts',(-37.3666271256303,31.8236486435546,8.));
#21889=CARTESIAN_POINT('Ctrl Pts',(-37.3837711593319,31.8386237468057,8.));
#21890=CARTESIAN_POINT('Ctrl Pts',(-37.3963054555396,31.8495723008716,8.));
#21891=CARTESIAN_POINT('Ctrl Pts',(-37.4087759352647,31.8605988651726,8.));
#21892=CARTESIAN_POINT('Ctrl Pts',(-37.4211729491963,31.8716947276461,8.));
#21893=CARTESIAN_POINT('Ctrl Pts',(-37.5137521425834,31.9545571010691,8.));
#21894=CARTESIAN_POINT('Ctrl Pts',(-37.6023754843508,32.0414011788236,8.));
#21895=CARTESIAN_POINT('Ctrl Pts',(-37.6867815485414,32.1319060425465,8.));
#21896=CARTESIAN_POINT('Ctrl Pts',(-37.7709958473242,32.2222052847627,8.));
#21897=CARTESIAN_POINT('Ctrl Pts',(-37.8510125269352,32.3161494024035,8.));
#21898=CARTESIAN_POINT('Ctrl Pts',(-37.9265315102947,32.413451696318,8.));
#21899=CARTESIAN_POINT('Ctrl Pts',(-38.0010181696068,32.5094238942302,8.));
#21900=CARTESIAN_POINT('Ctrl Pts',(-38.0711296560004,32.6086637703888,8.));
#21901=CARTESIAN_POINT('Ctrl Pts',(-38.1365319925539,32.7109170507384,8.));
#21902=CARTESIAN_POINT('Ctrl Pts',(-38.189837488265,32.7942575257788,8.));
#21903=CARTESIAN_POINT('Ctrl Pts',(-38.2400140119095,32.8796002993686,8.));
#21904=CARTESIAN_POINT('Ctrl Pts',(-38.2868547984211,32.966813541324,8.));
#21905=CARTESIAN_POINT('Ctrl Pts',(-38.2987553976748,32.9889713640128,8.));
#21906=CARTESIAN_POINT('Ctrl Pts',(-38.3104405526761,33.0112499393599,8.));
#21907=CARTESIAN_POINT('Ctrl Pts',(-38.3219066094193,33.0336471306571,8.));
#21908=CARTESIAN_POINT('Ctrl Pts',(-38.3300627268695,33.0495788608817,8.));
#21909=CARTESIAN_POINT('Ctrl Pts',(-38.3381042716881,33.0655634268488,8.));
#21910=CARTESIAN_POINT('Ctrl Pts',(-38.3460275803167,33.0815944092568,8.));
#21911=CARTESIAN_POINT('Ctrl Pts',(-38.3989884279579,33.1887484350122,8.));
#21912=CARTESIAN_POINT('Ctrl Pts',(-38.4467104251109,33.2980523321741,8.));
#21913=CARTESIAN_POINT('Ctrl Pts',(-38.4889147723839,33.409243488173,8.));
#21914=CARTESIAN_POINT('Ctrl Pts',(-38.5302829624144,33.5182317125689,8.));
#21915=CARTESIAN_POINT('Ctrl Pts',(-38.5663502410402,33.6290337883757,8.));
#21916=CARTESIAN_POINT('Ctrl Pts',(-38.596805840802,33.7414161893267,8.));
#21917=CARTESIAN_POINT('Ctrl Pts',(-38.6012600218942,33.7578522985917,8.));
#21918=CARTESIAN_POINT('Ctrl Pts',(-38.6055940819337,33.7743222252706,8.));
#21919=CARTESIAN_POINT('Ctrl Pts',(-38.6098069546845,33.7908252519299,8.));
#21920=CARTESIAN_POINT('Ctrl Pts',(-38.6394755059943,33.9070454470715,8.));
#21921=CARTESIAN_POINT('Ctrl Pts',(-38.6631380748325,34.0249075695662,8.));
#21922=CARTESIAN_POINT('Ctrl Pts',(-38.6808855164532,34.1439757769513,8.));
#21923=CARTESIAN_POINT('Ctrl Pts',(-38.6908690551697,34.2109556878445,8.));
#21924=CARTESIAN_POINT('Ctrl Pts',(-38.6989798315808,34.2783172077624,8.));
#21925=CARTESIAN_POINT('Ctrl Pts',(-38.7052269705051,34.3459812971573,8.));
#21926=CARTESIAN_POINT('Ctrl Pts',(-38.7081094451816,34.3772019929916,8.));
#21927=CARTESIAN_POINT('Ctrl Pts',(-38.7105950890294,34.4084870828833,8.));
#21928=CARTESIAN_POINT('Ctrl Pts',(-38.712684450918,34.4398286677084,8.));
#21929=CARTESIAN_POINT('Ctrl Pts',(-38.7138855420385,34.457845699339,8.));
#21930=CARTESIAN_POINT('Ctrl Pts',(-38.7149551618269,34.47587434695,8.));
#21931=CARTESIAN_POINT('Ctrl Pts',(-38.7158933795518,34.4939047698972,8.));
#21932=CARTESIAN_POINT('Ctrl Pts',(-38.722204302566,34.6151864384397,8.));
#21933=CARTESIAN_POINT('Ctrl Pts',(-38.7225826970351,34.7366654075262,8.));
#21934=CARTESIAN_POINT('Ctrl Pts',(-38.7171867711641,34.8578944234449,8.));
#21935=CARTESIAN_POINT('Ctrl Pts',(-38.7119027789398,34.9766086520668,8.));
#21936=CARTESIAN_POINT('Ctrl Pts',(-38.7010810476264,35.0950841138035,8.));
#21937=CARTESIAN_POINT('Ctrl Pts',(-38.6848167703974,35.2128948265086,8.));
#21938=CARTESIAN_POINT('Ctrl Pts',(-38.6687114015083,35.3295544825446,8.));
#21939=CARTESIAN_POINT('Ctrl Pts',(-38.6472689687305,35.445563152418,8.));
#21940=CARTESIAN_POINT('Ctrl Pts',(-38.6205351191465,35.5604883182129,8.));
#21941=CARTESIAN_POINT('Ctrl Pts',(-38.603128213054,35.6353182285994,8.));
#21942=CARTESIAN_POINT('Ctrl Pts',(-38.5834770455875,35.7096883679731,8.));
#21943=CARTESIAN_POINT('Ctrl Pts',(-38.5615844164204,35.7834724389555,8.));
#21944=CARTESIAN_POINT('Ctrl Pts',(-38.5541960688544,35.8083731649983,8.));
#21945=CARTESIAN_POINT('Ctrl Pts',(-38.546552371059,35.8332070872086,8.));
#21946=CARTESIAN_POINT('Ctrl Pts',(-38.5386532430018,35.8579691742342,8.));
#21947=CARTESIAN_POINT('Ctrl Pts',(-38.533566838996,35.8739139693719,8.));
#21948=CARTESIAN_POINT('Ctrl Pts',(-38.5283753166192,35.8898263677189,8.));
#21949=CARTESIAN_POINT('Ctrl Pts',(-38.5230815350611,35.9056970029845,8.));
#21950=CARTESIAN_POINT('Ctrl Pts',(-38.4861838533105,36.0163154036073,8.));
#21951=CARTESIAN_POINT('Ctrl Pts',(-38.4442854600859,36.1250223270562,8.));
#21952=CARTESIAN_POINT('Ctrl Pts',(-38.3974511486834,36.2313985734173,8.));
#21953=CARTESIAN_POINT('Ctrl Pts',(-38.3593370627389,36.3179682970844,8.));
#21954=CARTESIAN_POINT('Ctrl Pts',(-38.3179530705292,36.4029942704614,8.));
#21955=CARTESIAN_POINT('Ctrl Pts',(-38.2733131103528,36.4862349013589,8.));
#21956=CARTESIAN_POINT('Ctrl Pts',(-38.2516981197193,36.52654061512,8.));
#21957=CARTESIAN_POINT('Ctrl Pts',(-38.2293194750761,36.5664275009295,8.));
#21958=CARTESIAN_POINT('Ctrl Pts',(-38.2061772856241,36.6058666059334,8.));
#21959=CARTESIAN_POINT('Ctrl Pts',(-38.1925908747914,36.6290206763194,8.));
#21960=CARTESIAN_POINT('Ctrl Pts',(-38.1787392319563,36.6520234773565,8.));
#21961=CARTESIAN_POINT('Ctrl Pts',(-38.1646364321387,36.6748466577435,8.));
#21962=CARTESIAN_POINT('Ctrl Pts',(-38.1062049879234,36.7694088304221,8.));
#21963=CARTESIAN_POINT('Ctrl Pts',(-38.0434222829092,36.8609657921147,8.));
#21964=CARTESIAN_POINT('Ctrl Pts',(-37.9763223631119,36.9491268302023,8.));
#21965=CARTESIAN_POINT('Ctrl Pts',(-37.9162915853069,37.0279998855573,8.));
#21966=CARTESIAN_POINT('Ctrl Pts',(-37.8528047083354,37.1041548125789,8.));
#21967=CARTESIAN_POINT('Ctrl Pts',(-37.7858626225071,37.1772853000647,8.));
#21968=CARTESIAN_POINT('Ctrl Pts',(-37.7510076908282,37.2153623649398,8.));
#21969=CARTESIAN_POINT('Ctrl Pts',(-37.7152156561398,37.2526190163742,8.));
#21970=CARTESIAN_POINT('Ctrl Pts',(-37.6785239274887,37.2890398567007,8.));
#21971=CARTESIAN_POINT('Ctrl Pts',(37.6735319337713,37.2858331630076,8.));
#21972=CARTESIAN_POINT('Ctrl Pts',(37.7506743707736,37.2087205217211,8.));
#21973=CARTESIAN_POINT('Ctrl Pts',(37.8237044431802,37.1279857045437,8.));
#21974=CARTESIAN_POINT('Ctrl Pts',(37.8926298478593,37.044047215584,8.));
#21975=CARTESIAN_POINT('Ctrl Pts',(37.9633151675467,36.957965473245,8.));
#21976=CARTESIAN_POINT('Ctrl Pts',(38.0296839050274,36.8685139150261,8.));
#21977=CARTESIAN_POINT('Ctrl Pts',(38.0917144885261,36.7760977905708,8.));
#21978=CARTESIAN_POINT('Ctrl Pts',(38.1550361362519,36.681758176998,8.));
#21979=CARTESIAN_POINT('Ctrl Pts',(38.213837583624,36.5843287225808,8.));
#21980=CARTESIAN_POINT('Ctrl Pts',(38.2680590919843,36.4842010613249,8.));
#21981=CARTESIAN_POINT('Ctrl Pts',(38.3198483094818,36.3885649681376,8.));
#21982=CARTESIAN_POINT('Ctrl Pts',(38.367459260449,36.2904664802624,8.));
#21983=CARTESIAN_POINT('Ctrl Pts',(38.4108043761726,36.1902222494829,8.));
#21984=CARTESIAN_POINT('Ctrl Pts',(38.4178413961439,36.1739477363751,8.));
#21985=CARTESIAN_POINT('Ctrl Pts',(38.4247659020623,36.1576166279166,8.));
#21986=CARTESIAN_POINT('Ctrl Pts',(38.4315774256463,36.1412302363951,8.));
#21987=CARTESIAN_POINT('Ctrl Pts',(38.4380879567714,36.1255679384209,8.));
#21988=CARTESIAN_POINT('Ctrl Pts',(38.444492253249,36.1098623247479,8.));
#21989=CARTESIAN_POINT('Ctrl Pts',(38.4507880993566,36.0941200527897,8.));
#21990=CARTESIAN_POINT('Ctrl Pts',(38.4941733303702,35.9856386677758,8.));
#21991=CARTESIAN_POINT('Ctrl Pts',(38.5324447107219,35.8753402935035,8.));
#21992=CARTESIAN_POINT('Ctrl Pts',(38.5655736281431,35.7636567372894,8.));
#21993=CARTESIAN_POINT('Ctrl Pts',(38.5991370998293,35.6505082202659,8.));
#21994=CARTESIAN_POINT('Ctrl Pts',(38.6274227108421,35.5359371924552,8.));
#21995=CARTESIAN_POINT('Ctrl Pts',(38.6503580685478,35.4203601525596,8.));
#21996=CARTESIAN_POINT('Ctrl Pts',(38.6743329744418,35.2995445677074,8.));
#21997=CARTESIAN_POINT('Ctrl Pts',(38.6924624153241,35.1776288913195,8.));
#21998=CARTESIAN_POINT('Ctrl Pts',(38.7046079739425,35.0550654857614,8.));
#21999=CARTESIAN_POINT('Ctrl Pts',(38.7137171429063,34.9631429315928,8.));
#22000=CARTESIAN_POINT('Ctrl Pts',(38.7194592548969,34.8708554330634,8.));
#22001=CARTESIAN_POINT('Ctrl Pts',(38.7217527860176,34.7783903770868,8.));
#22002=CARTESIAN_POINT('Ctrl Pts',(38.7223003505608,34.7563149905001,8.));
#22003=CARTESIAN_POINT('Ctrl Pts',(38.7226511975219,34.7342249565511,8.));
#22004=CARTESIAN_POINT('Ctrl Pts',(38.7228041151383,34.7121518890107,8.));
#22005=CARTESIAN_POINT('Ctrl Pts',(38.7236388754478,34.5916574611757,8.));
#22006=CARTESIAN_POINT('Ctrl Pts',(38.7185854897377,34.4715178604479,8.));
#22007=CARTESIAN_POINT('Ctrl Pts',(38.7075750014661,34.3521591261975,8.));
#22008=CARTESIAN_POINT('Ctrl Pts',(38.6966351615249,34.2335662521979,8.));
#22009=CARTESIAN_POINT('Ctrl Pts',(38.6798146688512,34.1157433795803,8.));
#22010=CARTESIAN_POINT('Ctrl Pts',(38.6569964506754,33.9990955538343,8.));
#22011=CARTESIAN_POINT('Ctrl Pts',(38.6541228094095,33.9844053618549,8.));
#22012=CARTESIAN_POINT('Ctrl Pts',(38.6511539769623,33.9697337993248,8.));
#22013=CARTESIAN_POINT('Ctrl Pts',(38.6480896603102,33.9550816715453,8.));
#22014=CARTESIAN_POINT('Ctrl Pts',(38.6241791602958,33.840752853322,8.));
#22015=CARTESIAN_POINT('Ctrl Pts',(38.5944594648021,33.7276067766126,8.));
#22016=CARTESIAN_POINT('Ctrl Pts',(38.5592367168361,33.6159099315205,8.));
#22017=CARTESIAN_POINT('Ctrl Pts',(38.5372714828272,33.5462547375853,8.));
#22018=CARTESIAN_POINT('Ctrl Pts',(38.5131650961288,33.4771632221397,8.));
#22019=CARTESIAN_POINT('Ctrl Pts',(38.4869819486326,33.4087021985955,8.));
#22020=CARTESIAN_POINT('Ctrl Pts',(38.4780327050517,33.385302629251,8.));
#22021=CARTESIAN_POINT('Ctrl Pts',(38.4688407862625,33.3619767358619,8.));
#22022=CARTESIAN_POINT('Ctrl Pts',(38.4594085763077,33.3387272549231,8.));
#22023=CARTESIAN_POINT('Ctrl Pts',(38.4526591454727,33.3220905638083,8.));
#22024=CARTESIAN_POINT('Ctrl Pts',(38.4457861267366,33.3054918782784,8.));
#22025=CARTESIAN_POINT('Ctrl Pts',(38.438797464252,33.2889485050412,8.));
#22026=CARTESIAN_POINT('Ctrl Pts',(38.3928761431039,33.180244792853,8.));
#22027=CARTESIAN_POINT('Ctrl Pts',(38.3419017974374,33.073767495779,8.));
#22028=CARTESIAN_POINT('Ctrl Pts',(38.2862328647479,32.9697709587171,8.));
#22029=CARTESIAN_POINT('Ctrl Pts',(38.2286487527766,32.8621966269402,8.));
#22030=CARTESIAN_POINT('Ctrl Pts',(38.1660413106006,32.757275993628,8.));
#22031=CARTESIAN_POINT('Ctrl Pts',(38.0987518751312,32.6552979021095,8.));
#22032=CARTESIAN_POINT('Ctrl Pts',(38.0308292899206,32.5523602632,8.));
#22033=CARTESIAN_POINT('Ctrl Pts',(37.9581357532083,32.4524200570822,8.));
#22034=CARTESIAN_POINT('Ctrl Pts',(37.8809718147757,32.3557926317859,8.));
#22035=CARTESIAN_POINT('Ctrl Pts',(37.8265588287192,32.2876547573834,8.));
#22036=CARTESIAN_POINT('Ctrl Pts',(37.7699218575833,32.221164530513,8.));
#22037=CARTESIAN_POINT('Ctrl Pts',(37.7111532334385,32.156441009698,8.));
#22038=CARTESIAN_POINT('Ctrl Pts',(37.6849201407301,32.1275497748485,8.));
#22039=CARTESIAN_POINT('Ctrl Pts',(37.6582621737227,32.0990106723795,8.));
#22040=CARTESIAN_POINT('Ctrl Pts',(37.6311869343715,32.0708348649218,8.));
#22041=CARTESIAN_POINT('Ctrl Pts',(37.6195644247842,32.0587399176506,8.));
#22042=CARTESIAN_POINT('Ctrl Pts',(37.6078664443942,32.0467134553255,8.));
#22043=CARTESIAN_POINT('Ctrl Pts',(37.5961000985213,32.0347627427216,8.));
#22044=CARTESIAN_POINT('Ctrl Pts',(37.5076578370054,31.9449346804806,8.));
#22045=CARTESIAN_POINT('Ctrl Pts',(37.4152562466455,31.8592792534028,8.));
#22046=CARTESIAN_POINT('Ctrl Pts',(37.3192240628069,31.7781146097001,8.));
#22047=CARTESIAN_POINT('Ctrl Pts',(37.2371844701374,31.7087762478888,8.));
#22048=CARTESIAN_POINT('Ctrl Pts',(37.1524942030697,31.6427153977926,8.));
#22049=CARTESIAN_POINT('Ctrl Pts',(37.0653339993003,31.5801479843188,8.));
#22050=CARTESIAN_POINT('Ctrl Pts',(37.026223350155,31.552072646602,8.));
#22051=CARTESIAN_POINT('Ctrl Pts',(36.9866151034059,31.5247009668187,8.));
#22052=CARTESIAN_POINT('Ctrl Pts',(36.9465243462331,31.4980538108418,8.));
#22053=CARTESIAN_POINT('Ctrl Pts',(36.9192915198287,31.4799529461023,8.));
#22054=CARTESIAN_POINT('Ctrl Pts',(36.891830409748,31.4621830185383,8.));
#22055=CARTESIAN_POINT('Ctrl Pts',(36.8641757039143,31.4447693408987,8.));
#22056=CARTESIAN_POINT('Ctrl Pts',(36.7573714959831,31.3775166259847,8.));
#22057=CARTESIAN_POINT('Ctrl Pts',(36.6476205511297,31.3155307102762,8.));
#22058=CARTESIAN_POINT('Ctrl Pts',(36.53522484258,31.2591452484686,8.));
#22059=CARTESIAN_POINT('Ctrl Pts',(36.4331310435836,31.2079279370747,8.));
#22060=CARTESIAN_POINT('Ctrl Pts',(36.328854296794,31.161331443821,8.));
#22061=CARTESIAN_POINT('Ctrl Pts',(36.2225975660985,31.1196349359533,8.));
#22062=CARTESIAN_POINT('Ctrl Pts',(36.1671670804927,31.0978833004188,8.));
#22063=CARTESIAN_POINT('Ctrl Pts',(36.1111974373468,31.0774656305418,8.));
#22064=CARTESIAN_POINT('Ctrl Pts',(36.0547327596422,31.0583698145405,8.));
#22065=CARTESIAN_POINT('Ctrl Pts',(33.9479286229388,31.0647048309474,8.));
#22066=CARTESIAN_POINT('Ctrl Pts',(33.8318204903556,31.1043195030892,8.));
#22067=CARTESIAN_POINT('Ctrl Pts',(33.7179774196666,31.1494845762766,8.));
#22068=CARTESIAN_POINT('Ctrl Pts',(33.6066253055996,31.1998424449166,8.));
#22069=CARTESIAN_POINT('Ctrl Pts',(33.4927760432216,31.2513296236524,8.));
#22070=CARTESIAN_POINT('Ctrl Pts',(33.3815300897553,31.3082456117247,8.));
#22071=CARTESIAN_POINT('Ctrl Pts',(33.2731531534421,31.3702567766217,8.));
#22072=CARTESIAN_POINT('Ctrl Pts',(33.1592147882362,31.4354500824416,8.));
#22073=CARTESIAN_POINT('Ctrl Pts',(33.0484464742462,31.5062753311388,8.));
#22074=CARTESIAN_POINT('Ctrl Pts',(32.9411961197039,31.5823910435948,8.));
#22075=CARTESIAN_POINT('Ctrl Pts',(32.8473520594793,31.6489922919938,8.));
#22076=CARTESIAN_POINT('Ctrl Pts',(32.7562017414451,31.719645109407,8.));
#22077=CARTESIAN_POINT('Ctrl Pts',(32.6680097346461,31.7941428733673,8.));
#22078=CARTESIAN_POINT('Ctrl Pts',(32.6506331562116,31.8088212584686,8.));
#22079=CARTESIAN_POINT('Ctrl Pts',(32.6333715252365,31.8236489611523,8.));
#22080=CARTESIAN_POINT('Ctrl Pts',(32.6162270200198,31.8386244719266,8.));
#22081=CARTESIAN_POINT('Ctrl Pts',(32.6036927426372,31.8495730063766,8.));
#22082=CARTESIAN_POINT('Ctrl Pts',(32.5912222824502,31.8605995500244,8.));
#22083=CARTESIAN_POINT('Ctrl Pts',(32.5788252877513,31.8716953917,8.));
#22084=CARTESIAN_POINT('Ctrl Pts',(32.4862461171128,31.9545577179984,8.));
#22085=CARTESIAN_POINT('Ctrl Pts',(32.397622799937,32.0414017436923,8.));
#22086=CARTESIAN_POINT('Ctrl Pts',(32.3132167630922,32.1319065542212,8.));
#22087=CARTESIAN_POINT('Ctrl Pts',(32.2290025191065,32.2222057138629,8.));
#22088=CARTESIAN_POINT('Ctrl Pts',(32.1489858942929,32.3161497454154,8.));
#22089=CARTESIAN_POINT('Ctrl Pts',(32.0734669664008,32.4134519537301,8.));
#22090=CARTESIAN_POINT('Ctrl Pts',(31.9989803737659,32.5094240517922,8.));
#22091=CARTESIAN_POINT('Ctrl Pts',(31.9288689532965,32.6086638275202,8.));
#22092=CARTESIAN_POINT('Ctrl Pts',(31.8634666824091,32.7109170108275,8.));
#22093=CARTESIAN_POINT('Ctrl Pts',(31.8101613092083,32.7942572989124,8.));
#22094=CARTESIAN_POINT('Ctrl Pts',(31.7599848998086,32.8795998826136,8.));
#22095=CARTESIAN_POINT('Ctrl Pts',(31.7131442187192,32.9668129344489,8.));
#22096=CARTESIAN_POINT('Ctrl Pts',(31.7012430571606,32.9889718056646,8.));
#22097=CARTESIAN_POINT('Ctrl Pts',(31.6895573606131,33.0112514414787,8.));
#22098=CARTESIAN_POINT('Ctrl Pts',(31.6780907836173,33.033649704911,8.));
#22099=CARTESIAN_POINT('Ctrl Pts',(31.6699353210994,33.0495801955843,8.));
#22100=CARTESIAN_POINT('Ctrl Pts',(31.6618944152098,33.0655635106099,8.));
#22101=CARTESIAN_POINT('Ctrl Pts',(31.6539717264445,33.0815932364824,8.));
#22102=CARTESIAN_POINT('Ctrl Pts',(31.6010109140258,33.1887471750268,8.));
#22103=CARTESIAN_POINT('Ctrl Pts',(31.5532889518817,33.2980509944504,8.));
#22104=CARTESIAN_POINT('Ctrl Pts',(31.5110846398564,33.4092420858783,8.));
#22105=CARTESIAN_POINT('Ctrl Pts',(31.469716484976,33.5182302453998,8.));
#22106=CARTESIAN_POINT('Ctrl Pts',(31.4336492415757,33.6290322689246,8.));
#22107=CARTESIAN_POINT('Ctrl Pts',(31.4031936775095,33.7414146337669,8.));
#22108=CARTESIAN_POINT('Ctrl Pts',(31.39873956261,33.7578505127609,8.));
#22109=CARTESIAN_POINT('Ctrl Pts',(31.3944055654848,33.7743202085893,8.));
#22110=CARTESIAN_POINT('Ctrl Pts',(31.3901927523269,33.7908230038594,8.));
#22111=CARTESIAN_POINT('Ctrl Pts',(31.3605242058421,33.9070431945601,8.));
#22112=CARTESIAN_POINT('Ctrl Pts',(31.3368616451868,34.0249053317963,8.));
#22113=CARTESIAN_POINT('Ctrl Pts',(31.3191142145135,34.1439735700009,8.));
#22114=CARTESIAN_POINT('Ctrl Pts',(31.3091306818643,34.210953498841,8.));
#22115=CARTESIAN_POINT('Ctrl Pts',(31.3010199124296,34.2783150418024,8.));
#22116=CARTESIAN_POINT('Ctrl Pts',(31.294772781286,34.3459791587903,8.));
#22117=CARTESIAN_POINT('Ctrl Pts',(31.2918903120279,34.3771998475526,8.));
#22118=CARTESIAN_POINT('Ctrl Pts',(31.2894046732663,34.4084849312592,8.));
#22119=CARTESIAN_POINT('Ctrl Pts',(31.2873153161224,34.4398265107474,8.));
#22120=CARTESIAN_POINT('Ctrl Pts',(31.2861142259533,34.4578435659536,8.));
#22121=CARTESIAN_POINT('Ctrl Pts',(31.2850446073883,34.4758722375043,8.));
#22122=CARTESIAN_POINT('Ctrl Pts',(31.2841063911591,34.4939026846615,8.));
#22123=CARTESIAN_POINT('Ctrl Pts',(31.2777954835053,34.6151844142158,8.));
#22124=CARTESIAN_POINT('Ctrl Pts',(31.2774171066952,34.7366634572185,8.));
#22125=CARTESIAN_POINT('Ctrl Pts',(31.2828130518753,34.8578925565699,8.));
#22126=CARTESIAN_POINT('Ctrl Pts',(31.2880970630825,34.976606868563,8.));
#22127=CARTESIAN_POINT('Ctrl Pts',(31.2989188151177,35.0950824227959,8.));
#22128=CARTESIAN_POINT('Ctrl Pts',(31.3151831142098,35.2128932340069,8.));
#22129=CARTESIAN_POINT('Ctrl Pts',(31.3312885029229,35.3295529743629,8.));
#22130=CARTESIAN_POINT('Ctrl Pts',(31.3527309554357,35.4455617346014,8.));
#22131=CARTESIAN_POINT('Ctrl Pts',(31.3794648241005,35.5604869939325,8.));
#22132=CARTESIAN_POINT('Ctrl Pts',(31.3968717446295,35.6353169738744,8.));
#22133=CARTESIAN_POINT('Ctrl Pts',(31.4165229267736,35.7096871840419,8.));
#22134=CARTESIAN_POINT('Ctrl Pts',(31.438415570696,35.7834713262069,8.));
#22135=CARTESIAN_POINT('Ctrl Pts',(31.4458039136858,35.8083720440668,8.));
#22136=CARTESIAN_POINT('Ctrl Pts',(31.4534476062533,35.833205958311,8.));
#22137=CARTESIAN_POINT('Ctrl Pts',(31.4613467284242,35.8579680375739,8.));
#22138=CARTESIAN_POINT('Ctrl Pts',(31.4664331210497,35.8739128039203,8.));
#22139=CARTESIAN_POINT('Ctrl Pts',(31.4716246314855,35.8898251737367,8.));
#22140=CARTESIAN_POINT('Ctrl Pts',(31.4769184005249,35.9056957806736,8.));
#22141=CARTESIAN_POINT('Ctrl Pts',(31.5138160950465,36.0163142837243,8.));
#22142=CARTESIAN_POINT('Ctrl Pts',(31.5557145002446,36.1250213095504,8.));
#22143=CARTESIAN_POINT('Ctrl Pts',(31.6025488222259,36.2313976553429,8.));
#22144=CARTESIAN_POINT('Ctrl Pts',(31.6406629285514,36.3179674866662,8.));
#22145=CARTESIAN_POINT('Ctrl Pts',(31.6820469422375,36.4029935647969,8.));
#22146=CARTESIAN_POINT('Ctrl Pts',(31.7266869246432,36.4862342957322,8.));
#22147=CARTESIAN_POINT('Ctrl Pts',(31.7483019214948,36.5265400494563,8.));
#22148=CARTESIAN_POINT('Ctrl Pts',(31.7706805722115,36.5664269742985,8.));
#22149=CARTESIAN_POINT('Ctrl Pts',(31.7938227675543,36.605866117211,8.));
#22150=CARTESIAN_POINT('Ctrl Pts',(31.8074092117442,36.6290202608064,8.));
#22151=CARTESIAN_POINT('Ctrl Pts',(31.8212608890592,36.6520231340321,8.));
#22152=CARTESIAN_POINT('Ctrl Pts',(31.8353637243995,36.6748463853764,8.));
#22153=CARTESIAN_POINT('Ctrl Pts',(31.8937951632988,36.7694086052589,8.));
#22154=CARTESIAN_POINT('Ctrl Pts',(31.9565778581775,36.8609656088156,8.));
#22155=CARTESIAN_POINT('Ctrl Pts',(32.0236777625255,36.9491266811452,8.));
#22156=CARTESIAN_POINT('Ctrl Pts',(32.0837085788304,37.0279998358789,8.));
#22157=CARTESIAN_POINT('Ctrl Pts',(32.1471954960693,37.1041548514456,8.));
#22158=CARTESIAN_POINT('Ctrl Pts',(32.2141376235347,37.177285414151,8.));
#22159=CARTESIAN_POINT('Ctrl Pts',(32.248992559173,37.2153624988329,8.));
#22160=CARTESIAN_POINT('Ctrl Pts',(32.2847845972398,37.2526191672925,8.));
#22161=CARTESIAN_POINT('Ctrl Pts',(32.321476328717,37.2890400220485,8.));
#22162=CARTESIAN_POINT('Origin',(-35.,-35.,10.2084234471775));
#22163=CARTESIAN_POINT('Ctrl Pts',(-39.0784093524563,-34.997955826836,7.70842344717746));
#22164=CARTESIAN_POINT('Ctrl Pts',(-39.0792534643083,-34.8668875745646,
7.70328437820511));
#22165=CARTESIAN_POINT('Ctrl Pts',(-39.0145241717454,-33.401902569157,7.64581193344868));
#22166=CARTESIAN_POINT('Ctrl Pts',(-37.2468182307978,-30.7615622415685,
7.53600611290816));
#22167=CARTESIAN_POINT('Ctrl Pts',(-32.7044906448315,-30.7882310811688,
7.37900598555592));
#22168=CARTESIAN_POINT('Ctrl Pts',(-30.2206288723714,-34.591050784955,7.22200585820366));
#22169=CARTESIAN_POINT('Ctrl Pts',(-32.0224449816578,-38.760868439734,7.06500573085141));
#22170=CARTESIAN_POINT('Ctrl Pts',(-36.4942781630208,-39.5581356918704,
6.90800560349915));
#22171=CARTESIAN_POINT('Ctrl Pts',(-38.8653532597229,-37.0673722499186,
6.78914484227451));
#22172=CARTESIAN_POINT('Ctrl Pts',(-39.0751760778997,-35.366983894328,6.72261745683394));
#22173=CARTESIAN_POINT('Ctrl Pts',(-39.0721140267755,-35.0034548068065,
6.70842344717746));
#22174=CARTESIAN_POINT('Ctrl Pts',(-39.0691247390887,-35.0040754761348,
7.79157655282255));
#22175=CARTESIAN_POINT('Ctrl Pts',(-39.0629617458988,-34.1015748206833,
7.75638428364687));
#22176=CARTESIAN_POINT('Ctrl Pts',(-38.3270258918815,-31.8449563360523,
7.6688586386871));
#22177=CARTESIAN_POINT('Ctrl Pts',(-34.6204730922247,-30.2191423808613,
7.52899961794324));
#22178=CARTESIAN_POINT('Ctrl Pts',(-30.8030823517117,-32.6774434597138,
7.37199949059099));
#22179=CARTESIAN_POINT('Ctrl Pts',(-30.7475655592404,-37.2202136561835,
7.21499936323873));
#22180=CARTESIAN_POINT('Ctrl Pts',(-34.5060129709306,-39.7711989299046,
7.05799923588648));
#22181=CARTESIAN_POINT('Ctrl Pts',(-38.2826810114871,-38.2186958612719,
6.91685829908109));
#22182=CARTESIAN_POINT('Ctrl Pts',(-39.0636923276262,-35.9315794222149,
6.82805073805978));
#22183=CARTESIAN_POINT('Ctrl Pts',(-39.0709664927331,-34.9967444357251,
6.79157655282255));
#22184=CARTESIAN_POINT('Ctrl Pts',(-32.3264680662287,-32.7141668369925,
8.));
#22185=CARTESIAN_POINT('Ctrl Pts',(-31.5748397248436,-33.5932784036375,
7.94766662421592));
#22186=CARTESIAN_POINT('Ctrl Pts',(-31.0185761455706,-36.1362135079881,
7.84299987264775));
#22187=CARTESIAN_POINT('Ctrl Pts',(-33.7549095310954,-38.9529268308332,
7.68599974529549));
#22188=CARTESIAN_POINT('Ctrl Pts',(-37.6085237505035,-38.2165103725086,
7.52899961794325));
#22189=CARTESIAN_POINT('Ctrl Pts',(-39.122629513254,-34.5999498459216,7.37199949059098));
#22190=CARTESIAN_POINT('Ctrl Pts',(-36.940145606194,-31.3400749195329,7.21499936323873));
#22191=CARTESIAN_POINT('Ctrl Pts',(-33.0178092164465,-31.3631036769391,
7.05799923588649));
#22192=CARTESIAN_POINT('Ctrl Pts',(-30.8729746062518,-34.6468690649513,
6.90099910853422));
#22193=CARTESIAN_POINT('Ctrl Pts',(-32.4288573028063,-38.2475401342247,
6.74399898118198));
#22194=CARTESIAN_POINT('Ctrl Pts',(-36.2903212074201,-38.9359868162892,
6.58699885382972));
#22195=CARTESIAN_POINT('Ctrl Pts',(-38.9947353103719,-36.0950579107052,
6.42999872647747));
#22196=CARTESIAN_POINT('Ctrl Pts',(-38.117035111845,-32.2721495171465,6.27299859912521));
#22197=CARTESIAN_POINT('Ctrl Pts',(-34.444258048923,-30.8953459884408,6.11599847177297));
#22198=CARTESIAN_POINT('Ctrl Pts',(-31.2698209074708,-33.1992175611906,
5.9589983444207));
#22199=CARTESIAN_POINT('Ctrl Pts',(-31.4402707556255,-37.1178717601522,
5.80199821706845));
#22200=CARTESIAN_POINT('Ctrl Pts',(-34.8027641605008,-39.1374081785836,
5.6449980897162));
#22201=CARTESIAN_POINT('Ctrl Pts',(-38.3421207391464,-37.4468919117391,
5.48799796236395));
#22202=CARTESIAN_POINT('Ctrl Pts',(-38.8845656356524,-33.5622237360543,
5.33099783501169));
#22203=CARTESIAN_POINT('Ctrl Pts',(-35.943683236251,-30.9668235565892,5.17399770765944));
#22204=CARTESIAN_POINT('Ctrl Pts',(-32.1565910373224,-31.9880112738199,
5.01699758030718));
#22205=CARTESIAN_POINT('Ctrl Pts',(-30.919210927847,-35.7100782334501,4.85999745295493));
#22206=CARTESIAN_POINT('Ctrl Pts',(-33.3411135315715,-38.7954112012017,
4.70299732560268));
#22207=CARTESIAN_POINT('Ctrl Pts',(-37.2505555447442,-38.477362547094,4.54599719825042));
#22208=CARTESIAN_POINT('Ctrl Pts',(-39.141902810795,-35.0411295298515,4.38899707089817));
#22209=CARTESIAN_POINT('Ctrl Pts',(-37.3191660904533,-31.5680152720272,
4.23199694354592));
#22210=CARTESIAN_POINT('Ctrl Pts',(-33.4168108878721,-31.1723946430222,
4.07499681619366));
#22211=CARTESIAN_POINT('Ctrl Pts',(-30.9341165505443,-34.2090244589174,
3.91799668884141));
#22212=CARTESIAN_POINT('Ctrl Pts',(-32.0973389085718,-37.9549296302039,
3.76099656148916));
#22213=CARTESIAN_POINT('Ctrl Pts',(-35.8634053144019,-39.0511210542994,
3.6039964341369));
#22214=CARTESIAN_POINT('Ctrl Pts',(-38.8552478911374,-36.5146333635664,
3.44699630678465));
#22215=CARTESIAN_POINT('Ctrl Pts',(-38.3900526994102,-32.6199594063295,
3.2899961794324));
#22216=CARTESIAN_POINT('Ctrl Pts',(-34.8849647272175,-30.8594906798889,
3.13299605208015));
#22217=CARTESIAN_POINT('Ctrl Pts',(-31.4830299921864,-32.8118563882867,
2.97599592472789));
#22218=CARTESIAN_POINT('Ctrl Pts',(-31.2347959944593,-36.726351454856,2.81899579737564));
#22219=CARTESIAN_POINT('Ctrl Pts',(-34.3628565683332,-39.0928106312356,
2.66199567002338));
#22220=CARTESIAN_POINT('Ctrl Pts',(-38.0622497333952,-37.7892072071444,
2.50499554267113));
#22221=CARTESIAN_POINT('Ctrl Pts',(-39.0156942580864,-33.9844950081716,
2.34799541531887));
#22222=CARTESIAN_POINT('Ctrl Pts',(-36.3682270687435,-31.0903957040226,
2.19099528796663));
#22223=CARTESIAN_POINT('Ctrl Pts',(-32.4938578387906,-31.7020764289629,
2.03399516061437));
#22224=CARTESIAN_POINT('Ctrl Pts',(-30.866769727096,-35.2710361541464,1.87699503326212));
#22225=CARTESIAN_POINT('Ctrl Pts',(-32.9459900633082,-38.5969565794207,
1.71999490590986));
#22226=CARTESIAN_POINT('Ctrl Pts',(-36.8670583779424,-38.6974486722808,
1.56299477855761));
#22227=CARTESIAN_POINT('Ctrl Pts',(-39.1139224428247,-35.4824088304557,
1.40599465120536));
#22228=CARTESIAN_POINT('Ctrl Pts',(-37.6717828958998,-31.8347767559132,
1.2489945238531));
#22229=CARTESIAN_POINT('Ctrl Pts',(-33.8338499179097,-31.0254541111767,
1.09199439650085));
#22230=CARTESIAN_POINT('Ctrl Pts',(-31.0415747701051,-33.7800977940573,
0.934994269148597));
#22231=CARTESIAN_POINT('Ctrl Pts',(-31.7989383549478,-37.6287343727556,
0.777994141796342));
#22232=CARTESIAN_POINT('Ctrl Pts',(-35.4265617474899,-39.1199684759325,
0.620994014444089));
#22233=CARTESIAN_POINT('Ctrl Pts',(-38.6720112486245,-36.9171723860524,
0.463993887091836));
#22234=CARTESIAN_POINT('Ctrl Pts',(-38.6240720221873,-32.9944536386984,
0.306993759739581));
#22235=CARTESIAN_POINT('Ctrl Pts',(-35.3277245214386,-30.8716914151866,
0.149993632387329));
#22236=CARTESIAN_POINT('Ctrl Pts',(-31.7348166906651,-32.4476562217995,
-0.00700649496492554));
#22237=CARTESIAN_POINT('Ctrl Pts',(-31.0753023569953,-36.3188879616356,
-0.164006622317179));
#22238=CARTESIAN_POINT('Ctrl Pts',(-32.9741442474368,-38.0994349533405,
-0.268673373885348));
#22239=CARTESIAN_POINT('Ctrl Pts',(-34.0915279074966,-38.3981590173419,
-0.321006749669432));
#22240=CARTESIAN_POINT('Ctrl Pts',(-32.1856025125516,-32.5937287191406,
8.10700224988981));
#22241=CARTESIAN_POINT('Ctrl Pts',(-31.3943716733878,-33.5191597390956,
8.05466887410573));
#22242=CARTESIAN_POINT('Ctrl Pts',(-30.8087991578366,-36.1960793891008,
7.95000212253755));
#22243=CARTESIAN_POINT('Ctrl Pts',(-33.6893070387277,-39.1612023407069,
7.79300199518531));
#22244=CARTESIAN_POINT('Ctrl Pts',(-37.7459640921552,-38.3859848825408,
7.63600186783305));
#22245=CARTESIAN_POINT('Ctrl Pts',(-39.3398464769469,-34.5788716288481,
7.4790017404808));
#22246=CARTESIAN_POINT('Ctrl Pts',(-37.0423698143953,-31.1472373602114,
7.32200161312854));
#22247=CARTESIAN_POINT('Ctrl Pts',(-32.9133696925748,-31.171479478349,7.1650014857763));
#22248=CARTESIAN_POINT('Ctrl Pts',(-30.6555260282916,-34.6282629716192,
7.00800135842403));
#22249=CARTESIAN_POINT('Ctrl Pts',(-32.2933865290902,-38.4186495693944,
6.85100123107179));
#22250=CARTESIAN_POINT('Ctrl Pts',(-36.358306859287,-39.1433697748163,6.69400110371953));
#22251=CARTESIAN_POINT('Ctrl Pts',(-39.2052136645597,-36.1527553471755,
6.53700097636729));
#22252=CARTESIAN_POINT('Ctrl Pts',(-38.2812683762075,-32.1284219768986,
6.38000084901502));
#22253=CARTESIAN_POINT('Ctrl Pts',(-34.4149765966796,-30.6790761348112,
6.22300072166278));
#22254=CARTESIAN_POINT('Ctrl Pts',(-31.073281738985,-33.1043362500341,6.06600059431052));
#22255=CARTESIAN_POINT('Ctrl Pts',(-31.2527124083266,-37.2294601703531,
5.90900046695826));
#22256=CARTESIAN_POINT('Ctrl Pts',(-34.792372013923,-39.3554038144322,5.75200033960602));
#22257=CARTESIAN_POINT('Ctrl Pts',(-38.5182135257814,-37.5758160437388,
5.59500021225375));
#22258=CARTESIAN_POINT('Ctrl Pts',(-39.0892392668699,-33.4864688341112,
5.43800008490151));
#22259=CARTESIAN_POINT('Ctrl Pts',(-35.9934049021458,-30.7543197799925,
5.28099995754925));
#22260=CARTESIAN_POINT('Ctrl Pts',(-32.0067748436954,-31.8293127917771,
5.12399983019699));
#22261=CARTESIAN_POINT('Ctrl Pts',(-30.7041984924888,-35.7474915002398,
4.96699970284474));
#22262=CARTESIAN_POINT('Ctrl Pts',(-33.2537085681557,-38.9953873801041,
4.80999957549249));
#22263=CARTESIAN_POINT('Ctrl Pts',(-37.3691349224156,-38.6605810807291,
4.65299944814024));
#22264=CARTESIAN_POINT('Ctrl Pts',(-39.3601352640338,-35.0432966010287,
4.49599932078798));
#22265=CARTESIAN_POINT('Ctrl Pts',(-37.4413604847951,-31.3871876474119,
4.33899919343573));
#22266=CARTESIAN_POINT('Ctrl Pts',(-33.3333943376382,-30.9707221882978,
4.18199906608348));
#22267=CARTESIAN_POINT('Ctrl Pts',(-30.7198894765905,-34.1673487990413,
4.02499893873122));
#22268=CARTESIAN_POINT('Ctrl Pts',(-31.9444007833091,-38.1106217291751,
3.86799881137897));
#22269=CARTESIAN_POINT('Ctrl Pts',(-35.9088972219885,-39.2645703133555,
3.71099868402671));
#22270=CARTESIAN_POINT('Ctrl Pts',(-39.0583768015825,-36.5944377843333,
3.55399855667446));
#22271=CARTESIAN_POINT('Ctrl Pts',(-38.5686709700449,-32.4945575991672,
3.39699842932221));
#22272=CARTESIAN_POINT('Ctrl Pts',(-34.8789036410609,-30.641331648192,3.23999830196996));
#22273=CARTESIAN_POINT('Ctrl Pts',(-31.2977245835776,-32.6965654289773,
3.0829981746177));
#22274=CARTESIAN_POINT('Ctrl Pts',(-31.0364114005639,-36.8173110766423,
2.92599804726545));
#22275=CARTESIAN_POINT('Ctrl Pts',(-34.3292861586667,-39.3084564697542,
2.76899791991319));
#22276=CARTESIAN_POINT('Ctrl Pts',(-38.2235964144439,-37.9361675679284,
2.61199779256094));
#22277=CARTESIAN_POINT('Ctrl Pts',(-39.2272769169348,-33.9309891303743,
2.45499766520869));
#22278=CARTESIAN_POINT('Ctrl Pts',(-36.4403174975728,-30.8844028124269,
2.29799753785644));
#22279=CARTESIAN_POINT('Ctrl Pts',(-32.3618118741726,-31.5283123441018,
2.14099741050418));
#22280=CARTESIAN_POINT('Ctrl Pts',(-30.6489942206534,-35.2853167607994,
1.98399728315193));
#22281=CARTESIAN_POINT('Ctrl Pts',(-32.8377664646538,-38.7864763954034,
1.82699715579967));
#22282=CARTESIAN_POINT('Ctrl Pts',(-36.9654316978321,-38.89226330974,1.66999702844742));
#22283=CARTESIAN_POINT('Ctrl Pts',(-39.3306806402386,-35.5078264385801,
1.51299690109516));
#22284=CARTESIAN_POINT('Ctrl Pts',(-37.8125562946319,-31.668004510122,1.35599677374291));
#22285=CARTESIAN_POINT('Ctrl Pts',(-33.7724067105519,-30.8160395161343,
1.19899664639066));
#22286=CARTESIAN_POINT('Ctrl Pts',(-30.8330095554335,-33.7158224444716,
1.04199651903841));
#22287=CARTESIAN_POINT('Ctrl Pts',(-31.630277821932,-37.7672395905951,0.884996391686153));
#22288=CARTESIAN_POINT('Ctrl Pts',(-35.4490368322191,-39.3370452323995,
0.727996264333899));
#22289=CARTESIAN_POINT('Ctrl Pts',(-38.8654856152897,-37.0181861597217,
0.570996136981647));
#22290=CARTESIAN_POINT('Ctrl Pts',(-38.815020522006,-32.8887835342792,0.413996009629392));
#22291=CARTESIAN_POINT('Ctrl Pts',(-35.3449919778631,-30.6541752272542,
0.256995882277139));
#22292=CARTESIAN_POINT('Ctrl Pts',(-31.5627776553664,-32.3131759431282,
0.0999957549248853));
#22293=CARTESIAN_POINT('Ctrl Pts',(-30.8685142129999,-36.3883787653949,
-0.0570043724273683));
#22294=CARTESIAN_POINT('Ctrl Pts',(-32.8674040627957,-38.2627408840732,
-0.161671123995537));
#22295=CARTESIAN_POINT('Ctrl Pts',(-34.0436614793107,-38.5772044012455,
-0.214004499779622));
#22296=CARTESIAN_POINT('Ctrl Pts',(-32.0447369588746,-32.4732906012887,
8.21400449977962));
#22297=CARTESIAN_POINT('Ctrl Pts',(-31.2139036219321,-33.4450410745538,
8.16167112399554));
#22298=CARTESIAN_POINT('Ctrl Pts',(-30.5990221701027,-36.2559452702134,
8.05700437242737));
#22299=CARTESIAN_POINT('Ctrl Pts',(-33.6237045463599,-39.3694778505807,
7.90000424507512));
#22300=CARTESIAN_POINT('Ctrl Pts',(-37.883404433807,-38.555459392573,7.74300411772286));
#22301=CARTESIAN_POINT('Ctrl Pts',(-39.5570634406398,-34.5577934117747,
7.58600399037061));
#22302=CARTESIAN_POINT('Ctrl Pts',(-37.1445940225965,-30.95439980089,7.42900386301835));
#22303=CARTESIAN_POINT('Ctrl Pts',(-32.8089301687032,-30.9798552797588,
7.2720037356661));
#22304=CARTESIAN_POINT('Ctrl Pts',(-30.4380774503315,-34.6096568782872,
7.11500360831385));
#22305=CARTESIAN_POINT('Ctrl Pts',(-32.157915755374,-38.5897590045642,6.9580034809616));
#22306=CARTESIAN_POINT('Ctrl Pts',(-36.4262925111539,-39.3507527333434,
6.80100335360934));
#22307=CARTESIAN_POINT('Ctrl Pts',(-39.4156920187475,-36.2104527836457,
6.64400322625709));
#22308=CARTESIAN_POINT('Ctrl Pts',(-38.4455016405701,-31.9846944366506,
6.48700309890483));
#22309=CARTESIAN_POINT('Ctrl Pts',(-34.3856951444362,-30.4628062811815,
6.33000297155259));
#22310=CARTESIAN_POINT('Ctrl Pts',(-30.8767425704992,-33.0094549388777,
6.17300284420032));
#22311=CARTESIAN_POINT('Ctrl Pts',(-31.0651540610276,-37.3410485805539,
6.01600271684808));
#22312=CARTESIAN_POINT('Ctrl Pts',(-34.7819798673453,-39.5733994502808,
5.85900258949582));
#22313=CARTESIAN_POINT('Ctrl Pts',(-38.6943063124164,-37.7047401757385,
5.70200246214356));
#22314=CARTESIAN_POINT('Ctrl Pts',(-39.2939128980875,-33.4107139321682,
5.54500233479131));
#22315=CARTESIAN_POINT('Ctrl Pts',(-36.0431265680407,-30.5418160033959,
5.38800220743906));
#22316=CARTESIAN_POINT('Ctrl Pts',(-31.8569586500684,-31.6706143097344,
5.2310020800868));
#22317=CARTESIAN_POINT('Ctrl Pts',(-30.4891860571307,-35.7849047670295,
5.07400195273456));
#22318=CARTESIAN_POINT('Ctrl Pts',(-33.1663036047398,-39.1953635590066,
4.9170018253823));
#22319=CARTESIAN_POINT('Ctrl Pts',(-37.487714300087,-38.8437996143642,4.76000169803005));
#22320=CARTESIAN_POINT('Ctrl Pts',(-39.5783677172726,-35.0454636722059,
4.60300157067779));
#22321=CARTESIAN_POINT('Ctrl Pts',(-37.563554879137,-31.2063600227966,4.44600144332554));
#22322=CARTESIAN_POINT('Ctrl Pts',(-33.2499777874043,-30.7690497335734,
4.28900131597329));
#22323=CARTESIAN_POINT('Ctrl Pts',(-30.5056624026368,-34.1256731391653,
4.13200118862103));
#22324=CARTESIAN_POINT('Ctrl Pts',(-31.7914626580464,-38.2663138281463,
3.97500106126878));
#22325=CARTESIAN_POINT('Ctrl Pts',(-35.9543891295751,-39.4780195724117,
3.81800093391652));
#22326=CARTESIAN_POINT('Ctrl Pts',(-39.2615057120276,-36.6742422051002,
3.66100080656427));
#22327=CARTESIAN_POINT('Ctrl Pts',(-38.7472892406796,-32.3691557920048,
3.50400067921202));
#22328=CARTESIAN_POINT('Ctrl Pts',(-34.8728425549044,-30.4231726164951,
3.34700055185977));
#22329=CARTESIAN_POINT('Ctrl Pts',(-31.1124191749688,-32.5812744696679,
3.19000042450751));
#22330=CARTESIAN_POINT('Ctrl Pts',(-30.8380268066686,-36.9082706984286,
3.03300029715526));
#22331=CARTESIAN_POINT('Ctrl Pts',(-34.295715749,-39.5241023082727,2.876000169803));
#22332=CARTESIAN_POINT('Ctrl Pts',(-38.3849430954928,-38.0831279287123,
2.71900004245075));
#22333=CARTESIAN_POINT('Ctrl Pts',(-39.438859575783,-33.8774832525769,2.5619999150985));
#22334=CARTESIAN_POINT('Ctrl Pts',(-36.5124079264021,-30.6784099208313,
2.40499978774625));
#22335=CARTESIAN_POINT('Ctrl Pts',(-32.2297659095544,-31.3545482592407,
2.24799966039399));
#22336=CARTESIAN_POINT('Ctrl Pts',(-30.4312187142109,-35.2995973674523,
2.09099953304174));
#22337=CARTESIAN_POINT('Ctrl Pts',(-32.7295428659994,-38.9759962113862,
1.93399940568948));
#22338=CARTESIAN_POINT('Ctrl Pts',(-37.0638050177218,-39.0870779471991,
1.77699927833723));
#22339=CARTESIAN_POINT('Ctrl Pts',(-39.5474388376525,-35.5332440467046,
1.61999915098498));
#22340=CARTESIAN_POINT('Ctrl Pts',(-37.953329693364,-31.5012322643307,1.46299902363272));
#22341=CARTESIAN_POINT('Ctrl Pts',(-33.7109635031942,-30.6066249210918,
1.30599889628047));
#22342=CARTESIAN_POINT('Ctrl Pts',(-30.624444340762,-33.6515470948858,1.14899876892822));
#22343=CARTESIAN_POINT('Ctrl Pts',(-31.4616172889162,-37.9057448084347,
0.991998641575964));
#22344=CARTESIAN_POINT('Ctrl Pts',(-35.4715119169482,-39.5541219888666,
0.83499851422371));
#22345=CARTESIAN_POINT('Ctrl Pts',(-39.0589599819549,-37.1191999333909,
0.677998386871458));
#22346=CARTESIAN_POINT('Ctrl Pts',(-39.0059690218246,-32.78311342986,0.520998259519202));
#22347=CARTESIAN_POINT('Ctrl Pts',(-35.3622594342876,-30.4366590393219,
0.36399813216695));
#22348=CARTESIAN_POINT('Ctrl Pts',(-31.3907386200676,-32.1786956644568,
0.206998004814696));
#22349=CARTESIAN_POINT('Ctrl Pts',(-30.6617260690046,-36.4578695691541,
0.0499978774624427));
#22350=CARTESIAN_POINT('Ctrl Pts',(-32.7606638781546,-38.426046814806,-0.0546688741057264));
#22351=CARTESIAN_POINT('Ctrl Pts',(-33.9957950511247,-38.756249785149,-0.107002249889811));
#22352=CARTESIAN_POINT('Ctrl Pts',(-31.9038714051976,-32.3528524834368,
8.32100674966943));
#22353=CARTESIAN_POINT('Ctrl Pts',(-31.0334355704763,-33.370922410012,8.26867337388535));
#22354=CARTESIAN_POINT('Ctrl Pts',(-30.3892451823686,-36.3158111513261,
8.16400662231718));
#22355=CARTESIAN_POINT('Ctrl Pts',(-33.5581020539921,-39.5777533604545,
8.00700649496493));
#22356=CARTESIAN_POINT('Ctrl Pts',(-38.0208447754587,-38.7249339026052,
7.85000636761267));
#22357=CARTESIAN_POINT('Ctrl Pts',(-39.7742804043327,-34.5367151947012,
7.69300624026042));
#22358=CARTESIAN_POINT('Ctrl Pts',(-37.2468182307978,-30.7615622415685,
7.53600611290816));
#22359=CARTESIAN_POINT('Ctrl Pts',(-32.7044906448315,-30.7882310811688,
7.37900598555592));
#22360=CARTESIAN_POINT('Ctrl Pts',(-30.2206288723714,-34.591050784955,7.22200585820366));
#22361=CARTESIAN_POINT('Ctrl Pts',(-32.0224449816578,-38.760868439734,7.06500573085141));
#22362=CARTESIAN_POINT('Ctrl Pts',(-36.4942781630208,-39.5581356918704,
6.90800560349915));
#22363=CARTESIAN_POINT('Ctrl Pts',(-39.6261703729353,-36.2681502201159,
6.75100547614691));
#22364=CARTESIAN_POINT('Ctrl Pts',(-38.6097349049326,-31.8409668964026,
6.59400534879464));
#22365=CARTESIAN_POINT('Ctrl Pts',(-34.3564136921927,-30.2465364275518,
6.4370052214424));
#22366=CARTESIAN_POINT('Ctrl Pts',(-30.6802034020135,-32.9145736277213,
6.28000509409013));
#22367=CARTESIAN_POINT('Ctrl Pts',(-30.8775957137286,-37.4526369907548,
6.12300496673789));
#22368=CARTESIAN_POINT('Ctrl Pts',(-34.7715877207675,-39.7913950861294,
5.96600483938563));
#22369=CARTESIAN_POINT('Ctrl Pts',(-38.8703990990513,-37.8336643077382,
5.80900471203337));
#22370=CARTESIAN_POINT('Ctrl Pts',(-39.498586529305,-33.3349590302252,5.65200458468112));
#22371=CARTESIAN_POINT('Ctrl Pts',(-36.0928482339355,-30.3293122267992,
5.49500445732888));
#22372=CARTESIAN_POINT('Ctrl Pts',(-31.7071424564414,-31.5119158276916,
5.33800432997661));
#22373=CARTESIAN_POINT('Ctrl Pts',(-30.2741736217725,-35.8223180338192,
5.18100420262437));
#22374=CARTESIAN_POINT('Ctrl Pts',(-33.0788986413239,-39.395339737909,5.02400407527211));
#22375=CARTESIAN_POINT('Ctrl Pts',(-37.6062936777584,-39.0270181479993,
4.86700394791986));
#22376=CARTESIAN_POINT('Ctrl Pts',(-39.7966001705114,-35.0476307433831,
4.7100038205676));
#22377=CARTESIAN_POINT('Ctrl Pts',(-37.6857492734788,-31.0255323981813,
4.55300369321535));
#22378=CARTESIAN_POINT('Ctrl Pts',(-33.1665612371704,-30.5673772788489,
4.39600356586309));
#22379=CARTESIAN_POINT('Ctrl Pts',(-30.291435328683,-34.0839974792893,4.23900343851084));
#22380=CARTESIAN_POINT('Ctrl Pts',(-31.6385245327839,-38.4220059271175,
4.08200331115859));
#22381=CARTESIAN_POINT('Ctrl Pts',(-35.9998810371616,-39.6914688314679,
3.92500318380634));
#22382=CARTESIAN_POINT('Ctrl Pts',(-39.4646346224728,-36.7540466258671,
3.76800305645408));
#22383=CARTESIAN_POINT('Ctrl Pts',(-38.9259075113142,-32.2437539848424,
3.61100292910183));
#22384=CARTESIAN_POINT('Ctrl Pts',(-34.8667814687478,-30.2050135847982,
3.45400280174957));
#22385=CARTESIAN_POINT('Ctrl Pts',(-30.9271137663599,-32.4659835103585,
3.29700267439732));
#22386=CARTESIAN_POINT('Ctrl Pts',(-30.6396422127733,-36.9992303202149,
3.14000254704507));
#22387=CARTESIAN_POINT('Ctrl Pts',(-34.2621453393335,-39.7397481467912,
2.98300241969281));
#22388=CARTESIAN_POINT('Ctrl Pts',(-38.5462897765416,-38.2300882894962,
2.82600229234056));
#22389=CARTESIAN_POINT('Ctrl Pts',(-39.6504422346313,-33.8239773747795,
2.66900216498831));
#22390=CARTESIAN_POINT('Ctrl Pts',(-36.5844983552314,-30.4724170292356,
2.51200203763606));
#22391=CARTESIAN_POINT('Ctrl Pts',(-32.0977199449364,-31.1807841743797,
2.3550019102838));
#22392=CARTESIAN_POINT('Ctrl Pts',(-30.2134432077683,-35.3138779741053,
2.19800178293155));
#22393=CARTESIAN_POINT('Ctrl Pts',(-32.621319267345,-39.1655160273689,2.04100165557929));
#22394=CARTESIAN_POINT('Ctrl Pts',(-37.1621783376115,-39.2818925846584,
1.88400152822705));
#22395=CARTESIAN_POINT('Ctrl Pts',(-39.7641970350665,-35.558661654829,1.72700140087479));
#22396=CARTESIAN_POINT('Ctrl Pts',(-38.0941030920961,-31.3344600185395,
1.57000127352254));
#22397=CARTESIAN_POINT('Ctrl Pts',(-33.6495202958365,-30.3972103260493,
1.41300114617028));
#22398=CARTESIAN_POINT('Ctrl Pts',(-30.4158791260905,-33.5872717453,1.25600101881803));
#22399=CARTESIAN_POINT('Ctrl Pts',(-31.2929567559004,-38.0442500262742,
1.09900089146578));
#22400=CARTESIAN_POINT('Ctrl Pts',(-35.4939870016774,-39.7711987453336,
0.942000764113521));
#22401=CARTESIAN_POINT('Ctrl Pts',(-39.2524343486202,-37.2202137070602,
0.785000636761268));
#22402=CARTESIAN_POINT('Ctrl Pts',(-39.1969175216432,-32.6774433254408,
0.628000509409014));
#22403=CARTESIAN_POINT('Ctrl Pts',(-35.3795268907121,-30.2191428513895,
0.471000382056761));
#22404=CARTESIAN_POINT('Ctrl Pts',(-31.2186995847689,-32.0442153857854,
0.314000254704507));
#22405=CARTESIAN_POINT('Ctrl Pts',(-30.4549379250093,-36.5273603729133,
0.157000127352253));
#22406=CARTESIAN_POINT('Ctrl Pts',(-32.6539236935135,-38.5893527455387,
0.0523333757840845));
#22407=CARTESIAN_POINT('Ctrl Pts',(-33.9479286229388,-38.9352951690526,
0.));
#22408=CARTESIAN_POINT('Ctrl Pts',(-33.9479286229388,-38.9352951690526,
5.55111512312578E-17));
#22409=CARTESIAN_POINT('Ctrl Pts',(-33.8318206360164,-38.8956805466085,
1.21569200333733E-16));
#22410=CARTESIAN_POINT('Ctrl Pts',(-33.7179777099102,-38.8505155072641,
1.50554103324791E-15));
#22411=CARTESIAN_POINT('Ctrl Pts',(-33.6066257375518,-38.8001576608968,
1.0547118733939E-15));
#22412=CARTESIAN_POINT('Ctrl Pts',(-33.492776560763,-38.7486704781164,5.93772317186044E-16));
#22413=CARTESIAN_POINT('Ctrl Pts',(-33.3815306925957,-38.6917544682482,
3.73522748729697E-15));
#22414=CARTESIAN_POINT('Ctrl Pts',(-33.2731538396993,-38.6297432688828,
2.72004641033163E-15));
#22415=CARTESIAN_POINT('Ctrl Pts',(-33.1592154520342,-38.5645498637963,
1.65276966251693E-15));
#22416=CARTESIAN_POINT('Ctrl Pts',(-33.048447119632,-38.4937244909346,-6.09647221355942E-16));
#22417=CARTESIAN_POINT('Ctrl Pts',(-32.9411967497889,-38.4176086362753,
-1.0547118733939E-15));
#22418=CARTESIAN_POINT('Ctrl Pts',(-32.8473526761762,-38.3510072634485,
-1.44414344392711E-15));
#22419=CARTESIAN_POINT('Ctrl Pts',(-32.7562023471369,-38.2803543077884,
-2.56653707031024E-15));
#22420=CARTESIAN_POINT('Ctrl Pts',(-32.6680103311015,-38.2058563963449,
-2.83106871279415E-15));
#22421=CARTESIAN_POINT('Ctrl Pts',(-32.6506345001076,-38.1911786151031,
-2.88318745685931E-15));
#22422=CARTESIAN_POINT('Ctrl Pts',(-32.6333736067294,-38.1763515287969,
-1.26352082166837E-15));
#22423=CARTESIAN_POINT('Ctrl Pts',(-32.6162298289787,-38.1613766467586,
-1.22124532708767E-15));
#22424=CARTESIAN_POINT('Ctrl Pts',(-32.6036955222168,-38.1504280817505,
-1.1903365025982E-15));
#22425=CARTESIAN_POINT('Ctrl Pts',(-32.5912250315541,-38.1394015059403,
9.6075348530294E-17));
#22426=CARTESIAN_POINT('Ctrl Pts',(-32.5788280068545,-38.1283056318751,
1.11022302462516E-16));
#22427=CARTESIAN_POINT('Ctrl Pts',(-32.4862488011484,-38.0454432328352,
2.22644014631185E-16));
#22428=CARTESIAN_POINT('Ctrl Pts',(-32.3976254460622,-37.9585991267844,
2.93313669984113E-16));
#22429=CARTESIAN_POINT('Ctrl Pts',(-32.3132193670584,-37.8680942341505,
1.66533453693773E-16));
#22430=CARTESIAN_POINT('Ctrl Pts',(-32.2290050385629,-37.7777949470768,
4.00412518592805E-17));
#22431=CARTESIAN_POINT('Ctrl Pts',(-32.1489883292395,-37.6838507826712,
-7.67367206503618E-16));
#22432=CARTESIAN_POINT('Ctrl Pts',(-32.0734693158047,-37.5865484422576,
-3.88578058618805E-16));
#22433=CARTESIAN_POINT('Ctrl Pts',(-31.9989826203281,-37.4905761901068,
-1.49668231824771E-17));
#22434=CARTESIAN_POINT('Ctrl Pts',(-31.9288710981801,-37.3913362593944,
6.39667558614738E-17));
#22435=CARTESIAN_POINT('Ctrl Pts',(-31.8634687260135,-37.2890829263301,
2.77555756156289E-16));
#22436=CARTESIAN_POINT('Ctrl Pts',(-31.8101631638829,-37.2057423498624,
4.51639376496992E-16));
#22437=CARTESIAN_POINT('Ctrl Pts',(-31.7599865782998,-37.1203994732574,
-1.91642689345195E-15));
#22438=CARTESIAN_POINT('Ctrl Pts',(-31.7131457346326,-37.0331861281649,
-2.08166817117217E-15));
#22439=CARTESIAN_POINT('Ctrl Pts',(-31.7012454402134,-37.0110288738836,
-2.12364905155618E-15));
#22440=CARTESIAN_POINT('Ctrl Pts',(-31.6895605787933,-36.988750873417,8.89729854294519E-16));
#22441=CARTESIAN_POINT('Ctrl Pts',(-31.6780948040882,-36.9663542633258,
9.71445146547012E-16));
#22442=CARTESIAN_POINT('Ctrl Pts',(-31.6699383315321,-36.9504218610016,
1.0295754129979E-15));
#22443=CARTESIAN_POINT('Ctrl Pts',(-31.661896440285,-36.9344366167593,-7.00903233658188E-16));
#22444=CARTESIAN_POINT('Ctrl Pts',(-31.6539727955662,-36.9184049530428,
-6.38378239159465E-16));
#22445=CARTESIAN_POINT('Ctrl Pts',(-31.6010119288307,-36.8112508799156,
-2.20467287978913E-16));
#22446=CARTESIAN_POINT('Ctrl Pts',(-31.5532899127003,-36.7019469405238,
-5.43579179869397E-17));
#22447=CARTESIAN_POINT('Ctrl Pts',(-31.5110855463215,-36.5907557494425,
2.77555756156289E-17));
#22448=CARTESIAN_POINT('Ctrl Pts',(-31.4697173372396,-36.4817674898051,
1.08242228141372E-16));
#22449=CARTESIAN_POINT('Ctrl Pts',(-31.433650039522,-36.3709653855926,-1.8533573671039E-16));
#22450=CARTESIAN_POINT('Ctrl Pts',(-31.4031944204139,-36.2585829650152,
-1.08246744900953E-15));
#22451=CARTESIAN_POINT('Ctrl Pts',(-31.3987402034729,-36.2421467310371,
-1.21367539645156E-15));
#22452=CARTESIAN_POINT('Ctrl Pts',(-31.3944061093602,-36.2256766793315,
1.54092145767103E-16));
#22453=CARTESIAN_POINT('Ctrl Pts',(-31.3901932043347,-36.2091735273543,
1.66533453693773E-16));
#22454=CARTESIAN_POINT('Ctrl Pts',(-31.3605246504064,-36.0929533297801,
3.08986100652746E-16));
#22455=CARTESIAN_POINT('Ctrl Pts',(-31.3368620771271,-35.9750912152647,
2.82593330474131E-15));
#22456=CARTESIAN_POINT('Ctrl Pts',(-31.319114629565,-35.8560230245863,3.49720252756924E-15));
#22457=CARTESIAN_POINT('Ctrl Pts',(-31.3091310875555,-35.7890431234222,
3.87481426369542E-15));
#22458=CARTESIAN_POINT('Ctrl Pts',(-31.3010203073581,-35.7216816160001,
-1.45794491220195E-16));
#22459=CARTESIAN_POINT('Ctrl Pts',(-31.294773164211,-35.6540175415704,-4.71844785465692E-16));
#22460=CARTESIAN_POINT('Ctrl Pts',(-31.2918906865937,-35.6227968418935,
-6.22286780009977E-16));
#22461=CARTESIAN_POINT('Ctrl Pts',(-31.2894050399855,-35.5915117486406,
3.58433295205778E-16));
#22462=CARTESIAN_POINT('Ctrl Pts',(-31.2873156755218,-35.5601701609149,
2.4980018054066E-16));
#22463=CARTESIAN_POINT('Ctrl Pts',(-31.286114583885,-35.5421531420771,1.87351370019253E-16));
#22464=CARTESIAN_POINT('Ctrl Pts',(-31.2850449634327,-35.5241245074566,
-4.29409397736477E-17));
#22465=CARTESIAN_POINT('Ctrl Pts',(-31.284106744896,-35.5060940976467,-5.55111512312578E-17));
#22466=CARTESIAN_POINT('Ctrl Pts',(-31.2777958135452,-35.3848124622,-1.40064737065375E-16));
#22467=CARTESIAN_POINT('Ctrl Pts',(-31.2774174094918,-35.2633335332142,
2.82866543587948E-15));
#22468=CARTESIAN_POINT('Ctrl Pts',(-31.282813324883,-35.142104562563,2.35922392732846E-15));
#22469=CARTESIAN_POINT('Ctrl Pts',(-31.2880973068045,-35.0233903791791,
1.89952056570822E-15));
#22470=CARTESIAN_POINT('Ctrl Pts',(-31.2989190268708,-34.9049149676345,
7.28996419448176E-16));
#22471=CARTESIAN_POINT('Ctrl Pts',(-31.3151832922329,-34.7871043083849,
6.93889390390723E-16));
#22472=CARTESIAN_POINT('Ctrl Pts',(-31.3312886503615,-34.670444698108,6.59125368578839E-16));
#22473=CARTESIAN_POINT('Ctrl Pts',(-31.3527310724264,-34.5544360772762,
1.70606179182567E-15));
#22474=CARTESIAN_POINT('Ctrl Pts',(-31.379464911652,-34.4395109622456,2.28983498828939E-15));
#22475=CARTESIAN_POINT('Ctrl Pts',(-31.3968718099089,-34.3646810896034,
2.66994053729605E-15));
#22476=CARTESIAN_POINT('Ctrl Pts',(-31.4165229694089,-34.2903109886468,
-2.96848706176688E-17));
#22477=CARTESIAN_POINT('Ctrl Pts',(-31.4384155905674,-34.2165269562934,
1.38777878078145E-17));
#22478=CARTESIAN_POINT('Ctrl Pts',(-31.4458039406444,-34.1916262257156,
2.85793700622958E-17));
#22479=CARTESIAN_POINT('Ctrl Pts',(-31.4534476413064,-34.1667922990885,
3.06223347651583E-15));
#22480=CARTESIAN_POINT('Ctrl Pts',(-31.4613467725894,-34.1420302077573,
3.1641356201817E-15));
#22481=CARTESIAN_POINT('Ctrl Pts',(-31.4664331829338,-34.1260853964884,
3.22975247083094E-15));
#22482=CARTESIAN_POINT('Ctrl Pts',(-31.4716247119601,-34.1101729821539,
1.52985938675526E-15));
#22483=CARTESIAN_POINT('Ctrl Pts',(-31.4769185004878,-34.0943023310132,
1.56819002228303E-15));
#22484=CARTESIAN_POINT('Ctrl Pts',(-31.5138161753674,-33.9836839859762,
1.8353543263008E-15));
#22485=CARTESIAN_POINT('Ctrl Pts',(-31.5557145621555,-33.8749771180903,
2.68190903327311E-15));
#22486=CARTESIAN_POINT('Ctrl Pts',(-31.60254886788,-33.7686009256992,2.26207941267376E-15));
#22487=CARTESIAN_POINT('Ctrl Pts',(-31.6406629427424,-33.6820312606289,
1.92041922701669E-15));
#22488=CARTESIAN_POINT('Ctrl Pts',(-31.6820469232643,-33.5970053442715,
1.26636124083292E-15));
#22489=CARTESIAN_POINT('Ctrl Pts',(-31.7266868713332,-33.5137647678308,
1.40165656858926E-15));
#22490=CARTESIAN_POINT('Ctrl Pts',(-31.7483018585373,-33.473459075901,1.46716754933025E-15));
#22491=CARTESIAN_POINT('Ctrl Pts',(-31.7706804998245,-33.4335722114158,
1.17298588323861E-16));
#22492=CARTESIAN_POINT('Ctrl Pts',(-31.7938226860146,-33.3941331271239,
-4.02455846426619E-16));
#22493=CARTESIAN_POINT('Ctrl Pts',(-31.8074090785167,-33.3709790968731,
-7.07595028060502E-16));
#22494=CARTESIAN_POINT('Ctrl Pts',(-31.8212607024029,-33.3479763354121,
-4.73580047421181E-16));
#22495=CARTESIAN_POINT('Ctrl Pts',(-31.8353634826968,-33.3251531939272,
-3.88578058618805E-16));
#22496=CARTESIAN_POINT('Ctrl Pts',(-31.8937949297824,-33.2305910468749,
-3.63929499130585E-17));
#22497=CARTESIAN_POINT('Ctrl Pts',(-31.9565776402818,-33.1390341079118,
1.65098064735663E-15));
#22498=CARTESIAN_POINT('Ctrl Pts',(-32.0236775684477,-33.0508730884183,
2.24126273096203E-15));
#22499=CARTESIAN_POINT('Ctrl Pts',(-32.0837083254303,-32.9720000868933,
2.76935689262062E-15));
#22500=CARTESIAN_POINT('Ctrl Pts',(-32.1471951806296,-32.895845207831,1.97196154581884E-15));
#22501=CARTESIAN_POINT('Ctrl Pts',(-32.2141372439519,-32.8227147610826,
2.21437451708439E-15));
#22502=CARTESIAN_POINT('Ctrl Pts',(-32.2489921734814,-32.7846377069649,
2.36892565463969E-15));
#22503=CARTESIAN_POINT('Ctrl Pts',(-32.2847842063358,-32.7473810647789,
1.32299506859179E-17));
#22504=CARTESIAN_POINT('Ctrl Pts',(-32.3214759334524,-32.7109602322923,
-5.55111512312578E-17));
#22505=CARTESIAN_POINT('Ctrl Pts',(-38.5163032009778,-35.0029832534533,
6.38741669750803));
#22506=CARTESIAN_POINT('Ctrl Pts',(-38.5189473067417,-35.316893543218,6.40161070716451));
#22507=CARTESIAN_POINT('Ctrl Pts',(-38.4802906988737,-35.6301637893069,
6.41580471682099));
#22508=CARTESIAN_POINT('Ctrl Pts',(-38.3977162601254,-35.9313946627094,
6.42999872647747));
#22509=CARTESIAN_POINT('Ctrl Pts',(-38.0932639427213,-37.0420342125665,
6.48233210226156));
#22510=CARTESIAN_POINT('Ctrl Pts',(-37.1917925750707,-37.9890105144279,
6.53466547804564));
#22511=CARTESIAN_POINT('Ctrl Pts',(-36.0974795738098,-38.3477575516811,
6.58699885382972));
#22512=CARTESIAN_POINT('Ctrl Pts',(-35.0031665725488,-38.7065045889344,
6.63933222961381));
#22513=CARTESIAN_POINT('Ctrl Pts',(-33.7160119376775,-38.4770223615795,
6.69166560539789));
#22514=CARTESIAN_POINT('Ctrl Pts',(-32.8131208374828,-37.7621694030232,
6.74399898118198));
#22515=CARTESIAN_POINT('Ctrl Pts',(-31.9102297372881,-37.0473164444669,
6.79633235696606));
#22516=CARTESIAN_POINT('Ctrl Pts',(-31.3916021717699,-35.8470927547091,
6.84866573275014));
#22517=CARTESIAN_POINT('Ctrl Pts',(-31.4897608240433,-34.6996866784948,
6.90099910853423));
#22518=CARTESIAN_POINT('Ctrl Pts',(-31.5879194763167,-33.5522806022806,
6.95333248431831));
#22519=CARTESIAN_POINT('Ctrl Pts',(-32.3028643463816,-32.4576921396098,
7.0056658601024));
#22520=CARTESIAN_POINT('Ctrl Pts',(-33.3140595130386,-31.9065597820401,
7.05799923588649));
#22521=CARTESIAN_POINT('Ctrl Pts',(-34.3252546796956,-31.3554274244703,
7.11033261167057));
#22522=CARTESIAN_POINT('Ctrl Pts',(-35.6327001429448,-31.3477511720016,
7.16266598745465));
#22523=CARTESIAN_POINT('Ctrl Pts',(-36.6501701924127,-31.8872255334987,
7.21499936323874));
#22524=CARTESIAN_POINT('Ctrl Pts',(-37.6676402418807,-32.4266998949958,
7.26733273902282));
#22525=CARTESIAN_POINT('Ctrl Pts',(-38.3951348775673,-33.5133248704587,
7.3196661148069));
#22526=CARTESIAN_POINT('Ctrl Pts',(-38.5065312349523,-34.6593974459546,
7.37199949059099));
#22527=CARTESIAN_POINT('Ctrl Pts',(-38.5174702113759,-34.7719402721061,
7.37713855956333));
#22528=CARTESIAN_POINT('Ctrl Pts',(-38.5224681626868,-34.8850563504433,
7.38227762853568));
#22529=CARTESIAN_POINT('Ctrl Pts',(-38.5217392653161,-34.9982348400382,
7.38741669750802));
#22530=CARTESIAN_POINT('Ctrl Pts',(-36.0520713770612,-38.9352951690526,
8.));
#22531=CARTESIAN_POINT('Ctrl Pts',(-37.3460763064865,-38.5893527455387,
7.94766662421592));
#22532=CARTESIAN_POINT('Ctrl Pts',(-39.5450618542894,-36.527358944407,7.84299987264775));
#22533=CARTESIAN_POINT('Ctrl Pts',(-38.7813006061664,-32.0442159203332,
7.6859997452955));
#22534=CARTESIAN_POINT('Ctrl Pts',(-34.6204730922247,-30.2191423808613,
7.52899961794324));
#22535=CARTESIAN_POINT('Ctrl Pts',(-30.8030823517117,-32.6774434597138,
7.37199949059099));
#22536=CARTESIAN_POINT('Ctrl Pts',(-30.7475655592404,-37.2202136561835,
7.21499936323873));
#22537=CARTESIAN_POINT('Ctrl Pts',(-34.5060129709306,-39.7711989299046,
7.05799923588648));
#22538=CARTESIAN_POINT('Ctrl Pts',(-38.7070433506006,-38.044250072918,6.90099910853423));
#22539=CARTESIAN_POINT('Ctrl Pts',(-39.584120987438,-33.5872717262032,6.74399898118198));
#22540=CARTESIAN_POINT('Ctrl Pts',(-36.3504797430715,-30.3972101963624,
6.58699885382972));
#22541=CARTESIAN_POINT('Ctrl Pts',(-31.905896825022,-31.3344599279876,6.42999872647746));
#22542=CARTESIAN_POINT('Ctrl Pts',(-30.2358028418083,-35.5586616666892,
6.27299859912522));
#22543=CARTESIAN_POINT('Ctrl Pts',(-32.83782160528,-39.2818926978495,6.11599847177295));
#22544=CARTESIAN_POINT('Ctrl Pts',(-37.3786807951101,-39.1655161353224,
5.95899834442071));
#22545=CARTESIAN_POINT('Ctrl Pts',(-39.7865569169479,-35.3138779826965,
5.80199821706845));
#22546=CARTESIAN_POINT('Ctrl Pts',(-37.9022801309199,-31.1807840744948,
5.64499808971621));
#22547=CARTESIAN_POINT('Ctrl Pts',(-33.4155016033557,-30.4724169111822,
5.48799796236394));
#22548=CARTESIAN_POINT('Ctrl Pts',(-30.3495576440316,-33.8239773440302,
5.3309978350117));
#22549=CARTESIAN_POINT('Ctrl Pts',(-31.4537101308888,-38.230088373826,5.17399770765944));
#22550=CARTESIAN_POINT('Ctrl Pts',(-35.7378546799324,-39.7397482704758,
5.01699758030718));
#22551=CARTESIAN_POINT('Ctrl Pts',(-39.3603579010204,-36.9992303723996,
4.85999745295493));
#22552=CARTESIAN_POINT('Ctrl Pts',(-39.0728863399384,-32.4659834442205,
4.70299732560268));
#22553=CARTESIAN_POINT('Ctrl Pts',(-35.1332185347277,-30.2050134596587,
4.54599719825043));
#22554=CARTESIAN_POINT('Ctrl Pts',(-31.0740923862265,-32.2437539129077,
4.38899707089817));
#22555=CARTESIAN_POINT('Ctrl Pts',(-30.535365261007,-36.7540466716456,4.23199694354592));
#22556=CARTESIAN_POINT('Ctrl Pts',(-34.0001189367432,-39.6914689539076,
4.07499681619366));
#22557=CARTESIAN_POINT('Ctrl Pts',(-38.3614755549453,-38.4220060164266,
3.91799668884141));
#22558=CARTESIAN_POINT('Ctrl Pts',(-39.7085647942032,-34.0839974553828,
3.76099656148916));
#22559=CARTESIAN_POINT('Ctrl Pts',(-36.8334388106793,-30.5673771631648,
3.6039964341369));
#22560=CARTESIAN_POINT('Ctrl Pts',(-32.3142506564274,-31.0255322944533,
3.44699630678465));
#22561=CARTESIAN_POINT('Ctrl Pts',(-30.2033997043049,-35.0476307446275,
3.28999617943239));
#22562=CARTESIAN_POINT('Ctrl Pts',(-32.3937062542216,-39.0270182530956,
3.13299605208014));
#22563=CARTESIAN_POINT('Ctrl Pts',(-36.9211014088136,-39.3953398526252,
2.97599592472789));
#22564=CARTESIAN_POINT('Ctrl Pts',(-39.7258265015647,-35.8223180552711,
2.81899579737564));
#22565=CARTESIAN_POINT('Ctrl Pts',(-38.2928576294957,-31.5119157366759,
2.66199567002338));
#22566=CARTESIAN_POINT('Ctrl Pts',(-33.9071517375455,-30.3293121048675,
2.50499554267113));
#22567=CARTESIAN_POINT('Ctrl Pts',(-30.5014133532831,-33.3349589868354,
2.34799541531887));
#22568=CARTESIAN_POINT('Ctrl Pts',(-31.12960079995,-37.8336643815683,2.19099528796663));
#22569=CARTESIAN_POINT('Ctrl Pts',(-35.2284122851668,-39.7913952114128,
2.03399516061437));
#22570=CARTESIAN_POINT('Ctrl Pts',(-39.1224043939168,-37.4526370543192,
1.87699503326212));
#22571=CARTESIAN_POINT('Ctrl Pts',(-39.3197967106052,-32.9145735741338,
1.71999490590986));
#22572=CARTESIAN_POINT('Ctrl Pts',(-35.6435863248602,-30.2465363019221,
1.56299477855761));
#22573=CARTESIAN_POINT('Ctrl Pts',(-31.3902650003177,-31.8409668168855,
1.40599465120536));
#22574=CARTESIAN_POINT('Ctrl Pts',(-30.3738295074692,-36.2681502477922,
1.2489945238531));
#22575=CARTESIAN_POINT('Ctrl Pts',(-33.5057217955833,-39.5581358207848,
1.09199439650085));
#22576=CARTESIAN_POINT('Ctrl Pts',(-37.977555101084,-38.7608685197788,0.934994269148597));
#22577=CARTESIAN_POINT('Ctrl Pts',(-39.7793712418172,-34.5910508068424,
0.777994141796343));
#22578=CARTESIAN_POINT('Ctrl Pts',(-37.2955094371433,-30.7882309135474,
0.620994014444089));
#22579=CARTESIAN_POINT('Ctrl Pts',(-32.7531816644513,-30.7615622313046,
0.463993887091836));
#22580=CARTESIAN_POINT('Ctrl Pts',(-30.2257195673566,-34.5367150123096,
0.306993759739581));
#22581=CARTESIAN_POINT('Ctrl Pts',(-31.9791549439529,-38.7249342807031,
0.149993632387329));
#22582=CARTESIAN_POINT('Ctrl Pts',(-36.441898406148,-39.5777530280863,-0.00700649496492615));
#22583=CARTESIAN_POINT('Ctrl Pts',(-39.6107538265857,-36.3158122035465,
-0.164006622317178));
#22584=CARTESIAN_POINT('Ctrl Pts',(-38.9665644295237,-33.3709224100119,
-0.268673373885348));
#22585=CARTESIAN_POINT('Ctrl Pts',(-38.0961285948024,-32.3528524834368,
-0.321006749669432));
#22586=CARTESIAN_POINT('Ctrl Pts',(-36.0042049488753,-38.756249785149,8.10700224988981));
#22587=CARTESIAN_POINT('Ctrl Pts',(-37.2393361218454,-38.4260468148059,
8.05466887410573));
#22588=CARTESIAN_POINT('Ctrl Pts',(-39.3382737203354,-36.457868205641,7.95000212253756));
#22589=CARTESIAN_POINT('Ctrl Pts',(-38.6092615621806,-32.178696174684,7.7930019951853));
#22590=CARTESIAN_POINT('Ctrl Pts',(-34.6377405494255,-30.4366585902015,
7.63600186783305));
#22591=CARTESIAN_POINT('Ctrl Pts',(-30.9940308572923,-32.7831135580239,
7.4790017404808));
#22592=CARTESIAN_POINT('Ctrl Pts',(-30.9410399300978,-37.119199884829,7.32200161312854));
#22593=CARTESIAN_POINT('Ctrl Pts',(-34.528488056906,-39.5541221650401,7.16500148577629));
#22594=CARTESIAN_POINT('Ctrl Pts',(-38.5383828127393,-37.9057448529564,
7.00800135842404));
#22595=CARTESIAN_POINT('Ctrl Pts',(-39.3755557676012,-33.6515470766578,
6.85100123107178));
#22596=CARTESIAN_POINT('Ctrl Pts',(-36.2890365339436,-30.6066247973054,
6.69400110371953));
#22597=CARTESIAN_POINT('Ctrl Pts',(-32.046670227525,-31.5012321778987,6.53700097636728));
#22598=CARTESIAN_POINT('Ctrl Pts',(-30.4525610448241,-35.5332440580251,
6.38000084901503));
#22599=CARTESIAN_POINT('Ctrl Pts',(-32.936194927768,-39.0870780552405,6.22300072166276));
#22600=CARTESIAN_POINT('Ctrl Pts',(-37.2704571936142,-38.975996314428,6.06600059431052));
#22601=CARTESIAN_POINT('Ctrl Pts',(-39.5687814048312,-35.2995973756527,
5.90900046695826));
#22602=CARTESIAN_POINT('Ctrl Pts',(-37.7702341628505,-31.3545481639004,
5.75200033960601));
#22603=CARTESIAN_POINT('Ctrl Pts',(-33.4875920340692,-30.678409808149,5.59500021225376));
#22604=CARTESIAN_POINT('Ctrl Pts',(-30.5611403084004,-33.8774832232266,
5.4380000849015));
#22605=CARTESIAN_POINT('Ctrl Pts',(-31.6150568161493,-38.0831280092054,
5.28099995754926));
#22606=CARTESIAN_POINT('Ctrl Pts',(-35.7042842693892,-39.5241024263299,
5.12399983019699));
#22607=CARTESIAN_POINT('Ctrl Pts',(-39.1619733019478,-36.908270748239,4.96699970284474));
#22608=CARTESIAN_POINT('Ctrl Pts',(-38.8875809264933,-32.581274406539,4.80999957549249));
#22609=CARTESIAN_POINT('Ctrl Pts',(-35.127157448413,-30.4231724970492,4.65299944814023));
#22610=CARTESIAN_POINT('Ctrl Pts',(-31.2527106615227,-32.3691557233429,
4.49599932078798));
#22611=CARTESIAN_POINT('Ctrl Pts',(-30.7384941767535,-36.6742422487958,
4.33899919343573));
#22612=CARTESIAN_POINT('Ctrl Pts',(-34.045610845517,-39.4780196892807,4.18199906608348));
#22613=CARTESIAN_POINT('Ctrl Pts',(-38.2085374256912,-38.2663139133921,
4.02499893873122));
#22614=CARTESIAN_POINT('Ctrl Pts',(-39.4943377146584,-34.1256731163465,
3.86799881137897));
#22615=CARTESIAN_POINT('Ctrl Pts',(-36.7500222582684,-30.7690496231526,
3.71099868402672));
#22616=CARTESIAN_POINT('Ctrl Pts',(-32.4364450539584,-31.206359923788,3.55399855667446));
#22617=CARTESIAN_POINT('Ctrl Pts',(-30.4216321632391,-35.0454636733936,
3.39699842932221));
#22618=CARTESIAN_POINT('Ctrl Pts',(-32.5122856349878,-38.843799714679,3.23999830196996));
#22619=CARTESIAN_POINT('Ctrl Pts',(-36.8336964431165,-39.1953636685035,
3.0829981746177));
#22620=CARTESIAN_POINT('Ctrl Pts',(-39.510814060595,-35.7849047875054,2.92599804726545));
#22621=CARTESIAN_POINT('Ctrl Pts',(-38.1430414319588,-31.6706142228596,
2.76899791991319));
#22622=CARTESIAN_POINT('Ctrl Pts',(-33.9568734047379,-30.5418158870118,
2.61199779256094));
#22623=CARTESIAN_POINT('Ctrl Pts',(-30.7060869898426,-33.4107138907526,
2.45499766520869));
#22624=CARTESIAN_POINT('Ctrl Pts',(-31.3056935911801,-37.7047402462095,
2.29799753785644));
#22625=CARTESIAN_POINT('Ctrl Pts',(-35.2180201383191,-39.5733995698641,
2.14099741050418));
#22626=CARTESIAN_POINT('Ctrl Pts',(-38.9348460417202,-37.3410486412263,
1.98399728315193));
#22627=CARTESIAN_POINT('Ctrl Pts',(-39.1232575369955,-33.0094548877283,
1.82699715579967));
#22628=CARTESIAN_POINT('Ctrl Pts',(-35.614304871841,-30.4628061612676,1.66999702844742));
#22629=CARTESIAN_POINT('Ctrl Pts',(-31.5544982689911,-31.9846943607513,
1.51299690109517));
#22630=CARTESIAN_POINT('Ctrl Pts',(-30.5843078670984,-36.2104528100627,
1.35599677374291));
#22631=CARTESIAN_POINT('Ctrl Pts',(-33.5737074493336,-39.3507528563925,
1.19899664639066));
#22632=CARTESIAN_POINT('Ctrl Pts',(-37.8420843236033,-38.5897590809672,
1.04199651903841));
#22633=CARTESIAN_POINT('Ctrl Pts',(-39.5619226586618,-34.6096568991787,
0.884996391686153));
#22634=CARTESIAN_POINT('Ctrl Pts',(-37.191069909542,-30.9798551197638,0.7279962643339));
#22635=CARTESIAN_POINT('Ctrl Pts',(-32.8554058774184,-30.954399791093,0.570996136981647));
#22636=CARTESIAN_POINT('Ctrl Pts',(-30.4429365323376,-34.5577932376814,
0.413996009629392));
#22637=CARTESIAN_POINT('Ctrl Pts',(-32.1165952983707,-38.5554597534685,
0.25699588227714));
#22638=CARTESIAN_POINT('Ctrl Pts',(-36.3762958928451,-39.3694775333344,
0.0999957549248847));
#22639=CARTESIAN_POINT('Ctrl Pts',(-39.4009768839417,-36.2559462745606,
-0.0570043724273669));
#22640=CARTESIAN_POINT('Ctrl Pts',(-38.7860963780679,-33.4450410745538,
-0.161671123995537));
#22641=CARTESIAN_POINT('Ctrl Pts',(-37.9552630411254,-32.4732906012887,
-0.214004499779622));
#22642=CARTESIAN_POINT('Ctrl Pts',(-35.9563385206894,-38.5772044012455,
8.21400449977962));
#22643=CARTESIAN_POINT('Ctrl Pts',(-37.1325959372043,-38.2627408840732,
8.16167112399554));
#22644=CARTESIAN_POINT('Ctrl Pts',(-39.1314855863814,-36.388377466875,8.05700437242737));
#22645=CARTESIAN_POINT('Ctrl Pts',(-38.4372225181948,-32.3131764290349,
7.90000424507512));
#22646=CARTESIAN_POINT('Ctrl Pts',(-34.6550080066264,-30.6541747995416,
7.74300411772286));
#22647=CARTESIAN_POINT('Ctrl Pts',(-31.184979362873,-32.8887836563341,7.58600399037061));
#22648=CARTESIAN_POINT('Ctrl Pts',(-31.1345143009551,-37.0181861134745,
7.42900386301835));
#22649=CARTESIAN_POINT('Ctrl Pts',(-34.5509631428814,-39.3370454001755,
7.2720037356661));
#22650=CARTESIAN_POINT('Ctrl Pts',(-38.3697222748781,-37.7672396329946,
7.11500360831385));
#22651=CARTESIAN_POINT('Ctrl Pts',(-39.1669905477644,-33.7158224271125,
6.95800348096159));
#22652=CARTESIAN_POINT('Ctrl Pts',(-36.2275933248156,-30.8160393982482,
6.80100335360935));
#22653=CARTESIAN_POINT('Ctrl Pts',(-32.187443630028,-31.6680044278098,6.64400322625708));
#22654=CARTESIAN_POINT('Ctrl Pts',(-30.6693192478399,-35.5078264493611,
6.48700309890484));
#22655=CARTESIAN_POINT('Ctrl Pts',(-33.0345682502559,-38.8922634126314,
6.33000297155257));
#22656=CARTESIAN_POINT('Ctrl Pts',(-37.1622335921182,-38.7864764935337,
6.17300284420033));
#22657=CARTESIAN_POINT('Ctrl Pts',(-39.3510058927144,-35.2853167686088,
6.01600271684807));
#22658=CARTESIAN_POINT('Ctrl Pts',(-37.6381881947812,-31.5283122533059,
5.85900258949583));
#22659=CARTESIAN_POINT('Ctrl Pts',(-33.5596824647827,-30.8844027051158,
5.70200246214357));
#22660=CARTESIAN_POINT('Ctrl Pts',(-30.7727229727691,-33.9309891024229,
5.54500233479131));
#22661=CARTESIAN_POINT('Ctrl Pts',(-31.7764035014098,-37.9361676445846,
5.38800220743907));
#22662=CARTESIAN_POINT('Ctrl Pts',(-35.6707138588461,-39.3084565821841,
5.2310020800868));
#22663=CARTESIAN_POINT('Ctrl Pts',(-38.9635887028751,-36.8173111240784,
5.07400195273455));
#22664=CARTESIAN_POINT('Ctrl Pts',(-38.7022755130482,-32.6965653688576,
4.9170018253823));
#22665=CARTESIAN_POINT('Ctrl Pts',(-35.1210963620983,-30.6413315344396,
4.76000169803004));
#22666=CARTESIAN_POINT('Ctrl Pts',(-31.431328936819,-32.4945575337781,4.6030015706778));
#22667=CARTESIAN_POINT('Ctrl Pts',(-30.9416230925,-36.5944378259461,4.44600144332554));
#22668=CARTESIAN_POINT('Ctrl Pts',(-34.0911027542909,-39.2645704246538,
4.28900131597328));
#22669=CARTESIAN_POINT('Ctrl Pts',(-38.0555992964371,-38.1106218103576,
4.13200118862104));
#22670=CARTESIAN_POINT('Ctrl Pts',(-39.2801106351136,-34.1673487773102,
3.97500106126878));
#22671=CARTESIAN_POINT('Ctrl Pts',(-36.6666057058575,-30.9707220831404,
3.81800093391653));
#22672=CARTESIAN_POINT('Ctrl Pts',(-32.5586394514893,-31.3871875531226,
3.66100080656427));
#22673=CARTESIAN_POINT('Ctrl Pts',(-30.6398646221734,-35.0432966021599,
3.50400067921202));
#22674=CARTESIAN_POINT('Ctrl Pts',(-32.6308650157539,-38.6605811762622,
3.34700055185977));
#22675=CARTESIAN_POINT('Ctrl Pts',(-36.7462914774195,-38.9953874843817,
3.19000042450751));
#22676=CARTESIAN_POINT('Ctrl Pts',(-39.2958016196254,-35.7474915197397,
3.03300029715526));
#22677=CARTESIAN_POINT('Ctrl Pts',(-37.9932252344219,-31.8293127090433,
2.876000169803));
#22678=CARTESIAN_POINT('Ctrl Pts',(-34.0065950719303,-30.754319669156,2.71900004245075));
#22679=CARTESIAN_POINT('Ctrl Pts',(-30.910760626402,-33.4864687946697,2.5619999150985));
#22680=CARTESIAN_POINT('Ctrl Pts',(-31.4817863824102,-37.5758161108508,
2.40499978774625));
#22681=CARTESIAN_POINT('Ctrl Pts',(-35.2076279914714,-39.3554039283154,
2.24799966039399));
#22682=CARTESIAN_POINT('Ctrl Pts',(-38.7472876895237,-37.2294602281335,
2.09099953304174));
#22683=CARTESIAN_POINT('Ctrl Pts',(-38.9267183633859,-33.1043362013228,
1.93399940568948));
#22684=CARTESIAN_POINT('Ctrl Pts',(-35.5850234188216,-30.6790760206131,
1.77699927833723));
#22685=CARTESIAN_POINT('Ctrl Pts',(-31.7187315376645,-32.128421904617,1.61999915098498));
#22686=CARTESIAN_POINT('Ctrl Pts',(-30.7947862267274,-36.1527553723333,
1.46299902363272));
#22687=CARTESIAN_POINT('Ctrl Pts',(-33.6416931030839,-39.1433698920001,
1.30599889628047));
#22688=CARTESIAN_POINT('Ctrl Pts',(-37.7066135461226,-38.4186496421557,
1.14899876892822));
#22689=CARTESIAN_POINT('Ctrl Pts',(-39.3444740755065,-34.628262991515,0.991998641575964));
#22690=CARTESIAN_POINT('Ctrl Pts',(-37.0866303819407,-31.1714793259802,
0.83499851422371));
#22691=CARTESIAN_POINT('Ctrl Pts',(-32.9576300903856,-31.1472373508815,
0.677998386871457));
#22692=CARTESIAN_POINT('Ctrl Pts',(-30.6601534973185,-34.5788714630532,
0.520998259519203));
#22693=CARTESIAN_POINT('Ctrl Pts',(-32.2540356527884,-38.3859852262338,
0.363998132166951));
#22694=CARTESIAN_POINT('Ctrl Pts',(-36.3106933795422,-39.1612020385825,
0.206998004814695));
#22695=CARTESIAN_POINT('Ctrl Pts',(-39.1911999412976,-36.1960803455747,
0.049997877462444));
#22696=CARTESIAN_POINT('Ctrl Pts',(-38.6056283266121,-33.5191597390956,
-0.0546688741057268));
#22697=CARTESIAN_POINT('Ctrl Pts',(-37.8143974874483,-32.5937287191406,
-0.107002249889811));
#22698=CARTESIAN_POINT('Ctrl Pts',(-35.9084720925035,-38.3981590173419,
8.32100674966943));
#22699=CARTESIAN_POINT('Ctrl Pts',(-37.0258557525633,-38.0994349533404,
8.26867337388535));
#22700=CARTESIAN_POINT('Ctrl Pts',(-38.9246974524274,-36.318886728109,8.16400662231718));
#22701=CARTESIAN_POINT('Ctrl Pts',(-38.265183474209,-32.4476566833857,8.00700649496493));
#22702=CARTESIAN_POINT('Ctrl Pts',(-34.6722754638272,-30.8716910088818,
7.85000636761267));
#22703=CARTESIAN_POINT('Ctrl Pts',(-31.3759278684536,-32.9944537546442,
7.69300624026043));
#22704=CARTESIAN_POINT('Ctrl Pts',(-31.3279886718125,-36.9171723421199,
7.53600611290816));
#22705=CARTESIAN_POINT('Ctrl Pts',(-34.5734382288568,-39.119968635311,7.37900598555592));
#22706=CARTESIAN_POINT('Ctrl Pts',(-38.2010617370167,-37.6287344130329,
7.22200585820366));
#22707=CARTESIAN_POINT('Ctrl Pts',(-38.9584253279276,-33.7800977775671,
7.0650057308514));
#22708=CARTESIAN_POINT('Ctrl Pts',(-36.1661501156877,-31.0254539991911,
6.90800560349916));
#22709=CARTESIAN_POINT('Ctrl Pts',(-32.328217032531,-31.834776677721,6.75100547614689));
#22710=CARTESIAN_POINT('Ctrl Pts',(-30.8860774508557,-35.482408840697,6.59400534879465));
#22711=CARTESIAN_POINT('Ctrl Pts',(-33.1329415727439,-38.6974487700223,
6.43700522144238));
#22712=CARTESIAN_POINT('Ctrl Pts',(-37.0540099906223,-38.5969566726394,
6.28000509409015));
#22713=CARTESIAN_POINT('Ctrl Pts',(-39.1332303805976,-35.271036161565,6.12300496673788));
#22714=CARTESIAN_POINT('Ctrl Pts',(-37.5061422267118,-31.7020763427115,
5.96600483938563));
#22715=CARTESIAN_POINT('Ctrl Pts',(-33.6317728954962,-31.0903956020826,
5.80900471203338));
#22716=CARTESIAN_POINT('Ctrl Pts',(-30.9843056371378,-33.9844949816193,
5.65200458468112));
#22717=CARTESIAN_POINT('Ctrl Pts',(-31.9377501866703,-37.7892072799639,
5.49500445732888));
#22718=CARTESIAN_POINT('Ctrl Pts',(-35.6371434483029,-39.0928107380382,
5.33800432997661));
#22719=CARTESIAN_POINT('Ctrl Pts',(-38.7652041038025,-36.7263514999179,
5.18100420262437));
#22720=CARTESIAN_POINT('Ctrl Pts',(-38.5169700996031,-32.8118563311761,
5.02400407527211));
#22721=CARTESIAN_POINT('Ctrl Pts',(-35.1150352757837,-30.85949057183,4.86700394791986));
#22722=CARTESIAN_POINT('Ctrl Pts',(-31.6099472121153,-32.6199593442133,
4.7100038205676));
#22723=CARTESIAN_POINT('Ctrl Pts',(-31.1447520082465,-36.5146334030964,
4.55300369321535));
#22724=CARTESIAN_POINT('Ctrl Pts',(-34.1365946630648,-39.0511211600269,
4.3960035658631));
#22725=CARTESIAN_POINT('Ctrl Pts',(-37.902661167183,-37.9549297073231,4.23900343851084));
#22726=CARTESIAN_POINT('Ctrl Pts',(-39.0658835555688,-34.2090244382739,
4.08200331115859));
#22727=CARTESIAN_POINT('Ctrl Pts',(-36.5831891534466,-31.1723945431281,
3.92500318380633));
#22728=CARTESIAN_POINT('Ctrl Pts',(-32.6808338490201,-31.5680151824572,
3.76800305645409));
#22729=CARTESIAN_POINT('Ctrl Pts',(-30.8580970811077,-35.041129530926,3.61100292910183));
#22730=CARTESIAN_POINT('Ctrl Pts',(-32.74944439652,-38.4773626378456,3.45400280174958));
#22731=CARTESIAN_POINT('Ctrl Pts',(-36.6588865117225,-38.79541130026,3.29700267439732));
#22732=CARTESIAN_POINT('Ctrl Pts',(-39.0807891786557,-35.710078251974,3.14000254704507));
#22733=CARTESIAN_POINT('Ctrl Pts',(-37.8434090368849,-31.988011195227,2.98300241969281));
#22734=CARTESIAN_POINT('Ctrl Pts',(-34.0563167391228,-30.9668234513003,
2.82600229234056));
#22735=CARTESIAN_POINT('Ctrl Pts',(-31.1154342629614,-33.5622236985868,
2.66900216498831));
#22736=CARTESIAN_POINT('Ctrl Pts',(-31.6578791736403,-37.446891975492,2.51200203763606));
#22737=CARTESIAN_POINT('Ctrl Pts',(-35.1972358446236,-39.1374082867668,
2.3550019102838));
#22738=CARTESIAN_POINT('Ctrl Pts',(-38.5597293373271,-37.1178718150406,
2.19800178293155));
#22739=CARTESIAN_POINT('Ctrl Pts',(-38.7301791897763,-33.1992175149173,
2.04100165557929));
#22740=CARTESIAN_POINT('Ctrl Pts',(-35.5557419658023,-30.8953458799586,
1.88400152822704));
#22741=CARTESIAN_POINT('Ctrl Pts',(-31.8829648063379,-32.2721494484828,
1.72700140087479));
#22742=CARTESIAN_POINT('Ctrl Pts',(-31.0052645863564,-36.0950579346039,
1.57000127352254));
#22743=CARTESIAN_POINT('Ctrl Pts',(-33.7096787568343,-38.9359869276078,
1.41300114617028));
#22744=CARTESIAN_POINT('Ctrl Pts',(-37.5711427686419,-38.247540203344,1.25600101881803));
#22745=CARTESIAN_POINT('Ctrl Pts',(-39.1270254923511,-34.6468690838513,
1.09900089146578));
#22746=CARTESIAN_POINT('Ctrl Pts',(-36.9821908543394,-31.3631035321966,
0.94200076411352));
#22747=CARTESIAN_POINT('Ctrl Pts',(-33.0598543033527,-31.3400749106699,
0.785000636761268));
#22748=CARTESIAN_POINT('Ctrl Pts',(-30.8773704622995,-34.599949688425,0.628000509409013));
#22749=CARTESIAN_POINT('Ctrl Pts',(-32.3914760072062,-38.2165106989991,
0.471000382056762));
#22750=CARTESIAN_POINT('Ctrl Pts',(-36.2450908662393,-38.9529265438306,
0.314000254704506));
#22751=CARTESIAN_POINT('Ctrl Pts',(-38.9814229986536,-36.1362144165888,
0.157000127352255));
#22752=CARTESIAN_POINT('Ctrl Pts',(-38.4251602751564,-33.5932784036374,
0.0523333757840841));
#22753=CARTESIAN_POINT('Ctrl Pts',(-37.6735319337713,-32.7141668369925,
0.));
#22754=CARTESIAN_POINT('Ctrl Pts',(-37.6735319337713,-32.7141668369925,
0.));
#22755=CARTESIAN_POINT('Ctrl Pts',(-37.7506744675535,-32.7912795750214,
1.11409720010452E-16));
#22756=CARTESIAN_POINT('Ctrl Pts',(-37.8237046409441,-32.8720144826054,
2.54111086902063E-16));
#22757=CARTESIAN_POINT('Ctrl Pts',(-37.8926301480271,-32.9559530569886,
5.55111512312578E-17));
#22758=CARTESIAN_POINT('Ctrl Pts',(-37.9633155600031,-33.0420348714294,
-1.48159722809431E-16));
#22759=CARTESIAN_POINT('Ctrl Pts',(-38.0296843928246,-33.1314864952968,
-2.01877327443104E-15));
#22760=CARTESIAN_POINT('Ctrl Pts',(-38.0917150717573,-33.2239026806474,
-1.83186799063151E-15));
#22761=CARTESIAN_POINT('Ctrl Pts',(-38.155036796301,-33.318242325688,-1.64107264387499E-15));
#22762=CARTESIAN_POINT('Ctrl Pts',(-38.2138383235334,-33.4156718046105,
-8.85373385211783E-16));
#22763=CARTESIAN_POINT('Ctrl Pts',(-38.268059911681,-33.515799485594,-9.43689570931383E-16));
#22764=CARTESIAN_POINT('Ctrl Pts',(-38.319849146258,-33.6114354884346,-9.99389721462685E-16));
#22765=CARTESIAN_POINT('Ctrl Pts',(-38.3674601237765,-33.7095338759835,
-7.11957983305256E-16));
#22766=CARTESIAN_POINT('Ctrl Pts',(-38.4108052730721,-33.809777999414,-7.21644966006352E-16));
#22767=CARTESIAN_POINT('Ctrl Pts',(-38.4178427440334,-33.8260535254913,
-7.23217733907022E-16));
#22768=CARTESIAN_POINT('Ctrl Pts',(-38.4247676868796,-33.8423856539009,
2.30001299369943E-15));
#22769=CARTESIAN_POINT('Ctrl Pts',(-38.4315796332288,-33.8587730721181,
2.33146835171283E-15));
#22770=CARTESIAN_POINT('Ctrl Pts',(-38.4380896782009,-33.8744342097871,
2.3615296271221E-15));
#22771=CARTESIAN_POINT('Ctrl Pts',(-38.4444935030833,-33.8901386536763,
1.24943603957411E-15));
#22772=CARTESIAN_POINT('Ctrl Pts',(-38.4507888941826,-33.9058797515619,
1.16573417585641E-15));
#22773=CARTESIAN_POINT('Ctrl Pts',(-38.4941742238636,-34.0143611327099,
5.88894247237743E-16));
#22774=CARTESIAN_POINT('Ctrl Pts',(-38.5324456986686,-34.1246595013341,
-1.81750747552515E-15));
#22775=CARTESIAN_POINT('Ctrl Pts',(-38.5655747031801,-34.2363430523647,
-1.22124532708767E-15));
#22776=CARTESIAN_POINT('Ctrl Pts',(-38.5991382485882,-34.3494915152183,
-6.17162228628305E-16));
#22777=CARTESIAN_POINT('Ctrl Pts',(-38.6274239303319,-34.4640624881056,
-2.28097715513866E-15));
#22778=CARTESIAN_POINT('Ctrl Pts',(-38.6503593525615,-34.5796394751672,
-2.85882428840978E-15));
#22779=CARTESIAN_POINT('Ctrl Pts',(-38.6743343050071,-34.7004548994865,
-3.46286189462104E-15));
#22780=CARTESIAN_POINT('Ctrl Pts',(-38.6924637958468,-34.8223704157046,
7.50012201101083E-16));
#22781=CARTESIAN_POINT('Ctrl Pts',(-38.7046094044796,-34.9449336658503,
9.15933995315754E-16));
#22782=CARTESIAN_POINT('Ctrl Pts',(-38.7137186109542,-35.0368561034595,
1.04037534097676E-15));
#22783=CARTESIAN_POINT('Ctrl Pts',(-38.7194607604909,-35.1291434881023,
1.55226768069038E-15));
#22784=CARTESIAN_POINT('Ctrl Pts',(-38.7217543278029,-35.2216084347256,
1.52655665885959E-15));
#22785=CARTESIAN_POINT('Ctrl Pts',(-38.7223018974601,-35.2436836530358,
1.52041837142613E-15));
#22786=CARTESIAN_POINT('Ctrl Pts',(-38.7226527519925,-35.2657735186889,
2.89381252678048E-15));
#22787=CARTESIAN_POINT('Ctrl Pts',(-38.722805679631,-35.2878464184275,2.85882428840978E-15));
#22788=CARTESIAN_POINT('Ctrl Pts',(-38.7236405005601,-35.4083407832928,
2.66782602310891E-15));
#22789=CARTESIAN_POINT('Ctrl Pts',(-38.7185871650491,-35.5284803305467,
-1.0113839359997E-15));
#22790=CARTESIAN_POINT('Ctrl Pts',(-38.7075767134548,-35.6478390239293,
-6.10622663543836E-16));
#22791=CARTESIAN_POINT('Ctrl Pts',(-38.696636914708,-35.766431805807,-2.12433031749896E-16));
#22792=CARTESIAN_POINT('Ctrl Pts',(-38.6798164549903,-35.8842545994116,
4.47017550934916E-16));
#22793=CARTESIAN_POINT('Ctrl Pts',(-38.6569982586142,-36.0009023628565,
1.11022302462516E-15));
#22794=CARTESIAN_POINT('Ctrl Pts',(-38.6541246129484,-36.0155925835174,
1.19374485534308E-15));
#22795=CARTESIAN_POINT('Ctrl Pts',(-38.6511557754508,-36.0302641749016,
1.91345521755541E-15));
#22796=CARTESIAN_POINT('Ctrl Pts',(-38.6480914530901,-36.044916331709,1.97064586870965E-15));
#22797=CARTESIAN_POINT('Ctrl Pts',(-38.6241809707793,-36.1592450787926,
2.44399783547239E-15));
#22798=CARTESIAN_POINT('Ctrl Pts',(-38.594461283178,-36.2723911010901,-8.48644965904397E-16));
#22799=CARTESIAN_POINT('Ctrl Pts',(-38.5592385353076,-36.3840879064664,
-8.60422844084496E-16));
#22800=CARTESIAN_POINT('Ctrl Pts',(-38.5372732895732,-36.4537431130068,
-8.67767642662035E-16));
#22801=CARTESIAN_POINT('Ctrl Pts',(-38.5131668858195,-36.5228346461715,
9.22437028861002E-17));
#22802=CARTESIAN_POINT('Ctrl Pts',(-38.4869837165243,-36.5912956919754,
8.32667268468867E-17));
#22803=CARTESIAN_POINT('Ctrl Pts',(-38.4780341824549,-36.6146960089858,
8.01983529614736E-17));
#22804=CARTESIAN_POINT('Ctrl Pts',(-38.4688419572729,-36.6380226459113,
-1.61456985271483E-15));
#22805=CARTESIAN_POINT('Ctrl Pts',(-38.4594094252689,-36.6612728659742,
-1.77635683940025E-15));
#22806=CARTESIAN_POINT('Ctrl Pts',(-38.4526602969819,-36.6779087722017,
-1.89211802927477E-15));
#22807=CARTESIAN_POINT('Ctrl Pts',(-38.4457875924452,-36.6945066762169,
2.33562128204704E-15));
#22808=CARTESIAN_POINT('Ctrl Pts',(-38.4387992548886,-36.7110492733397,
2.24820162486594E-15));
#22809=CARTESIAN_POINT('Ctrl Pts',(-38.3928779298073,-36.8197529491441,
1.67375506108868E-15));
#22810=CARTESIAN_POINT('Ctrl Pts',(-38.341903576542,-36.9262302239648,1.3366443388947E-15));
#22811=CARTESIAN_POINT('Ctrl Pts',(-38.2862346344182,-37.0302267509451,
1.30451205393456E-15));
#22812=CARTESIAN_POINT('Ctrl Pts',(-38.2286504882323,-37.1378011179799,
1.2712743072873E-15));
#22813=CARTESIAN_POINT('Ctrl Pts',(-38.1660430056126,-37.2427217973211,
4.33181580130382E-15));
#22814=CARTESIAN_POINT('Ctrl Pts',(-38.098753525921,-37.3446999432836,3.3584246494911E-15));
#22815=CARTESIAN_POINT('Ctrl Pts',(-38.030830880622,-37.4476376605642,2.37587429771653E-15));
#22816=CARTESIAN_POINT('Ctrl Pts',(-37.9581372777995,-37.5475779522675,
-1.61807423508707E-16));
#22817=CARTESIAN_POINT('Ctrl Pts',(-37.8809732699071,-37.6442054678576,
-4.30211422042248E-16));
#22818=CARTESIAN_POINT('Ctrl Pts',(-37.826560213076,-37.7123434332233,-6.19479481397997E-16));
#22819=CARTESIAN_POINT('Ctrl Pts',(-37.769923167717,-37.7788337520814,-1.16007728999665E-15));
#22820=CARTESIAN_POINT('Ctrl Pts',(-37.7111544669349,-37.8435573649047,
-1.58206781009085E-15));
#22821=CARTESIAN_POINT('Ctrl Pts',(-37.6849217834628,-37.8724481524459,
-1.77043242585642E-15));
#22822=CARTESIAN_POINT('Ctrl Pts',(-37.6582642395734,-37.9009868195143,
-1.55320898075906E-15));
#22823=CARTESIAN_POINT('Ctrl Pts',(-37.6311894369306,-37.9291622039588,
-1.76247905159244E-15));
#22824=CARTESIAN_POINT('Ctrl Pts',(-37.6195672281553,-37.9412568516894,
-1.85231093276087E-15));
#22825=CARTESIAN_POINT('Ctrl Pts',(-37.6078695516101,-37.9532830190668,
-1.32384934798458E-15));
#22826=CARTESIAN_POINT('Ctrl Pts',(-37.5961035133295,-37.9652334405448,
-1.346145417358E-15));
#22827=CARTESIAN_POINT('Ctrl Pts',(-37.5076612499423,-38.0550616646887,
-1.51373919811968E-15));
#22828=CARTESIAN_POINT('Ctrl Pts',(-37.4152596553304,-38.1407172584711,
9.39449970766038E-16));
#22829=CARTESIAN_POINT('Ctrl Pts',(-37.3192274679083,-38.221882071393,-9.29811783123569E-16));
#22830=CARTESIAN_POINT('Ctrl Pts',(-37.2371876089162,-38.2912208002711,
-2.52671355975721E-15));
#22831=CARTESIAN_POINT('Ctrl Pts',(-37.1524970590086,-38.3572819982496,
-3.43309726072543E-16));
#22832=CARTESIAN_POINT('Ctrl Pts',(-37.0653365594432,-38.419849736978,-1.11022302462516E-16));
#22833=CARTESIAN_POINT('Ctrl Pts',(-37.0262256852631,-38.4479252869043,
-6.78971724635936E-18));
#22834=CARTESIAN_POINT('Ctrl Pts',(-36.9866172085179,-38.4752971710175,
-3.75915299087743E-16));
#22835=CARTESIAN_POINT('Ctrl Pts',(-36.9465262167991,-38.5019445229708,
-5.06539254985228E-16));
#22836=CARTESIAN_POINT('Ctrl Pts',(-36.9192926653871,-38.5200458968282,
-5.95271263500483E-16));
#22837=CARTESIAN_POINT('Ctrl Pts',(-36.8918308185162,-38.5378163160328,
-1.49578843933597E-15));
#22838=CARTESIAN_POINT('Ctrl Pts',(-36.8641753660581,-38.555230466303,-1.48492329543615E-15));
#22839=CARTESIAN_POINT('Ctrl Pts',(-36.7573710739483,-38.6224832438564,
-1.44296252821847E-15));
#22840=CARTESIAN_POINT('Ctrl Pts',(-36.6476200524945,-38.6844692154967,
-2.67652767243929E-15));
#22841=CARTESIAN_POINT('Ctrl Pts',(-36.5352242775472,-38.7408547238633,
-3.18495230189342E-15));
#22842=CARTESIAN_POINT('Ctrl Pts',(-36.4331305324386,-38.792072020258,-3.64677548475584E-15));
#22843=CARTESIAN_POINT('Ctrl Pts',(-36.3288538528326,-38.8386685011131,
8.48923205726707E-17));
#22844=CARTESIAN_POINT('Ctrl Pts',(-36.2225972039516,-38.8803649981066,
1.52308721190764E-15));
#22845=CARTESIAN_POINT('Ctrl Pts',(-36.1671666977136,-38.9021166528128,
2.30316661476457E-15));
#22846=CARTESIAN_POINT('Ctrl Pts',(-36.1111970366882,-38.922534339231,-1.9802954995054E-18));
#22847=CARTESIAN_POINT('Ctrl Pts',(-36.0547323436802,-38.9416301693299,
1.11022302462516E-16));
#22848=CARTESIAN_POINT('Ctrl Pts',(-38.5153122961063,-34.9971887940747,
7.11258330249198));
#22849=CARTESIAN_POINT('Ctrl Pts',(-38.5180434423612,-34.646197163443,7.09672411194512));
#22850=CARTESIAN_POINT('Ctrl Pts',(-38.4695960103246,-34.2959413770096,
7.08086492139826));
#22851=CARTESIAN_POINT('Ctrl Pts',(-38.3668188607358,-33.9624299204154,
7.0650057308514));
#22852=CARTESIAN_POINT('Ctrl Pts',(-38.0276669238477,-32.8618831847751,
7.01267235506732));
#22853=CARTESIAN_POINT('Ctrl Pts',(-37.0969085197677,-31.9436685919831,
6.96033897928324));
#22854=CARTESIAN_POINT('Ctrl Pts',(-35.9918738038683,-31.6194484086754,
6.90800560349915));
#22855=CARTESIAN_POINT('Ctrl Pts',(-34.8868390879688,-31.2952282253677,
6.85567222771507));
#22856=CARTESIAN_POINT('Ctrl Pts',(-33.6075280602499,-31.5650024515443,
6.80333885193098));
#22857=CARTESIAN_POINT('Ctrl Pts',(-32.7275159494446,-32.307828258462,6.75100547614689));
#22858=CARTESIAN_POINT('Ctrl Pts',(-31.8475038386392,-33.0506540653796,
6.69867210036281));
#22859=CARTESIAN_POINT('Ctrl Pts',(-31.3667906447475,-34.2665314530383,
6.64633872457873));
#22860=CARTESIAN_POINT('Ctrl Pts',(-31.5009114014496,-35.4103101350885,
6.59400534879465));
#22861=CARTESIAN_POINT('Ctrl Pts',(-31.6350321581518,-36.5540888171387,
6.54167197301056));
#22862=CARTESIAN_POINT('Ctrl Pts',(-32.3839868654478,-37.6257687935805,
6.48933859722647));
#22863=CARTESIAN_POINT('Ctrl Pts',(-33.4119756220756,-38.1448600989042,
6.43700522144239));
#22864=CARTESIAN_POINT('Ctrl Pts',(-34.4399643787034,-38.663951404228,6.3846718456583));
#22865=CARTESIAN_POINT('Ctrl Pts',(-35.7469871846628,-38.6304540384337,
6.33233846987422));
#22866=CARTESIAN_POINT('Ctrl Pts',(-36.7470353193051,-38.0593852703575,
6.28000509409014));
#22867=CARTESIAN_POINT('Ctrl Pts',(-37.7470834539474,-37.4883165022812,
6.22767171830606));
#22868=CARTESIAN_POINT('Ctrl Pts',(-38.4401569172725,-36.3796763319231,
6.17533834252197));
#22869=CARTESIAN_POINT('Ctrl Pts',(-38.5155122899541,-35.2305296102685,
6.12300496673788));
#22870=CARTESIAN_POINT('Ctrl Pts',(-38.5205143775731,-35.1542492816832,
6.11953107865591));
#22871=CARTESIAN_POINT('Ctrl Pts',(-38.5227946134492,-35.0777904690468,
6.11605719057395));
#22872=CARTESIAN_POINT('Ctrl Pts',(-38.522424122767,-35.0013091826171,6.11258330249198));
#22873=CARTESIAN_POINT('Origin',(35.,35.,10.2084234471775));
#22874=CARTESIAN_POINT('Ctrl Pts',(30.9215901961247,35.0020443570103,7.70842344717745));
#22875=CARTESIAN_POINT('Ctrl Pts',(30.9207461022984,35.1331126499304,7.70328437820511));
#22876=CARTESIAN_POINT('Ctrl Pts',(30.985475579174,36.5980980633283,7.64581193344868));
#22877=CARTESIAN_POINT('Ctrl Pts',(32.753181262015,39.238437809064,7.53600611290817));
#22878=CARTESIAN_POINT('Ctrl Pts',(37.2955097522044,39.2117697306779,7.37900598555592));
#22879=CARTESIAN_POINT('Ctrl Pts',(39.7793716811886,35.4089491092894,7.22200585820366));
#22880=CARTESIAN_POINT('Ctrl Pts',(37.9775554192851,31.2391311721338,7.06500573085141));
#22881=CARTESIAN_POINT('Ctrl Pts',(33.5057216363881,30.441863683446,6.90800560349916));
#22882=CARTESIAN_POINT('Ctrl Pts',(31.1346462527125,32.9326274967327,6.7891448422745));
#22883=CARTESIAN_POINT('Ctrl Pts',(30.9248234084473,34.6330160680086,6.72261745683393));
#22884=CARTESIAN_POINT('Ctrl Pts',(30.9278854598697,34.9965452008231,6.70842344717745));
#22885=CARTESIAN_POINT('Ctrl Pts',(30.9308749498806,34.995920959377,7.79157655282255));
#22886=CARTESIAN_POINT('Ctrl Pts',(30.9370382260235,35.8984227922016,7.75638428364686));
#22887=CARTESIAN_POINT('Ctrl Pts',(31.6729751170447,38.1550462153353,7.66885863868709));
#22888=CARTESIAN_POINT('Ctrl Pts',(35.3795268052061,39.7808547962683,7.52899961794324));
#22889=CARTESIAN_POINT('Ctrl Pts',(39.1969168896572,37.3225573472918,7.37199949059099));
#22890=CARTESIAN_POINT('Ctrl Pts',(39.2524338890068,32.7797860374403,7.21499936323873));
#22891=CARTESIAN_POINT('Ctrl Pts',(35.4939868648458,30.2288021766129,7.05799923588648));
#22892=CARTESIAN_POINT('Ctrl Pts',(31.7173195455156,31.7813045011721,6.91685829908108));
#22893=CARTESIAN_POINT('Ctrl Pts',(30.9363083182476,34.0684206807159,6.82805073805977));
#22894=CARTESIAN_POINT('Ctrl Pts',(30.9290341434093,35.0032555560525,6.79157655282255));
#22895=CARTESIAN_POINT('Ctrl Pts',(37.6735319337713,37.2858331630076,8.));
#22896=CARTESIAN_POINT('Ctrl Pts',(38.4251602751564,36.4067215963626,7.94766662421592));
#22897=CARTESIAN_POINT('Ctrl Pts',(38.981419710079,33.8637820915388,7.84299987264775));
#22898=CARTESIAN_POINT('Ctrl Pts',(36.2450923914777,31.0470745569746,7.68599974529549));
#22899=CARTESIAN_POINT('Ctrl Pts',(32.3914750767338,31.7834880469926,7.52899961794325));
#22900=CARTESIAN_POINT('Ctrl Pts',(30.877370367455,35.4000509161799,7.37199949059098));
#22901=CARTESIAN_POINT('Ctrl Pts',(33.0598539558457,38.6599251241887,7.21499936323874));
#22902=CARTESIAN_POINT('Ctrl Pts',(36.9821911263972,38.6368970240971,7.05799923588648));
#22903=CARTESIAN_POINT('Ctrl Pts',(39.1270258717517,35.3531308437279,6.90099910853422));
#22904=CARTESIAN_POINT('Ctrl Pts',(37.5711430434112,31.75245953062,6.74399898118198));
#22905=CARTESIAN_POINT('Ctrl Pts',(33.7096786193679,31.0640126442915,6.58699885382972));
#22906=CARTESIAN_POINT('Ctrl Pts',(31.0052641890983,33.9049419734146,6.42999872647747));
#22907=CARTESIAN_POINT('Ctrl Pts',(31.882964491631,37.7278508156672,6.27299859912521));
#22908=CARTESIAN_POINT('Ctrl Pts',(35.5557420224402,39.1046545373095,6.11599847177296));
#22909=CARTESIAN_POINT('Ctrl Pts',(38.7301795638466,36.8007826630852,5.9589983444207));
#22910=CARTESIAN_POINT('Ctrl Pts',(38.559729694875,32.8821279738221,5.80199821706846));
#22911=CARTESIAN_POINT('Ctrl Pts',(35.1972358643355,30.8625912971014,5.64499808971619));
#22912=CARTESIAN_POINT('Ctrl Pts',(31.6578788381682,32.5531077792767,5.48799796236396));
#22913=CARTESIAN_POINT('Ctrl Pts',(31.1154338729727,36.437776445535,5.33099783501168));
#22914=CARTESIAN_POINT('Ctrl Pts',(34.0563166443959,39.033176953701,5.17399770765944));
#22915=CARTESIAN_POINT('Ctrl Pts',(37.843409322329,38.0119891070858,5.01699758030718));
#22916=CARTESIAN_POINT('Ctrl Pts',(39.0807895883257,34.2899216767724,4.85999745295493));
#22917=CARTESIAN_POINT('Ctrl Pts',(36.6588866782563,31.2045883187048,4.70299732560268));
#22918=CARTESIAN_POINT('Ctrl Pts',(32.7494441705885,31.5226370130723,4.54599719825042));
#22919=CARTESIAN_POINT('Ctrl Pts',(30.8580966653042,34.9588704649406,4.38899707089817));
#22920=CARTESIAN_POINT('Ctrl Pts',(32.6808336162004,38.4319851620801,4.23199694354592));
#22921=CARTESIAN_POINT('Ctrl Pts',(36.5831893123819,38.8276058411217,4.07499681619366));
#22922=CARTESIAN_POINT('Ctrl Pts',(39.0658839637408,35.7909756411325,3.91799668884141));
#22923=CARTESIAN_POINT('Ctrl Pts',(37.9026614585792,32.0450699960324,3.76099656148916));
#22924=CARTESIAN_POINT('Ctrl Pts',(34.1365945763887,30.9488784332844,3.6039964341369));
#22925=CARTESIAN_POINT('Ctrl Pts',(31.1447516212191,33.4853664448484,3.44699630678465));
#22926=CARTESIAN_POINT('Ctrl Pts',(31.6099468717921,37.3800408947213,3.2899961794324));
#22927=CARTESIAN_POINT('Ctrl Pts',(35.1150352873275,39.1405098438263,3.13299605208014));
#22928=CARTESIAN_POINT('Ctrl Pts',(38.5169704526781,37.1881438885041,2.97599592472789));
#22929=CARTESIAN_POINT('Ctrl Pts',(38.7652044817734,33.2736483267483,2.81899579737564));
#22930=CARTESIAN_POINT('Ctrl Pts',(35.6371435122955,30.9071888511377,2.66199567002338));
#22931=CARTESIAN_POINT('Ctrl Pts',(31.9377498791963,32.2107924399309,2.50499554267113));
#22932=CARTESIAN_POINT('Ctrl Pts',(30.9843052341107,36.0155051205153,2.34799541531888));
#22933=CARTESIAN_POINT('Ctrl Pts',(33.6317727579422,38.9096047900383,2.19099528796662));
#22934=CARTESIAN_POINT('Ctrl Pts',(37.5061424786706,38.297923989058,2.03399516061437));
#22935=CARTESIAN_POINT('Ctrl Pts',(39.1332307948504,34.7289638099038,1.87699503326212));
#22936=CARTESIAN_POINT('Ctrl Pts',(37.0540101980664,31.4030429687795,1.71999490590986));
#22937=CARTESIAN_POINT('Ctrl Pts',(33.1329413830615,31.3025508540242,1.56299477855761));
#22938=CARTESIAN_POINT('Ctrl Pts',(30.8860770418796,34.5175911198794,1.40599465120536));
#22939=CARTESIAN_POINT('Ctrl Pts',(32.3282167572518,38.1652236231046,1.2489945238531));
#22940=CARTESIAN_POINT('Ctrl Pts',(36.1661502448953,38.9745464314742,1.09199439650085));
#22941=CARTESIAN_POINT('Ctrl Pts',(38.9584257050592,36.219902286033,0.934994269148596));
#22942=CARTESIAN_POINT('Ctrl Pts',(38.2010620907038,32.3712654317411,0.777994141796343));
#22943=CARTESIAN_POINT('Ctrl Pts',(34.5734381379524,30.8800307521414,0.620994014444089));
#22944=CARTESIAN_POINT('Ctrl Pts',(31.3279883656859,33.0828278259953,0.463993887091835));
#22945=CARTESIAN_POINT('Ctrl Pts',(31.3759274478189,37.0055458008236,0.306993759739581));
#22946=CARTESIAN_POINT('Ctrl Pts',(34.6722754073454,39.1283105516069,0.149993632387328));
#22947=CARTESIAN_POINT('Ctrl Pts',(38.2651841076192,37.5523415454803,-0.007006494964925));
#22948=CARTESIAN_POINT('Ctrl Pts',(38.9246967202481,33.681118012335,-0.164006622317179));
#22949=CARTESIAN_POINT('Ctrl Pts',(37.0258557525633,31.9005650466596,-0.268673373885348));
#22950=CARTESIAN_POINT('Ctrl Pts',(35.9084720925035,31.6018409826581,-0.321006749669432));
#22951=CARTESIAN_POINT('Ctrl Pts',(37.8143974874483,37.4062712808594,8.10700224988981));
#22952=CARTESIAN_POINT('Ctrl Pts',(38.6056283266121,36.4808402609044,8.05466887410573));
#22953=CARTESIAN_POINT('Ctrl Pts',(39.1911964794515,33.80391597857,7.95000212253756));
#22954=CARTESIAN_POINT('Ctrl Pts',(36.3106949851439,30.8387991202229,7.7930019951853));
#22955=CARTESIAN_POINT('Ctrl Pts',(32.2540346732905,31.6140134536857,7.63600186783305));
#22956=CARTESIAN_POINT('Ctrl Pts',(30.6601533974768,35.4211291734076,7.4790017404808));
#22957=CARTESIAN_POINT('Ctrl Pts',(32.9576297245688,38.8527626858139,7.32200161312855));
#22958=CARTESIAN_POINT('Ctrl Pts',(37.0866306683329,38.828521259624,7.16500148577629));
#22959=CARTESIAN_POINT('Ctrl Pts',(39.3444744748973,35.3717369322484,7.00800135842404));
#22960=CARTESIAN_POINT('Ctrl Pts',(37.7066138353691,31.5813500777913,6.85100123107178));
#22961=CARTESIAN_POINT('Ctrl Pts',(33.6416929583746,30.856629657343,6.69400110371953));
#22962=CARTESIAN_POINT('Ctrl Pts',(30.7947858085381,33.8472445308389,6.53700097636727));
#22963=CARTESIAN_POINT('Ctrl Pts',(31.7187312063761,37.8715783734507,6.38000084901503));
#22964=CARTESIAN_POINT('Ctrl Pts',(35.5850234784437,39.3209244186404,6.22300072166276));
#22965=CARTESIAN_POINT('Ctrl Pts',(38.9267187571656,36.8956639860585,6.06600059431053));
#22966=CARTESIAN_POINT('Ctrl Pts',(38.7472880659103,32.7705395496047,5.90900046695826));
#22967=CARTESIAN_POINT('Ctrl Pts',(35.2076280122218,30.6445956336272,5.75200033960601));
#22968=CARTESIAN_POINT('Ctrl Pts',(31.4817860292625,32.4241836309969,5.59500021225375));
#22969=CARTESIAN_POINT('Ctrl Pts',(30.9107602158652,36.5135313570458,5.4380000849015));
#22970=CARTESIAN_POINT('Ctrl Pts',(34.0065949722125,39.2456807571843,5.28099995754925));
#22971=CARTESIAN_POINT('Ctrl Pts',(37.9932255349056,38.1706876091981,5.12399983019699));
#22972=CARTESIAN_POINT('Ctrl Pts',(39.2958020508805,34.2525084052524,4.96699970284474));
#22973=CARTESIAN_POINT('Ctrl Pts',(36.7462916527279,31.0046121145067,4.80999957549249));
#22974=CARTESIAN_POINT('Ctrl Pts',(32.6308647779182,31.3394184562628,4.65299944814024));
#22975=CARTESIAN_POINT('Ctrl Pts',(30.6398641844617,34.956703393489,4.49599932078798));
#22976=CARTESIAN_POINT('Ctrl Pts',(32.5586392064025,38.612812809568,4.33899919343573));
#22977=CARTESIAN_POINT('Ctrl Pts',(36.6666058731669,39.0292783213552,4.18199906608348));
#22978=CARTESIAN_POINT('Ctrl Pts',(39.2801110647917,35.8326513062801,4.02499893873122));
#22979=CARTESIAN_POINT('Ctrl Pts',(38.0555996031866,31.889377877368,3.86799881137897));
#22980=CARTESIAN_POINT('Ctrl Pts',(34.0911026630479,30.7354291472295,3.71099868402672));
#22981=CARTESIAN_POINT('Ctrl Pts',(30.9416226850806,33.4055620139871,3.55399855667446));
#22982=CARTESIAN_POINT('Ctrl Pts',(31.4313285785645,37.5054427177457,3.39699842932221));
#22983=CARTESIAN_POINT('Ctrl Pts',(35.1210963742505,39.3586689031172,3.23999830196995));
#22984=CARTESIAN_POINT('Ctrl Pts',(38.7022758847263,37.3034348623974,3.0829981746177));
#22985=CARTESIAN_POINT('Ctrl Pts',(38.9635891007609,33.1826886934549,2.92599804726545));
#22986=CARTESIAN_POINT('Ctrl Pts',(35.6707139262103,30.691542985346,2.76899791991319));
#22987=CARTESIAN_POINT('Ctrl Pts',(31.7764031777353,32.0638320605518,2.61199779256094));
#22988=CARTESIAN_POINT('Ctrl Pts',(30.7727225485069,36.0690110050931,2.45499766520869));
#22989=CARTESIAN_POINT('Ctrl Pts',(33.5596823199811,39.1155977076656,2.29799753785643));
#22990=CARTESIAN_POINT('Ctrl Pts',(37.6381884600154,38.4716880959441,2.14099741050418));
#22991=CARTESIAN_POINT('Ctrl Pts',(39.3510063287937,34.7146832013567,1.98399728315193));
#22992=CARTESIAN_POINT('Ctrl Pts',(37.1622338104923,31.2135231289919,1.82699715579967));
#22993=CARTESIAN_POINT('Ctrl Pts',(33.0345680505794,31.1077361916065,1.66999702844742));
#22994=CARTESIAN_POINT('Ctrl Pts',(30.6693188173153,34.4921735091382,1.51299690109517));
#22995=CARTESIAN_POINT('Ctrl Pts',(32.1874433402447,38.3319958888659,1.35599677374292));
#22996=CARTESIAN_POINT('Ctrl Pts',(36.227593460831,39.1839610551084,1.19899664639066));
#22997=CARTESIAN_POINT('Ctrl Pts',(39.1669909447667,36.2841776398386,1.04199651903841));
#22998=CARTESIAN_POINT('Ctrl Pts',(38.3697226472005,32.2327602036007,0.884996391686153));
#22999=CARTESIAN_POINT('Ctrl Pts',(34.5509630471873,30.6629539550025,0.727996264333901));
#23000=CARTESIAN_POINT('Ctrl Pts',(31.1345139786991,32.9818140634986,0.570996136981646));
#23001=CARTESIAN_POINT('Ctrl Pts',(31.1849789200754,37.1112158757118,0.413996009629392));
#23002=CARTESIAN_POINT('Ctrl Pts',(34.6550079471686,39.3458268431676,0.256995882277139));
#23003=CARTESIAN_POINT('Ctrl Pts',(38.4372231849787,37.6868217065119,0.0999957549248859));
#23004=CARTESIAN_POINT('Ctrl Pts',(39.1314848156243,33.611627523338,-0.0570043724273679));
#23005=CARTESIAN_POINT('Ctrl Pts',(37.1325959372044,31.7372591159268,-0.161671123995537));
#23006=CARTESIAN_POINT('Ctrl Pts',(35.9563385206894,31.4227955987545,-0.214004499779622));
#23007=CARTESIAN_POINT('Ctrl Pts',(37.9552630411254,37.5267093987114,8.21400449977962));
#23008=CARTESIAN_POINT('Ctrl Pts',(38.7860963780679,36.5549589254462,8.16167112399554));
#23009=CARTESIAN_POINT('Ctrl Pts',(39.4009732488241,33.744049865601,8.05700437242737));
#23010=CARTESIAN_POINT('Ctrl Pts',(36.37629757881,30.6305236834712,7.90000424507512));
#23011=CARTESIAN_POINT('Ctrl Pts',(32.1165942698471,31.4445388603786,7.74300411772287));
#23012=CARTESIAN_POINT('Ctrl Pts',(30.4429364274986,35.4422074306354,7.58600399037061));
#23013=CARTESIAN_POINT('Ctrl Pts',(32.8554054932919,39.0456002474389,7.42900386301836));
#23014=CARTESIAN_POINT('Ctrl Pts',(37.1910702102687,39.020145495151,7.2720037356661));
#23015=CARTESIAN_POINT('Ctrl Pts',(39.561923078043,35.3903430207689,7.11500360831385));
#23016=CARTESIAN_POINT('Ctrl Pts',(37.8420846273271,31.4102406249626,6.95800348096159));
#23017=CARTESIAN_POINT('Ctrl Pts',(33.5737072973814,30.6492466703945,6.80100335360934));
#23018=CARTESIAN_POINT('Ctrl Pts',(30.5843074279779,33.789547088263,6.64400322625708));
#23019=CARTESIAN_POINT('Ctrl Pts',(31.5544979211211,38.0153059312343,6.48700309890484));
#23020=CARTESIAN_POINT('Ctrl Pts',(35.6143049344472,39.5371942999712,6.33000297155258));
#23021=CARTESIAN_POINT('Ctrl Pts',(39.1232579504846,36.9905453090318,6.17300284420033));
#23022=CARTESIAN_POINT('Ctrl Pts',(38.9348464369457,32.6589511253872,6.01600271684807));
#23023=CARTESIAN_POINT('Ctrl Pts',(35.2180201601081,30.4265999701529,5.85900258949582));
#23024=CARTESIAN_POINT('Ctrl Pts',(31.3056932203567,32.2952594827172,5.70200246214357));
#23025=CARTESIAN_POINT('Ctrl Pts',(30.7060865587576,36.5892862685565,5.54500233479131));
#23026=CARTESIAN_POINT('Ctrl Pts',(33.956873300029,39.4581845606676,5.38800220743906));
#23027=CARTESIAN_POINT('Ctrl Pts',(38.1430417474823,38.3293861113103,5.2310020800868));
#23028=CARTESIAN_POINT('Ctrl Pts',(39.5108145134353,34.2150951337324,5.07400195273456));
#23029=CARTESIAN_POINT('Ctrl Pts',(36.8336966271993,30.8046359103087,4.9170018253823));
#23030=CARTESIAN_POINT('Ctrl Pts',(32.512285385248,31.1561998994534,4.76000169803005));
#23031=CARTESIAN_POINT('Ctrl Pts',(30.4216317036192,34.9545363220374,4.60300157067779));
#23032=CARTESIAN_POINT('Ctrl Pts',(32.4364447966046,38.7936404570559,4.44600144332554));
#23033=CARTESIAN_POINT('Ctrl Pts',(36.750022433952,39.2309508015887,4.28900131597329));
#23034=CARTESIAN_POINT('Ctrl Pts',(39.4943381658426,35.8743269714277,4.13200118862103));
#23035=CARTESIAN_POINT('Ctrl Pts',(38.2085377477941,31.7336857587036,3.97500106126878));
#23036=CARTESIAN_POINT('Ctrl Pts',(34.0456107497072,30.5219798611747,3.81800093391652));
#23037=CARTESIAN_POINT('Ctrl Pts',(30.738493748942,33.3257575831257,3.66100080656427));
#23038=CARTESIAN_POINT('Ctrl Pts',(31.252710285337,37.6308445407701,3.50400067921202));
#23039=CARTESIAN_POINT('Ctrl Pts',(35.1271574611734,39.5768279624082,3.34700055185977));
#23040=CARTESIAN_POINT('Ctrl Pts',(38.8875813167745,37.4187258362905,3.19000042450751));
#23041=CARTESIAN_POINT('Ctrl Pts',(39.1619737197485,33.0917290601617,3.03300029715526));
#23042=CARTESIAN_POINT('Ctrl Pts',(35.7042843401251,30.4758971195542,2.876000169803));
#23043=CARTESIAN_POINT('Ctrl Pts',(31.6150564762743,31.9168716811727,2.71900004245075));
#23044=CARTESIAN_POINT('Ctrl Pts',(30.5611398629031,36.1225168896708,2.5619999150985));
#23045=CARTESIAN_POINT('Ctrl Pts',(33.48759188202,39.3215906252928,2.40499978774624));
#23046=CARTESIAN_POINT('Ctrl Pts',(37.7702344413602,38.6454522028303,2.24799966039399));
#23047=CARTESIAN_POINT('Ctrl Pts',(39.568781862737,34.7004025928096,2.09099953304174));
#23048=CARTESIAN_POINT('Ctrl Pts',(37.2704574229183,31.0240032892043,1.93399940568949));
#23049=CARTESIAN_POINT('Ctrl Pts',(32.9361947180972,30.9129215291889,1.77699927833723));
#23050=CARTESIAN_POINT('Ctrl Pts',(30.4525605927511,34.4667558983969,1.61999915098498));
#23051=CARTESIAN_POINT('Ctrl Pts',(32.0466699232375,38.4987681546272,1.46299902363272));
#23052=CARTESIAN_POINT('Ctrl Pts',(36.2890366767668,39.3933756787425,1.30599889628047));
#23053=CARTESIAN_POINT('Ctrl Pts',(39.3755561844741,36.3484529936443,1.14899876892822));
#23054=CARTESIAN_POINT('Ctrl Pts',(38.5383832036972,32.0942549754603,0.991998641575964));
#23055=CARTESIAN_POINT('Ctrl Pts',(34.5284879564222,30.4458771578634,0.834998514223711));
#23056=CARTESIAN_POINT('Ctrl Pts',(30.9410395917123,32.8808003010019,0.677998386871457));
#23057=CARTESIAN_POINT('Ctrl Pts',(30.9940303923319,37.2168859506,0.520998259519203));
#23058=CARTESIAN_POINT('Ctrl Pts',(34.6377404869918,39.5633431347282,0.36399813216695));
#23059=CARTESIAN_POINT('Ctrl Pts',(38.6092622623382,37.8213018675437,0.206998004814697));
#23060=CARTESIAN_POINT('Ctrl Pts',(39.3382729110006,33.5421370343408,0.0499978774624429));
#23061=CARTESIAN_POINT('Ctrl Pts',(37.2393361218455,31.5739531851941,-0.0546688741057264));
#23062=CARTESIAN_POINT('Ctrl Pts',(36.0042049488753,31.243750214851,-0.107002249889811));
#23063=CARTESIAN_POINT('Ctrl Pts',(38.0961285948024,37.6471475165633,8.32100674966943));
#23064=CARTESIAN_POINT('Ctrl Pts',(38.9665644295237,36.6290775899881,8.26867337388535));
#23065=CARTESIAN_POINT('Ctrl Pts',(39.6107500181967,33.6841837526321,8.16400662231718));
#23066=CARTESIAN_POINT('Ctrl Pts',(36.441900172476,30.4222482467195,8.00700649496493));
#23067=CARTESIAN_POINT('Ctrl Pts',(31.9791538664038,31.2750642670716,7.85000636761267));
#23068=CARTESIAN_POINT('Ctrl Pts',(30.2257194575204,35.4632856878632,7.69300624026042));
#23069=CARTESIAN_POINT('Ctrl Pts',(32.753181262015,39.238437809064,7.53600611290817));
#23070=CARTESIAN_POINT('Ctrl Pts',(37.2955097522044,39.2117697306779,7.37900598555592));
#23071=CARTESIAN_POINT('Ctrl Pts',(39.7793716811886,35.4089491092894,7.22200585820366));
#23072=CARTESIAN_POINT('Ctrl Pts',(37.9775554192851,31.2391311721338,7.06500573085141));
#23073=CARTESIAN_POINT('Ctrl Pts',(33.5057216363881,30.441863683446,6.90800560349916));
#23074=CARTESIAN_POINT('Ctrl Pts',(30.3738290474178,33.7318496456872,6.75100547614689));
#23075=CARTESIAN_POINT('Ctrl Pts',(31.3902646358661,38.1590334890178,6.59400534879465));
#23076=CARTESIAN_POINT('Ctrl Pts',(35.6435863904507,39.7534641813021,6.43700522144238));
#23077=CARTESIAN_POINT('Ctrl Pts',(39.3197971438036,37.085426632005,6.28000509409014));
#23078=CARTESIAN_POINT('Ctrl Pts',(39.122404807981,32.5473627011697,6.12300496673788));
#23079=CARTESIAN_POINT('Ctrl Pts',(35.2284123079944,30.2086043066787,5.96600483938564));
#23080=CARTESIAN_POINT('Ctrl Pts',(31.1296004114509,32.1663353344374,5.80900471203338));
#23081=CARTESIAN_POINT('Ctrl Pts',(30.5014129016501,36.6650411800673,5.65200458468112));
#23082=CARTESIAN_POINT('Ctrl Pts',(33.9071516278456,39.6706883641509,5.49500445732887));
#23083=CARTESIAN_POINT('Ctrl Pts',(38.2928579600589,38.4880846134226,5.33800432997661));
#23084=CARTESIAN_POINT('Ctrl Pts',(39.72582697599,34.1776818622125,5.18100420262437));
#23085=CARTESIAN_POINT('Ctrl Pts',(36.9211016016709,30.6046597061106,5.0240040752721));
#23086=CARTESIAN_POINT('Ctrl Pts',(32.3937059925777,30.9729813426439,4.86700394791986));
#23087=CARTESIAN_POINT('Ctrl Pts',(30.2033992227766,34.9523692505858,4.7100038205676));
#23088=CARTESIAN_POINT('Ctrl Pts',(32.3142503868067,38.9744681045439,4.55300369321535));
#23089=CARTESIAN_POINT('Ctrl Pts',(36.833438994737,39.4326232818222,4.39600356586309));
#23090=CARTESIAN_POINT('Ctrl Pts',(39.7085652668935,35.9160026365752,4.23900343851085));
#23091=CARTESIAN_POINT('Ctrl Pts',(38.3614758924016,31.5779936400392,4.08200331115859));
#23092=CARTESIAN_POINT('Ctrl Pts',(34.0001188363665,30.3085305751198,3.92500318380634));
#23093=CARTESIAN_POINT('Ctrl Pts',(30.5353648128034,33.2459531522644,3.76800305645408));
#23094=CARTESIAN_POINT('Ctrl Pts',(31.0740919921095,37.7562463637945,3.61100292910183));
#23095=CARTESIAN_POINT('Ctrl Pts',(35.1332185480963,39.7949870216991,3.45400280174957));
#23096=CARTESIAN_POINT('Ctrl Pts',(39.0728867488228,37.5340168101838,3.29700267439732));
#23097=CARTESIAN_POINT('Ctrl Pts',(39.360358338736,33.0007694268683,3.14000254704507));
#23098=CARTESIAN_POINT('Ctrl Pts',(35.7378547540399,30.2602512537625,2.98300241969282));
#23099=CARTESIAN_POINT('Ctrl Pts',(31.4537097748133,31.7699113017935,2.82600229234056));
#23100=CARTESIAN_POINT('Ctrl Pts',(30.3495571772993,36.1760227742485,2.66900216498831));
#23101=CARTESIAN_POINT('Ctrl Pts',(33.415501444059,39.52758354292,2.51200203763605));
#23102=CARTESIAN_POINT('Ctrl Pts',(37.902280422705,38.8192163097165,2.3550019102838));
#23103=CARTESIAN_POINT('Ctrl Pts',(39.7865573966804,34.6861219842625,2.19800178293155));
#23104=CARTESIAN_POINT('Ctrl Pts',(37.3786810353442,30.8344834494167,2.0410016555793));
#23105=CARTESIAN_POINT('Ctrl Pts',(32.8378213856151,30.7181068667712,1.88400152822704));
#23106=CARTESIAN_POINT('Ctrl Pts',(30.2358023681867,34.4413382876556,1.72700140087479));
#23107=CARTESIAN_POINT('Ctrl Pts',(31.9058965062304,38.6655404203885,1.57000127352254));
#23108=CARTESIAN_POINT('Ctrl Pts',(36.3504798927025,39.6027903023767,1.41300114617028));
#23109=CARTESIAN_POINT('Ctrl Pts',(39.5841214241815,36.41272834745,1.25600101881803));
#23110=CARTESIAN_POINT('Ctrl Pts',(38.7070437601939,31.9557497473198,1.09900089146578));
#23111=CARTESIAN_POINT('Ctrl Pts',(34.5060128656572,30.2288003607244,0.942000764113522));
#23112=CARTESIAN_POINT('Ctrl Pts',(30.7475652047255,32.7797865385051,0.785000636761267));
#23113=CARTESIAN_POINT('Ctrl Pts',(30.8030818645885,37.3225560254883,0.628000509409015));
#23114=CARTESIAN_POINT('Ctrl Pts',(34.620473026815,39.7808594262888,0.47100038205676));
#23115=CARTESIAN_POINT('Ctrl Pts',(38.7813013396977,37.9557820285754,0.314000254704507));
#23116=CARTESIAN_POINT('Ctrl Pts',(39.5450610063768,33.4726465453437,0.157000127352254));
#23117=CARTESIAN_POINT('Ctrl Pts',(37.3460763064866,31.4106472544613,0.0523333757840845));
#23118=CARTESIAN_POINT('Ctrl Pts',(36.0520713770613,31.0647048309474,0.));
#23119=CARTESIAN_POINT('Ctrl Pts',(36.0520713770613,31.0647048309474,0.));
#23120=CARTESIAN_POINT('Ctrl Pts',(36.1681792227746,31.1043194052127,-1.93406836379874E-16));
#23121=CARTESIAN_POINT('Ctrl Pts',(36.2820220087194,31.1494844117486,-1.00024874895392E-15));
#23122=CARTESIAN_POINT('Ctrl Pts',(36.3933738437048,31.1998422365254,-1.16573417585641E-15));
#23123=CARTESIAN_POINT('Ctrl Pts',(36.5072229375308,31.2513294232309,-1.33493090168249E-15));
#23124=CARTESIAN_POINT('Ctrl Pts',(36.6184687230184,31.3082454542348,-1.64395861563978E-15));
#23125=CARTESIAN_POINT('Ctrl Pts',(36.7268454950609,31.3702566870239,-9.99200722162641E-16));
#23126=CARTESIAN_POINT('Ctrl Pts',(36.8407839045068,31.435450188349,-3.21355391692774E-16));
#23127=CARTESIAN_POINT('Ctrl Pts',(36.9515522547681,31.5062756815887,8.02288849704332E-16));
#23128=CARTESIAN_POINT('Ctrl Pts',(37.058802639455,31.5823916741173,9.99200722162641E-16));
#23129=CARTESIAN_POINT('Ctrl Pts',(37.1526467260561,31.6489931675798,1.17149861056366E-15));
#23130=CARTESIAN_POINT('Ctrl Pts',(37.2437970657742,31.7196462572752,8.48680262035355E-16));
#23131=CARTESIAN_POINT('Ctrl Pts',(37.3319890907744,31.7941443117117,9.99200722162641E-16));
#23132=CARTESIAN_POINT('Ctrl Pts',(37.3493641971328,31.8088215075162,1.02885543304851E-15));
#23133=CARTESIAN_POINT('Ctrl Pts',(37.3666243754182,31.8236479962496,-1.0299785826125E-15));
#23134=CARTESIAN_POINT('Ctrl Pts',(37.3837674478979,31.8386222687341,-1.0547118733939E-15));
#23135=CARTESIAN_POINT('Ctrl Pts',(37.3963017832026,31.8495708634207,-1.07279587555905E-15));
#23136=CARTESIAN_POINT('Ctrl Pts',(37.4087723034701,31.8605974704649,-2.60456824673694E-15));
#23137=CARTESIAN_POINT('Ctrl Pts',(37.4211693573137,31.8716933759855,-2.4980018054066E-15));
#23138=CARTESIAN_POINT('Ctrl Pts',(37.5137485970205,31.954555845562,-1.70218045614906E-15));
#23139=CARTESIAN_POINT('Ctrl Pts',(37.6023719888639,32.0414000295362,-2.33877871405102E-15));
#23140=CARTESIAN_POINT('Ctrl Pts',(37.6867781087441,32.1319050017937,-1.99840144432528E-15));
#23141=CARTESIAN_POINT('Ctrl Pts',(37.7709925191637,32.2222044124232,-1.65879726478403E-15));
#23142=CARTESIAN_POINT('Ctrl Pts',(37.8510093104121,32.3161487056446,-9.47721428060247E-16));
#23143=CARTESIAN_POINT('Ctrl Pts',(37.9265284067741,32.4134511741487,-1.30451205393456E-15));
#23144=CARTESIAN_POINT('Ctrl Pts',(38.0010152019123,32.5094235756611,-1.65642556372184E-15));
#23145=CARTESIAN_POINT('Ctrl Pts',(38.0711268225993,32.6086636566059,-6.10757404334397E-16));
#23146=CARTESIAN_POINT('Ctrl Pts',(38.1365292929227,32.710917134839,-5.27355936696949E-16));
#23147=CARTESIAN_POINT('Ctrl Pts',(38.1898350382321,32.7942579909372,-4.59380256721482E-16));
#23148=CARTESIAN_POINT('Ctrl Pts',(38.2400117946351,32.8796011515617,-1.29327937900734E-15));
#23149=CARTESIAN_POINT('Ctrl Pts',(38.28685279593,32.9668147810226,-1.63757896132211E-15));
#23150=CARTESIAN_POINT('Ctrl Pts',(38.298752249944,32.9889704682297,-1.72504457763057E-15));
#23151=CARTESIAN_POINT('Ctrl Pts',(38.3104363019817,33.0112468837781,3.54805112116964E-15));
#23152=CARTESIAN_POINT('Ctrl Pts',(38.3219012991264,33.0336418915139,3.66373598126302E-15));
#23153=CARTESIAN_POINT('Ctrl Pts',(38.3300587509266,33.0495761472196,3.74604683213415E-15));
#23154=CARTESIAN_POINT('Ctrl Pts',(38.3381015974855,33.0655632618739,-7.08373702740619E-16));
#23155=CARTESIAN_POINT('Ctrl Pts',(38.3460261690062,33.0815968043693,-6.93889390390723E-16));
#23156=CARTESIAN_POINT('Ctrl Pts',(38.3989870883303,33.1887510080204,-5.97088888833881E-16));
#23157=CARTESIAN_POINT('Ctrl Pts',(38.4467091567301,33.2980550637735,1.26900815615077E-15));
#23158=CARTESIAN_POINT('Ctrl Pts',(38.4889135757351,33.409246351529,1.0547118733939E-15));
#23159=CARTESIAN_POINT('Ctrl Pts',(38.5302818373033,33.5182347083035,8.44661246299018E-16));
#23160=CARTESIAN_POINT('Ctrl Pts',(38.5663491876186,33.6290368908256,3.13106813660632E-16));
#23161=CARTESIAN_POINT('Ctrl Pts',(38.5968048600256,33.7414193655312,4.9960036108132E-16));
#23162=CARTESIAN_POINT('Ctrl Pts',(38.6012591757497,33.7578559431745,5.26876105632901E-16));
#23163=CARTESIAN_POINT('Ctrl Pts',(38.6055933637529,33.7743263394091,3.42924457172855E-16));
#23164=CARTESIAN_POINT('Ctrl Pts',(38.6098063577125,33.7908298367184,3.33066907387547E-16));
#23165=CARTESIAN_POINT('Ctrl Pts',(38.6394749188516,33.9070500410733,3.19833619294622E-16));
#23166=CARTESIAN_POINT('Ctrl Pts',(38.6631375043611,34.0249121336904,2.13657224701249E-16));
#23167=CARTESIAN_POINT('Ctrl Pts',(38.6808849682855,34.1439802784308,6.10622663543836E-16));
#23168=CARTESIAN_POINT('Ctrl Pts',(38.6908685193634,34.2109601528418,8.33929201973265E-16));
#23169=CARTESIAN_POINT('Ctrl Pts',(38.6989793099884,34.2783216258907,1.0776972087123E-15));
#23170=CARTESIAN_POINT('Ctrl Pts',(38.705226464765,34.3459856591442,1.13797860024079E-15));
#23171=CARTESIAN_POINT('Ctrl Pts',(38.7081089504882,34.3772063695005,1.1657929023787E-15));
#23172=CARTESIAN_POINT('Ctrl Pts',(38.7105946047039,34.4084914721069,9.83922849187538E-16));
#23173=CARTESIAN_POINT('Ctrl Pts',(38.7126839762627,34.4398330679179,1.02695629777827E-15));
#23174=CARTESIAN_POINT('Ctrl Pts',(38.7138850693151,34.4578500514573,1.05169444256127E-15));
#23175=CARTESIAN_POINT('Ctrl Pts',(38.7149546915907,34.4758786502346,-4.64302084245928E-16));
#23176=CARTESIAN_POINT('Ctrl Pts',(38.715892912359,34.4939090237972,-4.44089209850063E-16));
#23177=CARTESIAN_POINT('Ctrl Pts',(38.7222038666684,34.6151905681615,-3.08127044991787E-16));
#23178=CARTESIAN_POINT('Ctrl Pts',(38.7225822971166,34.7366693867671,-2.99144274726584E-15));
#23179=CARTESIAN_POINT('Ctrl Pts',(38.7171864105867,34.8578982328034,-2.05391259555654E-15));
#23180=CARTESIAN_POINT('Ctrl Pts',(38.71190245704,34.9766122916381,-1.13583069320137E-15));
#23181=CARTESIAN_POINT('Ctrl Pts',(38.7010807679502,35.0950875649844,1.78168855748587E-15));
#23182=CARTESIAN_POINT('Ctrl Pts',(38.6848165352731,35.2128980770419,1.76247905159244E-15));
#23183=CARTESIAN_POINT('Ctrl Pts',(38.6687112067838,35.3295575613132,1.74345722568323E-15));
#23184=CARTESIAN_POINT('Ctrl Pts',(38.6472688142291,35.4455660470931,1.26625388930718E-16));
#23185=CARTESIAN_POINT('Ctrl Pts',(38.62053500354,35.5604910223212,1.80411241501588E-16));
#23186=CARTESIAN_POINT('Ctrl Pts',(38.6031281268642,35.6353207910372,2.15432201045671E-16));
#23187=CARTESIAN_POINT('Ctrl Pts',(38.5834769893052,35.7096907862118,1.51379352364637E-15));
#23188=CARTESIAN_POINT('Ctrl Pts',(38.5615843902035,35.7834747121961,1.2490009027033E-15));
#23189=CARTESIAN_POINT('Ctrl Pts',(38.5541960332861,35.8083754550181,1.15963817406959E-15));
#23190=CARTESIAN_POINT('Ctrl Pts',(38.5465523248095,35.8332093935643,2.32778305945499E-15));
#23191=CARTESIAN_POINT('Ctrl Pts',(38.5386531847276,35.8579714965102,2.3037127760972E-15));
#23192=CARTESIAN_POINT('Ctrl Pts',(38.5335667575399,35.8739163502969,2.28821339990993E-15));
#23193=CARTESIAN_POINT('Ctrl Pts',(38.528375210839,35.8898288067619,1.8799349255917E-16));
#23194=CARTESIAN_POINT('Ctrl Pts',(38.5230814037796,35.9056994997334,2.77555756156289E-16));
#23195=CARTESIAN_POINT('Ctrl Pts',(38.4861837480683,36.016317691632,9.0180169672523E-16));
#23196=CARTESIAN_POINT('Ctrl Pts',(38.4442853792632,36.1250244064477,1.67610385059537E-15));
#23197=CARTESIAN_POINT('Ctrl Pts',(38.3974510894444,36.2314004501635,1.54737334057131E-15));
#23198=CARTESIAN_POINT('Ctrl Pts',(38.3593370450265,36.3179699544917,1.44261162867242E-15));
#23199=CARTESIAN_POINT('Ctrl Pts',(38.3179530965748,36.4029957144323,1.09861093914672E-15));
#23200=CARTESIAN_POINT('Ctrl Pts',(38.27331318169,36.4862361414904,1.49186218934005E-15));
#23201=CARTESIAN_POINT('Ctrl Pts',(38.2516982037212,36.526541773829,1.68227736219745E-15));
#23202=CARTESIAN_POINT('Ctrl Pts',(38.2293195714479,36.5664285801089,1.70359564472489E-15));
#23203=CARTESIAN_POINT('Ctrl Pts',(38.2061773939932,36.6058676078699,1.76247905159244E-15));
#23204=CARTESIAN_POINT('Ctrl Pts',(38.1925910511184,36.629021529097,1.79704840691352E-15));
#23205=CARTESIAN_POINT('Ctrl Pts',(38.1787394785284,36.652024183054,3.81993764399042E-15));
#23206=CARTESIAN_POINT('Ctrl Pts',(38.1646367510805,36.6748472188681,3.75394160201381E-15));
#23207=CARTESIAN_POINT('Ctrl Pts',(38.1062052960737,36.7694092952617,3.48050195910614E-15));
#23208=CARTESIAN_POINT('Ctrl Pts',(38.0434225704545,36.8609661715359,-8.52927663010733E-16));
#23209=CARTESIAN_POINT('Ctrl Pts',(37.9763226192313,36.9491271397218,-6.21031004399697E-16));
#23210=CARTESIAN_POINT('Ctrl Pts',(37.9162919198372,37.0279999925776,-4.13565598690696E-16));
#23211=CARTESIAN_POINT('Ctrl Pts',(37.8528051248739,37.1041547391556,2.13873726282784E-15));
#23212=CARTESIAN_POINT('Ctrl Pts',(37.7858631238401,37.1772850733286,2.38004060904018E-15));
#23213=CARTESIAN_POINT('Ctrl Pts',(37.7510082002317,37.215362097793,2.52360662668101E-15));
#23214=CARTESIAN_POINT('Ctrl Pts',(37.71521617243,37.2526187144799,1.78459625189646E-16));
#23215=CARTESIAN_POINT('Ctrl Pts',(37.6785244495408,37.2890395253442,2.4980018054066E-16));
#23216=CARTESIAN_POINT('Ctrl Pts',(31.4836963557363,34.997016753135,6.38741669750802));
#23217=CARTESIAN_POINT('Ctrl Pts',(31.4810522497149,34.6831064242593,6.4016107071645));
#23218=CARTESIAN_POINT('Ctrl Pts',(31.5197088623892,34.3698361384337,6.41580471682098));
#23219=CARTESIAN_POINT('Ctrl Pts',(31.602283311232,34.0686052256029,6.42999872647746));
#23220=CARTESIAN_POINT('Ctrl Pts',(31.9067356658548,32.9579655303736,6.48233210226155));
#23221=CARTESIAN_POINT('Ctrl Pts',(32.8082071426114,32.0109890873326,6.53466547804563));
#23222=CARTESIAN_POINT('Ctrl Pts',(33.9025202849968,31.6522420135335,6.58699885382972));
#23223=CARTESIAN_POINT('Ctrl Pts',(34.9968334273823,31.2934949397344,6.6393322296138));
#23224=CARTESIAN_POINT('Ctrl Pts',(36.2839882353967,31.5229772351772,6.69166560539789));
#23225=CARTESIAN_POINT('Ctrl Pts',(37.1868794441274,32.2378302684166,6.74399898118197));
#23226=CARTESIAN_POINT('Ctrl Pts',(38.089770652858,32.952683301656,6.79633235696606));
#23227=CARTESIAN_POINT('Ctrl Pts',(38.6083982623049,34.1529070726919,6.84866573275014));
#23228=CARTESIAN_POINT('Ctrl Pts',(38.5102396094692,35.3003133216048,6.90099910853422));
#23229=CARTESIAN_POINT('Ctrl Pts',(38.4120809566336,36.4477195705176,6.95333248431831));
#23230=CARTESIAN_POINT('Ctrl Pts',(37.6971360415154,37.5423082973073,7.00566586010239));
#23231=CARTESIAN_POINT('Ctrl Pts',(36.6859407221977,38.0934406773841,7.05799923588648));
#23232=CARTESIAN_POINT('Ctrl Pts',(35.67474540288,38.6445730574609,7.11033261167056));
#23233=CARTESIAN_POINT('Ctrl Pts',(34.3672996793629,38.6522490908248,7.16266598745465));
#23234=CARTESIAN_POINT('Ctrl Pts',(33.3498295528725,38.1127747395053,7.21499936323873));
#23235=CARTESIAN_POINT('Ctrl Pts',(32.3323594263822,37.5733003881858,7.26733273902282));
#23236=CARTESIAN_POINT('Ctrl Pts',(31.6048648969186,36.4866756521828,7.3196661148069));
#23237=CARTESIAN_POINT('Ctrl Pts',(31.4934684170666,35.3406028059835,7.37199949059098));
#23238=CARTESIAN_POINT('Ctrl Pts',(31.4825294286169,35.2280599532493,7.37713855956333));
#23239=CARTESIAN_POINT('Ctrl Pts',(31.4775314630746,35.1149438434099,7.38227762853567));
#23240=CARTESIAN_POINT('Ctrl Pts',(31.47826034488,35.0017653187145,7.38741669750802));
#23241=CARTESIAN_POINT('Ctrl Pts',(33.9479286229388,31.0647048309474,8.));
#23242=CARTESIAN_POINT('Ctrl Pts',(32.6539236935135,31.4106472544613,7.94766662421592));
#23243=CARTESIAN_POINT('Ctrl Pts',(30.454936822078,33.4726324908028,7.84299987264775));
#23244=CARTESIAN_POINT('Ctrl Pts',(31.2187005389846,37.9557872897229,7.6859997452955));
#23245=CARTESIAN_POINT('Ctrl Pts',(35.3795268052061,39.7808547962683,7.52899961794324));
#23246=CARTESIAN_POINT('Ctrl Pts',(39.1969168896572,37.3225573472918,7.37199949059099));
#23247=CARTESIAN_POINT('Ctrl Pts',(39.2524338890068,32.7797860374403,7.21499936323873));
#23248=CARTESIAN_POINT('Ctrl Pts',(35.4939868648458,30.2288021766129,7.05799923588648));
#23249=CARTESIAN_POINT('Ctrl Pts',(31.2929572874421,31.9557502059188,6.90099910853422));
#23250=CARTESIAN_POINT('Ctrl Pts',(30.4158796925061,36.4127281597254,6.74399898118197));
#23251=CARTESIAN_POINT('Ctrl Pts',(33.6495204900336,39.6027890266495,6.58699885382972));
#23252=CARTESIAN_POINT('Ctrl Pts',(38.0941026784935,38.6655395297167,6.42999872647747));
#23253=CARTESIAN_POINT('Ctrl Pts',(39.7641964207046,34.4413384042963,6.27299859912521));
#23254=CARTESIAN_POINT('Ctrl Pts',(37.1621780526355,30.7181079801836,6.11599847177296));
#23255=CARTESIAN_POINT('Ctrl Pts',(32.6213195789955,30.8344845112897,5.95899834442071));
#23256=CARTESIAN_POINT('Ctrl Pts',(30.2134438300848,34.686122068773,5.80199821706845));
#23257=CARTESIAN_POINT('Ctrl Pts',(32.0977203234525,38.8192153272012,5.6449980897162));
#23258=CARTESIAN_POINT('Ctrl Pts',(36.5844981485848,39.5275823816942,5.48799796236394));
#23259=CARTESIAN_POINT('Ctrl Pts',(39.6504416291735,36.1760224717832,5.33099783501169));
#23260=CARTESIAN_POINT('Ctrl Pts',(38.5462893146292,31.7699121313011,5.17399770765944));
#23261=CARTESIAN_POINT('Ctrl Pts',(34.2621454354683,30.2602524703801,5.01699758030718));
#23262=CARTESIAN_POINT('Ctrl Pts',(30.6396427805907,33.0007699401812,4.85999745295493));
#23263=CARTESIAN_POINT('Ctrl Pts',(30.927114296777,37.5340161596205,4.70299732560268));
#23264=CARTESIAN_POINT('Ctrl Pts',(34.86678148609,39.7949857907703,4.54599719825042));
#23265=CARTESIAN_POINT('Ctrl Pts',(38.9259070000539,37.7562456562111,4.38899707089817));
#23266=CARTESIAN_POINT('Ctrl Pts',(39.4646340410498,33.2459536025622,4.23199694354592));
#23267=CARTESIAN_POINT('Ctrl Pts',(35.9998809069499,30.3085317794917,4.07499681619366));
#23268=CARTESIAN_POINT('Ctrl Pts',(31.6385249705421,31.5779945185253,3.91799668884141));
#23269=CARTESIAN_POINT('Ctrl Pts',(30.291435941871,35.9160024014201,3.76099656148915));
#23270=CARTESIAN_POINT('Ctrl Pts',(33.1665614759356,39.4326221439007,3.60399643413691));
#23271=CARTESIAN_POINT('Ctrl Pts',(37.6857489237188,38.9744670842276,3.44699630678464));
#23272=CARTESIAN_POINT('Ctrl Pts',(39.7965995458586,34.9523692628263,3.2899961794324));
#23273=CARTESIAN_POINT('Ctrl Pts',(37.6062933383462,30.9729823764193,3.13299605208014));
#23274=CARTESIAN_POINT('Ctrl Pts',(33.078898891504,30.6046608345122,2.97599592472789));
#23275=CARTESIAN_POINT('Ctrl Pts',(30.2741742372111,34.1776820732232,2.81899579737563));
#23276=CARTESIAN_POINT('Ctrl Pts',(31.7071428852578,38.4880837181509,2.66199567002338));
#23277=CARTESIAN_POINT('Ctrl Pts',(36.0928480916297,39.6706871647746,2.50499554267113));
#23278=CARTESIAN_POINT('Ctrl Pts',(39.4985859434327,36.6650407532663,2.34799541531887));
#23279=CARTESIAN_POINT('Ctrl Pts',(38.8703985950797,32.1663360606625,2.19099528796662));
#23280=CARTESIAN_POINT('Ctrl Pts',(34.7715877503781,30.208605539026,2.03399516061437));
#23281=CARTESIAN_POINT('Ctrl Pts',(30.8775962508689,32.547363326415,1.87699503326212));
#23282=CARTESIAN_POINT('Ctrl Pts',(30.6802039639638,37.0854261049008,1.71999490590986));
#23283=CARTESIAN_POINT('Ctrl Pts',(34.3564137772933,39.7534629455386,1.56299477855761));
#23284=CARTESIAN_POINT('Ctrl Pts',(38.6097344321268,38.159032706872,1.40599465120535));
#23285=CARTESIAN_POINT('Ctrl Pts',(39.6261697761982,33.7318499178854,1.2489945238531));
#23286=CARTESIAN_POINT('Ctrl Pts',(36.4942779564007,30.441864951573,1.09199439650085));
#23287=CARTESIAN_POINT('Ctrl Pts',(32.0224453946446,31.2391319593762,0.934994269148593));
#23288=CARTESIAN_POINT('Ctrl Pts',(30.2206294419397,35.4089493247815,0.77799414179634));
#23289=CARTESIAN_POINT('Ctrl Pts',(32.7044910542971,39.2117680815463,0.620994014444087));
#23290=CARTESIAN_POINT('Ctrl Pts',(37.246817707304,39.2384377086451,0.463993887091833));
#23291=CARTESIAN_POINT('Ctrl Pts',(39.7742802645754,35.4632838929154,0.30699375973958));
#23292=CARTESIAN_POINT('Ctrl Pts',(38.0208433725288,31.2750679875305,0.149993632387326));
#23293=CARTESIAN_POINT('Ctrl Pts',(33.5581043558821,30.4222449751611,-0.00700649496492684));
#23294=CARTESIAN_POINT('Ctrl Pts',(30.3892402311535,33.6841941049532,-0.164006622317179));
#23295=CARTESIAN_POINT('Ctrl Pts',(31.0334355704763,36.629077589988,-0.26867337388535));
#23296=CARTESIAN_POINT('Ctrl Pts',(31.9038714051976,37.6471475165632,-0.321006749669435));
#23297=CARTESIAN_POINT('Ctrl Pts',(33.9957950511247,31.243750214851,8.10700224988981));
#23298=CARTESIAN_POINT('Ctrl Pts',(32.7606638781546,31.573953185194,8.05466887410573));
#23299=CARTESIAN_POINT('Ctrl Pts',(30.6617250162538,33.5421236192438,7.95000212253755));
#23300=CARTESIAN_POINT('Ctrl Pts',(31.3907395308691,37.8213068893232,7.79300199518531));
#23301=CARTESIAN_POINT('Ctrl Pts',(35.3622593526719,39.5633387153612,7.63600186783305));
#23302=CARTESIAN_POINT('Ctrl Pts',(39.0059684185923,37.2168872122651,7.4790017404808));
#23303=CARTESIAN_POINT('Ctrl Pts',(39.0589595432527,32.8807998227341,7.32200161312854));
#23304=CARTESIAN_POINT('Ctrl Pts',(35.4715117863422,30.4458788911338,7.16500148577629));
#23305=CARTESIAN_POINT('Ctrl Pts',(31.4616177962741,32.0942554131942,7.00800135842404));
#23306=CARTESIAN_POINT('Ctrl Pts',(30.6244448814073,36.3484528144607,6.85100123107178));
#23307=CARTESIAN_POINT('Ctrl Pts',(33.7109636885558,39.3933744610575,6.69400110371954));
#23308=CARTESIAN_POINT('Ctrl Pts',(37.9533292985792,38.4987673044786,6.53700097636727));
#23309=CARTESIAN_POINT('Ctrl Pts',(39.5474382512424,34.4667560097307,6.38000084901502));
#23310=CARTESIAN_POINT('Ctrl Pts',(37.0638047457115,30.9129225919439,6.22300072166277));
#23311=CARTESIAN_POINT('Ctrl Pts',(32.7295431634706,31.0240043027649,6.06600059431052));
#23312=CARTESIAN_POINT('Ctrl Pts',(30.4312193082136,34.7004026734751,5.90900046695826));
#23313=CARTESIAN_POINT('Ctrl Pts',(32.2297662708491,38.6454512650169,5.75200033960601));
#23314=CARTESIAN_POINT('Ctrl Pts',(36.5124077291574,39.3215895168996,5.59500021225375));
#23315=CARTESIAN_POINT('Ctrl Pts',(39.4388589978718,36.1225166009669,5.4380000849015));
#23316=CARTESIAN_POINT('Ctrl Pts',(38.3849426545962,31.9168724729398,5.28099995754925));
#23317=CARTESIAN_POINT('Ctrl Pts',(34.295715840761,30.4758982808191,5.12399983019699));
#23318=CARTESIAN_POINT('Ctrl Pts',(30.8380273486519,33.0917295501202,4.96699970284475));
#23319=CARTESIAN_POINT('Ctrl Pts',(31.1124196812533,37.4187252153261,4.80999957549248));
#23320=CARTESIAN_POINT('Ctrl Pts',(34.8728425714575,39.5768267874833,4.65299944814023));
#23321=CARTESIAN_POINT('Ctrl Pts',(38.7472887526802,37.6308438653799,4.49599932078798));
#23322=CARTESIAN_POINT('Ctrl Pts',(39.2615051570579,33.3257580129361,4.33899919343573));
#23323=CARTESIAN_POINT('Ctrl Pts',(35.9543890052876,30.5219810107509,4.18199906608348));
#23324=CARTESIAN_POINT('Ctrl Pts',(31.7914630758879,31.7336865972209,4.02499893873122));
#23325=CARTESIAN_POINT('Ctrl Pts',(30.5056629879263,35.8743267469715,3.86799881137897));
#23326=CARTESIAN_POINT('Ctrl Pts',(33.2499780153063,39.2309497154396,3.71099868402671));
#23327=CARTESIAN_POINT('Ctrl Pts',(37.5635545452901,38.7936394831613,3.55399855667446));
#23328=CARTESIAN_POINT('Ctrl Pts',(39.5783671210399,34.954536333721,3.39699842932221));
#23329=CARTESIAN_POINT('Ctrl Pts',(37.4877139761171,31.1562008861948,3.23999830196995));
#23330=CARTESIAN_POINT('Ctrl Pts',(33.1663038435374,30.804636987371,3.0829981746177));
#23331=CARTESIAN_POINT('Ctrl Pts',(30.4891866445685,34.2150953351428,2.92599804726545));
#23332=CARTESIAN_POINT('Ctrl Pts',(31.8569590593748,38.3293852567711,2.76899791991319));
#23333=CARTESIAN_POINT('Ctrl Pts',(36.0431264322094,39.4581834158598,2.61199779256094));
#23334=CARTESIAN_POINT('Ctrl Pts',(39.2939123388708,36.5892858611738,2.45499766520869));
#23335=CARTESIAN_POINT('Ctrl Pts',(38.6943058313741,32.295260175901,2.29799753785643));
#23336=CARTESIAN_POINT('Ctrl Pts',(34.7819798956087,30.4266011464317,2.14099741050418));
#23337=CARTESIAN_POINT('Ctrl Pts',(31.0651545737294,32.6589517221855,1.98399728315193));
#23338=CARTESIAN_POINT('Ctrl Pts',(30.8767431068824,36.9905448059094,1.82699715579967));
#23339=CARTESIAN_POINT('Ctrl Pts',(34.3856952256649,39.5371931204316,1.66999702844742));
#23340=CARTESIAN_POINT('Ctrl Pts',(38.4455011892756,38.015305184674,1.51299690109516));
#23341=CARTESIAN_POINT('Ctrl Pts',(39.4156914491603,33.789547348077,1.35599677374291));
#23342=CARTESIAN_POINT('Ctrl Pts',(36.4262923139345,30.6492478808251,1.19899664639066));
#23343=CARTESIAN_POINT('Ctrl Pts',(32.1579161495709,31.4102413763875,1.0419965190384));
#23344=CARTESIAN_POINT('Ctrl Pts',(30.438077993986,35.3903432264567,0.884996391686151));
#23345=CARTESIAN_POINT('Ctrl Pts',(32.8089305595391,39.0201439210504,0.727996264333897));
#23346=CARTESIAN_POINT('Ctrl Pts',(37.1445935229203,39.0456001515887,0.570996136981644));
#23347=CARTESIAN_POINT('Ctrl Pts',(39.5570633072411,35.4422057173529,0.413996009629391));
#23348=CARTESIAN_POINT('Ctrl Pts',(37.8834030947066,31.4445424115665,0.256995882277137));
#23349=CARTESIAN_POINT('Ctrl Pts',(33.6237067435201,30.63052056076,0.0999957549248841));
#23350=CARTESIAN_POINT('Ctrl Pts',(30.5990174441545,33.7440597469193,-0.0570043724273687));
#23351=CARTESIAN_POINT('Ctrl Pts',(31.2139036219321,36.5549589254462,-0.161671123995539));
#23352=CARTESIAN_POINT('Ctrl Pts',(32.0447369588746,37.5267093987113,-0.214004499779624));
#23353=CARTESIAN_POINT('Ctrl Pts',(34.0436614793107,31.4227955987545,8.21400449977962));
#23354=CARTESIAN_POINT('Ctrl Pts',(32.8674040627957,31.7372591159268,8.16167112399554));
#23355=CARTESIAN_POINT('Ctrl Pts',(30.8685132104295,33.6116147476849,8.05700437242736));
#23356=CARTESIAN_POINT('Ctrl Pts',(31.5627785227536,37.6868264889233,7.90000424507513));
#23357=CARTESIAN_POINT('Ctrl Pts',(35.3449919001376,39.3458226344541,7.74300411772285));
#23358=CARTESIAN_POINT('Ctrl Pts',(38.8150199475273,37.1112170772383,7.58600399037062));
#23359=CARTESIAN_POINT('Ctrl Pts',(38.8654851974986,32.9818136080279,7.42900386301834));
#23360=CARTESIAN_POINT('Ctrl Pts',(35.4490367078385,30.6629556056548,7.27200373566611));
#23361=CARTESIAN_POINT('Ctrl Pts',(31.6302783051062,32.2327606204696,7.11500360831384));
#23362=CARTESIAN_POINT('Ctrl Pts',(30.8330100703084,36.284177469196,6.9580034809616));
#23363=CARTESIAN_POINT('Ctrl Pts',(33.7724068870781,39.1839598954654,6.80100335360933));
#23364=CARTESIAN_POINT('Ctrl Pts',(37.812555918665,38.3319950792405,6.64400322625709));
#23365=CARTESIAN_POINT('Ctrl Pts',(39.3306800817804,34.4921736151651,6.48700309890483));
#23366=CARTESIAN_POINT('Ctrl Pts',(36.9654314387874,31.1077372037044,6.33000297155258));
#23367=CARTESIAN_POINT('Ctrl Pts',(32.8377667479458,31.2135240942401,6.17300284420033));
#23368=CARTESIAN_POINT('Ctrl Pts',(30.6489947863424,34.7146832781773,6.01600271684807));
#23369=CARTESIAN_POINT('Ctrl Pts',(32.3618122182458,38.4716872028325,5.85900258949582));
#23370=CARTESIAN_POINT('Ctrl Pts',(36.4403173097299,39.1155966521051,5.70200246214356));
#23371=CARTESIAN_POINT('Ctrl Pts',(39.2272763665704,36.0690107301504,5.54500233479131));
#23372=CARTESIAN_POINT('Ctrl Pts',(38.2235959945632,32.0638328145787,5.38800220743906));
#23373=CARTESIAN_POINT('Ctrl Pts',(34.3292862460537,30.6915440912579,5.2310020800868));
#23374=CARTESIAN_POINT('Ctrl Pts',(31.0364119167131,33.1826891600592,5.07400195273456));
#23375=CARTESIAN_POINT('Ctrl Pts',(31.2977250657295,37.3034342710318,4.9170018253823));
#23376=CARTESIAN_POINT('Ctrl Pts',(34.8789036568251,39.3586677841964,4.76000169803004));
#23377=CARTESIAN_POINT('Ctrl Pts',(38.5686705053066,37.5054420745486,4.60300157067779));
#23378=CARTESIAN_POINT('Ctrl Pts',(39.0583762730659,33.4055624233101,4.44600144332554));
#23379=CARTESIAN_POINT('Ctrl Pts',(35.9088971036253,30.7354302420101,4.28900131597329));
#23380=CARTESIAN_POINT('Ctrl Pts',(31.9444011812337,31.8893786759165,4.13200118862103));
#23381=CARTESIAN_POINT('Ctrl Pts',(30.7198900339817,35.8326510925229,3.97500106126878));
#23382=CARTESIAN_POINT('Ctrl Pts',(33.333394554677,39.0292772869785,3.81800093391652));
#23383=CARTESIAN_POINT('Ctrl Pts',(37.4413601668615,38.6128118820951,3.66100080656427));
#23384=CARTESIAN_POINT('Ctrl Pts',(39.3601346962212,34.9567034046157,3.50400067921202));
#23385=CARTESIAN_POINT('Ctrl Pts',(37.3691346138881,31.3394193959702,3.34700055185976));
#23386=CARTESIAN_POINT('Ctrl Pts',(33.2537087955707,31.0046131402298,3.19000042450751));
#23387=CARTESIAN_POINT('Ctrl Pts',(30.7041990519258,34.2525085970623,3.03300029715526));
#23388=CARTESIAN_POINT('Ctrl Pts',(32.0067752334918,38.1706867953913,2.876000169803));
#23389=CARTESIAN_POINT('Ctrl Pts',(35.9934047727891,39.2456796669448,2.71900004245075));
#23390=CARTESIAN_POINT('Ctrl Pts',(39.0892387343089,36.5135309690814,2.5619999150985));
#23391=CARTESIAN_POINT('Ctrl Pts',(38.5182130676685,32.4241842911394,2.40499978774624));
#23392=CARTESIAN_POINT('Ctrl Pts',(34.7923720408392,30.6445967538374,2.24799966039399));
#23393=CARTESIAN_POINT('Ctrl Pts',(31.25271289659,32.770540117956,2.09099953304174));
#23394=CARTESIAN_POINT('Ctrl Pts',(31.0732822498009,36.8956635069179,1.93399940568948));
#23395=CARTESIAN_POINT('Ctrl Pts',(34.4149766740365,39.3209232953247,1.77699927833723));
#23396=CARTESIAN_POINT('Ctrl Pts',(38.2812679464245,37.8715776624759,1.61999915098497));
#23397=CARTESIAN_POINT('Ctrl Pts',(39.2052131221224,33.8472447782685,1.46299902363272));
#23398=CARTESIAN_POINT('Ctrl Pts',(36.3583066714682,30.8566308100772,1.30599889628047));
#23399=CARTESIAN_POINT('Ctrl Pts',(32.2933869044973,31.5813507933988,1.14899876892822));
#23400=CARTESIAN_POINT('Ctrl Pts',(30.6555265460323,35.3717371281319,0.991998641575962));
#23401=CARTESIAN_POINT('Ctrl Pts',(32.9133700647812,38.8285197605545,0.834998514223708));
#23402=CARTESIAN_POINT('Ctrl Pts',(37.0423693385366,38.8527625945324,0.677998386871455));
#23403=CARTESIAN_POINT('Ctrl Pts',(39.3398463499068,35.4211275417905,0.520998259519202));
#23404=CARTESIAN_POINT('Ctrl Pts',(37.7459628168843,31.6140168356026,0.363998132166948));
#23405=CARTESIAN_POINT('Ctrl Pts',(33.6893091311581,30.8387961463588,0.206998004814695));
#23406=CARTESIAN_POINT('Ctrl Pts',(30.8087946571555,33.8039253888853,0.0499978774624422));
#23407=CARTESIAN_POINT('Ctrl Pts',(31.3943716733878,36.4808402609044,-0.0546688741057282));
#23408=CARTESIAN_POINT('Ctrl Pts',(32.1856025125517,37.4062712808594,-0.107002249889813));
#23409=CARTESIAN_POINT('Ctrl Pts',(34.0915279074966,31.601840982658,8.32100674966943));
#23410=CARTESIAN_POINT('Ctrl Pts',(32.9741442474368,31.9005650466595,8.26867337388535));
#23411=CARTESIAN_POINT('Ctrl Pts',(31.0753014046052,33.6811058761259,8.16400662231717));
#23412=CARTESIAN_POINT('Ctrl Pts',(31.7348175146381,37.5523460885235,8.00700649496493));
#23413=CARTESIAN_POINT('Ctrl Pts',(35.3277244476034,39.128306553547,7.85000636761267));
#23414=CARTESIAN_POINT('Ctrl Pts',(38.6240714764623,37.0055469422116,7.69300624026043));
#23415=CARTESIAN_POINT('Ctrl Pts',(38.6720108517446,33.0828273933217,7.53600611290816));
#23416=CARTESIAN_POINT('Ctrl Pts',(35.4265616293347,30.8800323201757,7.37900598555592));
#23417=CARTESIAN_POINT('Ctrl Pts',(31.7989388139383,32.371265827745,7.22200585820365));
#23418=CARTESIAN_POINT('Ctrl Pts',(31.0415752592096,36.2199021239313,7.06500573085141));
#23419=CARTESIAN_POINT('Ctrl Pts',(33.8338500856003,38.9745453298735,6.90800560349915));
#23420=CARTESIAN_POINT('Ctrl Pts',(37.6717825387507,38.1652228540024,6.75100547614691));
#23421=CARTESIAN_POINT('Ctrl Pts',(39.1139219123182,34.5175912205995,6.59400534879464));
#23422=CARTESIAN_POINT('Ctrl Pts',(36.8670581318634,31.3025518154648,6.4370052214424));
#23423=CARTESIAN_POINT('Ctrl Pts',(32.9459903324209,31.4030438857154,6.28000509409014));
#23424=CARTESIAN_POINT('Ctrl Pts',(30.8667702644712,34.7289638828794,6.12300496673789));
#23425=CARTESIAN_POINT('Ctrl Pts',(32.4938581656424,38.2979231406482,5.96600483938563));
#23426=CARTESIAN_POINT('Ctrl Pts',(36.3682268903025,38.9096037873106,5.80900471203337));
#23427=CARTESIAN_POINT('Ctrl Pts',(39.0156937352688,36.0155048593341,5.65200458468113));
#23428=CARTESIAN_POINT('Ctrl Pts',(38.0622493345301,32.2107931562174,5.49500445732887));
#23429=CARTESIAN_POINT('Ctrl Pts',(34.3628566513464,30.9071899016968,5.33800432997662));
#23430=CARTESIAN_POINT('Ctrl Pts',(31.2347964847743,33.2736487699982,5.18100420262436));
#23431=CARTESIAN_POINT('Ctrl Pts',(31.4830304502057,37.1881433267374,5.02400407527211));
#23432=CARTESIAN_POINT('Ctrl Pts',(34.8849647421926,39.1405087809095,4.86700394791985));
#23433=CARTESIAN_POINT('Ctrl Pts',(38.3900522579329,37.3800402837173,4.71000382056761));
#23434=CARTESIAN_POINT('Ctrl Pts',(38.855247389074,33.4853668336842,4.55300369321535));
#23435=CARTESIAN_POINT('Ctrl Pts',(35.863405201963,30.9488794732692,4.3960035658631));
#23436=CARTESIAN_POINT('Ctrl Pts',(32.0973392865795,32.0450707546122,4.23900343851084));
#23437=CARTESIAN_POINT('Ctrl Pts',(30.9341170800371,35.7909754380742,4.08200331115859));
#23438=CARTESIAN_POINT('Ctrl Pts',(33.4168110940477,38.8276048585174,3.92500318380633));
#23439=CARTESIAN_POINT('Ctrl Pts',(37.3191657884328,38.4319842810288,3.76800305645409));
#23440=CARTESIAN_POINT('Ctrl Pts',(39.1419022714024,34.9588704755104,3.61100292910183));
#23441=CARTESIAN_POINT('Ctrl Pts',(37.250555251659,31.5226379057457,3.45400280174958));
#23442=CARTESIAN_POINT('Ctrl Pts',(33.3411137476041,31.2045892930886,3.29700267439732));
#23443=CARTESIAN_POINT('Ctrl Pts',(30.9192114592832,34.2899218589819,3.14000254704507));
#23444=CARTESIAN_POINT('Ctrl Pts',(32.1565914076088,38.0119883340115,2.98300241969281));
#23445=CARTESIAN_POINT('Ctrl Pts',(35.9436831133688,39.0331759180299,2.82600229234056));
#23446=CARTESIAN_POINT('Ctrl Pts',(38.884565129747,36.4377760769889,2.66900216498831));
#23447=CARTESIAN_POINT('Ctrl Pts',(38.3421203039629,32.5531084063779,2.51200203763606));
#23448=CARTESIAN_POINT('Ctrl Pts',(34.8027641860698,30.8625923612432,2.3550019102838));
#23449=CARTESIAN_POINT('Ctrl Pts',(31.4402712194505,32.8821285137264,2.19800178293155));
#23450=CARTESIAN_POINT('Ctrl Pts',(31.2698213927195,36.8007822079265,2.04100165557929));
#23451=CARTESIAN_POINT('Ctrl Pts',(34.4442581224081,39.1046534702177,1.88400152822704));
#23452=CARTESIAN_POINT('Ctrl Pts',(38.1170347035733,37.7278501402779,1.72700140087479));
#23453=CARTESIAN_POINT('Ctrl Pts',(38.9947347950846,33.90494220846,1.57000127352253));
#23454=CARTESIAN_POINT('Ctrl Pts',(36.290321029002,31.0640137393293,1.41300114617028));
#23455=CARTESIAN_POINT('Ctrl Pts',(32.4288576594237,31.7524602104101,1.25600101881803));
#23456=CARTESIAN_POINT('Ctrl Pts',(30.8729750980786,35.353131029807,1.09900089146577));
#23457=CARTESIAN_POINT('Ctrl Pts',(33.0178095700233,38.6368956000587,0.94200076411352));
#23458=CARTESIAN_POINT('Ctrl Pts',(36.9401451541529,38.6599250374761,0.785000636761265));
#23459=CARTESIAN_POINT('Ctrl Pts',(39.1226293925725,35.400049366228,0.628000509409013));
#23460=CARTESIAN_POINT('Ctrl Pts',(37.6085225390622,31.7834912596387,0.471000382056759));
#23461=CARTESIAN_POINT('Ctrl Pts',(33.754911518796,31.0470717319576,0.314000254704506));
#23462=CARTESIAN_POINT('Ctrl Pts',(31.0185718701565,33.8637910308514,0.157000127352253));
#23463=CARTESIAN_POINT('Ctrl Pts',(31.5748397248436,36.4067215963626,0.0523333757840826));
#23464=CARTESIAN_POINT('Ctrl Pts',(32.3264680662287,37.2858331630075,-2.22044604925031E-15));
#23465=CARTESIAN_POINT('Ctrl Pts',(32.3264680662287,37.2858331630075,-2.16493489801906E-15));
#23466=CARTESIAN_POINT('Ctrl Pts',(32.2493253814486,37.208720274039,-2.02930540817935E-15));
#23467=CARTESIAN_POINT('Ctrl Pts',(32.1762950504991,37.1279852253981,-2.22088175559797E-15));
#23468=CARTESIAN_POINT('Ctrl Pts',(32.1073693836416,37.0440465177293,-2.44249065417534E-15));
#23469=CARTESIAN_POINT('Ctrl Pts',(32.0366838276613,36.957964590773,-2.66975792514024E-15));
#23470=CARTESIAN_POINT('Ctrl Pts',(31.9703148460741,36.8685128644539,-1.62037951577862E-15));
#23471=CARTESIAN_POINT('Ctrl Pts',(31.9082840182324,36.7760965840633,-1.60982338570648E-15));
#23472=CARTESIAN_POINT('Ctrl Pts',(31.8449621738338,36.681756889908,-1.59904755618531E-15));
#23473=CARTESIAN_POINT('Ctrl Pts',(31.7861605220008,36.5843273727301,-2.0500807145436E-15));
#23474=CARTESIAN_POINT('Ctrl Pts',(31.7319388093681,36.4841996609406,-1.27675647831893E-15));
#23475=CARTESIAN_POINT('Ctrl Pts',(31.6801495481474,36.3885637990409,-5.38124499843711E-16));
#23476=CARTESIAN_POINT('Ctrl Pts',(31.6325385292086,36.2904655679991,-4.81778164441647E-15));
#23477=CARTESIAN_POINT('Ctrl Pts',(31.5891933275412,36.1902216120283,-5.77315972805081E-15));
#23478=CARTESIAN_POINT('Ctrl Pts',(31.5821551531175,36.1739445059149,-5.92828918493564E-15));
#23479=CARTESIAN_POINT('Ctrl Pts',(31.5752295287451,36.1576107865788,-2.14687895786075E-15));
#23480=CARTESIAN_POINT('Ctrl Pts',(31.5684169229622,36.1412217669136,-2.1094237467878E-15));
#23481=CARTESIAN_POINT('Ctrl Pts',(31.5619076362096,36.1255624388982,-2.07363616168158E-15));
#23482=CARTESIAN_POINT('Ctrl Pts',(31.5555045468442,36.1098598194457,-5.01667023260332E-15));
#23483=CARTESIAN_POINT('Ctrl Pts',(31.5492098653947,36.0941205526839,-4.94049245958195E-15));
#23484=CARTESIAN_POINT('Ctrl Pts',(31.5058243818098,35.9856391775398,-4.41544452070402E-15));
#23485=CARTESIAN_POINT('Ctrl Pts',(31.4675527596774,35.875340817696,2.70422581427715E-15));
#23486=CARTESIAN_POINT('Ctrl Pts',(31.4344236193294,35.7636572747171,2.16493489801906E-15));
#23487=CARTESIAN_POINT('Ctrl Pts',(31.4008599589415,35.6505088963383,1.61857067083336E-15));
#23488=CARTESIAN_POINT('Ctrl Pts',(31.3725741668882,35.5359380090966,1.5704555898309E-16));
#23489=CARTESIAN_POINT('Ctrl Pts',(31.3496386440377,35.4203611044154,3.88578058618805E-16));
#23490=CARTESIAN_POINT('Ctrl Pts',(31.3256636190246,35.2995459305591,6.30604259909078E-16));
#23491=CARTESIAN_POINT('Ctrl Pts',(31.3075340503036,35.1776306642325,-4.77206768499493E-16));
#23492=CARTESIAN_POINT('Ctrl Pts',(31.2953883637021,35.0550676565495,-7.49400541621981E-16));
#23493=CARTESIAN_POINT('Ctrl Pts',(31.2862790987509,34.9631454007872,-9.53545871463847E-16));
#23494=CARTESIAN_POINT('Ctrl Pts',(31.2805368906832,34.8708581938176,-1.66063273915206E-15));
#23495=CARTESIAN_POINT('Ctrl Pts',(31.2782432669551,34.7783934177904,-1.83186799063151E-15));
#23496=CARTESIAN_POINT('Ctrl Pts',(31.2776956893352,34.7563184621811,-1.87274853712248E-15));
#23497=CARTESIAN_POINT('Ctrl Pts',(31.2773448230031,34.7342288592592,-1.15850189636716E-15));
#23498=CARTESIAN_POINT('Ctrl Pts',(31.2771918797387,34.7121562214804,-1.19348975147204E-15));
#23499=CARTESIAN_POINT('Ctrl Pts',(31.2763569642807,34.5916619548496,-1.38448803559665E-15));
#23500=CARTESIAN_POINT('Ctrl Pts',(31.2814102215213,34.471522491006,-2.99090776565717E-15));
#23501=CARTESIAN_POINT('Ctrl Pts',(31.2924206159431,34.3521638613563,-2.66453525910038E-15));
#23502=CARTESIAN_POINT('Ctrl Pts',(31.3033603504718,34.2335712231593,-2.34025726846702E-15));
#23503=CARTESIAN_POINT('Ctrl Pts',(31.3201807588279,34.1157485527733,3.70943136885229E-16));
#23504=CARTESIAN_POINT('Ctrl Pts',(31.342998921253,33.9991008864625,6.93889390390723E-16));
#23505=CARTESIAN_POINT('Ctrl Pts',(31.3458725738232,33.9844106208813,7.34560296054722E-16));
#23506=CARTESIAN_POINT('Ctrl Pts',(31.348841419242,33.9697389843081,-2.36384243829245E-16));
#23507=CARTESIAN_POINT('Ctrl Pts',(31.3519057505532,33.9550867820407,-2.22044604925031E-16));
#23508=CARTESIAN_POINT('Ctrl Pts',(31.3758162053254,33.8407581458576,-1.09500521307372E-16));
#23509=CARTESIAN_POINT('Ctrl Pts',(31.405535880703,33.7276122083523,-1.31284998081472E-15));
#23510=CARTESIAN_POINT('Ctrl Pts',(31.4407586285186,33.6159154648327,-2.41473507855972E-15));
#23511=CARTESIAN_POINT('Ctrl Pts',(31.4627238926124,33.5462602385377,-3.10188184234126E-15));
#23512=CARTESIAN_POINT('Ctrl Pts',(31.4868303230444,33.4771686776378,-2.63257088976062E-16));
#23513=CARTESIAN_POINT('Ctrl Pts',(31.5130135264214,33.4087075970126,-2.22044604925031E-16));
#23514=CARTESIAN_POINT('Ctrl Pts',(31.5219635139129,33.385306112999,-2.0795728293307E-16));
#23515=CARTESIAN_POINT('Ctrl Pts',(31.5311562173418,33.361978315516,-2.32755725796262E-15));
#23516=CARTESIAN_POINT('Ctrl Pts',(31.5405892520308,33.3387269417829,-2.58126853225349E-15));
#23517=CARTESIAN_POINT('Ctrl Pts',(31.5473379087033,33.3220922591317,-2.76278066918334E-15));
#23518=CARTESIAN_POINT('Ctrl Pts',(31.5542101234624,33.3054955734371,-8.17270399285879E-16));
#23519=CARTESIAN_POINT('Ctrl Pts',(31.5611979545174,33.288954186216,-7.7715611723761E-16));
#23520=CARTESIAN_POINT('Ctrl Pts',(31.6071192859873,33.1802505670847,-5.13540522049862E-16));
#23521=CARTESIAN_POINT('Ctrl Pts',(31.6580936513602,33.0737733268919,-1.22043518676627E-15));
#23522=CARTESIAN_POINT('Ctrl Pts',(31.713762608453,32.9697768155529,-8.60422844084496E-16));
#23523=CARTESIAN_POINT('Ctrl Pts',(31.7713468082815,32.8622023934125,-4.88024585443386E-16));
#23524=CARTESIAN_POINT('Ctrl Pts',(31.8339543542604,32.7572816421653,-1.6844387016455E-15));
#23525=CARTESIAN_POINT('Ctrl Pts',(31.9012439032021,32.6553034111749,-1.60982338570648E-15));
#23526=CARTESIAN_POINT('Ctrl Pts',(31.9691666425039,32.5523655715406,-1.53450594440749E-15));
#23527=CARTESIAN_POINT('Ctrl Pts',(32.0418603487199,32.4524251462352,-2.14412608245669E-16));
#23528=CARTESIAN_POINT('Ctrl Pts',(32.119024465224,32.3557974897081,-1.11022302462516E-16));
#23529=CARTESIAN_POINT('Ctrl Pts',(32.1734376325243,32.2876593825328,-3.81154351168831E-17));
#23530=CARTESIAN_POINT('Ctrl Pts',(32.2300747937192,32.2211689202647,2.3957932567246E-15));
#23531=CARTESIAN_POINT('Ctrl Pts',(32.2888436140898,32.1564451639975,2.85882428840978E-15));
#23532=CARTESIAN_POINT('Ctrl Pts',(32.3150756619651,32.1275550712175,3.06550279776831E-15));
#23533=CARTESIAN_POINT('Ctrl Pts',(32.3417325486905,32.0990170804093,1.33832078810492E-15));
#23534=CARTESIAN_POINT('Ctrl Pts',(32.3688066730543,32.0708423529797,1.58206781009085E-15));
#23535=CARTESIAN_POINT('Ctrl Pts',(32.3804284156068,32.0587481694606,1.68669779181855E-15));
#23536=CARTESIAN_POINT('Ctrl Pts',(32.3921256212299,32.0467224591722,5.62787663488911E-16));
#23537=CARTESIAN_POINT('Ctrl Pts',(32.4038911827787,32.0347724888588,5.27355936696949E-16));
#23538=CARTESIAN_POINT('Ctrl Pts',(32.4923334498706,31.9449440126051,2.61014017404201E-16));
#23539=CARTESIAN_POINT('Ctrl Pts',(32.584735051869,31.8592881592603,-7.81291389151021E-17));
#23540=CARTESIAN_POINT('Ctrl Pts',(32.6807672456031,31.778123082898,1.11022302462516E-16));
#23541=CARTESIAN_POINT('Ctrl Pts',(32.7628075187761,31.7087837834614,2.72614319871455E-16));
#23542=CARTESIAN_POINT('Ctrl Pts',(32.8474985084852,31.6427220447333,9.36044375735486E-16));
#23543=CARTESIAN_POINT('Ctrl Pts',(32.9346594679295,31.5801538004245,1.38777878078145E-16));
#23544=CARTESIAN_POINT('Ctrl Pts',(32.9737706916096,31.5520779208788,-2.18974819016821E-16));
#23545=CARTESIAN_POINT('Ctrl Pts',(33.0133795255453,31.5247057193814,-1.25086984652678E-15));
#23546=CARTESIAN_POINT('Ctrl Pts',(33.0534708815057,31.4980580630162,-1.7277845820729E-15));
#23547=CARTESIAN_POINT('Ctrl Pts',(33.0807055590029,31.479955898353,-2.0517601300469E-15));
#23548=CARTESIAN_POINT('Ctrl Pts',(33.1081685502538,31.462184715489,8.66601268491E-16));
#23549=CARTESIAN_POINT('Ctrl Pts',(33.1358251623594,31.4447698310871,9.5062846483529E-16));
#23550=CARTESIAN_POINT('Ctrl Pts',(33.2426295858021,31.377516955689,1.27512505265964E-15));
#23551=CARTESIAN_POINT('Ctrl Pts',(33.3523807267505,31.315530896685,3.7726686237795E-15));
#23552=CARTESIAN_POINT('Ctrl Pts',(33.4647766052556,31.2591453155976,2.97331603782425E-15));
#23553=CARTESIAN_POINT('Ctrl Pts',(33.5668702670808,31.2079280421183,2.24723218426034E-15));
#23554=CARTESIAN_POINT('Ctrl Pts',(33.6711468426795,31.1613315802118,-1.73124610826904E-15));
#23555=CARTESIAN_POINT('Ctrl Pts',(33.7774033647392,31.1196350998879,-2.12763834328555E-15));
#23556=CARTESIAN_POINT('Ctrl Pts',(33.8328339031569,31.0978834152884,-2.36077539403599E-15));
#23557=CARTESIAN_POINT('Ctrl Pts',(33.8888035920626,31.0774657030867,3.31895026664625E-16));
#23558=CARTESIAN_POINT('Ctrl Pts',(33.9452683089267,31.0583698510224,1.66533453693773E-16));
#23559=CARTESIAN_POINT('Ctrl Pts',(31.4846882532079,35.0028111988253,7.11258330249198));
#23560=CARTESIAN_POINT('Ctrl Pts',(31.4819571032991,35.3538027877235,7.09672411194513));
#23561=CARTESIAN_POINT('Ctrl Pts',(31.5304045241347,35.7040585316776,7.08086492139827));
#23562=CARTESIAN_POINT('Ctrl Pts',(31.6331816560628,36.037569942224,7.06500573085141));
#23563=CARTESIAN_POINT('Ctrl Pts',(31.9723335346732,37.138116525912,7.01267235506733));
#23564=CARTESIAN_POINT('Ctrl Pts',(32.9030918101368,38.0563309278927,6.96033897928324));
#23565=CARTESIAN_POINT('Ctrl Pts',(34.008126356727,38.3805510495713,6.90800560349915));
#23566=CARTESIAN_POINT('Ctrl Pts',(35.1131609033171,38.7047711712498,6.85567222771507));
#23567=CARTESIAN_POINT('Ctrl Pts',(36.3924717210339,38.4349970126261,6.80333885193099));
#23568=CARTESIAN_POINT('Ctrl Pts',(37.2724836921536,37.6921713277471,6.75100547614691));
#23569=CARTESIAN_POINT('Ctrl Pts',(38.1524956632732,36.9493456428681,6.69867210036282));
#23570=CARTESIAN_POINT('Ctrl Pts',(38.6332087877957,35.7334684317338,6.64633872457873));
#23571=CARTESIAN_POINT('Ctrl Pts',(38.4990880533145,34.5896899253109,6.59400534879465));
#23572=CARTESIAN_POINT('Ctrl Pts',(38.3649673188333,33.4459114188879,6.54167197301056));
#23573=CARTESIAN_POINT('Ctrl Pts',(37.6160127253483,32.3742316171763,6.48933859722648));
#23574=CARTESIAN_POINT('Ctrl Pts',(36.5880241286988,31.8551403946957,6.4370052214424));
#23575=CARTESIAN_POINT('Ctrl Pts',(35.5600355320492,31.336049172215,6.38467184565831));
#23576=CARTESIAN_POINT('Ctrl Pts',(34.2530129322351,31.3695465289652,6.33233846987422));
#23577=CARTESIAN_POINT('Ctrl Pts',(33.2529649543364,31.9406152068676,6.28000509409014));
#23578=CARTESIAN_POINT('Ctrl Pts',(32.2529169764377,32.51168388477,6.22767171830605));
#23579=CARTESIAN_POINT('Ctrl Pts',(31.5598436204544,33.6203238838247,6.17533834252197));
#23580=CARTESIAN_POINT('Ctrl Pts',(31.4844882593247,34.7694704263135,6.12300496673789));
#23581=CARTESIAN_POINT('Ctrl Pts',(31.4794861724725,34.8457507430058,6.11953107865592));
#23582=CARTESIAN_POINT('Ctrl Pts',(31.4772059369411,34.9222095437145,6.11605719057395));
#23583=CARTESIAN_POINT('Ctrl Pts',(31.4775764275568,34.998690818207,6.11258330249198));
#23584=CARTESIAN_POINT('Origin',(-35.,35.,10.2084234471775));
#23585=CARTESIAN_POINT('Ctrl Pts',(-39.0784090602678,35.0020440536088,7.70842344717747));
#23586=CARTESIAN_POINT('Ctrl Pts',(-39.0792531838394,35.133112279499,7.70328437820512));
#23587=CARTESIAN_POINT('Ctrl Pts',(-39.0145240110799,36.5980970201662,7.64581193344869));
#23588=CARTESIAN_POINT('Ctrl Pts',(-37.2468179015868,39.238437726829,7.53600611290815));
#23589=CARTESIAN_POINT('Ctrl Pts',(-32.7044909023729,39.2117683922069,7.37900598555592));
#23590=CARTESIAN_POINT('Ctrl Pts',(-30.2206292307696,35.4089492839864,7.22200585820365));
#23591=CARTESIAN_POINT('Ctrl Pts',(-32.0224452414743,31.2391318114334,7.0650057308514));
#23592=CARTESIAN_POINT('Ctrl Pts',(-36.4942780330333,30.4418647129305,6.90800560349915));
#23593=CARTESIAN_POINT('Ctrl Pts',(-38.8653529438983,32.9326279141667,6.7891448422745));
#23594=CARTESIAN_POINT('Ctrl Pts',(-39.0751757451768,34.6330161300415,6.72261745683394));
#23595=CARTESIAN_POINT('Ctrl Pts',(-39.0721136942453,34.9965451882256,6.70842344717746));
#23596=CARTESIAN_POINT('Ctrl Pts',(-39.0691248821302,34.9959228837483,7.79157655282255));
#23597=CARTESIAN_POINT('Ctrl Pts',(-39.0629617588157,35.8984240805364,7.75638428364687));
#23598=CARTESIAN_POINT('Ctrl Pts',(-38.3270254278953,38.1550448362135,7.6688586386871));
#23599=CARTESIAN_POINT('Ctrl Pts',(-34.6204731393245,39.7808563212243,7.52899961794324));
#23600=CARTESIAN_POINT('Ctrl Pts',(-30.8030827008644,37.3225569109026,7.37199949059099));
#23601=CARTESIAN_POINT('Ctrl Pts',(-30.7475658132336,32.7797862032913,7.21499936323873));
#23602=CARTESIAN_POINT('Ctrl Pts',(-34.5060130464714,30.2288015790917,7.05799923588648));
#23603=CARTESIAN_POINT('Ctrl Pts',(-38.2826807551488,31.7813043056651,6.91685829908108));
#23604=CARTESIAN_POINT('Ctrl Pts',(-39.0636920303636,34.0684206251935,6.82805073805977));
#23605=CARTESIAN_POINT('Ctrl Pts',(-39.070966199943,35.0032555604945,6.79157655282255));
#23606=CARTESIAN_POINT('Ctrl Pts',(-32.3264680662287,37.2858331630075,8.));
#23607=CARTESIAN_POINT('Ctrl Pts',(-31.5748397248436,36.4067215963625,7.94766662421592));
#23608=CARTESIAN_POINT('Ctrl Pts',(-31.0185734566188,33.863789346735,7.84299987264775));
#23609=CARTESIAN_POINT('Ctrl Pts',(-33.7549107807148,31.0470722659105,7.68599974529549));
#23610=CARTESIAN_POINT('Ctrl Pts',(-37.6085229887763,31.7834906538058,7.52899961794324));
#23611=CARTESIAN_POINT('Ctrl Pts',(-39.122629437071,35.4000496587684,7.37199949059099));
#23612=CARTESIAN_POINT('Ctrl Pts',(-36.9401453219176,38.6599250531781,7.21499936323873));
#23613=CARTESIAN_POINT('Ctrl Pts',(-33.0178094388356,38.6368958683166,7.05799923588648));
#23614=CARTESIAN_POINT('Ctrl Pts',(-30.8729749157314,35.3531309945801,6.90099910853423));
#23615=CARTESIAN_POINT('Ctrl Pts',(-32.4288575271599,31.7524600826604,6.74399898118197));
#23616=CARTESIAN_POINT('Ctrl Pts',(-36.2903210951748,31.0640135332596,6.58699885382972));
#23617=CARTESIAN_POINT('Ctrl Pts',(-38.9947349861635,33.9049421642868,6.42999872647747));
#23618=CARTESIAN_POINT('Ctrl Pts',(-38.1170348549754,37.7278502673058,6.27299859912521));
#23619=CARTESIAN_POINT('Ctrl Pts',(-34.4442580951562,39.1046536709688,6.11599847177296));
#23620=CARTESIAN_POINT('Ctrl Pts',(-31.2698212127753,36.8007822935419,5.95899834442071));
#23621=CARTESIAN_POINT('Ctrl Pts',(-31.4402710474498,32.8821284121656,5.80199821706844));
#23622=CARTESIAN_POINT('Ctrl Pts',(-34.8027641765881,30.8625921610582,5.6449980897162));
#23623=CARTESIAN_POINT('Ctrl Pts',(-38.3421204653421,32.553108288411,5.48799796236394));
#23624=CARTESIAN_POINT('Ctrl Pts',(-38.884565317352,36.4377761463179,5.33099783501169));
#23625=CARTESIAN_POINT('Ctrl Pts',(-35.9436831589371,39.0331761128571,5.17399770765944));
#23626=CARTESIAN_POINT('Ctrl Pts',(-32.1565912702954,38.0119884794394,5.01699758030718));
#23627=CARTESIAN_POINT('Ctrl Pts',(-30.9192112622106,34.2899218247053,4.85999745295493));
#23628=CARTESIAN_POINT('Ctrl Pts',(-33.3411136674927,31.2045891097909,4.70299732560268));
#23629=CARTESIAN_POINT('Ctrl Pts',(-37.2505553603438,31.522637737819,4.54599719825043));
#23630=CARTESIAN_POINT('Ctrl Pts',(-39.1419024714255,34.9588704735221,4.38899707089817));
#23631=CARTESIAN_POINT('Ctrl Pts',(-37.3191659004311,38.4319844467691,4.23199694354592));
#23632=CARTESIAN_POINT('Ctrl Pts',(-33.4168110175916,38.8276050433616,4.07499681619367));
#23633=CARTESIAN_POINT('Ctrl Pts',(-30.9341168836852,35.7909754762728,3.91799668884141));
#23634=CARTESIAN_POINT('Ctrl Pts',(-32.0973391464029,32.0450706119108,3.76099656148916));
#23635=CARTESIAN_POINT('Ctrl Pts',(-35.8634052436587,30.9488792776308,3.6039964341369));
#23636=CARTESIAN_POINT('Ctrl Pts',(-38.8552475752543,33.4853667605377,3.44699630678465));
#23637=CARTESIAN_POINT('Ctrl Pts',(-38.390052421646,37.3800403986573,3.2899961794324));
#23638=CARTESIAN_POINT('Ctrl Pts',(-34.8849647366394,39.1405089808617,3.13299605208014));
#23639=CARTESIAN_POINT('Ctrl Pts',(-31.4830302803583,37.1881434324151,2.97599592472789));
#23640=CARTESIAN_POINT('Ctrl Pts',(-31.2347963029507,33.2736486866154,2.81899579737564));
#23641=CARTESIAN_POINT('Ctrl Pts',(-34.3628566205626,30.9071897040694,2.66199567002338));
#23642=CARTESIAN_POINT('Ctrl Pts',(-38.0622494824414,32.2107930214718,2.50499554267113));
#23643=CARTESIAN_POINT('Ctrl Pts',(-39.0156939291453,36.0155049084671,2.34799541531888));
#23644=CARTESIAN_POINT('Ctrl Pts',(-36.368226956474,38.9096039759392,2.19099528796663));
#23645=CARTESIAN_POINT('Ctrl Pts',(-32.4938580444355,38.2979233002502,2.03399516061437));
#23646=CARTESIAN_POINT('Ctrl Pts',(-30.8667700651969,34.7289638691476,1.87699503326212));
#23647=CARTESIAN_POINT('Ctrl Pts',(-32.9459902326247,31.4030437132317,1.71999490590986));
#23648=CARTESIAN_POINT('Ctrl Pts',(-36.8670582231188,31.3025516345889,1.56299477855761));
#23649=CARTESIAN_POINT('Ctrl Pts',(-39.1139221090429,34.517591201676,1.40599465120536));
#23650=CARTESIAN_POINT('Ctrl Pts',(-37.6717826711976,38.1652229986406,1.2489945238531));
#23651=CARTESIAN_POINT('Ctrl Pts',(-33.8338500234071,38.9745455371789,1.09199439650085));
#23652=CARTESIAN_POINT('Ctrl Pts',(-31.041575077848,36.2199021542904,0.934994269148598));
#23653=CARTESIAN_POINT('Ctrl Pts',(-31.7989386437116,32.3712657534865,0.777994141796342));
#23654=CARTESIAN_POINT('Ctrl Pts',(-35.4265616731752,30.8800320247936,0.620994014444089));
#23655=CARTESIAN_POINT('Ctrl Pts',(-38.6720109988941,33.0828274754107,0.463993887091835));
#23656=CARTESIAN_POINT('Ctrl Pts',(-38.6240716788406,37.0055467263343,0.306993759739582));
#23657=CARTESIAN_POINT('Ctrl Pts',(-35.3277244750448,39.1283073075518,0.149993632387328));
#23658=CARTESIAN_POINT('Ctrl Pts',(-31.734817208837,37.552345230412,-0.00700649496492534));
#23659=CARTESIAN_POINT('Ctrl Pts',(-31.0753017580586,33.6811081626476,-0.164006622317179));
#23660=CARTESIAN_POINT('Ctrl Pts',(-32.9741442474368,31.9005650466595,-0.268673373885348));
#23661=CARTESIAN_POINT('Ctrl Pts',(-34.0915279074966,31.601840982658,-0.321006749669432));
#23662=CARTESIAN_POINT('Ctrl Pts',(-32.1856025125516,37.4062712808594,8.10700224988981));
#23663=CARTESIAN_POINT('Ctrl Pts',(-31.3943716733878,36.4808402609044,8.05466887410573));
#23664=CARTESIAN_POINT('Ctrl Pts',(-30.8087963272068,33.8039236160346,7.95000212253756));
#23665=CARTESIAN_POINT('Ctrl Pts',(-33.6893083541881,30.8387967084451,7.79300199518531));
#23666=CARTESIAN_POINT('Ctrl Pts',(-37.7459632902934,31.614016197849,7.63600186783304));
#23667=CARTESIAN_POINT('Ctrl Pts',(-39.3398463967498,35.4211278497445,7.47900174048081));
#23668=CARTESIAN_POINT('Ctrl Pts',(-37.0423695151407,38.8527626110617,7.32200161312853));
#23669=CARTESIAN_POINT('Ctrl Pts',(-32.9133699266814,38.8285200429468,7.1650014857763));
#23670=CARTESIAN_POINT('Ctrl Pts',(-30.6555263540774,35.3717370910488,7.00800135842403));
#23671=CARTESIAN_POINT('Ctrl Pts',(-32.2933867652647,31.5813506589181,6.85100123107178));
#23672=CARTESIAN_POINT('Ctrl Pts',(-36.3583067411276,30.8566305931499,6.69400110371953));
#23673=CARTESIAN_POINT('Ctrl Pts',(-39.2052133232691,33.8472447317679,6.53700097636727));
#23674=CARTESIAN_POINT('Ctrl Pts',(-38.2812681058037,37.8715777961968,6.38000084901503));
#23675=CARTESIAN_POINT('Ctrl Pts',(-34.4149766453488,39.3209235066531,6.22300072166276));
#23676=CARTESIAN_POINT('Ctrl Pts',(-31.0732820603757,36.8956635970443,6.06600059431052));
#23677=CARTESIAN_POINT('Ctrl Pts',(-31.2527127155268,32.770540011044,5.90900046695826));
#23678=CARTESIAN_POINT('Ctrl Pts',(-34.7923720308581,30.644596543105,5.75200033960601));
#23679=CARTESIAN_POINT('Ctrl Pts',(-38.5182132375505,32.424184166957,5.59500021225375));
#23680=CARTESIAN_POINT('Ctrl Pts',(-39.0892389317987,36.5135310420632,5.43800008490151));
#23681=CARTESIAN_POINT('Ctrl Pts',(-35.9934048207584,39.2456798720372,5.28099995754924));
#23682=CARTESIAN_POINT('Ctrl Pts',(-32.0067750889435,38.1706869484817,5.12399983019699));
#23683=CARTESIAN_POINT('Ctrl Pts',(-30.7041988444697,34.2525085609798,4.96699970284475));
#23684=CARTESIAN_POINT('Ctrl Pts',(-33.2537087112384,31.0046129472743,4.80999957549248));
#23685=CARTESIAN_POINT('Ctrl Pts',(-37.3691347282993,31.3394192191957,4.65299944814024));
#23686=CARTESIAN_POINT('Ctrl Pts',(-39.3601349067833,34.9567034025226,4.49599932078798));
#23687=CARTESIAN_POINT('Ctrl Pts',(-37.4413602847608,38.6128120565681,4.33899919343573));
#23688=CARTESIAN_POINT('Ctrl Pts',(-33.3333944741925,39.0292774815619,4.18199906608348));
#23689=CARTESIAN_POINT('Ctrl Pts',(-30.7198898272843,35.8326511327341,4.02499893873122));
#23690=CARTESIAN_POINT('Ctrl Pts',(-31.9444010336713,31.8893785256963,3.86799881137897));
#23691=CARTESIAN_POINT('Ctrl Pts',(-35.9088971475179,30.7354300360637,3.71099868402671));
#23692=CARTESIAN_POINT('Ctrl Pts',(-39.0583764690558,33.4055623463097,3.55399855667446));
#23693=CARTESIAN_POINT('Ctrl Pts',(-38.5686706776456,37.5054421955447,3.39699842932221));
#23694=CARTESIAN_POINT('Ctrl Pts',(-34.8789036509792,39.3586679946839,3.23999830196995));
#23695=CARTESIAN_POINT('Ctrl Pts',(-31.297724886933,37.3034343822775,3.0829981746177));
#23696=CARTESIAN_POINT('Ctrl Pts',(-31.0364117253094,33.1826890722831,2.92599804726545));
#23697=CARTESIAN_POINT('Ctrl Pts',(-34.3292862136479,30.6915438832177,2.76899791991319));
#23698=CARTESIAN_POINT('Ctrl Pts',(-38.2235961502677,32.0638326727334,2.61199779256094));
#23699=CARTESIAN_POINT('Ctrl Pts',(-39.2272765706619,36.0690107818723,2.45499766520869));
#23700=CARTESIAN_POINT('Ctrl Pts',(-36.440317379388,39.1155968506723,2.29799753785644));
#23701=CARTESIAN_POINT('Ctrl Pts',(-32.3618120906526,38.4716873708438,2.14099741050418));
#23702=CARTESIAN_POINT('Ctrl Pts',(-30.6489945765686,34.714683263722,1.98399728315193));
#23703=CARTESIAN_POINT('Ctrl Pts',(-32.8377666428914,31.2135239126685,1.82699715579967));
#23704=CARTESIAN_POINT('Ctrl Pts',(-36.965431534851,31.1077370132983,1.66999702844742));
#23705=CARTESIAN_POINT('Ctrl Pts',(-39.3306802888702,34.4921735952445,1.51299690109517));
#23706=CARTESIAN_POINT('Ctrl Pts',(-37.8125560580904,38.3319952314996,1.35599677374291));
#23707=CARTESIAN_POINT('Ctrl Pts',(-33.7724068216079,39.1839601136936,1.19899664639066));
#23708=CARTESIAN_POINT('Ctrl Pts',(-30.8330098793911,36.2841775011547,1.04199651903841));
#23709=CARTESIAN_POINT('Ctrl Pts',(-31.6302781259105,32.2327605422985,0.884996391686154));
#23710=CARTESIAN_POINT('Ctrl Pts',(-35.4490367539887,30.6629552947093,0.7279962643339));
#23711=CARTESIAN_POINT('Ctrl Pts',(-38.8654853524014,32.981813694442,0.570996136981647));
#23712=CARTESIAN_POINT('Ctrl Pts',(-38.8150201605686,37.1112168499867,0.413996009629392));
#23713=CARTESIAN_POINT('Ctrl Pts',(-35.3449919290248,39.3458234281866,0.256995882277139));
#23714=CARTESIAN_POINT('Ctrl Pts',(-31.5627782008402,37.6868255855989,0.0999957549248854));
#23715=CARTESIAN_POINT('Ctrl Pts',(-30.8685135825059,33.611617154681,-0.0570043724273683));
#23716=CARTESIAN_POINT('Ctrl Pts',(-32.8674040627957,31.7372591159268,-0.161671123995537));
#23717=CARTESIAN_POINT('Ctrl Pts',(-34.0436614793107,31.4227955987545,-0.214004499779622));
#23718=CARTESIAN_POINT('Ctrl Pts',(-32.0447369588746,37.5267093987113,8.21400449977962));
#23719=CARTESIAN_POINT('Ctrl Pts',(-31.2139036219321,36.5549589254462,8.16167112399554));
#23720=CARTESIAN_POINT('Ctrl Pts',(-30.5990191977949,33.7440578853343,8.05700437242737));
#23721=CARTESIAN_POINT('Ctrl Pts',(-33.6237059276614,30.6305211509797,7.90000424507511));
#23722=CARTESIAN_POINT('Ctrl Pts',(-37.8834035918105,31.4445417418923,7.74300411772286));
#23723=CARTESIAN_POINT('Ctrl Pts',(-39.5570633564287,35.4422060407206,7.58600399037061));
#23724=CARTESIAN_POINT('Ctrl Pts',(-37.1445937083637,39.0456001689453,7.42900386301835));
#23725=CARTESIAN_POINT('Ctrl Pts',(-32.8089304145272,39.0201442175769,7.27200373566611));
#23726=CARTESIAN_POINT('Ctrl Pts',(-30.4380777924235,35.3903431875176,7.11500360831384));
#23727=CARTESIAN_POINT('Ctrl Pts',(-32.1579160033695,31.4102412351758,6.9580034809616));
#23728=CARTESIAN_POINT('Ctrl Pts',(-36.4262923870805,30.6492476530402,6.80100335360934));
#23729=CARTESIAN_POINT('Ctrl Pts',(-39.4156916603747,33.7895472992489,6.64400322625709));
#23730=CARTESIAN_POINT('Ctrl Pts',(-38.4455013566321,38.0153053250877,6.48700309890483));
#23731=CARTESIAN_POINT('Ctrl Pts',(-34.3856951955414,39.5371933423375,6.33000297155258));
#23732=CARTESIAN_POINT('Ctrl Pts',(-30.876742907976,36.9905449005467,6.17300284420033));
#23733=CARTESIAN_POINT('Ctrl Pts',(-31.0651543836038,32.6589516099224,6.01600271684807));
#23734=CARTESIAN_POINT('Ctrl Pts',(-34.781979885128,30.4266009251517,5.85900258949583));
#23735=CARTESIAN_POINT('Ctrl Pts',(-38.694306009759,32.295260045503,5.70200246214356));
#23736=CARTESIAN_POINT('Ctrl Pts',(-39.2939125462453,36.5892859378086,5.54500233479132));
#23737=CARTESIAN_POINT('Ctrl Pts',(-36.0431264825797,39.4581836312174,5.38800220743905));
#23738=CARTESIAN_POINT('Ctrl Pts',(-31.8569589075916,38.3293854175239,5.23100208008681));
#23739=CARTESIAN_POINT('Ctrl Pts',(-30.4891864267288,34.2150952972543,5.07400195273455));
#23740=CARTESIAN_POINT('Ctrl Pts',(-33.166303754984,30.8046367847576,4.9170018253823));
#23741=CARTESIAN_POINT('Ctrl Pts',(-37.487714096255,31.1562007005724,4.76000169803004));
#23742=CARTESIAN_POINT('Ctrl Pts',(-39.578367342141,34.9545363315231,4.60300157067779));
#23743=CARTESIAN_POINT('Ctrl Pts',(-37.5635546690906,38.7936396663671,4.44600144332554));
#23744=CARTESIAN_POINT('Ctrl Pts',(-33.2499779307934,39.2309499197622,4.28900131597329));
#23745=CARTESIAN_POINT('Ctrl Pts',(-30.5056627708833,35.8743267891954,4.13200118862103));
#23746=CARTESIAN_POINT('Ctrl Pts',(-31.7914629209398,31.7336864394819,3.97500106126878));
#23747=CARTESIAN_POINT('Ctrl Pts',(-35.9543890513771,30.5219807944966,3.81800093391652));
#23748=CARTESIAN_POINT('Ctrl Pts',(-39.2615053628575,33.3257579320817,3.66100080656427));
#23749=CARTESIAN_POINT('Ctrl Pts',(-38.747288933645,37.630843992432,3.50400067921202));
#23750=CARTESIAN_POINT('Ctrl Pts',(-34.8728425653191,39.5768270085061,3.34700055185976));
#23751=CARTESIAN_POINT('Ctrl Pts',(-31.1124194935077,37.4187253321399,3.19000042450751));
#23752=CARTESIAN_POINT('Ctrl Pts',(-30.8380271476682,33.0917294579507,3.03300029715526));
#23753=CARTESIAN_POINT('Ctrl Pts',(-34.2957158067332,30.4758980623661,2.87600016980301));
#23754=CARTESIAN_POINT('Ctrl Pts',(-38.3849428180941,31.916872323995,2.71900004245075));
#23755=CARTESIAN_POINT('Ctrl Pts',(-39.4388592121786,36.1225166552775,2.5619999150985));
#23756=CARTESIAN_POINT('Ctrl Pts',(-36.5124078023019,39.3215897254055,2.40499978774625));
#23757=CARTESIAN_POINT('Ctrl Pts',(-32.2297661368697,38.6454514414374,2.24799966039399));
#23758=CARTESIAN_POINT('Ctrl Pts',(-30.4312190879402,34.7004026582963,2.09099953304174));
#23759=CARTESIAN_POINT('Ctrl Pts',(-32.7295430531581,31.0240041121053,1.93399940568948));
#23760=CARTESIAN_POINT('Ctrl Pts',(-37.0638048465832,30.9129223920078,1.77699927833723));
#23761=CARTESIAN_POINT('Ctrl Pts',(-39.5474384686975,34.466755988813,1.61999915098498));
#23762=CARTESIAN_POINT('Ctrl Pts',(-37.9533294449832,38.4987674643586,1.46299902363273));
#23763=CARTESIAN_POINT('Ctrl Pts',(-33.7109636198088,39.3933746902084,1.30599889628047));
#23764=CARTESIAN_POINT('Ctrl Pts',(-30.6244446809342,36.348452848019,1.14899876892822));
#23765=CARTESIAN_POINT('Ctrl Pts',(-31.4616176081094,32.0942553311105,0.991998641575964));
#23766=CARTESIAN_POINT('Ctrl Pts',(-35.4715118348024,30.445878564625,0.834998514223711));
#23767=CARTESIAN_POINT('Ctrl Pts',(-39.0589597059086,32.8807999134734,0.677998386871457));
#23768=CARTESIAN_POINT('Ctrl Pts',(-39.0059686422967,37.2168869736391,0.520998259519203));
#23769=CARTESIAN_POINT('Ctrl Pts',(-35.3622593830049,39.5633395488214,0.36399813216695));
#23770=CARTESIAN_POINT('Ctrl Pts',(-31.3907391928433,37.8213059407857,0.206998004814696));
#23771=CARTESIAN_POINT('Ctrl Pts',(-30.6617254069532,33.5421261467143,0.0499978774624425));
#23772=CARTESIAN_POINT('Ctrl Pts',(-32.7606638781546,31.573953185194,-0.0546688741057264));
#23773=CARTESIAN_POINT('Ctrl Pts',(-33.9957950511247,31.243750214851,-0.107002249889811));
#23774=CARTESIAN_POINT('Ctrl Pts',(-31.9038714051976,37.6471475165632,8.32100674966943));
#23775=CARTESIAN_POINT('Ctrl Pts',(-31.0334355704763,36.629077589988,8.26867337388535));
#23776=CARTESIAN_POINT('Ctrl Pts',(-30.3892420683829,33.6841921546339,8.16400662231718));
#23777=CARTESIAN_POINT('Ctrl Pts',(-33.5581035011348,30.4222455935143,8.00700649496493));
#23778=CARTESIAN_POINT('Ctrl Pts',(-38.0208438933277,31.2750672859355,7.85000636761266));
#23779=CARTESIAN_POINT('Ctrl Pts',(-39.7742803161076,35.4632842316967,7.69300624026044));
#23780=CARTESIAN_POINT('Ctrl Pts',(-37.2468179015868,39.238437726829,7.53600611290815));
#23781=CARTESIAN_POINT('Ctrl Pts',(-32.7044909023729,39.2117683922069,7.37900598555592));
#23782=CARTESIAN_POINT('Ctrl Pts',(-30.2206292307696,35.4089492839864,7.22200585820365));
#23783=CARTESIAN_POINT('Ctrl Pts',(-32.0224452414743,31.2391318114334,7.0650057308514));
#23784=CARTESIAN_POINT('Ctrl Pts',(-36.4942780330333,30.4418647129305,6.90800560349915));
#23785=CARTESIAN_POINT('Ctrl Pts',(-39.6261699974803,33.7318498667299,6.7510054761469));
#23786=CARTESIAN_POINT('Ctrl Pts',(-38.6097346074605,38.1590328539788,6.59400534879465));
#23787=CARTESIAN_POINT('Ctrl Pts',(-34.3564137457339,39.7534631780217,6.4370052214424));
#23788=CARTESIAN_POINT('Ctrl Pts',(-30.6802037555765,37.0854262040492,6.28000509409013));
#23789=CARTESIAN_POINT('Ctrl Pts',(-30.8775960516807,32.5473632088007,6.12300496673789));
#23790=CARTESIAN_POINT('Ctrl Pts',(-34.7715877393978,30.2086053071985,5.96600483938563));
#23791=CARTESIAN_POINT('Ctrl Pts',(-38.8703987819675,32.166335924049,5.80900471203337));
#23792=CARTESIAN_POINT('Ctrl Pts',(-39.4985861606919,36.6650408335539,5.65200458468113));
#23793=CARTESIAN_POINT('Ctrl Pts',(-36.092848144401,39.6706873903976,5.49500445732886));
#23794=CARTESIAN_POINT('Ctrl Pts',(-31.7071427262397,38.4880838865661,5.33800432997662));
#23795=CARTESIAN_POINT('Ctrl Pts',(-30.2741740089879,34.1776820335287,5.18100420262436));
#23796=CARTESIAN_POINT('Ctrl Pts',(-33.0788987987297,30.6046606222411,5.02400407527212));
#23797=CARTESIAN_POINT('Ctrl Pts',(-37.6062934642105,30.9729821819491,4.86700394791985));
#23798=CARTESIAN_POINT('Ctrl Pts',(-39.7965997774987,34.9523692605237,4.7100038205676));
#23799=CARTESIAN_POINT('Ctrl Pts',(-37.6857490534203,38.974467276166,4.55300369321535));
#23800=CARTESIAN_POINT('Ctrl Pts',(-33.1665613873943,39.4326223579625,4.3960035658631));
#23801=CARTESIAN_POINT('Ctrl Pts',(-30.2914357144823,35.9160024456566,4.23900343851084));
#23802=CARTESIAN_POINT('Ctrl Pts',(-31.6385248082081,31.5779943532675,4.08200331115859));
#23803=CARTESIAN_POINT('Ctrl Pts',(-35.9998809552364,30.3085315529294,3.92500318380634));
#23804=CARTESIAN_POINT('Ctrl Pts',(-39.464634256659,33.2459535178537,3.76800305645409));
#23805=CARTESIAN_POINT('Ctrl Pts',(-38.9259071896446,37.7562457893193,3.61100292910183));
#23806=CARTESIAN_POINT('Ctrl Pts',(-34.866781479659,39.7949860223284,3.45400280174958));
#23807=CARTESIAN_POINT('Ctrl Pts',(-30.9271141000824,37.5340162820022,3.29700267439732));
#23808=CARTESIAN_POINT('Ctrl Pts',(-30.6396425700269,33.0007698436185,3.14000254704507));
#23809=CARTESIAN_POINT('Ctrl Pts',(-34.2621453998186,30.2602522415144,2.98300241969281));
#23810=CARTESIAN_POINT('Ctrl Pts',(-38.5462894859204,31.7699119752566,2.82600229234057));
#23811=CARTESIAN_POINT('Ctrl Pts',(-39.6504418536953,36.1760225286826,2.66900216498831));
#23812=CARTESIAN_POINT('Ctrl Pts',(-36.5844982252159,39.5275826001387,2.51200203763606));
#23813=CARTESIAN_POINT('Ctrl Pts',(-32.0977201830868,38.819215512031,2.3550019102838));
#23814=CARTESIAN_POINT('Ctrl Pts',(-30.2134435993119,34.6861220528707,2.19800178293155));
#23815=CARTESIAN_POINT('Ctrl Pts',(-32.6213194634248,30.8344843115421,2.04100165557929));
#23816=CARTESIAN_POINT('Ctrl Pts',(-37.1621781583154,30.7181077707172,1.88400152822704));
#23817=CARTESIAN_POINT('Ctrl Pts',(-39.7641966485248,34.4413383823816,1.72700140087479));
#23818=CARTESIAN_POINT('Ctrl Pts',(-38.0941028318759,38.6655396972175,1.57000127352254));
#23819=CARTESIAN_POINT('Ctrl Pts',(-33.6495204180096,39.602789266723,1.41300114617028));
#23820=CARTESIAN_POINT('Ctrl Pts',(-30.4158794824773,36.4127281948833,1.25600101881803));
#23821=CARTESIAN_POINT('Ctrl Pts',(-31.2929570903083,31.9557501199225,1.09900089146578));
#23822=CARTESIAN_POINT('Ctrl Pts',(-35.4939869156159,30.2288018345407,0.942000764113521));
#23823=CARTESIAN_POINT('Ctrl Pts',(-39.2524340594159,32.7797861325047,0.785000636761268));
#23824=CARTESIAN_POINT('Ctrl Pts',(-39.1969171240247,37.3225570972915,0.628000509409013));
#23825=CARTESIAN_POINT('Ctrl Pts',(-35.379526836985,39.7808556694562,0.471000382056761));
#23826=CARTESIAN_POINT('Ctrl Pts',(-31.2187001848465,37.9557862959725,0.314000254704507));
#23827=CARTESIAN_POINT('Ctrl Pts',(-30.4549372314006,33.4726351387477,0.157000127352253));
#23828=CARTESIAN_POINT('Ctrl Pts',(-32.6539236935135,31.4106472544613,0.0523333757840845));
#23829=CARTESIAN_POINT('Ctrl Pts',(-33.9479286229388,31.0647048309474,0.));
#23830=CARTESIAN_POINT('Ctrl Pts',(-33.9479286229388,31.0647048309474,0.));
#23831=CARTESIAN_POINT('Ctrl Pts',(-33.8318205444026,31.104319484649,-6.12910217551102E-18));
#23832=CARTESIAN_POINT('Ctrl Pts',(-33.7179775273608,31.1494845452793,-1.6976040424202E-15));
#23833=CARTESIAN_POINT('Ctrl Pts',(-33.6066254658749,31.1998424056554,-1.16573417585641E-15));
#23834=CARTESIAN_POINT('Ctrl Pts',(-33.4927762352539,31.2513295858929,-6.21936653918048E-16));
#23835=CARTESIAN_POINT('Ctrl Pts',(-33.3815303134372,31.3082455820535,1.45039252013455E-15));
#23836=CARTESIAN_POINT('Ctrl Pts',(-33.2731534080755,31.3702567597409,9.99200722162641E-16));
#23837=CARTESIAN_POINT('Ctrl Pts',(-33.1592150345376,31.4354501023936,5.24855570462807E-16));
#23838=CARTESIAN_POINT('Ctrl Pts',(-33.0484467137175,31.5062753971616,-4.62145718692395E-16));
#23839=CARTESIAN_POINT('Ctrl Pts',(-32.9411963534997,31.5823911623814,-5.55111512312578E-16));
#23840=CARTESIAN_POINT('Ctrl Pts',(-32.8473522883091,31.6489924569487,-6.36456581730239E-16));
#23841=CARTESIAN_POINT('Ctrl Pts',(-32.7562019661932,31.7196453256574,-1.95036301750383E-15));
#23842=CARTESIAN_POINT('Ctrl Pts',(-32.6680099559688,31.7941431443398,-1.99840144432528E-15));
#23843=CARTESIAN_POINT('Ctrl Pts',(-32.6506336549248,31.8088213053349,-2.00786636256454E-15));
#23844=CARTESIAN_POINT('Ctrl Pts',(-32.6333722976869,31.8236487792666,-7.57847684029515E-16));
#23845=CARTESIAN_POINT('Ctrl Pts',(-32.6162280624477,31.8386240567023,-7.7715611723761E-16));
#23846=CARTESIAN_POINT('Ctrl Pts',(-32.6036937742642,31.8495726024021,-7.91272667951259E-16));
#23847=CARTESIAN_POINT('Ctrl Pts',(-32.5912233028683,31.8605991578939,4.81364284937086E-16));
#23848=CARTESIAN_POINT('Ctrl Pts',(-32.5788262971356,31.8716950114967,4.44089209850063E-16));
#23849=CARTESIAN_POINT('Ctrl Pts',(-32.4862471134748,31.9545573647705,1.6572392577578E-16));
#23850=CARTESIAN_POINT('Ctrl Pts',(-32.3976237822216,32.0414014202655,8.13390076176465E-16));
#23851=CARTESIAN_POINT('Ctrl Pts',(-32.3132177297223,32.1319062612438,6.38378239159465E-16));
#23852=CARTESIAN_POINT('Ctrl Pts',(-32.2290034543674,32.222205468154,4.63764042706654E-16));
#23853=CARTESIAN_POINT('Ctrl Pts',(-32.1489867981842,32.3161495489862,3.17588722629917E-16));
#23854=CARTESIAN_POINT('Ctrl Pts',(-32.0734678385385,32.4134518063003,8.88178419700125E-16));
#23855=CARTESIAN_POINT('Ctrl Pts',(-31.9989812077255,32.5094239615292,1.4509682715575E-15));
#23856=CARTESIAN_POINT('Ctrl Pts',(-31.9288697495096,32.6086637947563,-1.05272258015246E-15));
#23857=CARTESIAN_POINT('Ctrl Pts',(-31.8634674410238,32.710917033623,-1.02695629777827E-15));
#23858=CARTESIAN_POINT('Ctrl Pts',(-31.8101619976839,32.7942574287394,-1.00595576833249E-15));
#23859=CARTESIAN_POINT('Ctrl Pts',(-31.7599855228772,32.8796001211512,6.44886685271164E-16));
#23860=CARTESIAN_POINT('Ctrl Pts',(-31.7131447814318,32.9668132818295,6.10622663543836E-16));
#23861=CARTESIAN_POINT('Ctrl Pts',(-31.7012439418187,32.9889715527142,6.01917194448022E-16));
#23862=CARTESIAN_POINT('Ctrl Pts',(-31.6895585553312,33.0112505813609,1.19774783640231E-15));
#23863=CARTESIAN_POINT('Ctrl Pts',(-31.6780922762038,33.0336482309453,1.16573417585641E-15));
#23864=CARTESIAN_POINT('Ctrl Pts',(-31.6699364387253,33.0495794312833,1.14296321331454E-15));
#23865=CARTESIAN_POINT('Ctrl Pts',(-31.661895167037,33.0655634624947,-2.51368181031482E-15));
#23866=CARTESIAN_POINT('Ctrl Pts',(-31.6539721233883,33.0815939077556,-2.4980018054066E-15));
#23867=CARTESIAN_POINT('Ctrl Pts',(-31.6010112907938,33.1887478962384,-2.3931903021702E-15));
#23868=CARTESIAN_POINT('Ctrl Pts',(-31.5532893085976,33.2980517601776,-1.33576692347369E-15));
#23869=CARTESIAN_POINT('Ctrl Pts',(-31.5110849763849,33.409242888583,-1.0547118733939E-15));
#23870=CARTESIAN_POINT('Ctrl Pts',(-31.469716801377,33.5182310852453,-7.79225119096594E-16));
#23871=CARTESIAN_POINT('Ctrl Pts',(-31.4336495378063,33.6290331387016,-1.04560375035282E-15));
#23872=CARTESIAN_POINT('Ctrl Pts',(-31.4031939533011,33.7414155242157,-1.19348975147204E-15));
#23873=CARTESIAN_POINT('Ctrl Pts',(-31.3987398005021,33.7578515350533,-1.2151181935629E-15));
#23874=CARTESIAN_POINT('Ctrl Pts',(-31.3944057673546,33.7743213630571,-1.05328088726205E-15));
#23875=CARTESIAN_POINT('Ctrl Pts',(-31.390192920076,33.7908242908111,-1.11022302462516E-15));
#23876=CARTESIAN_POINT('Ctrl Pts',(-31.3605243708329,33.9070444840312,-1.45504712955035E-15));
#23877=CARTESIAN_POINT('Ctrl Pts',(-31.336861805495,34.0249066128039,2.32711961845814E-15));
#23878=CARTESIAN_POINT('Ctrl Pts',(-31.3191143685546,34.1439748333396,2.41473507855972E-15));
#23879=CARTESIAN_POINT('Ctrl Pts',(-31.3091308324304,34.2109547519018,2.46402175098999E-15));
#23880=CARTESIAN_POINT('Ctrl Pts',(-31.3010200590003,34.2783162816674,1.31577829093223E-15));
#23881=CARTESIAN_POINT('Ctrl Pts',(-31.2947729234008,34.3459803828548,1.66533453693773E-15));
#23882=CARTESIAN_POINT('Ctrl Pts',(-31.2918904510582,34.3772010754682,1.82662224956662E-15));
#23883=CARTESIAN_POINT('Ctrl Pts',(-31.2894048093972,34.4084861625173,5.36743605776751E-16));
#23884=CARTESIAN_POINT('Ctrl Pts',(-31.2873154495445,34.4398277448617,5.55111512312578E-16));
#23885=CARTESIAN_POINT('Ctrl Pts',(-31.2861143588149,34.4578447867584,5.6567049870877E-16));
#23886=CARTESIAN_POINT('Ctrl Pts',(-31.2850447395365,34.4758734447918,-4.83710549279582E-16));
#23887=CARTESIAN_POINT('Ctrl Pts',(-31.2841065224407,34.4939038782769,-4.44089209850063E-16));
#23888=CARTESIAN_POINT('Ctrl Pts',(-31.2777956059898,34.6151855728967,-1.77576305814986E-16));
#23889=CARTESIAN_POINT('Ctrl Pts',(-31.2774172190669,34.7366645735772,1.74591754833025E-15));
#23890=CARTESIAN_POINT('Ctrl Pts',(-31.2828131531898,34.8578936251582,1.77635683940025E-15));
#23891=CARTESIAN_POINT('Ctrl Pts',(-31.2880971535264,34.9766078894115,1.80616469483294E-15));
#23892=CARTESIAN_POINT('Ctrl Pts',(-31.2989188936952,35.0950833906807,2.23513941723243E-15));
#23893=CARTESIAN_POINT('Ctrl Pts',(-31.3151831802674,35.2128941454877,2.73392419813945E-15));
#23894=CARTESIAN_POINT('Ctrl Pts',(-31.3312885576294,35.3295538375714,3.22783563306706E-15));
#23895=CARTESIAN_POINT('Ctrl Pts',(-31.3527309988427,35.445562546077,2.65572620552751E-15));
#23896=CARTESIAN_POINT('Ctrl Pts',(-31.3794648565834,35.5604877518601,3.06699110552699E-15));
#23897=CARTESIAN_POINT('Ctrl Pts',(-31.3968717688464,35.6353176919788,3.33477333511016E-15));
#23898=CARTESIAN_POINT('Ctrl Pts',(-31.4165229425865,35.7096878616141,5.4636862845821E-16));
#23899=CARTESIAN_POINT('Ctrl Pts',(-31.4384155780607,35.7834719630247,4.85722573273506E-16));
#23900=CARTESIAN_POINT('Ctrl Pts',(-31.4458039236167,35.8083726853891,4.65255690113341E-16));
#23901=CARTESIAN_POINT('Ctrl Pts',(-31.45344761912,35.8332066040146,2.20922363074103E-15));
#23902=CARTESIAN_POINT('Ctrl Pts',(-31.4613467446,35.8579686875435,2.27595720048157E-15));
#23903=CARTESIAN_POINT('Ctrl Pts',(-31.4664331437066,35.8739134702743,2.31892823194254E-15));
#23904=CARTESIAN_POINT('Ctrl Pts',(-31.4716246609433,35.8898258563265,-1.15821499265833E-16));
#23905=CARTESIAN_POINT('Ctrl Pts',(-31.4769184371132,35.9056964793841,2.77555756156289E-17));
#23906=CARTESIAN_POINT('Ctrl Pts',(-31.5138161242914,36.0163149237837,1.02848961215397E-15));
#23907=CARTESIAN_POINT('Ctrl Pts',(-31.5557145226016,36.1250218909898,1.27042107846669E-15));
#23908=CARTESIAN_POINT('Ctrl Pts',(-31.6025488384922,36.2313981798515,1.95676808090184E-15));
#23909=CARTESIAN_POINT('Ctrl Pts',(-31.6406629331589,36.3179679496208,2.51532208404033E-15));
#23910=CARTESIAN_POINT('Ctrl Pts',(-31.6820469345646,36.4029939678578,-2.48735046316874E-16));
#23911=CARTESIAN_POINT('Ctrl Pts',(-31.7266869042645,36.4862346415976,-4.02455846426619E-16));
#23912=CARTESIAN_POINT('Ctrl Pts',(-31.748301897583,36.5265403725114,-4.76888559747074E-16));
#23913=CARTESIAN_POINT('Ctrl Pts',(-31.7706805448521,36.566427275075,1.22980137611631E-15));
#23914=CARTESIAN_POINT('Ctrl Pts',(-31.7938227368542,36.6058663963511,1.14491749414469E-15));
#23915=CARTESIAN_POINT('Ctrl Pts',(-31.8074091619825,36.6290204981016,1.09508347207335E-15));
#23916=CARTESIAN_POINT('Ctrl Pts',(-31.8212608195948,36.6520233300662,-7.62339319688486E-16));
#23917=CARTESIAN_POINT('Ctrl Pts',(-31.8353636346369,36.6748465408533,-5.68989300120393E-16));
#23918=CARTESIAN_POINT('Ctrl Pts',(-31.8937950765752,36.7694087337193,2.32107531151829E-16));
#23919=CARTESIAN_POINT('Ctrl Pts',(-31.9565777772527,36.8609657133175,3.78686475409805E-16));
#23920=CARTESIAN_POINT('Ctrl Pts',(-32.0236776904421,36.9491267660533,4.5102810375397E-17));
#23921=CARTESIAN_POINT('Ctrl Pts',(-32.0837084847486,37.0279998639616,-2.53337104489111E-16));
#23922=CARTESIAN_POINT('Ctrl Pts',(-32.1471953789829,37.1041548289018,-7.94184032652028E-16));
#23923=CARTESIAN_POINT('Ctrl Pts',(-32.2141374826654,37.1772853486058,-1.07986536379556E-15));
#23924=CARTESIAN_POINT('Ctrl Pts',(-32.2489924160368,37.2153624219495,-1.21791469682805E-15));
#23925=CARTESIAN_POINT('Ctrl Pts',(-32.2847844521695,37.2526190806637,6.40917790468134E-17));
#23926=CARTESIAN_POINT('Ctrl Pts',(-32.3214761820288,37.2890399271606,-2.77555756156289E-17));
#23927=CARTESIAN_POINT('Ctrl Pts',(-38.5163029138352,34.997016742257,6.38741669750802));
#23928=CARTESIAN_POINT('Ctrl Pts',(-38.5189470194328,34.6831064778252,6.4016107071645));
#23929=CARTESIAN_POINT('Ctrl Pts',(-38.4802904146781,34.3698362574768,6.41580471682098));
#23930=CARTESIAN_POINT('Ctrl Pts',(-38.3977159824674,34.0686054096188,6.42999872647747));
#23931=CARTESIAN_POINT('Ctrl Pts',(-38.0932636891673,32.9579659539444,6.48233210226155));
#23932=CARTESIAN_POINT('Ctrl Pts',(-37.1917923921711,32.010989743602,6.53466547804563));
#23933=CARTESIAN_POINT('Ctrl Pts',(-36.0974794823371,31.6522427299976,6.58699885382972));
#23934=CARTESIAN_POINT('Ctrl Pts',(-35.0031665725032,31.2934957163932,6.6393322296138));
#23935=CARTESIAN_POINT('Ctrl Pts',(-33.7160120498315,31.5229778995268,6.69166560539789));
#23936=CARTESIAN_POINT('Ctrl Pts',(-32.8131210199243,32.2378308097469,6.74399898118197));
#23937=CARTESIAN_POINT('Ctrl Pts',(-31.9102299900171,32.952683719967,6.79633235696605));
#23938=CARTESIAN_POINT('Ctrl Pts',(-31.3916024528742,34.1529073572735,6.84866573275014));
#23939=CARTESIAN_POINT('Ctrl Pts',(-31.4897611048202,35.3003133215496,6.90099910853422));
#23940=CARTESIAN_POINT('Ctrl Pts',(-31.5879197567661,36.4477192858256,6.95333248431831));
#23941=CARTESIAN_POINT('Ctrl Pts',(-32.3028645978009,37.5423075770711,7.00566586010239));
#23942=CARTESIAN_POINT('Ctrl Pts',(-33.3140596654986,38.0934399201708,7.05799923588648));
#23943=CARTESIAN_POINT('Ctrl Pts',(-34.3252547331963,38.6445722632704,7.11033261167056));
#23944=CARTESIAN_POINT('Ctrl Pts',(-35.6327000275569,38.6522486582243,7.16266598745464));
#23945=CARTESIAN_POINT('Ctrl Pts',(-36.6501700272628,38.1127742899662,7.21499936323873));
#23946=CARTESIAN_POINT('Ctrl Pts',(-37.6676400269687,37.5732999217082,7.26733273902281));
#23947=CARTESIAN_POINT('Ctrl Pts',(-38.3951347320199,36.4866747902383,7.3196661148069));
#23948=CARTESIAN_POINT('Ctrl Pts',(-38.5065310098296,35.3406023903429,7.37199949059099));
#23949=CARTESIAN_POINT('Ctrl Pts',(-38.5174699784391,35.2280595814352,7.37713855956333));
#23950=CARTESIAN_POINT('Ctrl Pts',(-38.5224679204996,35.1149435235394,7.38227762853568));
#23951=CARTESIAN_POINT('Ctrl Pts',(-38.521739013009,35.0017650567249,7.38741669750802));
#23952=CARTESIAN_POINT('Ctrl Pts',(-36.0520713770612,31.0647048309474,8.));
#23953=CARTESIAN_POINT('Ctrl Pts',(-37.3460763064866,31.4106472544613,7.94766662421592));
#23954=CARTESIAN_POINT('Ctrl Pts',(-39.5450624630061,33.4726371160361,7.84299987264775));
#23955=CARTESIAN_POINT('Ctrl Pts',(-38.7813000795415,37.9557855546777,7.6859997452955));
#23956=CARTESIAN_POINT('Ctrl Pts',(-34.6204731393245,39.7808563212243,7.52899961794324));
#23957=CARTESIAN_POINT('Ctrl Pts',(-30.8030827008644,37.3225569109026,7.37199949059099));
#23958=CARTESIAN_POINT('Ctrl Pts',(-30.7475658132336,32.7797862032913,7.21499936323873));
#23959=CARTESIAN_POINT('Ctrl Pts',(-34.5060130464714,30.2288015790917,7.05799923588648));
#23960=CARTESIAN_POINT('Ctrl Pts',(-38.707043056971,31.9557500555838,6.90099910853422));
#23961=CARTESIAN_POINT('Ctrl Pts',(-39.5841206744658,36.4127282212004,6.74399898118198));
#23962=CARTESIAN_POINT('Ctrl Pts',(-36.3504796357983,39.6027894460767,6.58699885382972));
#23963=CARTESIAN_POINT('Ctrl Pts',(-31.905897053523,38.6655398223873,6.42999872647746));
#23964=CARTESIAN_POINT('Ctrl Pts',(-30.2358031812474,34.4413383659989,6.27299859912522));
#23965=CARTESIAN_POINT('Ctrl Pts',(-32.8378217627235,30.7181076142107,6.11599847177296));
#23966=CARTESIAN_POINT('Ctrl Pts',(-37.3786806229274,30.8344841622903,5.95899834442071));
#23967=CARTESIAN_POINT('Ctrl Pts',(-39.7865565731199,34.68612204099,5.80199821706845));
#23968=CARTESIAN_POINT('Ctrl Pts',(-37.9022799217924,38.8192156501332,5.6449980897162));
#23969=CARTESIAN_POINT('Ctrl Pts',(-33.4155017175264,39.5275827633586,5.48799796236395));
#23970=CARTESIAN_POINT('Ctrl Pts',(-30.3495579785441,36.176022571197,5.33099783501169));
#23971=CARTESIAN_POINT('Ctrl Pts',(-31.4537103860929,31.7699118586619,5.17399770765944));
#23972=CARTESIAN_POINT('Ctrl Pts',(-35.7378546268185,30.2602520705083,5.01699758030719));
#23973=CARTESIAN_POINT('Ctrl Pts',(-39.3603575873042,33.0007697714678,4.85999745295493));
#23974=CARTESIAN_POINT('Ctrl Pts',(-39.0728860468858,37.5340163734447,4.70299732560268));
#23975=CARTESIAN_POINT('Ctrl Pts',(-35.1332185251462,39.7949861953461,4.54599719825043));
#23976=CARTESIAN_POINT('Ctrl Pts',(-31.0740926686951,37.7562458887763,4.38899707089817));
#23977=CARTESIAN_POINT('Ctrl Pts',(-30.5353655822401,33.2459534545604,4.23199694354592));
#23978=CARTESIAN_POINT('Ctrl Pts',(-34.0001190086845,30.3085313836444,4.07499681619366));
#23979=CARTESIAN_POINT('Ctrl Pts',(-38.3614753130862,31.5779942297887,3.91799668884141));
#23980=CARTESIAN_POINT('Ctrl Pts',(-39.70856445542,35.9160024787098,3.76099656148916));
#23981=CARTESIAN_POINT('Ctrl Pts',(-36.8334386787628,39.4326225179073,3.6039964341369));
#23982=CARTESIAN_POINT('Ctrl Pts',(-32.314250849668,38.9744674195804,3.44699630678465));
#23983=CARTESIAN_POINT('Ctrl Pts',(-30.2034000494222,34.9523692588031,3.2899961794324));
#23984=CARTESIAN_POINT('Ctrl Pts',(-32.3937064417451,30.9729820366429,3.13299605208014));
#23985=CARTESIAN_POINT('Ctrl Pts',(-36.9211012705904,30.6046604636344,2.97599592472789));
#23986=CARTESIAN_POINT('Ctrl Pts',(-39.7258261615381,34.1776820038694,2.81899579737564));
#23987=CARTESIAN_POINT('Ctrl Pts',(-38.2928573925768,38.4880840124043,2.66199567002338));
#23988=CARTESIAN_POINT('Ctrl Pts',(-33.9071518161688,39.6706875589806,2.50499554267113));
#23989=CARTESIAN_POINT('Ctrl Pts',(-30.5014136769744,36.6650408935442,2.34799541531887));
#23990=CARTESIAN_POINT('Ctrl Pts',(-31.1296010783918,32.1663358219723,2.19099528796663));
#23991=CARTESIAN_POINT('Ctrl Pts',(-35.2284122688067,30.2086051339802,2.03399516061437));
#23992=CARTESIAN_POINT('Ctrl Pts',(-39.1224040971504,32.5473631209192,1.87699503326212));
#23993=CARTESIAN_POINT('Ctrl Pts',(-39.319796400129,37.0854262781345,1.71999490590986));
#23994=CARTESIAN_POINT('Ctrl Pts',(-35.6435862778458,39.7534633517259,1.56299477855761));
#23995=CARTESIAN_POINT('Ctrl Pts',(-31.3902652615342,38.1590329639038,1.40599465120536));
#23996=CARTESIAN_POINT('Ctrl Pts',(-30.3738298371754,33.7318498284919,1.2489945238531));
#23997=CARTESIAN_POINT('Ctrl Pts',(-33.5057219097166,30.4418645346457,1.09199439650085));
#23998=CARTESIAN_POINT('Ctrl Pts',(-37.9775548729557,31.2391317008465,0.934994269148598));
#23999=CARTESIAN_POINT('Ctrl Pts',(-39.7793709270477,35.4089492535829,0.777994141796342));
#24000=CARTESIAN_POINT('Ctrl Pts',(-37.2955092110801,39.2117686241983,0.620994014444089));
#24001=CARTESIAN_POINT('Ctrl Pts',(-32.7531819533668,39.2384377406302,0.463993887091835));
#24002=CARTESIAN_POINT('Ctrl Pts',(-30.2257196451616,35.46328448449,0.306993759739582));
#24003=CARTESIAN_POINT('Ctrl Pts',(-31.9791557179606,31.2750667622313,0.149993632387329));
#24004=CARTESIAN_POINT('Ctrl Pts',(-36.4418971366481,30.4222460546565,-0.00700649496492604));
#24005=CARTESIAN_POINT('Ctrl Pts',(-39.6107565597589,33.6841906982476,-0.164006622317178));
#24006=CARTESIAN_POINT('Ctrl Pts',(-38.9665644295237,36.6290775899881,-0.268673373885348));
#24007=CARTESIAN_POINT('Ctrl Pts',(-38.0961285948024,37.6471475165632,-0.321006749669432));
#24008=CARTESIAN_POINT('Ctrl Pts',(-36.0042049488753,31.243750214851,8.10700224988981));
#24009=CARTESIAN_POINT('Ctrl Pts',(-37.2393361218455,31.5739531851941,8.05466887410573));
#24010=CARTESIAN_POINT('Ctrl Pts',(-39.3382743013571,33.5421280340415,7.95000212253756));
#24011=CARTESIAN_POINT('Ctrl Pts',(-38.6092610595157,37.8213052332178,7.79300199518531));
#24012=CARTESIAN_POINT('Ctrl Pts',(-34.6377405943825,39.5633401709358,7.63600186783305));
#24013=CARTESIAN_POINT('Ctrl Pts',(-30.9940311905596,37.2168867957304,7.4790017404808));
#24014=CARTESIAN_POINT('Ctrl Pts',(-30.941040172535,32.8807999810394,7.32200161312854));
#24015=CARTESIAN_POINT('Ctrl Pts',(-34.5284881290099,30.4458783207982,7.16500148577629));
#24016=CARTESIAN_POINT('Ctrl Pts',(-38.5383825324691,32.0942552696991,7.00800135842404));
#24017=CARTESIAN_POINT('Ctrl Pts',(-39.3755554688683,36.3484528731387,6.85100123107178));
#24018=CARTESIAN_POINT('Ctrl Pts',(-36.2890364315511,39.3933748614019,6.69400110371953));
#24019=CARTESIAN_POINT('Ctrl Pts',(-32.0466704456298,38.4987675838335,6.53700097636727));
#24020=CARTESIAN_POINT('Ctrl Pts',(-30.4525613688197,34.4667559731757,6.38000084901503));
#24021=CARTESIAN_POINT('Ctrl Pts',(-32.9361950780481,30.9129222426219,6.22300072166277));
#24022=CARTESIAN_POINT('Ctrl Pts',(-37.2704570292653,31.024003969644,6.06600059431052));
#24023=CARTESIAN_POINT('Ctrl Pts',(-39.5687810766463,34.7004026469562,5.90900046695827));
#24024=CARTESIAN_POINT('Ctrl Pts',(-37.7702339632379,38.6454515732563,5.752000339606));
#24025=CARTESIAN_POINT('Ctrl Pts',(-33.4875921430454,39.3215898811993,5.59500021225376));
#24026=CARTESIAN_POINT('Ctrl Pts',(-30.5611406276935,36.1225166958576,5.4380000849015));
#24027=CARTESIAN_POINT('Ctrl Pts',(-31.6150570597422,31.916872212705,5.28099995754925));
#24028=CARTESIAN_POINT('Ctrl Pts',(-35.7042842186919,30.4758978991403,5.123999830197));
#24029=CARTESIAN_POINT('Ctrl Pts',(-39.1619730025048,33.0917293890828,4.96699970284474));
#24030=CARTESIAN_POINT('Ctrl Pts',(-38.8875806467738,37.4187254194219,4.80999957549249));
#24031=CARTESIAN_POINT('Ctrl Pts',(-35.1271574392675,39.576827173652,4.65299944814024));
#24032=CARTESIAN_POINT('Ctrl Pts',(-31.2527109311398,37.6308440873639,4.49599932078798));
#24033=CARTESIAN_POINT('Ctrl Pts',(-30.7384944833714,33.3257578716681,4.33899919343573));
#24034=CARTESIAN_POINT('Ctrl Pts',(-34.0456109141852,30.5219806329136,4.18199906608347));
#24035=CARTESIAN_POINT('Ctrl Pts',(-38.208537194836,31.7336863216211,4.02499893873123));
#24036=CARTESIAN_POINT('Ctrl Pts',(-39.4943373912889,35.8743268207447,3.86799881137897));
#24037=CARTESIAN_POINT('Ctrl Pts',(-36.7500221323538,39.23095007243,3.71099868402672));
#24038=CARTESIAN_POINT('Ctrl Pts',(-32.4364452384069,38.7936398032564,3.55399855667446));
#24039=CARTESIAN_POINT('Ctrl Pts',(-30.4216324926546,34.9545363298808,3.39699842932221));
#24040=CARTESIAN_POINT('Ctrl Pts',(-32.5122858139794,31.1562005618773,3.23999830196995));
#24041=CARTESIAN_POINT('Ctrl Pts',(-36.8336963111821,30.8046366333671,3.0829981746177));
#24042=CARTESIAN_POINT('Ctrl Pts',(-39.5108137360388,34.2150952689444,2.92599804726545));
#24043=CARTESIAN_POINT('Ctrl Pts',(-38.1430412058191,38.3293855376367,2.7689979199132));
#24044=CARTESIAN_POINT('Ctrl Pts',(-33.9568734797841,39.4581837921304,2.61199779256094));
#24045=CARTESIAN_POINT('Ctrl Pts',(-30.7060872988067,36.5892859950694,2.45499766520869));
#24046=CARTESIAN_POINT('Ctrl Pts',(-31.3056938569536,32.2952599480705,2.29799753785643));
#24047=CARTESIAN_POINT('Ctrl Pts',(-35.2180201227033,30.4266007598144,2.14099741050418));
#24048=CARTESIAN_POINT('Ctrl Pts',(-38.9348457584559,32.6589515260392,1.98399728315193));
#24049=CARTESIAN_POINT('Ctrl Pts',(-39.1232572406452,36.9905449712614,1.82699715579967));
#24050=CARTESIAN_POINT('Ctrl Pts',(-35.6143048269655,39.5371935081385,1.66999702844742));
#24051=CARTESIAN_POINT('Ctrl Pts',(-31.554498518323,38.0153054300115,1.51299690109517));
#24052=CARTESIAN_POINT('Ctrl Pts',(-30.5843081818037,33.7895472627506,1.35599677374291));
#24053=CARTESIAN_POINT('Ctrl Pts',(-33.5737075582741,30.6492474828669,1.19899664639066));
#24054=CARTESIAN_POINT('Ctrl Pts',(-37.8420841058543,31.4102411296202,1.04199651903841));
#24055=CARTESIAN_POINT('Ctrl Pts',(-39.5619223582134,35.3903431584975,0.884996391686153));
#24056=CARTESIAN_POINT('Ctrl Pts',(-37.1910696937641,39.0201444390132,0.7279962643339));
#24057=CARTESIAN_POINT('Ctrl Pts',(-32.8554061531891,39.0456001821187,0.570996136981647));
#24058=CARTESIAN_POINT('Ctrl Pts',(-30.4429366066027,35.4422062820125,0.413996009629392));
#24059=CARTESIAN_POINT('Ctrl Pts',(-32.116596037163,31.4445412420153,0.25699588227714));
#24060=CARTESIAN_POINT('Ctrl Pts',(-36.3762946811041,30.6305215911411,0.0999957549248848));
#24061=CARTESIAN_POINT('Ctrl Pts',(-39.4009794927627,33.7440564952096,-0.057004372427367));
#24062=CARTESIAN_POINT('Ctrl Pts',(-38.7860963780679,36.5549589254462,-0.161671123995537));
#24063=CARTESIAN_POINT('Ctrl Pts',(-37.9552630411254,37.5267093987113,-0.214004499779622));
#24064=CARTESIAN_POINT('Ctrl Pts',(-35.9563385206894,31.4227955987545,8.21400449977962));
#24065=CARTESIAN_POINT('Ctrl Pts',(-37.1325959372044,31.7372591159268,8.16167112399554));
#24066=CARTESIAN_POINT('Ctrl Pts',(-39.1314861397082,33.6116189520467,8.05700437242738));
#24067=CARTESIAN_POINT('Ctrl Pts',(-38.4372220394899,37.6868249117579,7.90000424507511));
#24068=CARTESIAN_POINT('Ctrl Pts',(-34.6550080494404,39.3458240206473,7.74300411772287));
#24069=CARTESIAN_POINT('Ctrl Pts',(-31.1849796802547,37.1112166805582,7.5860039903706));
#24070=CARTESIAN_POINT('Ctrl Pts',(-31.1345145318363,32.9818137587874,7.42900386301836));
#24071=CARTESIAN_POINT('Ctrl Pts',(-34.5509632115484,30.6629550625048,7.2720037356661));
#24072=CARTESIAN_POINT('Ctrl Pts',(-38.3697220079671,32.2327604838143,7.11500360831385));
#24073=CARTESIAN_POINT('Ctrl Pts',(-39.166990263271,36.2841775250771,6.95800348096159));
#24074=CARTESIAN_POINT('Ctrl Pts',(-36.2275932273038,39.1839602767271,6.80100335360935));
#24075=CARTESIAN_POINT('Ctrl Pts',(-32.1874438377366,38.3319953452796,6.64400322625709));
#24076=CARTESIAN_POINT('Ctrl Pts',(-30.6693195563919,34.4921735803525,6.48700309890483));
#24077=CARTESIAN_POINT('Ctrl Pts',(-33.0345683933729,31.1077368710331,6.33000297155259));
#24078=CARTESIAN_POINT('Ctrl Pts',(-37.1622334356032,31.2135237769978,6.17300284420032));
#24079=CARTESIAN_POINT('Ctrl Pts',(-39.3510055801728,34.7146832529224,6.01600271684808));
#24080=CARTESIAN_POINT('Ctrl Pts',(-37.6381880046832,38.4716874963794,5.85900258949581));
#24081=CARTESIAN_POINT('Ctrl Pts',(-33.5596825685645,39.11559699904,5.70200246214357));
#24082=CARTESIAN_POINT('Ctrl Pts',(-30.7727232768428,36.0690108205182,5.54500233479131));
#24083=CARTESIAN_POINT('Ctrl Pts',(-31.7764037333916,32.0638325667482,5.38800220743906));
#24084=CARTESIAN_POINT('Ctrl Pts',(-35.6707138105653,30.6915437277723,5.23100208008681));
#24085=CARTESIAN_POINT('Ctrl Pts',(-38.9635884177054,33.1826890066978,5.07400195273455));
#24086=CARTESIAN_POINT('Ctrl Pts',(-38.7022752466618,37.3034344653991,4.9170018253823));
#24087=CARTESIAN_POINT('Ctrl Pts',(-35.1210963533887,39.3586681519579,4.76000169803004));
#24088=CARTESIAN_POINT('Ctrl Pts',(-31.4313291935845,37.5054422859516,4.6030015706778));
#24089=CARTESIAN_POINT('Ctrl Pts',(-30.9416233845026,33.4055622887757,4.44600144332554));
#24090=CARTESIAN_POINT('Ctrl Pts',(-34.091102819686,30.7354298821828,4.28900131597329));
#24091=CARTESIAN_POINT('Ctrl Pts',(-38.0555990765859,31.8893784134534,4.13200118862103));
#24092=CARTESIAN_POINT('Ctrl Pts',(-39.2801103271579,35.8326511627796,3.97500106126878));
#24093=CARTESIAN_POINT('Ctrl Pts',(-36.6666055859447,39.0292776269525,3.81800093391652));
#24094=CARTESIAN_POINT('Ctrl Pts',(-32.5586396271459,38.6128121869325,3.66100080656428));
#24095=CARTESIAN_POINT('Ctrl Pts',(-30.639864935887,34.9567034009586,3.50400067921202));
#24096=CARTESIAN_POINT('Ctrl Pts',(-32.6308651862137,31.3394190871117,3.34700055185977));
#24097=CARTESIAN_POINT('Ctrl Pts',(-36.7462913517739,31.0046128030999,3.19000042450751));
#24098=CARTESIAN_POINT('Ctrl Pts',(-39.2958013105393,34.2525085340193,3.03300029715526));
#24099=CARTESIAN_POINT('Ctrl Pts',(-37.9932250190614,38.1706870628692,2.876000169803));
#24100=CARTESIAN_POINT('Ctrl Pts',(-34.0065951433993,39.2456800252801,2.71900004245075));
#24101=CARTESIAN_POINT('Ctrl Pts',(-30.9107609206391,36.5135310965947,2.5619999150985));
#24102=CARTESIAN_POINT('Ctrl Pts',(-31.4817866355154,32.4241840741688,2.40499978774625));
#24103=CARTESIAN_POINT('Ctrl Pts',(-35.2076279765999,30.6445963856486,2.24799966039399));
#24104=CARTESIAN_POINT('Ctrl Pts',(-38.7472874197615,32.7705399311592,2.09099953304174));
#24105=CARTESIAN_POINT('Ctrl Pts',(-38.9267180811614,36.8956636643883,1.93399940568948));
#24106=CARTESIAN_POINT('Ctrl Pts',(-35.5850233760853,39.3209236645512,1.77699927833723));
#24107=CARTESIAN_POINT('Ctrl Pts',(-31.7187317751118,37.8715778961193,1.61999915098498));
#24108=CARTESIAN_POINT('Ctrl Pts',(-30.7947865264321,33.8472446970093,1.46299902363273));
#24109=CARTESIAN_POINT('Ctrl Pts',(-33.6416932068317,30.8566304310881,1.30599889628047));
#24110=CARTESIAN_POINT('Ctrl Pts',(-37.7066133387528,31.581350558394,1.14899876892822));
#24111=CARTESIAN_POINT('Ctrl Pts',(-39.3444737893792,35.371737063412,0.991998641575963));
#24112=CARTESIAN_POINT('Ctrl Pts',(-37.086630176448,38.8285202538281,0.834998514223711));
#24113=CARTESIAN_POINT('Ctrl Pts',(-32.9576303530114,38.8527626236071,0.677998386871457));
#24114=CARTESIAN_POINT('Ctrl Pts',(-30.6601535680437,35.421128079535,0.520998259519203));
#24115=CARTESIAN_POINT('Ctrl Pts',(-32.2540363563655,31.6140157217992,0.36399813216695));
#24116=CARTESIAN_POINT('Ctrl Pts',(-36.31069222556,30.8387971276259,0.206998004814696));
#24117=CARTESIAN_POINT('Ctrl Pts',(-39.1912024257666,33.8039222921716,0.0499978774624438));
#24118=CARTESIAN_POINT('Ctrl Pts',(-38.6056283266121,36.4808402609044,-0.0546688741057268));
#24119=CARTESIAN_POINT('Ctrl Pts',(-37.8143974874483,37.4062712808594,-0.107002249889811));
#24120=CARTESIAN_POINT('Ctrl Pts',(-35.9084720925035,31.6018409826581,8.32100674966943));
#24121=CARTESIAN_POINT('Ctrl Pts',(-37.0258557525633,31.9005650466595,8.26867337388535));
#24122=CARTESIAN_POINT('Ctrl Pts',(-38.9246979780591,33.681109870052,8.16400662231719));
#24123=CARTESIAN_POINT('Ctrl Pts',(-38.2651830194642,37.552344590298,8.00700649496492));
#24124=CARTESIAN_POINT('Ctrl Pts',(-34.6722755044984,39.1283078703588,7.85000636761267));
#24125=CARTESIAN_POINT('Ctrl Pts',(-31.3759281699498,37.005546565386,7.69300624026042));
#24126=CARTESIAN_POINT('Ctrl Pts',(-31.3279888911377,33.0828275365354,7.53600611290817));
#24127=CARTESIAN_POINT('Ctrl Pts',(-34.5734382940869,30.8800318042114,7.37900598555591));
#24128=CARTESIAN_POINT('Ctrl Pts',(-38.2010614834652,32.3712656979296,7.22200585820366));
#24129=CARTESIAN_POINT('Ctrl Pts',(-38.9584250576736,36.2199021770154,7.06500573085141));
#24130=CARTESIAN_POINT('Ctrl Pts',(-36.1661500230565,38.9745456920523,6.90800560349915));
#24131=CARTESIAN_POINT('Ctrl Pts',(-32.3282172298434,38.1652231067258,6.7510054761469));
#24132=CARTESIAN_POINT('Ctrl Pts',(-30.8860777439641,34.5175911875294,6.59400534879464));
#24133=CARTESIAN_POINT('Ctrl Pts',(-33.1329417086976,31.3025514994443,6.43700522144239));
#24134=CARTESIAN_POINT('Ctrl Pts',(-37.0540098419411,31.4030435843515,6.28000509409013));
#24135=CARTESIAN_POINT('Ctrl Pts',(-39.1332300836993,34.7289638588885,6.12300496673789));
#24136=CARTESIAN_POINT('Ctrl Pts',(-37.5061420461286,38.2979234195025,5.96600483938563));
#24137=CARTESIAN_POINT('Ctrl Pts',(-33.6317729940835,38.9096041168808,5.80900471203338));
#24138=CARTESIAN_POINT('Ctrl Pts',(-30.9843059259921,36.0155049451787,5.65200458468113));
#24139=CARTESIAN_POINT('Ctrl Pts',(-31.937750407041,32.2107929207913,5.49500445732887));
#24140=CARTESIAN_POINT('Ctrl Pts',(-35.6371434024388,30.9071895564043,5.33800432997662));
#24141=CARTESIAN_POINT('Ctrl Pts',(-38.765203832906,33.2736486243128,5.18100420262436));
#24142=CARTESIAN_POINT('Ctrl Pts',(-38.5169698465499,37.1881435113763,5.02400407527211));
#24143=CARTESIAN_POINT('Ctrl Pts',(-35.1150352675099,39.1405091302639,4.86700394791986));
#24144=CARTESIAN_POINT('Ctrl Pts',(-31.6099474560293,37.3800404845393,4.7100038205676));
#24145=CARTESIAN_POINT('Ctrl Pts',(-31.1447522856339,33.4853667058834,4.55300369321536));
#24146=CARTESIAN_POINT('Ctrl Pts',(-34.1365947251866,30.9488791314519,4.39600356586309));
#24147=CARTESIAN_POINT('Ctrl Pts',(-37.9026609583357,32.0450705052858,4.23900343851085));
#24148=CARTESIAN_POINT('Ctrl Pts',(-39.0658832630269,35.7909755048144,4.08200331115859));
#24149=CARTESIAN_POINT('Ctrl Pts',(-36.5831890395356,38.8276051814752,3.92500318380634));
#24150=CARTESIAN_POINT('Ctrl Pts',(-32.6808340158849,38.4319845706085,3.76800305645408));
#24151=CARTESIAN_POINT('Ctrl Pts',(-30.8580973791193,34.9588704720363,3.61100292910183));
#24152=CARTESIAN_POINT('Ctrl Pts',(-32.7494445584481,31.522637612346,3.45400280174958));
#24153=CARTESIAN_POINT('Ctrl Pts',(-36.6588863923657,31.2045889728327,3.29700267439732));
#24154=CARTESIAN_POINT('Ctrl Pts',(-39.0807888850399,34.2899217990943,3.14000254704507));
#24155=CARTESIAN_POINT('Ctrl Pts',(-37.8434088323037,38.0119885881016,2.98300241969281));
#24156=CARTESIAN_POINT('Ctrl Pts',(-34.0563168070145,39.0331762584299,2.82600229234057));
#24157=CARTESIAN_POINT('Ctrl Pts',(-31.1154345424715,36.4377761981199,2.66900216498831));
#24158=CARTESIAN_POINT('Ctrl Pts',(-31.6578794140771,32.553108200267,2.51200203763606));
#24159=CARTESIAN_POINT('Ctrl Pts',(-35.1972358304966,30.8625920114828,2.3550019102838));
#24160=CARTESIAN_POINT('Ctrl Pts',(-38.559729081067,32.8821283362792,2.19800178293155));
#24161=CARTESIAN_POINT('Ctrl Pts',(-38.7301789216776,36.8007823575152,2.04100165557929));
#24162=CARTESIAN_POINT('Ctrl Pts',(-35.555741925205,39.1046538209638,1.88400152822704));
#24163=CARTESIAN_POINT('Ctrl Pts',(-31.8829650319005,37.727850362227,1.72700140087479));
#24164=CARTESIAN_POINT('Ctrl Pts',(-31.0052648710604,33.904942131268,1.57000127352254));
#24165=CARTESIAN_POINT('Ctrl Pts',(-33.7096788553892,31.0640133793093,1.41300114617028));
#24166=CARTESIAN_POINT('Ctrl Pts',(-37.5711425716514,31.7524599871677,1.25600101881803));
#24167=CARTESIAN_POINT('Ctrl Pts',(-39.127025220545,35.3531309683265,1.09900089146578));
#24168=CARTESIAN_POINT('Ctrl Pts',(-36.982190659132,38.6368960686431,0.942000764113521));
#24169=CARTESIAN_POINT('Ctrl Pts',(-33.0598545528336,38.6599250650956,0.785000636761268));
#24170=CARTESIAN_POINT('Ctrl Pts',(-30.8773705294847,35.4000498770575,0.628000509409013));
#24171=CARTESIAN_POINT('Ctrl Pts',(-32.391476675568,31.7834902015831,0.471000382056762));
#24172=CARTESIAN_POINT('Ctrl Pts',(-36.2450897700159,31.0470726641105,0.314000254704506));
#24173=CARTESIAN_POINT('Ctrl Pts',(-38.9814253587705,33.8637880891336,0.157000127352255));
#24174=CARTESIAN_POINT('Ctrl Pts',(-38.4251602751564,36.4067215963626,0.0523333757840841));
#24175=CARTESIAN_POINT('Ctrl Pts',(-37.6735319337713,37.2858331630075,0.));
#24176=CARTESIAN_POINT('Ctrl Pts',(-37.6735319337713,37.2858331630075,0.));
#24177=CARTESIAN_POINT('Ctrl Pts',(-37.7506745369995,37.2087203555594,1.28363488612132E-16));
#24178=CARTESIAN_POINT('Ctrl Pts',(-37.8237047828546,37.1279853831031,-1.45961390077584E-15));
#24179=CARTESIAN_POINT('Ctrl Pts',(-37.8926303634218,37.044046747423,-1.27675647831893E-15));
#24180=CARTESIAN_POINT('Ctrl Pts',(-37.9633158416367,36.9579648812288,-1.08923010211539E-15));
#24181=CARTESIAN_POINT('Ctrl Pts',(-38.0296847428869,36.8685132102372,2.69373606469353E-15));
#24182=CARTESIAN_POINT('Ctrl Pts',(-38.0917154903142,36.776096981172,2.1094237467878E-15));
#24183=CARTESIAN_POINT('Ctrl Pts',(-38.1550372699928,36.6817573135345,1.51295026561079E-15));
#24184=CARTESIAN_POINT('Ctrl Pts',(-38.2138388545422,36.5843278170101,-6.22870230136456E-16));
#24185=CARTESIAN_POINT('Ctrl Pts',(-38.2680604999532,36.4842001218513,-1.22124532708767E-15));
#24186=CARTESIAN_POINT('Ctrl Pts',(-38.3198497467852,36.3885641838418,-1.7927771454093E-15));
#24187=CARTESIAN_POINT('Ctrl Pts',(-38.3674607433557,36.2904658682844,-1.21061342909026E-15));
#24188=CARTESIAN_POINT('Ctrl Pts',(-38.4108059167409,36.1902218218841,-1.49880108324396E-15));
#24189=CARTESIAN_POINT('Ctrl Pts',(-38.4178437109143,36.1739455698685,-1.54559303803029E-15));
#24190=CARTESIAN_POINT('Ctrl Pts',(-38.4247689668943,36.1576127105175,5.76904931418396E-16));
#24191=CARTESIAN_POINT('Ctrl Pts',(-38.4315812162273,36.1412245565248,6.10622663543836E-16));
#24192=CARTESIAN_POINT('Ctrl Pts',(-38.4380909127403,36.1255642505548,6.42842888099819E-16));
#24193=CARTESIAN_POINT('Ctrl Pts',(-38.4444943995979,36.1098606451587,1.94214412995646E-15));
#24194=CARTESIAN_POINT('Ctrl Pts',(-38.4507894645608,36.0941203888398,1.88737914186277E-15));
#24195=CARTESIAN_POINT('Ctrl Pts',(-38.4941748650482,35.9856390104596,1.50994047282167E-15));
#24196=CARTESIAN_POINT('Ctrl Pts',(-38.5324464076346,35.8753406458803,4.14672721999528E-16));
#24197=CARTESIAN_POINT('Ctrl Pts',(-38.5655754746426,35.7636570985597,-1.11022302462516E-16));
#24198=CARTESIAN_POINT('Ctrl Pts',(-38.599139072954,35.6505086745683,-6.43612508853869E-16));
#24199=CARTESIAN_POINT('Ctrl Pts',(-38.6274248054533,35.535937741082,5.81275891054099E-16));
#24200=CARTESIAN_POINT('Ctrl Pts',(-38.6503602739825,35.4203607919199,1.85962356624714E-15));
#24201=CARTESIAN_POINT('Ctrl Pts',(-38.6743352598313,35.2995454827809,3.19591052212541E-15));
#24202=CARTESIAN_POINT('Ctrl Pts',(-38.692464786516,35.1776300814803,-8.4407659709162E-16));
#24203=CARTESIAN_POINT('Ctrl Pts',(-38.7046104310317,35.0550669428354,-1.38777878078145E-15));
#24204=CARTESIAN_POINT('Ctrl Pts',(-38.7137196644185,34.9631445888517,-1.79555541854881E-15));
#24205=CARTESIAN_POINT('Ctrl Pts',(-38.7194618408911,34.8708572859148,2.82896256593911E-15));
#24206=CARTESIAN_POINT('Ctrl Pts',(-38.721755434165,34.7783924177428,2.94209101525666E-15));
#24207=CARTESIAN_POINT('Ctrl Pts',(-38.7223030074901,34.7563173201712,2.96909934400004E-15));
#24208=CARTESIAN_POINT('Ctrl Pts',(-38.7226538674535,34.7342275752707,-2.60000342473094E-16));
#24209=CARTESIAN_POINT('Ctrl Pts',(-38.7228068022813,34.7121547959299,-2.77555756156289E-16));
#24210=CARTESIAN_POINT('Ctrl Pts',(-38.7236416666969,34.5916604762348,-3.73389977849103E-16));
#24211=CARTESIAN_POINT('Ctrl Pts',(-38.7185883671926,34.4715209673338,1.72146304164403E-15));
#24212=CARTESIAN_POINT('Ctrl Pts',(-38.7075779418993,34.3521623032552,1.58206781009085E-15));
#24213=CARTESIAN_POINT('Ctrl Pts',(-38.6966381726954,34.2335695874665,1.44356710546673E-15));
#24214=CARTESIAN_POINT('Ctrl Pts',(-38.6798177366068,34.1157468505408,1.14312909921041E-17));
#24215=CARTESIAN_POINT('Ctrl Pts',(-38.6569995558515,33.9990991317786,-2.77555756156289E-16));
#24216=CARTESIAN_POINT('Ctrl Pts',(-38.654125907022,33.9844088905153,-3.13949862184534E-16));
#24217=CARTESIAN_POINT('Ctrl Pts',(-38.6511570658937,33.9697372784049,2.13659354022824E-15));
#24218=CARTESIAN_POINT('Ctrl Pts',(-38.6480927394297,33.9550851007466,2.1094237467878E-15));
#24219=CARTESIAN_POINT('Ctrl Pts',(-38.6241822697972,33.8407564046822,1.89676768741005E-15));
#24220=CARTESIAN_POINT('Ctrl Pts',(-38.5944625878303,33.7276104213963,7.3858195394121E-16));
#24221=CARTESIAN_POINT('Ctrl Pts',(-38.5592398399973,33.6159136444833,2.4980018054066E-16));
#24222=CARTESIAN_POINT('Ctrl Pts',(-38.5372745858279,33.5462584288701,-5.50089711192647E-17));
#24223=CARTESIAN_POINT('Ctrl Pts',(-38.5131681698132,33.4771668829623,6.13912691963219E-16));
#24224=CARTESIAN_POINT('Ctrl Pts',(-38.4869849848521,33.408705821156,6.93889390390723E-16));
#24225=CARTESIAN_POINT('Ctrl Pts',(-38.478035242453,33.3853049679579,7.21226433226402E-16));
#24226=CARTESIAN_POINT('Ctrl Pts',(-38.4688427975352,33.3619777978058,1.17968218996551E-15));
#24227=CARTESIAN_POINT('Ctrl Pts',(-38.4594100345669,33.3387270476804,1.30451205393456E-15));
#24228=CARTESIAN_POINT('Ctrl Pts',(-38.4526611227965,33.3220917032197,1.39382477610025E-15));
#24229=CARTESIAN_POINT('Ctrl Pts',(-38.4457886431155,33.3054943585584,8.23245697379087E-16));
#24230=CARTESIAN_POINT('Ctrl Pts',(-38.4388005380928,33.2889523169239,7.49400541621981E-16));
#24231=CARTESIAN_POINT('Ctrl Pts',(-38.3928792100309,33.1802486671866,2.64137711097381E-16));
#24232=CARTESIAN_POINT('Ctrl Pts',(-38.3419048511529,33.0737714082961,1.17255001397609E-15));
#24233=CARTESIAN_POINT('Ctrl Pts',(-38.2862359020984,32.9697748885158,9.43689570931383E-16));
#24234=CARTESIAN_POINT('Ctrl Pts',(-38.2286517312081,32.8622004961707,7.06955465363536E-16));
#24235=CARTESIAN_POINT('Ctrl Pts',(-38.1660442194156,32.7572797837933,2.65690729149937E-16));
#24236=CARTESIAN_POINT('Ctrl Pts',(-38.0987547078419,32.6553015987604,4.44089209850063E-16));
#24237=CARTESIAN_POINT('Ctrl Pts',(-38.0308320192805,32.5523638252493,6.24166374344619E-16));
#24238=CARTESIAN_POINT('Ctrl Pts',(-37.9581383688774,32.4524234721426,-1.26765506881022E-15));
#24239=CARTESIAN_POINT('Ctrl Pts',(-37.8809743110047,32.3557958917759,-1.62370117351429E-15));
#24240=CARTESIAN_POINT('Ctrl Pts',(-37.82656120339,32.2876578612733,-1.87477110872936E-15));
#24241=CARTESIAN_POINT('Ctrl Pts',(-37.7699241047827,32.2211674765398,1.39931090156461E-15));
#24242=CARTESIAN_POINT('Ctrl Pts',(-37.7111553490298,32.1564437978227,1.60982338570648E-15));
#24243=CARTESIAN_POINT('Ctrl Pts',(-37.6849229569216,32.1275533287794,1.70378906452554E-15));
#24244=CARTESIAN_POINT('Ctrl Pts',(-37.6582657142846,32.0990149717255,2.33543966985802E-16));
#24245=CARTESIAN_POINT('Ctrl Pts',(-37.6311912225754,32.0708398884709,3.05311331771918E-16));
#24246=CARTESIAN_POINT('Ctrl Pts',(-37.6195692277271,32.0587454537553,3.36118186902312E-16));
#24247=CARTESIAN_POINT('Ctrl Pts',(-37.6078717672662,32.0467194961249,-1.14899013469077E-15));
#24248=CARTESIAN_POINT('Ctrl Pts',(-37.5961059477358,32.034769281675,-1.17961196366423E-15));
#24249=CARTESIAN_POINT('Ctrl Pts',(-37.5076636824121,31.9449409416833,-1.40979260818075E-15));
#24250=CARTESIAN_POINT('Ctrl Pts',(-37.4152620841693,31.8592852286376,-2.45663089159861E-15));
#24251=CARTESIAN_POINT('Ctrl Pts',(-37.3192298936088,31.778120294682,-2.019218126037E-15));
#24252=CARTESIAN_POINT('Ctrl Pts',(-37.2371898445147,31.7087813040001,-1.64553754506066E-15));
#24253=CARTESIAN_POINT('Ctrl Pts',(-37.1524990927587,31.6427198578901,-2.42654488972963E-15));
#24254=CARTESIAN_POINT('Ctrl Pts',(-37.0653383821438,31.5801518871639,-2.52575738102223E-15));
#24255=CARTESIAN_POINT('Ctrl Pts',(-37.0262273476737,31.5520761860535,-2.57027632928952E-15));
#24256=CARTESIAN_POINT('Ctrl Pts',(-36.9866187071144,31.524704156366,-1.17712968719052E-15));
#24257=CARTESIAN_POINT('Ctrl Pts',(-36.946527548351,31.4980566647868,-6.31439345255558E-16));
#24258=CARTESIAN_POINT('Ctrl Pts',(-36.9192934800282,31.479954927928,-2.60749933581654E-16));
#24259=CARTESIAN_POINT('Ctrl Pts',(-36.89183110785,31.4621841581827,-1.11508673223599E-15));
#24260=CARTESIAN_POINT('Ctrl Pts',(-36.8641751230777,31.4447696709256,-1.17267306976032E-15));
#24261=CARTESIAN_POINT('Ctrl Pts',(-36.757370770553,31.3775168483861,-1.39506513224507E-15));
#24262=CARTESIAN_POINT('Ctrl Pts',(-36.6476196941272,31.3155308365787,-2.17833836995006E-15));
#24263=CARTESIAN_POINT('Ctrl Pts',(-36.5352238715355,31.2591452947779,-6.38378239159465E-16));
#24264=CARTESIAN_POINT('Ctrl Pts',(-36.4331301648989,31.2079280090246,7.60430312613923E-16));
#24265=CARTESIAN_POINT('Ctrl Pts',(-36.3288535333025,31.1613315369686,5.40797342115576E-17));
#24266=CARTESIAN_POINT('Ctrl Pts',(-36.2225969429285,31.1196350477066,-1.58727198051878E-16));
#24267=CARTESIAN_POINT('Ctrl Pts',(-36.1671664218874,31.0978833792477,-2.38185072021888E-16));
#24268=CARTESIAN_POINT('Ctrl Pts',(-36.1111967480356,31.0774656809663,2.2162435752245E-16));
#24269=CARTESIAN_POINT('Ctrl Pts',(-36.0547320440516,31.0583698407596,1.38777878078145E-16));
#24270=CARTESIAN_POINT('Ctrl Pts',(-38.5153120432796,35.002811202661,7.11258330249199));
#24271=CARTESIAN_POINT('Ctrl Pts',(-38.5180431912138,35.3538028140734,7.09672411194513));
#24272=CARTESIAN_POINT('Ctrl Pts',(-38.4695957643305,35.7040585809451,7.08086492139827));
#24273=CARTESIAN_POINT('Ctrl Pts',(-38.3668186228693,36.0375700163406,7.06500573085141));
#24274=CARTESIAN_POINT('Ctrl Pts',(-38.0276667128012,37.1381166820277,7.01267235506732));
#24275=CARTESIAN_POINT('Ctrl Pts',(-37.0969083679288,38.05633118704,6.96033897928324));
#24276=CARTESIAN_POINT('Ctrl Pts',(-35.9918737299572,38.3805513419917,6.90800560349915));
#24277=CARTESIAN_POINT('Ctrl Pts',(-34.8868390919855,38.7047714969434,6.85567222771507));
#24278=CARTESIAN_POINT('Ctrl Pts',(-33.6075281609145,38.4349973018346,6.80333885193099));
#24279=CARTESIAN_POINT('Ctrl Pts',(-32.7275161143991,37.6921715510808,6.7510054761469));
#24280=CARTESIAN_POINT('Ctrl Pts',(-31.8475040678837,36.949345800327,6.69867210036282));
#24281=CARTESIAN_POINT('Ctrl Pts',(-31.3667909059239,35.7334684939282,6.64633872457873));
#24282=CARTESIAN_POINT('Ctrl Pts',(-31.5009116523996,34.5896898927146,6.59400534879465));
#24283=CARTESIAN_POINT('Ctrl Pts',(-31.6350323988753,33.445911291501,6.54167197301056));
#24284=CARTESIAN_POINT('Ctrl Pts',(-32.3839870537864,32.3742313954726,6.48933859722648));
#24285=CARTESIAN_POINT('Ctrl Pts',(-33.4119757367826,31.8551401282763,6.43700522144239));
#24286=CARTESIAN_POINT('Ctrl Pts',(-34.4399644197788,31.33604886108,6.38467184565831));
#24287=CARTESIAN_POINT('Ctrl Pts',(-35.74698713086,31.3695462227158,6.33233846987422));
#24288=CARTESIAN_POINT('Ctrl Pts',(-36.7470351933603,31.9406149492898,6.28000509409014));
#24289=CARTESIAN_POINT('Ctrl Pts',(-37.7470832558605,32.5116836758639,6.22767171830605));
#24290=CARTESIAN_POINT('Ctrl Pts',(-38.4401566697799,33.6203237673762,6.17533834252197));
#24291=CARTESIAN_POINT('Ctrl Pts',(-38.5155120371445,34.769470406568,6.12300496673789));
#24292=CARTESIAN_POINT('Ctrl Pts',(-38.5205141244106,34.8457507296795,6.11953107865592));
#24293=CARTESIAN_POINT('Ctrl Pts',(-38.5227943601281,34.922209536826,6.11605719057395));
#24294=CARTESIAN_POINT('Ctrl Pts',(-38.5224238694764,34.9986908177615,6.11258330249199));
#24295=CARTESIAN_POINT('Origin',(35.,-35.,4.));
#24296=CARTESIAN_POINT('Origin',(-35.,-35.,4.));
#24297=CARTESIAN_POINT('Origin',(-35.,35.,4.));
#24298=CARTESIAN_POINT('Origin',(35.,35.,4.));
#24299=CARTESIAN_POINT('Origin',(50.,50.,0.));
#24300=CARTESIAN_POINT('',(50.,50.,0.));
#24301=CARTESIAN_POINT('',(-50.,50.,0.));
#24302=CARTESIAN_POINT('',(50.,50.,0.));
#24303=CARTESIAN_POINT('',(-50.,50.,0.));
#24304=CARTESIAN_POINT('',(50.,50.,0.));
#24305=CARTESIAN_POINT('Origin',(50.,-50.,0.));
#24306=CARTESIAN_POINT('',(50.,-50.,0.));
#24307=CARTESIAN_POINT('',(50.,-50.,0.));
#24308=CARTESIAN_POINT('',(50.,-50.,0.));
#24309=CARTESIAN_POINT('Origin',(-50.,-50.,0.));
#24310=CARTESIAN_POINT('',(-50.,-50.,0.));
#24311=CARTESIAN_POINT('',(-50.,-50.,0.));
#24312=CARTESIAN_POINT('',(-50.,-50.,0.));
#24313=CARTESIAN_POINT('Origin',(-50.,50.,0.));
#24314=CARTESIAN_POINT('',(-50.,50.,0.));
#24315=CARTESIAN_POINT('Origin',(0.,0.,0.));
#24316=CARTESIAN_POINT('',(0.,0.,0.));
#24317=CARTESIAN_POINT('Origin',(0.,0.,0.));
#24318=CARTESIAN_POINT('',(-3.94684541635378,0.00250618816942501,0.322176117089595));
#24319=CARTESIAN_POINT('',(-3.94571229786942,0.00420644411048898,0.1778238829104));
#24320=CARTESIAN_POINT('',(-3.942,-4.82755768223887E-16,0.));
#24321=CARTESIAN_POINT('',(1.7270326134187,3.54354657824448,0.));
#24322=CARTESIAN_POINT('Ctrl Pts',(-3.94684541635378,0.00250618816942501,
0.322176117089595));
#24323=CARTESIAN_POINT('Ctrl Pts',(-3.94773112778461,0.132835587750837,
0.316895328369763));
#24324=CARTESIAN_POINT('Ctrl Pts',(-3.94183789351545,0.26307859818693,0.311614539649932));
#24325=CARTESIAN_POINT('Ctrl Pts',(-3.92890301514817,0.39261184999977,0.3063337509301));
#24326=CARTESIAN_POINT('Ctrl Pts',(-3.79917189807037,1.69177315474756,0.253369772435476));
#24327=CARTESIAN_POINT('Ctrl Pts',(-2.96110743411295,2.91953839146377,0.200405793940852));
#24328=CARTESIAN_POINT('Ctrl Pts',(-1.79852789548214,3.51470668248002,0.147441815446229));
#24329=CARTESIAN_POINT('Ctrl Pts',(-0.719726524887938,4.06698577113378,
0.098294543630819));
#24330=CARTESIAN_POINT('Ctrl Pts',(0.638504507243322,4.07455564834572,0.0491472718154096));
#24331=CARTESIAN_POINT('Ctrl Pts',(1.73118107496479,3.54876586530513,-4.77048955893622E-17));
#24332=CARTESIAN_POINT('',(-1.72703261341866,3.5435465782445,0.));
#24333=CARTESIAN_POINT('Origin',(0.,0.,0.));
#24334=CARTESIAN_POINT('Ctrl Pts',(-1.72703261341866,3.5435465782445,-1.38777878078145E-15));
#24335=CARTESIAN_POINT('Ctrl Pts',(-2.90680413394004,2.96855656546122,0.0529882887282479));
#24336=CARTESIAN_POINT('Ctrl Pts',(-3.76655616656995,1.76297958901422,0.105976577456497));
#24337=CARTESIAN_POINT('Ctrl Pts',(-3.92036033233788,0.467860933696955,
0.158964866184747));
#24338=CARTESIAN_POINT('Ctrl Pts',(-3.93860710223307,0.314212741058287,
0.165251205093298));
#24339=CARTESIAN_POINT('Ctrl Pts',(-3.94691794439651,0.159304285881835,
0.171537544001849));
#24340=CARTESIAN_POINT('Ctrl Pts',(-3.94571229786942,0.00420644411048898,
0.1778238829104));
#24341=CARTESIAN_POINT('Origin',(0.,0.,0.));
#24342=CARTESIAN_POINT('',(-3.93670753965503,0.00216852164164449,1.32217611708959));
#24343=CARTESIAN_POINT('',(-3.93636006504333,0.00190811380198534,1.1778238829104));
#24344=CARTESIAN_POINT('',(-3.942,-4.82755768223887E-16,0.));
#24345=CARTESIAN_POINT('Ctrl Pts',(-3.93670753965503,0.00216852164164449,
1.32217611708959));
#24346=CARTESIAN_POINT('Ctrl Pts',(-3.93928378279248,0.519701728735777,
1.30134586600417));
#24347=CARTESIAN_POINT('Ctrl Pts',(-3.8445230015698,1.03632804611489,1.28051561491875));
#24348=CARTESIAN_POINT('Ctrl Pts',(-3.6480161981814,1.51081450660005,1.25968536383333));
#24349=CARTESIAN_POINT('Ctrl Pts',(-3.14836873517057,2.71726615166507,1.2067213853387));
#24350=CARTESIAN_POINT('Ctrl Pts',(-1.9909276922364,3.6512813246822,1.15375740684408));
#24351=CARTESIAN_POINT('Ctrl Pts',(-0.706151782787128,3.88482400643261,
1.10079342834945));
#24352=CARTESIAN_POINT('Ctrl Pts',(0.57862412666215,4.11836668818302,1.04782944985483));
#24353=CARTESIAN_POINT('Ctrl Pts',(1.99073490262654,3.65143687866671,0.994865471360208));
#24354=CARTESIAN_POINT('Ctrl Pts',(2.88298828242626,2.69797395029701,0.941901492865584));
#24355=CARTESIAN_POINT('Ctrl Pts',(3.77524166222597,1.74451102192732,0.88893751437096));
#24356=CARTESIAN_POINT('Ctrl Pts',(4.14763764586101,0.304514974704242,0.835973535876336));
#24357=CARTESIAN_POINT('Ctrl Pts',(3.82952478082154,-0.96194142997557,0.783009557381713));
#24358=CARTESIAN_POINT('Ctrl Pts',(3.51141191578207,-2.22839783465538,0.730045578887089));
#24359=CARTESIAN_POINT('Ctrl Pts',(2.50279020206811,-3.32131459679193,0.677081600392466));
#24360=CARTESIAN_POINT('Ctrl Pts',(1.26587965171505,-3.74001178475658,0.624117621897842));
#24361=CARTESIAN_POINT('Ctrl Pts',(0.0289691013620001,-4.15870897272123,
0.571153643403219));
#24362=CARTESIAN_POINT('Ctrl Pts',(-1.43623028563014,-3.90318658651399,
0.518189664908595));
#24363=CARTESIAN_POINT('Ctrl Pts',(-2.45813109402713,-3.09014670702069,
0.465225686413971));
#24364=CARTESIAN_POINT('Ctrl Pts',(-3.37814298820071,-2.35817120272038,
0.417542496639179));
#24365=CARTESIAN_POINT('Ctrl Pts',(-3.9388478333255,-1.17431072748125,0.369859306864387));
#24366=CARTESIAN_POINT('Ctrl Pts',(-3.94684541635378,0.00250618816942501,
0.322176117089595));
#24367=CARTESIAN_POINT('Ctrl Pts',(-3.94571229786942,0.00420644411048898,
0.1778238829104));
#24368=CARTESIAN_POINT('Ctrl Pts',(-3.93675540826681,-1.14803363217555,
0.224525832730098));
#24369=CARTESIAN_POINT('Ctrl Pts',(-3.40256651647006,-2.31072629277711,
0.271227782549796));
#24370=CARTESIAN_POINT('Ctrl Pts',(-2.51512664140724,-3.04478428612434,
0.317929732369494));
#24371=CARTESIAN_POINT('Ctrl Pts',(-1.50823248580272,-3.87765051644084,
0.370918021097743));
#24372=CARTESIAN_POINT('Ctrl Pts',(-0.0465878756876988,-4.1587226428863,
0.423906309825993));
#24373=CARTESIAN_POINT('Ctrl Pts',(1.1983574972874,-3.76190237425103,0.476894598554242));
#24374=CARTESIAN_POINT('Ctrl Pts',(2.44330287026249,-3.36508210561577,0.529882887282491));
#24375=CARTESIAN_POINT('Ctrl Pts',(3.47154900609766,-2.29036944189979,0.58287117601074));
#24376=CARTESIAN_POINT('Ctrl Pts',(3.81196419489399,-1.02929753659268,0.635859464738989));
#24377=CARTESIAN_POINT('Ctrl Pts',(4.15237938369031,0.231774368714438,0.688847753467239));
#24378=CARTESIAN_POINT('Ctrl Pts',(3.80496362544778,1.67920551561269,0.741836042195488));
#24379=CARTESIAN_POINT('Ctrl Pts',(2.92880392464218,2.64832610367255,0.794824330923737));
#24380=CARTESIAN_POINT('Ctrl Pts',(2.05264422383658,3.61744669173242,0.847812619651987));
#24381=CARTESIAN_POINT('Ctrl Pts',(0.647740580467906,4.1082567209539,0.900800908380236));
#24382=CARTESIAN_POINT('Ctrl Pts',(-0.641345987445116,3.89601342814375,
0.953789197108486));
#24383=CARTESIAN_POINT('Ctrl Pts',(-1.93043255535814,3.68377013533359,1.00677748583673));
#24384=CARTESIAN_POINT('Ctrl Pts',(-3.10370204781551,2.7684735204918,1.05976577456498));
#24385=CARTESIAN_POINT('Ctrl Pts',(-3.6230578333699,1.56976054866973,1.11275406329323));
#24386=CARTESIAN_POINT('Ctrl Pts',(-3.83564812513838,1.0790858560709,1.13444400316562));
#24387=CARTESIAN_POINT('Ctrl Pts',(-3.9386720278785,0.540923388712033,1.15613394303801));
#24388=CARTESIAN_POINT('Ctrl Pts',(-3.93636006504333,0.00190811380198534,
1.1778238829104));
#24389=CARTESIAN_POINT('Origin',(0.,0.,0.));
#24390=CARTESIAN_POINT('',(-3.93898402517327,-0.0032694952000395,2.32217611708959));
#24391=CARTESIAN_POINT('',(-3.93943713807335,-0.00339197931643889,2.1778238829104));
#24392=CARTESIAN_POINT('',(-3.942,-4.82755768223887E-16,0.));
#24393=CARTESIAN_POINT('Ctrl Pts',(-3.93898402517327,-0.0032694952000395,
2.32217611708959));
#24394=CARTESIAN_POINT('Ctrl Pts',(-3.93192709039827,0.89928000152811,2.28579640363858));
#24395=CARTESIAN_POINT('Ctrl Pts',(-3.6239186993101,1.80618191912708,2.24941669018756));
#24396=CARTESIAN_POINT('Ctrl Pts',(-3.05593295732034,2.50036976841156,2.21303697673655));
#24397=CARTESIAN_POINT('Ctrl Pts',(-2.22902197396405,3.51101407626844,2.16007299824193));
#24398=CARTESIAN_POINT('Ctrl Pts',(-0.851077281590667,4.07080133208995,
2.1071090197473));
#24399=CARTESIAN_POINT('Ctrl Pts',(0.446378324979883,3.92317725380663,2.05414504125268));
#24400=CARTESIAN_POINT('Ctrl Pts',(1.74383393155043,3.77555317552331,2.00118106275806));
#24401=CARTESIAN_POINT('Ctrl Pts',(2.96080045231815,2.92051776313515,1.94821708426343));
#24402=CARTESIAN_POINT('Ctrl Pts',(3.53953231896037,1.74993928366879,1.89525310576881));
#24403=CARTESIAN_POINT('Ctrl Pts',(4.11826418560259,0.57936080420243,1.84228912727419));
#24404=CARTESIAN_POINT('Ctrl Pts',(4.05876139811932,-0.906760742342139,
1.78932514877956));
#24405=CARTESIAN_POINT('Ctrl Pts',(3.38829497669137,-2.0273218478537,1.73636117028494));
#24406=CARTESIAN_POINT('Ctrl Pts',(2.71782855526341,-3.14788295336526,1.68339719179031));
#24407=CARTESIAN_POINT('Ctrl Pts',(1.43639849989078,-3.90288361784382,1.63043321329569));
#24408=CARTESIAN_POINT('Ctrl Pts',(0.131293493556904,-3.9463054651445,1.57746923480107));
#24409=CARTESIAN_POINT('Ctrl Pts',(-1.17381151277698,-3.98972731244518,
1.52450525630644));
#24410=CARTESIAN_POINT('Ctrl Pts',(-2.50259147007212,-3.32157034256797,
1.47154127781182));
#24411=CARTESIAN_POINT('Ctrl Pts',(-3.24605450717593,-2.24804779907291,
1.4185772993172));
#24412=CARTESIAN_POINT('Ctrl Pts',(-3.69712029286904,-1.59673190927805,
1.386443571908));
#24413=CARTESIAN_POINT('Ctrl Pts',(-3.93273330552895,-0.796202603784206,
1.3543098444988));
#24414=CARTESIAN_POINT('Ctrl Pts',(-3.93670753965503,0.00216852164164449,
1.32217611708959));
#24415=CARTESIAN_POINT('Ctrl Pts',(-3.93636006504333,0.00190811380198534,
1.1778238829104));
#24416=CARTESIAN_POINT('Ctrl Pts',(-3.93302392765509,-0.775885103331329,
1.20912223176626));
#24417=CARTESIAN_POINT('Ctrl Pts',(-3.71035557449182,-1.55545405153981,
1.24042058062212));
#24418=CARTESIAN_POINT('Ctrl Pts',(-3.28106611164764,-2.19667847798475,
1.27171892947798));
#24419=CARTESIAN_POINT('Ctrl Pts',(-2.5542765257196,-3.28227520401484,1.32470721820623));
#24420=CARTESIAN_POINT('Ctrl Pts',(-1.23525527521213,-3.97133932727269,
1.37769550693448));
#24421=CARTESIAN_POINT('Ctrl Pts',(0.0709513775297463,-3.94785759961686,
1.43068379566273));
#24422=CARTESIAN_POINT('Ctrl Pts',(1.37715803027162,-3.92437587196102,1.48367208439098));
#24423=CARTESIAN_POINT('Ctrl Pts',(2.67055008524789,-3.1883482933915,1.53666037311923));
#24424=CARTESIAN_POINT('Ctrl Pts',(3.3578681272901,-2.07735647460328,1.58964866184748));
#24425=CARTESIAN_POINT('Ctrl Pts',(4.0451861693323,-0.966364655815065,1.64263695057573));
#24426=CARTESIAN_POINT('Ctrl Pts',(4.12643019844044,0.519591403191845,1.69562523930397));
#24427=CARTESIAN_POINT('Ctrl Pts',(3.56432857554823,1.69889860460012,1.74861352803222));
#24428=CARTESIAN_POINT('Ctrl Pts',(3.00222695265603,2.87820580600839,1.80160181676047));
#24429=CARTESIAN_POINT('Ctrl Pts',(1.7967796777635,3.75086414981802,1.85459010548872));
#24430=CARTESIAN_POINT('Ctrl Pts',(0.500920035194316,3.91659925522552,1.90757839421697));
#24431=CARTESIAN_POINT('Ctrl Pts',(-0.794939607374858,4.08233436063301,
1.96056668294522));
#24432=CARTESIAN_POINT('Ctrl Pts',(-2.18121161762068,3.54114622763838,2.01355497167347));
#24433=CARTESIAN_POINT('Ctrl Pts',(-3.02202408579975,2.54126994215436,2.06654326040172));
#24434=CARTESIAN_POINT('Ctrl Pts',(-3.61062040344951,1.84132373296486,2.10363680123794));
#24435=CARTESIAN_POINT('Ctrl Pts',(-3.93191648715648,0.916599256990189,
2.14073034207417));
#24436=CARTESIAN_POINT('Ctrl Pts',(-3.93943713807335,-0.00339197931643889,
2.1778238829104));
#24437=CARTESIAN_POINT('Origin',(0.,0.,0.));
#24438=CARTESIAN_POINT('',(-3.94841909008794,-0.000476659622032916,3.3221761170896));
#24439=CARTESIAN_POINT('',(-3.94848727448062,-0.000227313299713517,3.1778238829104));
#24440=CARTESIAN_POINT('',(-3.942,-4.82755768223887E-16,0.));
#24441=CARTESIAN_POINT('Ctrl Pts',(-3.94841909008794,-0.000476659622032916,
3.3221761170896));
#24442=CARTESIAN_POINT('Ctrl Pts',(-3.94623626626659,1.27989932784314,3.27024694127299));
#24443=CARTESIAN_POINT('Ctrl Pts',(-3.2656648832367,2.56226681984272,3.21831776545638));
#24444=CARTESIAN_POINT('Ctrl Pts',(-2.20319423243154,3.27666141545475,3.16638858963978));
#24445=CARTESIAN_POINT('Ctrl Pts',(-1.11955152454134,4.00529188962783,3.11342461114515));
#24446=CARTESIAN_POINT('Ctrl Pts',(0.361362461026873,4.14308771897741,3.06046063265053));
#24447=CARTESIAN_POINT('Ctrl Pts',(1.56083317716561,3.62689600200629,3.00749665415591));
#24448=CARTESIAN_POINT('Ctrl Pts',(2.76030389330435,3.11070428503517,2.95453267566128));
#24449=CARTESIAN_POINT('Ctrl Pts',(3.67833134001362,1.94052502174336,2.90156869716666));
#24450=CARTESIAN_POINT('Ctrl Pts',(3.89417629964206,0.652660565018754,2.84860471867204));
#24451=CARTESIAN_POINT('Ctrl Pts',(4.11002125927051,-0.635203891705856,
2.79564074017741));
#24452=CARTESIAN_POINT('Ctrl Pts',(3.62368373181814,-2.04075354186327,2.74267676168279));
#24453=CARTESIAN_POINT('Ctrl Pts',(2.65805604729365,-2.91981385750971,2.68971278318817));
#24454=CARTESIAN_POINT('Ctrl Pts',(1.69242836276915,-3.79887417315615,2.63674880469354));
#24455=CARTESIAN_POINT('Ctrl Pts',(0.247510521172539,-4.15144515429161,
2.58378482619892));
#24456=CARTESIAN_POINT('Ctrl Pts',(-1.01448026111426,-3.8159408321598,2.53082084770429));
#24457=CARTESIAN_POINT('Ctrl Pts',(-2.27647104340105,-3.48043651002799,
2.47785686920967));
#24458=CARTESIAN_POINT('Ctrl Pts',(-3.35553476637803,-2.45685688462891,
2.42489289071505));
#24459=CARTESIAN_POINT('Ctrl Pts',(-3.75712799069693,-1.21431639198325,
2.37192891222042));
#24460=CARTESIAN_POINT('Ctrl Pts',(-3.88287625699264,-0.825247793982355,
2.35534464717681));
#24461=CARTESIAN_POINT('Ctrl Pts',(-3.94220103997636,-0.414710890659917,
2.3387603821332));
#24462=CARTESIAN_POINT('Ctrl Pts',(-3.93898402517327,-0.0032694952000395,
2.32217611708959));
#24463=CARTESIAN_POINT('Ctrl Pts',(-3.93943713807335,-0.00339197931643889,
2.1778238829104));
#24464=CARTESIAN_POINT('Ctrl Pts',(-3.9426597705752,-0.397612332356497,
2.19371863080242));
#24465=CARTESIAN_POINT('Ctrl Pts',(-3.8882681890457,-0.790963586497156,
2.20961337869445));
#24466=CARTESIAN_POINT('Ctrl Pts',(-3.77260571048107,-1.16538770550329,
2.22550812658647));
#24467=CARTESIAN_POINT('Ctrl Pts',(-3.387021940871,-2.41360462970351,2.27849641531472));
#24468=CARTESIAN_POINT('Ctrl Pts',(-2.32050147553854,-3.45147404013054,
2.33148470404296));
#24469=CARTESIAN_POINT('Ctrl Pts',(-1.06225033291184,-3.80293352608456,
2.38447299277121));
#24470=CARTESIAN_POINT('Ctrl Pts',(0.19600080971487,-4.15439301203859,2.43746128149946));
#24471=CARTESIAN_POINT('Ctrl Pts',(1.64598262963581,-3.81944257351961,2.49044957022771));
#24472=CARTESIAN_POINT('Ctrl Pts',(2.62259865984893,-2.95172107137353,2.54343785895596));
#24473=CARTESIAN_POINT('Ctrl Pts',(3.59921469006204,-2.08399956922746,2.59642614768421));
#24474=CARTESIAN_POINT('Ctrl Pts',(4.10246493056733,-0.683507003454308,
2.64941443641246));
#24475=CARTESIAN_POINT('Ctrl Pts',(3.90151184350976,0.607360005829592,2.70240272514071));
#24476=CARTESIAN_POINT('Ctrl Pts',(3.70055875645219,1.89822701511349,2.75539101386896));
#24477=CARTESIAN_POINT('Ctrl Pts',(2.79540234183177,3.07946846790813,2.80837930259721));
#24478=CARTESIAN_POINT('Ctrl Pts',(1.60123168012205,3.60925720078016,2.86136759132546));
#24479=CARTESIAN_POINT('Ctrl Pts',(0.407061018412325,4.1390459336522,2.91435588005371));
#24480=CARTESIAN_POINT('Ctrl Pts',(-1.0761238903867,4.01738194660163,2.96734416878196));
#24481=CARTESIAN_POINT('Ctrl Pts',(-2.16799636339283,3.30007158724765,3.0203324575102));
#24482=CARTESIAN_POINT('Ctrl Pts',(-3.24974830176843,2.58940995703755,3.07282959931027));
#24483=CARTESIAN_POINT('Ctrl Pts',(-3.94740831268547,1.29409283853931,3.12532674111033));
#24484=CARTESIAN_POINT('Ctrl Pts',(-3.94848727448062,-0.000227313299713517,
3.1778238829104));
#24485=CARTESIAN_POINT('Origin',(0.,0.,0.));
#24486=CARTESIAN_POINT('',(-3.94039517343639,0.00354505425716481,4.32217611708959));
#24487=CARTESIAN_POINT('',(-3.94011414712863,0.00351656949004968,4.1778238829104));
#24488=CARTESIAN_POINT('',(-3.942,-4.82755768223887E-16,0.));
#24489=CARTESIAN_POINT('Ctrl Pts',(-3.94039517343639,0.00354505425716481,
4.32217611708959));
#24490=CARTESIAN_POINT('Ctrl Pts',(-3.94353004938676,0.363314892612021,
4.30766145740202));
#24491=CARTESIAN_POINT('Ctrl Pts',(-3.89832073254977,0.722311104007169,
4.29314679771445));
#24492=CARTESIAN_POINT('Ctrl Pts',(-3.80162926767229,1.06685976451013,4.27863213802688));
#24493=CARTESIAN_POINT('Ctrl Pts',(-3.44880221029601,2.32411747761066,4.22566815953225));
#24494=CARTESIAN_POINT('Ctrl Pts',(-2.41048038450093,3.38900325344725,4.17270418103763));
#24495=CARTESIAN_POINT('Ctrl Pts',(-1.16253486527102,3.7734715492884,4.119740202543));
#24496=CARTESIAN_POINT('Ctrl Pts',(0.0854106539588831,4.15793984512954,
4.06677622404838));
#24497=CARTESIAN_POINT('Ctrl Pts',(1.54297986662362,3.86199066097525,4.01381224555376));
#24498=CARTESIAN_POINT('Ctrl Pts',(2.54215731665373,3.02125984033277,3.96084826705914));
#24499=CARTESIAN_POINT('Ctrl Pts',(3.54133476668386,2.18052901969028,3.90788428856451));
#24500=CARTESIAN_POINT('Ctrl Pts',(4.08212045407936,0.795016562559593,3.85492031006988));
#24501=CARTESIAN_POINT('Ctrl Pts',(3.91666803670668,-0.500286254334146,
3.80195633157526));
#24502=CARTESIAN_POINT('Ctrl Pts',(3.75121561933401,-1.79558907122787,3.74899235308063));
#24503=CARTESIAN_POINT('Ctrl Pts',(2.87952509719318,-3.00068224788464,3.69602837458601));
#24504=CARTESIAN_POINT('Ctrl Pts',(1.70109910586756,-3.56326208407903,3.64306439609139));
#24505=CARTESIAN_POINT('Ctrl Pts',(0.522673114541947,-4.12584192027342,
3.59010041759677));
#24506=CARTESIAN_POINT('Ctrl Pts',(-0.962488345968457,-4.04590841600543,
3.53713643910214));
#24507=CARTESIAN_POINT('Ctrl Pts',(-2.07372407526821,-3.36009572803379,
3.48417246060752));
#24508=CARTESIAN_POINT('Ctrl Pts',(-3.18495980456796,-2.67428304006214,
3.4312084821129));
#24509=CARTESIAN_POINT('Ctrl Pts',(-3.92226980265706,-1.38259116838684,
3.37824450361827));
#24510=CARTESIAN_POINT('Ctrl Pts',(-3.94773908659551,-0.0770126730508915,
3.32528052512365));
#24511=CARTESIAN_POINT('Ctrl Pts',(-3.94823670184224,-0.0515044661197667,
3.32424572244563));
#24512=CARTESIAN_POINT('Ctrl Pts',(-3.94846258763822,-0.025990958277152,
3.32321091976761));
#24513=CARTESIAN_POINT('Ctrl Pts',(-3.94841909008794,-0.000476659622032916,
3.3221761170896));
#24514=CARTESIAN_POINT('Ctrl Pts',(-3.94848727448062,-0.000227313299713517,
3.1778238829104));
#24515=CARTESIAN_POINT('Ctrl Pts',(-3.94849736891154,-0.0123365700109349,
3.17831502983858));
#24516=CARTESIAN_POINT('Ctrl Pts',(-3.94844649235883,-0.0244457394587464,
3.17880617676677));
#24517=CARTESIAN_POINT('Ctrl Pts',(-3.94833438892723,-0.0365543420562738,
3.17929732369495));
#24518=CARTESIAN_POINT('Ctrl Pts',(-3.9362399042423,-1.34291318034886,3.2322856124232));
#24519=CARTESIAN_POINT('Ctrl Pts',(-3.21149089765924,-2.64267412527665,
3.28527390115145));
#24520=CARTESIAN_POINT('Ctrl Pts',(-2.1065247612934,-3.33964579658387,3.3382621898797));
#24521=CARTESIAN_POINT('Ctrl Pts',(-1.00155862492758,-4.03661746789108,
3.39125047860795));
#24522=CARTESIAN_POINT('Ctrl Pts',(0.483624641221001,-4.13079986557773,
3.4442387673362));
#24523=CARTESIAN_POINT('Ctrl Pts',(1.66778169459976,-3.57899215935798,3.49722705606445));
#24524=CARTESIAN_POINT('Ctrl Pts',(2.85193874797851,-3.02718445313824,3.5502153447927));
#24525=CARTESIAN_POINT('Ctrl Pts',(3.73506958858744,-1.82938664301209,3.60320363352094));
#24526=CARTESIAN_POINT('Ctrl Pts',(3.91208817286041,-0.535020350876169,
3.65619192224919));
#24527=CARTESIAN_POINT('Ctrl Pts',(4.08910675713339,0.759345941259773,3.70918021097745));
#24528=CARTESIAN_POINT('Ctrl Pts',(3.56001308507038,2.1502807154055,3.7621684997057));
#24529=CARTESIAN_POINT('Ctrl Pts',(2.56749878545275,2.99977176280624,3.81515678843395));
#24530=CARTESIAN_POINT('Ctrl Pts',(1.57498448583515,3.84926281020697,3.86814507716219));
#24531=CARTESIAN_POINT('Ctrl Pts',(0.11904955866294,4.15731013086274,3.92113336589044));
#24532=CARTESIAN_POINT('Ctrl Pts',(-1.13247866152849,3.78261453618225,3.97412165461869));
#24533=CARTESIAN_POINT('Ctrl Pts',(-2.38400688171994,3.40791894150175,4.02710994334694));
#24534=CARTESIAN_POINT('Ctrl Pts',(-3.43112839493061,2.35048043148498,4.08009823207519));
#24535=CARTESIAN_POINT('Ctrl Pts',(-3.79353576624568,1.09533877709901,4.13308652080344));
#24536=CARTESIAN_POINT('Ctrl Pts',(-3.89552779876129,0.742105210239426,
4.14799897483909));
#24537=CARTESIAN_POINT('Ctrl Pts',(-3.94328881467064,0.373213076031263,
4.16291142887475));
#24538=CARTESIAN_POINT('Ctrl Pts',(-3.94011414712863,0.00351656949004968,
4.1778238829104));
#24539=CARTESIAN_POINT('Origin',(0.,0.,0.));
#24540=CARTESIAN_POINT('',(-3.93600110646763,-0.0014281919745418,5.32217611708959));
#24541=CARTESIAN_POINT('',(-3.93605515638862,-0.00152114337219748,5.1778238829104));
#24542=CARTESIAN_POINT('',(-3.942,-4.82755768223887E-16,0.));
#24543=CARTESIAN_POINT('Ctrl Pts',(-3.93600110646763,-0.0014281919745418,
5.32217611708959));
#24544=CARTESIAN_POINT('Ctrl Pts',(-3.93357236454694,0.74585693902175,5.29211199503643));
#24545=CARTESIAN_POINT('Ctrl Pts',(-3.72918845072319,1.49437332783476,5.26204787298327));
#24546=CARTESIAN_POINT('Ctrl Pts',(-3.33126090733014,2.11973479786067,5.2319837509301));
#24547=CARTESIAN_POINT('Ctrl Pts',(-2.63023175991589,3.22143440482896,5.17901977243548));
#24548=CARTESIAN_POINT('Ctrl Pts',(-1.32852280829314,3.94091180862283,5.12605579394085));
#24549=CARTESIAN_POINT('Ctrl Pts',(-0.0227175227337642,3.94842484544612,
5.07309181544622));
#24550=CARTESIAN_POINT('Ctrl Pts',(1.28308776282561,3.95593788226941,5.0201278369516));
#24551=CARTESIAN_POINT('Ctrl Pts',(2.59298938232161,3.25148655212212,4.96716385845699));
#24552=CARTESIAN_POINT('Ctrl Pts',(3.30664910123763,2.15792645084216,4.91419987996236));
#24553=CARTESIAN_POINT('Ctrl Pts',(4.02030882015365,1.06436634956219,4.86123590146774));
#24554=CARTESIAN_POINT('Ctrl Pts',(4.13772663848969,-0.418302522850447,
4.80827192297311));
#24555=CARTESIAN_POINT('Ctrl Pts',(3.60508904482309,-1.61056133843436,4.75530794447848));
#24556=CARTESIAN_POINT('Ctrl Pts',(3.07245145115649,-2.80282015401828,4.70234396598386));
#24557=CARTESIAN_POINT('Ctrl Pts',(1.88975844548724,-3.70466891277347,4.64937998748924));
#24558=CARTESIAN_POINT('Ctrl Pts',(0.599047552189011,-3.90278322178284,
4.59641600899462));
#24559=CARTESIAN_POINT('Ctrl Pts',(-0.691663341109217,-4.10089753079221,
4.54345203049999));
#24560=CARTESIAN_POINT('Ctrl Pts',(-2.09039212203642,-3.59527739005576,
4.49048805200536));
#24561=CARTESIAN_POINT('Ctrl Pts',(-2.95609036802126,-2.61765249450529,
4.43752407351074));
#24562=CARTESIAN_POINT('Ctrl Pts',(-3.58454594852404,-1.90794351207784,
4.39907475470369));
#24563=CARTESIAN_POINT('Ctrl Pts',(-3.93209089021995,-0.949484883048943,
4.36062543589664));
#24564=CARTESIAN_POINT('Ctrl Pts',(-3.94039517343639,0.00354505425716481,
4.32217611708959));
#24565=CARTESIAN_POINT('Ctrl Pts',(-3.94011414712863,0.00351656949004968,
4.1778238829104));
#24566=CARTESIAN_POINT('Ctrl Pts',(-3.93200829706235,-0.94042619377602,
4.215899717603));
#24567=CARTESIAN_POINT('Ctrl Pts',(-3.59183770381144,-1.88961289751958,
4.25397555229559));
#24568=CARTESIAN_POINT('Ctrl Pts',(-2.97445535308007,-2.59678570511794,
4.29205138698818));
#24569=CARTESIAN_POINT('Ctrl Pts',(-2.1152743391799,-3.5809237341938,4.34503967571643));
#24570=CARTESIAN_POINT('Ctrl Pts',(-0.719219081960083,-4.09635499359035,
4.39802796444469));
#24571=CARTESIAN_POINT('Ctrl Pts',(0.573349476162703,-3.90665471020838,
4.45101625317294));
#24572=CARTESIAN_POINT('Ctrl Pts',(1.86591803428548,-3.7169544268264,4.50400454190118));
#24573=CARTESIAN_POINT('Ctrl Pts',(3.05499989331122,-2.82212260066591,4.55699283062943));
#24574=CARTESIAN_POINT('Ctrl Pts',(3.59517138458731,-1.63261243464328,4.60998111935768));
#24575=CARTESIAN_POINT('Ctrl Pts',(4.13534287586339,-0.443102268620652,
4.66296940808593));
#24576=CARTESIAN_POINT('Ctrl Pts',(4.02660399938981,1.04108623726411,4.71595769681418));
#24577=CARTESIAN_POINT('Ctrl Pts',(3.31883252977577,2.13916602570979,4.76894598554243));
#24578=CARTESIAN_POINT('Ctrl Pts',(2.61106106016173,3.23724581415546,4.82193427427068));
#24579=CARTESIAN_POINT('Ctrl Pts',(1.3042569974072,3.94921688516205,4.87492256299893));
#24580=CARTESIAN_POINT('Ctrl Pts',(-0.00215762490102876,3.94850300633285,
4.92791085172718));
#24581=CARTESIAN_POINT('Ctrl Pts',(-1.30857224720925,3.94778912750366,4.98089914045543));
#24582=CARTESIAN_POINT('Ctrl Pts',(-2.61459742907118,3.23439029883869,5.03388742918367));
#24583=CARTESIAN_POINT('Ctrl Pts',(-3.32116840418697,2.13553765533301,5.08687571791192));
#24584=CARTESIAN_POINT('Ctrl Pts',(-3.72541706095167,1.50685388432656,5.11719177291141));
#24585=CARTESIAN_POINT('Ctrl Pts',(-3.93344647436031,0.751999581783958,
5.14750782791091));
#24586=CARTESIAN_POINT('Ctrl Pts',(-3.93605515638862,-0.00152114337219748,
5.1778238829104));
#24587=CARTESIAN_POINT('Origin',(0.,0.,0.));
#24588=CARTESIAN_POINT('',(-3.94563673384516,-0.00288256983268176,6.3221761170896));
#24589=CARTESIAN_POINT('',(-3.94570073178844,-0.00286656758253237,6.1778238829104));
#24590=CARTESIAN_POINT('',(-3.942,-4.82755768223887E-16,0.));
#24591=CARTESIAN_POINT('Ctrl Pts',(-3.94563673384516,-0.00288256983268176,
6.3221761170896));
#24592=CARTESIAN_POINT('Ctrl Pts',(-3.93638288024859,1.12386902299333,6.27656253267084));
#24593=CARTESIAN_POINT('Ctrl Pts',(-3.42887602753453,2.25790074792199,6.23094894825208));
#24594=CARTESIAN_POINT('Ctrl Pts',(-2.57675389815072,2.99180784716095,6.18533536383333));
#24595=CARTESIAN_POINT('Ctrl Pts',(-1.58731667872186,3.84398029351578,6.1323713853387));
#24596=CARTESIAN_POINT('Ctrl Pts',(-0.133249377743896,4.15668177021255,
6.07940740684408));
#24597=CARTESIAN_POINT('Ctrl Pts',(1.1190375023862,3.78659872632712,6.02644342834946));
#24598=CARTESIAN_POINT('Ctrl Pts',(2.37132438251632,3.41651568244167,5.97347944985483));
#24599=CARTESIAN_POINT('Ctrl Pts',(3.42183084179856,2.363648117974,5.92051547136021));
#24600=CARTESIAN_POINT('Ctrl Pts',(3.78910149173018,1.11053353453949,5.86755149286558));
#24601=CARTESIAN_POINT('Ctrl Pts',(4.15637214166179,-0.142581048895014,
5.81458751437096));
#24602=CARTESIAN_POINT('Ctrl Pts',(3.84040698224279,-1.59594265129635,5.76162353587634));
#24603=CARTESIAN_POINT('Ctrl Pts',(2.98601533590735,-2.58346419748652,5.70865955738171));
#24604=CARTESIAN_POINT('Ctrl Pts',(2.1316236895719,-3.57098574367668,5.65569557888709));
#24605=CARTESIAN_POINT('Ctrl Pts',(0.738805556320001,-4.09266723365567,
5.60273160039247));
#24606=CARTESIAN_POINT('Ctrl Pts',(-0.554099537676607,-3.9094179296049,
5.54976762189784));
#24607=CARTESIAN_POINT('Ctrl Pts',(-1.84700463167322,-3.72616862555414,
5.49680364340322));
#24608=CARTESIAN_POINT('Ctrl Pts',(-3.03999668641454,-2.83798852747363,
5.44383966490859));
#24609=CARTESIAN_POINT('Ctrl Pts',(-3.58631804218233,-1.65193757336201,
5.39087568641397));
#24610=CARTESIAN_POINT('Ctrl Pts',(-3.8225291610139,-1.1391287294386,5.36797582997251));
#24611=CARTESIAN_POINT('Ctrl Pts',(-3.93785108037402,-0.570635640986049,
5.34507597353105));
#24612=CARTESIAN_POINT('Ctrl Pts',(-3.93600110646763,-0.0014281919745418,
5.32217611708959));
#24613=CARTESIAN_POINT('Ctrl Pts',(-3.93605515638862,-0.00152114337219748,
5.1778238829104));
#24614=CARTESIAN_POINT('Ctrl Pts',(-3.93800609125369,-0.565050863861574,
5.20049611663916));
#24615=CARTESIAN_POINT('Ctrl Pts',(-3.82506562686086,-1.12783471721807,
5.22316835036792));
#24616=CARTESIAN_POINT('Ctrl Pts',(-3.59338498454405,-1.63654055836231,
5.24584058409668));
#24617=CARTESIAN_POINT('Ctrl Pts',(-3.05191382141567,-2.82545967020557,
5.29882887282492));
#24618=CARTESIAN_POINT('Ctrl Pts',(-1.86185472678928,-3.71899143554569,
5.35181716155317));
#24619=CARTESIAN_POINT('Ctrl Pts',(-0.569079620514193,-3.90727898054932,
5.40480545028142));
#24620=CARTESIAN_POINT('Ctrl Pts',(0.723695485760891,-4.09556652555295,
5.45779373900967));
#24621=CARTESIAN_POINT('Ctrl Pts',(2.11918660368467,-3.57860985022007,5.51078202773792));
#24622=CARTESIAN_POINT('Ctrl Pts',(2.97729155756073,-2.59353342519368,5.56377031646617));
#24623=CARTESIAN_POINT('Ctrl Pts',(3.83539651143679,-1.60845700016728,5.61675860519442));
#24624=CARTESIAN_POINT('Ctrl Pts',(4.15611530126515,-0.155260825447382,
5.66974689392266));
#24625=CARTESIAN_POINT('Ctrl Pts',(3.79233642449449,1.09948401069401,5.72273518265091));
#24626=CARTESIAN_POINT('Ctrl Pts',(3.42855754772383,2.35422884683541,5.77572347137916));
#24627=CARTESIAN_POINT('Ctrl Pts',(2.38028100435414,3.41052234439828,5.82871176010741));
#24628=CARTESIAN_POINT('Ctrl Pts',(1.12834403334923,3.78384994268096,5.88170004883566));
#24629=CARTESIAN_POINT('Ctrl Pts',(-0.12359293765566,4.15717754096363,5.93468833756392));
#24630=CARTESIAN_POINT('Ctrl Pts',(-1.57919033629578,3.8475392399661,5.98767662629216));
#24631=CARTESIAN_POINT('Ctrl Pts',(-2.57077564940419,2.99696399824068,6.04066491502041));
#24632=CARTESIAN_POINT('Ctrl Pts',(-3.4263409160258,2.26306584157345,6.08638457098374));
#24633=CARTESIAN_POINT('Ctrl Pts',(-3.93646396625886,1.126457364296,6.13210422694707));
#24634=CARTESIAN_POINT('Ctrl Pts',(-3.94570073178844,-0.00286656758253237,
6.1778238829104));
#24635=CARTESIAN_POINT('Origin',(0.,0.,0.));
#24636=CARTESIAN_POINT('',(-3.94505905468816,0.00309284708018512,7.32217611708959));
#24637=CARTESIAN_POINT('',(-3.94511280640764,0.00308469250234145,7.1778238829104));
#24638=CARTESIAN_POINT('',(-3.942,-4.82755768223887E-16,0.));
#24639=CARTESIAN_POINT('Ctrl Pts',(-3.94505905468816,0.00309284708018512,
7.32217611708959));
#24640=CARTESIAN_POINT('Ctrl Pts',(-3.9468047458557,0.205704294057958,7.31397704879987));
#24641=CARTESIAN_POINT('Ctrl Pts',(-3.93254600075262,0.408069386251045,
7.30577798051015));
#24642=CARTESIAN_POINT('Ctrl Pts',(-3.90142848745745,0.607808031556218,
7.29757891222042));
#24643=CARTESIAN_POINT('Ctrl Pts',(-3.7004169521544,1.89807089322147,7.2446149337258));
#24644=CARTESIAN_POINT('Ctrl Pts',(-2.79591524746178,3.0787362122301,7.19165095523118));
#24645=CARTESIAN_POINT('Ctrl Pts',(-1.60246363230549,3.60869576898733,7.13868697673655));
#24646=CARTESIAN_POINT('Ctrl Pts',(-0.409012017149199,4.13865532574456,
7.08572299824193));
#24647=CARTESIAN_POINT('Ctrl Pts',(1.07338950847076,4.01790912025038,7.03275901974731));
#24648=CARTESIAN_POINT('Ctrl Pts',(2.16534464372431,3.30179608998848,6.97979504125268));
#24649=CARTESIAN_POINT('Ctrl Pts',(3.25729977897786,2.58568305972658,6.92683106275806));
#24650=CARTESIAN_POINT('Ctrl Pts',(3.95880852386501,1.27420320469696,6.87386708426343));
#24651=CARTESIAN_POINT('Ctrl Pts',(3.94836389256626,-0.0315819228008631,
6.82090310576881));
#24652=CARTESIAN_POINT('Ctrl Pts',(3.93791926126751,-1.33736705029871,6.76793912727419));
#24653=CARTESIAN_POINT('Ctrl Pts',(3.21552125378285,-2.63745745026476,6.71497514877956));
#24654=CARTESIAN_POINT('Ctrl Pts',(2.11225056959203,-3.33601144740646,6.66201117028494));
#24655=CARTESIAN_POINT('Ctrl Pts',(1.00897988540122,-4.03456544454814,6.60904719179032));
#24656=CARTESIAN_POINT('Ctrl Pts',(-0.475163475495736,-4.1315830388655,
6.55608321329569));
#24657=CARTESIAN_POINT('Ctrl Pts',(-1.65998491543528,-3.58260030236365,
6.50311923480107));
#24658=CARTESIAN_POINT('Ctrl Pts',(-2.84480635537483,-3.0336175658618,6.45015525630644));
#24659=CARTESIAN_POINT('Ctrl Pts',(-3.73030587435696,-1.83863449854073,
6.39719127781182));
#24660=CARTESIAN_POINT('Ctrl Pts',(-3.91065206490815,-0.545321256873756,
6.3442272993172));
#24661=CARTESIAN_POINT('Ctrl Pts',(-3.93568069017971,-0.365833947574368,
6.33687690524133));
#24662=CARTESIAN_POINT('Ctrl Pts',(-3.94712794466584,-0.1844527827072,6.32952651116546));
#24663=CARTESIAN_POINT('Ctrl Pts',(-3.94563673384516,-0.00288256983268176,
6.3221761170896));
#24664=CARTESIAN_POINT('Ctrl Pts',(-3.94570073178844,-0.00286656758253237,
6.1778238829104));
#24665=CARTESIAN_POINT('Ctrl Pts',(-3.94716921739174,-0.182409496340425,
6.18509251567532));
#24666=CARTESIAN_POINT('Ctrl Pts',(-3.93597755777244,-0.361768304659314,
6.19236114844024));
#24667=CARTESIAN_POINT('Ctrl Pts',(-3.91150112201508,-0.539295483751872,
6.19962978120516));
#24668=CARTESIAN_POINT('Ctrl Pts',(-3.73306805394085,-1.83346754156567,
6.25261806993341));
#24669=CARTESIAN_POINT('Ctrl Pts',(-2.84862869021566,-3.03029947473994,
6.30560635866166));
#24670=CARTESIAN_POINT('Ctrl Pts',(-1.66386928259682,-3.58081270897423,
6.35859464738991));
#24671=CARTESIAN_POINT('Ctrl Pts',(-0.479109874977974,-4.13132594320853,
6.41158293611816));
#24672=CARTESIAN_POINT('Ctrl Pts',(1.00596957653452,-4.03552047850286,6.4645712248464));
#24673=CARTESIAN_POINT('Ctrl Pts',(2.11017334393921,-3.33734162243677,6.51755951357465));
#24674=CARTESIAN_POINT('Ctrl Pts',(3.21437711134392,-2.63916276637067,6.5705478023029));
#24675=CARTESIAN_POINT('Ctrl Pts',(3.9377051946408,-1.33861051894414,6.62353609103116));
#24676=CARTESIAN_POINT('Ctrl Pts',(3.94837197806129,-0.0322392490748367,
6.6765243797594));
#24677=CARTESIAN_POINT('Ctrl Pts',(3.95903876148178,1.27413202079445,6.72951266848765));
#24678=CARTESIAN_POINT('Ctrl Pts',(3.25704424502592,2.58632231310649,6.7825009572159));
#24679=CARTESIAN_POINT('Ctrl Pts',(2.16438848411372,3.30243896781703,6.83548924594415));
#24680=CARTESIAN_POINT('Ctrl Pts',(1.07173272320153,4.01855562252758,6.8884775346724));
#24681=CARTESIAN_POINT('Ctrl Pts',(-0.411584282167038,4.13859863963661,
6.94146582340065));
#24682=CARTESIAN_POINT('Ctrl Pts',(-1.60517522591216,3.60750511301625,6.9944541121289));
#24683=CARTESIAN_POINT('Ctrl Pts',(-2.7987661696573,3.07641158639588,7.04744240085715));
#24684=CARTESIAN_POINT('Ctrl Pts',(-3.70263105177901,1.89418151604613,7.1004306895854));
#24685=CARTESIAN_POINT('Ctrl Pts',(-3.9021732688668,0.603095702241273,7.15341897831364));
#24686=CARTESIAN_POINT('Ctrl Pts',(-3.9328077662116,0.404883186052253,7.16155394651256));
#24687=CARTESIAN_POINT('Ctrl Pts',(-3.94684167082104,0.204104985193814,
7.16968891471148));
#24688=CARTESIAN_POINT('Ctrl Pts',(-3.94511280640764,0.00308469250234145,
7.1778238829104));
#24689=CARTESIAN_POINT('Origin',(0.,0.,0.));
#24690=CARTESIAN_POINT('',(-3.93579878224384,0.00110209819909501,8.3221761170896));
#24691=CARTESIAN_POINT('',(-3.93583379497513,0.00119086740244391,8.17782388291041));
#24692=CARTESIAN_POINT('',(-3.942,-4.82755768223887E-16,0.));
#24693=CARTESIAN_POINT('Ctrl Pts',(-3.93579878224384,0.00110209819909501,
8.3221761170896));
#24694=CARTESIAN_POINT('Ctrl Pts',(-3.93727495532409,0.591480280077664,
8.29842758643428));
#24695=CARTESIAN_POINT('Ctrl Pts',(-3.81287497830763,1.18126751761344,8.27467905577897));
#24696=CARTESIAN_POINT('Ctrl Pts',(-3.55943403140727,1.70909456204991,8.25093052512365));
#24697=CARTESIAN_POINT('Ctrl Pts',(-2.9942099737124,2.88625455717395,8.19796654662903));
#24698=CARTESIAN_POINT('Ctrl Pts',(-1.78716283564177,3.75523737390689,8.1450025681344));
#24699=CARTESIAN_POINT('Ctrl Pts',(-0.491491832360601,3.91778133957111,
8.09203858963978));
#24700=CARTESIAN_POINT('Ctrl Pts',(0.804179170920576,4.08032530523533,8.03907461114515));
#24701=CARTESIAN_POINT('Ctrl Pts',(2.18847403941229,3.53643041983081,7.98611063265053));
#24702=CARTESIAN_POINT('Ctrl Pts',(3.02695952634759,2.53536799534552,7.93314665415591));
#24703=CARTESIAN_POINT('Ctrl Pts',(3.86544501328289,1.53430557086022,7.88018267566129));
#24704=CARTESIAN_POINT('Ctrl Pts',(4.15812111866178,0.0760756072941503,
7.82721869716666));
#24705=CARTESIAN_POINT('Ctrl Pts',(3.77085207703933,-1.17100361188895,7.77425471867203));
#24706=CARTESIAN_POINT('Ctrl Pts',(3.38358303541687,-2.41808283107204,7.72129074017741));
#24707=CARTESIAN_POINT('Ctrl Pts',(2.31636884679309,-3.45401130587216,7.66832676168279));
#24708=CARTESIAN_POINT('Ctrl Pts',(1.05832218368842,-3.8040148529523,7.61536278318817));
#24709=CARTESIAN_POINT('Ctrl Pts',(-0.199724479416271,-4.15401840003245,
7.56239880469355));
#24710=CARTESIAN_POINT('Ctrl Pts',(-1.64860361700185,-3.81809701939261,
7.50943482619892));
#24711=CARTESIAN_POINT('Ctrl Pts',(-2.62428250283791,-2.95020612691174,
7.45647084770429));
#24712=CARTESIAN_POINT('Ctrl Pts',(-3.44892179457277,-2.21666874973946,
7.41170593749939));
#24713=CARTESIAN_POINT('Ctrl Pts',(-3.93552800730583,-1.10311616471836,
7.36694102729449));
#24714=CARTESIAN_POINT('Ctrl Pts',(-3.94505905468816,0.00309284708018512,
7.32217611708959));
#24715=CARTESIAN_POINT('Ctrl Pts',(-3.94511280640764,0.00308469250234145,
7.1778238829104));
#24716=CARTESIAN_POINT('Ctrl Pts',(-3.93558046309789,-1.10526968584544,
7.22267720343973));
#24717=CARTESIAN_POINT('Ctrl Pts',(-3.44685564182305,-2.22098372195378,
7.26753052396906));
#24718=CARTESIAN_POINT('Ctrl Pts',(-2.61937124393104,-2.95458540793588,
7.31238384449839));
#24719=CARTESIAN_POINT('Ctrl Pts',(-1.64180744985364,-3.82123914704826,
7.36537213322664));
#24720=CARTESIAN_POINT('Ctrl Pts',(-0.191460309644946,-4.15460506801304,
7.41836042195489));
#24721=CARTESIAN_POINT('Ctrl Pts',(1.06640592095225,-3.80177051623037,7.47134871068314));
#24722=CARTESIAN_POINT('Ctrl Pts',(2.32427215154943,-3.44893596444769,7.52433699941139));
#24723=CARTESIAN_POINT('Ctrl Pts',(3.38965747253514,-2.40990093991759,7.57732528813964));
#24724=CARTESIAN_POINT('Ctrl Pts',(3.77387696635039,-1.16126366048821,7.63031357686789));
#24725=CARTESIAN_POINT('Ctrl Pts',(4.15809646016565,0.0873736189411645,
7.68330186559614));
#24726=CARTESIAN_POINT('Ctrl Pts',(3.86115012681045,1.5456131532698,7.73629015432439));
#24727=CARTESIAN_POINT('Ctrl Pts',(3.01924520659187,2.54457049986684,7.78927844305264));
#24728=CARTESIAN_POINT('Ctrl Pts',(2.17734028637328,3.54352784646387,7.84226673178089));
#24729=CARTESIAN_POINT('Ctrl Pts',(0.79047677929132,4.08320300532929,7.89525502050913));
#24730=CARTESIAN_POINT('Ctrl Pts',(-0.505200564699283,3.91605069371529,
7.94824330923738));
#24731=CARTESIAN_POINT('Ctrl Pts',(-1.80087790868988,3.74889838210129,8.00123159796563));
#24732=CARTESIAN_POINT('Ctrl Pts',(-3.00536908958914,2.87491860000785,8.05421988669388));
#24733=CARTESIAN_POINT('Ctrl Pts',(-3.56618228885602,1.69499986105314,8.10720817542213));
#24734=CARTESIAN_POINT('Ctrl Pts',(-3.81530790878367,1.17085387502675,8.13074674458489));
#24735=CARTESIAN_POINT('Ctrl Pts',(-3.93741444221381,0.586335951582262,
8.15428531374765));
#24736=CARTESIAN_POINT('Ctrl Pts',(-3.93583379497513,0.00119086740244391,
8.17782388291041));
#24737=CARTESIAN_POINT('Origin',(0.,0.,0.));
#24738=CARTESIAN_POINT('',(-3.94101045068862,-0.00360005201630542,9.3221761170896));
#24739=CARTESIAN_POINT('',(-3.94073510056759,-0.00358878591061127,9.1778238829104));
#24740=CARTESIAN_POINT('',(-3.942,-4.82755768223887E-16,0.));
#24741=CARTESIAN_POINT('Ctrl Pts',(-3.94101045068862,-0.00360005201630542,
9.3221761170896));
#24742=CARTESIAN_POINT('Ctrl Pts',(-3.93228175108165,0.970079126201241,
9.28287812406869));
#24743=CARTESIAN_POINT('Ctrl Pts',(-3.56768740150403,1.94959821666609,9.24358013104778));
#24744=CARTESIAN_POINT('Ctrl Pts',(-2.91383898553304,2.66460451331084,9.20428213802687));
#24745=CARTESIAN_POINT('Ctrl Pts',(-2.03261297931419,3.6282562219074,9.15131815953225));
#24746=CARTESIAN_POINT('Ctrl Pts',(-0.625975040492547,4.11143697314778,
9.09835418103763));
#24747=CARTESIAN_POINT('Ctrl Pts',(0.661401578964616,3.89270122117173,9.04539020254301));
#24748=CARTESIAN_POINT('Ctrl Pts',(1.9487781984218,3.67396546919568,8.99242622404838));
#24749=CARTESIAN_POINT('Ctrl Pts',(3.11689349851449,2.75331321400316,8.93946224555376));
#24750=CARTESIAN_POINT('Ctrl Pts',(3.63039103221387,1.55268663908397,8.88649826705913));
#24751=CARTESIAN_POINT('Ctrl Pts',(4.14388856591324,0.352060064164805,8.83353428856451));
#24752=CARTESIAN_POINT('Ctrl Pts',(4.00276833321932,-1.12854083048104,8.78057031006989));
#24753=CARTESIAN_POINT('Ctrl Pts',(3.2717068488331,-2.21054498738825,8.72760633157527));
#24754=CARTESIAN_POINT('Ctrl Pts',(2.54064536444688,-3.29254914429547,8.67464235308064));
#24755=CARTESIAN_POINT('Ctrl Pts',(1.21964262836836,-3.97595656346406,8.62167837458601));
#24756=CARTESIAN_POINT('Ctrl Pts',(-0.0858753956759256,-3.94755623929365,
8.56871439609139));
#24757=CARTESIAN_POINT('Ctrl Pts',(-1.39139341972021,-3.91915591512325,
8.51575041759677));
#24758=CARTESIAN_POINT('Ctrl Pts',(-2.68142673173026,-3.17894784761384,
8.46278643910214));
#24759=CARTESIAN_POINT('Ctrl Pts',(-3.36474289907574,-2.06617522710156,
8.40982246060752));
#24760=CARTESIAN_POINT('Ctrl Pts',(-3.74166677096472,-1.45235898112435,
8.38060701276821));
#24761=CARTESIAN_POINT('Ctrl Pts',(-3.93398279378317,-0.725181276064265,
8.35139156492891));
#24762=CARTESIAN_POINT('Ctrl Pts',(-3.93579878224384,0.00110209819909501,
8.3221761170896));
#24763=CARTESIAN_POINT('Ctrl Pts',(-3.93583379497513,0.00119086740244391,
8.17782388291041));
#24764=CARTESIAN_POINT('Ctrl Pts',(-3.93385620587065,-0.730899452746949,
8.2072736024759));
#24765=CARTESIAN_POINT('Ctrl Pts',(-3.73826901230947,-1.46397147804348,
8.23672332204139));
#24766=CARTESIAN_POINT('Ctrl Pts',(-3.35559744737338,-2.0810205230852,8.26617304160688));
#24767=CARTESIAN_POINT('Ctrl Pts',(-2.66706418898931,-3.19126447245286,
8.31916133033513));
#24768=CARTESIAN_POINT('Ctrl Pts',(-1.37286245458661,-3.92589467537216,
8.37214961906338));
#24769=CARTESIAN_POINT('Ctrl Pts',(-0.0666336764464662,-3.94794131155515,
8.42513790779163));
#24770=CARTESIAN_POINT('Ctrl Pts',(1.23959510169366,-3.96998794773813,8.47812619651988));
#24771=CARTESIAN_POINT('Ctrl Pts',(2.55785092357125,-3.27945101718484,8.53111448524812));
#24772=CARTESIAN_POINT('Ctrl Pts',(3.28345891245731,-2.19307505948273,8.58410277397638));
#24773=CARTESIAN_POINT('Ctrl Pts',(4.00906690134337,-1.10669910178063,8.63709106270462));
#24774=CARTESIAN_POINT('Ctrl Pts',(4.14202705723791,0.375515883070263,8.69007935143287));
#24775=CARTESIAN_POINT('Ctrl Pts',(3.62135147131388,1.57368807822049,8.74306764016112));
#24776=CARTESIAN_POINT('Ctrl Pts',(3.10067588538986,2.77186027337072,8.79605592888937));
#24777=CARTESIAN_POINT('Ctrl Pts',(1.92636455764724,3.68598967882027,8.84904421761762));
#24778=CARTESIAN_POINT('Ctrl Pts',(0.637066015602396,3.89677142492153,8.90203250634587));
#24779=CARTESIAN_POINT('Ctrl Pts',(-0.652232526442438,4.1075531710228,8.95502079507412));
#24780=CARTESIAN_POINT('Ctrl Pts',(-2.05651828278951,3.61498725777581,9.00800908380237));
#24781=CARTESIAN_POINT('Ctrl Pts',(-2.93165503760022,2.64501028104501,9.06099737253062));
#24782=CARTESIAN_POINT('Ctrl Pts',(-3.57481082178969,1.93215449058061,9.09993954265721));
#24783=CARTESIAN_POINT('Ctrl Pts',(-3.93216906200874,0.9614452240408,9.13888171278381));
#24784=CARTESIAN_POINT('Ctrl Pts',(-3.94073510056759,-0.00358878591061127,
9.1778238829104));
#24785=CARTESIAN_POINT('Origin',(0.,0.,0.));
#24786=CARTESIAN_POINT('',(-3.94826120782986,0.000860587304522282,10.3221761170896));
#24787=CARTESIAN_POINT('',(-3.94838239458768,0.000624922565347272,10.1778238829104));
#24788=CARTESIAN_POINT('',(-3.942,-4.82755768223887E-16,0.));
#24789=CARTESIAN_POINT('Ctrl Pts',(-3.94826120782986,0.000860587304522282,
10.3221761170896));
#24790=CARTESIAN_POINT('Ctrl Pts',(-3.94839882197096,0.0473049479418113,
10.3202926401977));
#24791=CARTESIAN_POINT('Ctrl Pts',(-3.94765033544244,0.0937447675908473,
10.3184091633059));
#24792=CARTESIAN_POINT('Ctrl Pts',(-3.94600203836796,0.140152628104641,
10.316525686414));
#24793=CARTESIAN_POINT('Ctrl Pts',(-3.89965139229318,1.4451566538172,10.2635617079194));
#24794=CARTESIAN_POINT('Ctrl Pts',(-3.14177325024928,2.72488891140618,10.2105977294247));
#24795=CARTESIAN_POINT('Ctrl Pts',(-2.0197091369755,3.39283802265691,10.1576337509301));
#24796=CARTESIAN_POINT('Ctrl Pts',(-0.897645023701731,4.06078713390763,
10.1046697724355));
#24797=CARTESIAN_POINT('Ctrl Pts',(0.588605060801912,4.11695309882012,10.0517057939409));
#24798=CARTESIAN_POINT('Ctrl Pts',(1.75788099084149,3.53559461307527,9.99874181544624));
#24799=CARTESIAN_POINT('Ctrl Pts',(2.92715692088108,2.95423612733042,9.94577783695161));
#24800=CARTESIAN_POINT('Ctrl Pts',(3.7794586964566,1.73535319092823,9.89281385845698));
#24801=CARTESIAN_POINT('Ctrl Pts',(3.92416969750304,0.437569458677891,9.83984987996236));
#24802=CARTESIAN_POINT('Ctrl Pts',(4.06888069854947,-0.860214273572448,
9.78688590146773));
#24803=CARTESIAN_POINT('Ctrl Pts',(3.50600092506682,-2.23689880167093,9.73392192297312));
#24804=CARTESIAN_POINT('Ctrl Pts',(2.49350261285418,-3.06153875782394,9.68095794447849));
#24805=CARTESIAN_POINT('Ctrl Pts',(1.48100430064151,-3.88617871397697,9.62799396598387));
#24806=CARTESIAN_POINT('Ctrl Pts',(0.0188874496988303,-4.15877409818449,
9.57502998748924));
#24807=CARTESIAN_POINT('Ctrl Pts',(-1.22274826539589,-3.75439229775474,
9.52206600899461));
#24808=CARTESIAN_POINT('Ctrl Pts',(-2.46438398049055,-3.350010497325,9.46910203049999));
#24809=CARTESIAN_POINT('Ctrl Pts',(-3.48553855973727,-2.26865151225807,
9.41613805200537));
#24810=CARTESIAN_POINT('Ctrl Pts',(-3.81820881255261,-1.00591068674825,
9.36317407351075));
#24811=CARTESIAN_POINT('Ctrl Pts',(-3.90404577140141,-0.680093059958056,
9.34950808803704));
#24812=CARTESIAN_POINT('Ctrl Pts',(-3.94404588005443,-0.342199672065631,
9.33584210256332));
#24813=CARTESIAN_POINT('Ctrl Pts',(-3.94101045068862,-0.00360005201630542,
9.3221761170896));
#24814=CARTESIAN_POINT('Ctrl Pts',(-3.94073510056759,-0.00358878591061127,
9.1778238829104));
#24815=CARTESIAN_POINT('Ctrl Pts',(-3.94382479981015,-0.351668569711599,
9.19187000151206));
#24816=CARTESIAN_POINT('Ctrl Pts',(-3.90153714912137,-0.6990100110183,9.20591612011371));
#24817=CARTESIAN_POINT('Ctrl Pts',(-3.81091609517323,-1.03324690266663,
9.21996223871536));
#24818=CARTESIAN_POINT('Ctrl Pts',(-3.46905264466117,-2.29413906943288,
9.27295052744361));
#24819=CARTESIAN_POINT('Ctrl Pts',(-2.4393379903627,-3.36853536275074,9.32593881617186));
#24820=CARTESIAN_POINT('Ctrl Pts',(-1.194095160419,-3.76361759404226,9.37892710490011));
#24821=CARTESIAN_POINT('Ctrl Pts',(0.0511476695246889,-4.15869982533377,
9.43191539362836));
#24822=CARTESIAN_POINT('Ctrl Pts',(1.5119186751136,-3.87446799459896,9.48490368235661));
#24823=CARTESIAN_POINT('Ctrl Pts',(2.5181722452647,-3.04129728726066,9.53789197108486));
#24824=CARTESIAN_POINT('Ctrl Pts',(3.5244258154158,-2.20812657992236,9.59088025981311));
#24825=CARTESIAN_POINT('Ctrl Pts',(4.07616195012909,-0.826016995980571,
9.64386854854136));
#24826=CARTESIAN_POINT('Ctrl Pts',(3.92030308000722,0.471067306450377,9.69685683726961));
#24827=CARTESIAN_POINT('Ctrl Pts',(3.76444420988535,1.76815160888132,9.74984512599786));
#24828=CARTESIAN_POINT('Ctrl Pts',(2.90099033492832,2.98021062980143,9.8028334147261));
#24829=CARTESIAN_POINT('Ctrl Pts',(1.72600180756239,3.55128123451409,9.85582170345435));
#24830=CARTESIAN_POINT('Ctrl Pts',(0.551013280196442,4.12235183922675,9.90880999218261));
#24831=CARTESIAN_POINT('Ctrl Pts',(-0.935509899578419,4.05243402773195,
9.96179828091086));
#24832=CARTESIAN_POINT('Ctrl Pts',(-2.05170977553871,3.37359861917203,10.0147865696391));
#24833=CARTESIAN_POINT('Ctrl Pts',(-3.16790965149901,2.69476321061211,10.0677748583674));
#24834=CARTESIAN_POINT('Ctrl Pts',(-3.91378622364473,1.40701020498706,10.1207631470956));
#24835=CARTESIAN_POINT('Ctrl Pts',(-3.94721103949169,0.101023047050935,
10.1737514358238));
#24836=CARTESIAN_POINT('Ctrl Pts',(-3.94806733432703,0.0675655685271688,
10.175108918186));
#24837=CARTESIAN_POINT('Ctrl Pts',(-3.94845604040098,0.0340961227584357,
10.1764664005482));
#24838=CARTESIAN_POINT('Ctrl Pts',(-3.94838239458768,0.000624922565347272,
10.1778238829104));
#24839=CARTESIAN_POINT('Origin',(0.,0.,0.));
#24840=CARTESIAN_POINT('',(-3.93845364011251,0.00310220437029302,11.3221761170896));
#24841=CARTESIAN_POINT('',(-3.93886953396072,0.00324640498314072,11.1778238829104));
#24842=CARTESIAN_POINT('',(-3.942,-4.82755768223887E-16,0.));
#24843=CARTESIAN_POINT('Ctrl Pts',(-3.93845364011251,0.00310220437029302,
11.3221761170896));
#24844=CARTESIAN_POINT('Ctrl Pts',(-3.94163276156383,0.435745363096063,
11.3047431778321));
#24845=CARTESIAN_POINT('Ctrl Pts',(-3.87593103620607,0.867449899692147,
11.2873102385747));
#24846=CARTESIAN_POINT('Ctrl Pts',(-3.73722250128773,1.27426167714383,11.2698772993172));
#24847=CARTESIAN_POINT('Ctrl Pts',(-3.31580441728399,2.51021907446466,11.2169133208226));
#24848=CARTESIAN_POINT('Ctrl Pts',(-2.2205051385,3.51640664107286,11.163949342328));
#24849=CARTESIAN_POINT('Ctrl Pts',(-0.953308955593125,3.83168068622044,
11.1109853638333));
#24850=CARTESIAN_POINT('Ctrl Pts',(0.313887227313751,4.14695473136801,11.0580213853387));
#24851=CARTESIAN_POINT('Ctrl Pts',(1.75298031434354,3.77131525505496,11.0050574068441));
#24852=CARTESIAN_POINT('Ctrl Pts',(2.70442260335169,2.87692078939432,10.9520934283495));
#24853=CARTESIAN_POINT('Ctrl Pts',(3.65586489235987,1.98252632373365,10.8991294498548));
#24854=CARTESIAN_POINT('Ctrl Pts',(4.11965638334642,0.569376868725343,10.8461654713602));
#24855=CARTESIAN_POINT('Ctrl Pts',(3.88323778121684,-0.714870044482812,
10.7932014928656));
#24856=CARTESIAN_POINT('Ctrl Pts',(3.64681917908728,-1.99911695769091,10.740237514371));
#24857=CARTESIAN_POINT('Ctrl Pts',(2.71019048384171,-3.15446132909884,10.6872735358763));
#24858=CARTESIAN_POINT('Ctrl Pts',(1.5026160073439,-3.65139972893172,10.6343095573817));
#24859=CARTESIAN_POINT('Ctrl Pts',(0.295041530846062,-4.14833812876461,
10.5813455788871));
#24860=CARTESIAN_POINT('Ctrl Pts',(-1.18347872690403,-3.98687055702237,
10.5283816003925));
#24861=CARTESIAN_POINT('Ctrl Pts',(-2.25532728072623,-3.24099887423319,
10.4754176218978));
#24862=CARTESIAN_POINT('Ctrl Pts',(-3.28905932517556,-2.52165148434584,
10.4243371202951));
#24863=CARTESIAN_POINT('Ctrl Pts',(-3.94452906787893,-1.25872547303165,
10.3732566186924));
#24864=CARTESIAN_POINT('Ctrl Pts',(-3.94826120782986,0.000860587304522282,
10.3221761170896));
#24865=CARTESIAN_POINT('Ctrl Pts',(-3.94838239458768,0.000624922565347272,
10.1778238829104));
#24866=CARTESIAN_POINT('Ctrl Pts',(-3.94558133224467,-1.27242665007483,
10.2294546892765));
#24867=CARTESIAN_POINT('Ctrl Pts',(-3.27394054517676,-2.548016178621,10.2810854956425));
#24868=CARTESIAN_POINT('Ctrl Pts',(-2.22159520444575,-3.26422967848529,
10.3327163020086));
#24869=CARTESIAN_POINT('Ctrl Pts',(-1.14158149400459,-3.99927393583826,
10.3857045907369));
#24870=CARTESIAN_POINT('Ctrl Pts',(0.339418986425944,-4.14514114029698,
10.4386928794651));
#24871=CARTESIAN_POINT('Ctrl Pts',(1.54208150481898,-3.63492300865035,10.4916811681933));
#24872=CARTESIAN_POINT('Ctrl Pts',(2.744744023212,-3.12470487700374,10.5446694569216));
#24873=CARTESIAN_POINT('Ctrl Pts',(3.66906857956751,-1.95840140925179,10.5976577456498));
#24874=CARTESIAN_POINT('Ctrl Pts',(3.89107385865357,-0.670987982622134,
10.6506460343781));
#24875=CARTESIAN_POINT('Ctrl Pts',(4.11307913773965,0.616425444007545,10.7036343231063));
#24876=CARTESIAN_POINT('Ctrl Pts',(3.63276513955622,2.02494882951498,10.7566226118346));
#24877=CARTESIAN_POINT('Ctrl Pts',(2.67044859081355,2.90850218671784,10.8096109005628));
#24878=CARTESIAN_POINT('Ctrl Pts',(1.70813204207087,3.79205554392072,10.8625991892911));
#24879=CARTESIAN_POINT('Ctrl Pts',(0.263812942768934,4.15063887281905,10.9155874780193));
#24880=CARTESIAN_POINT('Ctrl Pts',(-1.00000947224434,3.81977246727369,10.9685757667476));
#24881=CARTESIAN_POINT('Ctrl Pts',(-2.2638318872576,3.48890606172833,11.0215640554758));
#24882=CARTESIAN_POINT('Ctrl Pts',(-3.34715761798219,2.46858992173929,11.0745523442041));
#24883=CARTESIAN_POINT('Ctrl Pts',(-3.75307260433058,1.22683604158983,11.1275406329323));
#24884=CARTESIAN_POINT('Ctrl Pts',(-3.88147031395203,0.834048488809281,
11.1443017162584));
#24885=CARTESIAN_POINT('Ctrl Pts',(-3.94208881978707,0.419104697969423,
11.1610627995844));
#24886=CARTESIAN_POINT('Ctrl Pts',(-3.93886953396072,0.00324640498314072,
11.1778238829104));
#24887=CARTESIAN_POINT('Origin',(0.,0.,0.));
#24888=CARTESIAN_POINT('',(-3.93708098219134,-0.00243404615490106,12.3221761170896));
#24889=CARTESIAN_POINT('',(-3.93670434321626,-0.00217448122624482,12.1778238829104));
#24890=CARTESIAN_POINT('',(-3.942,-4.82755768223887E-16,0.));
#24891=CARTESIAN_POINT('Ctrl Pts',(-3.93708098219134,-0.00243404615490106,
12.3221761170896));
#24892=CARTESIAN_POINT('Ctrl Pts',(-3.93246581499902,0.816826384091263,
12.2891937154665));
#24893=CARTESIAN_POINT('Ctrl Pts',(-3.68329161894405,1.63865836153011,12.2562113138435));
#24894=CARTESIAN_POINT('Ctrl Pts',(-3.20967797357049,2.29968305467193,12.2232289122204));
#24895=CARTESIAN_POINT('Ctrl Pts',(-2.4491371489512,3.36117330126154,12.1702649337258));
#24896=CARTESIAN_POINT('Ctrl Pts',(-1.10983987433617,4.00799378602558,12.1173009552312));
#24897=CARTESIAN_POINT('Ctrl Pts',(0.194403355371928,3.94370158371407,12.0643369767366));
#24898=CARTESIAN_POINT('Ctrl Pts',(1.49864658508003,3.87940938140256,12.0113729982419));
#24899=CARTESIAN_POINT('Ctrl Pts',(2.7678357698812,3.1040044920155,11.9584090197473));
#24900=CARTESIAN_POINT('Ctrl Pts',(3.42029150490108,1.97286108671397,11.9054450412527));
#24901=CARTESIAN_POINT('Ctrl Pts',(4.07274723992097,0.841717681412442,11.8524810627581));
#24902=CARTESIAN_POINT('Ctrl Pts',(4.10846952515958,-0.645164239803552,
11.7995170842634));
#24903=CARTESIAN_POINT('Ctrl Pts',(3.51108655579286,-1.8063349754958,11.7465531057688));
#24904=CARTESIAN_POINT('Ctrl Pts',(2.91370358642613,-2.96750571118807,11.6935891272742));
#24905=CARTESIAN_POINT('Ctrl Pts',(1.68321536245406,-3.80296526135658,11.6406251487796));
#24906=CARTESIAN_POINT('Ctrl Pts',(0.383564333431266,-3.92981593056064,
11.5876611702849));
#24907=CARTESIAN_POINT('Ctrl Pts',(-0.91608669559151,-4.0566665997647,11.5346971917903));
#24908=CARTESIAN_POINT('Ctrl Pts',(-2.28490052966501,-3.47490838800432,
11.4817332132957));
#24909=CARTESIAN_POINT('Ctrl Pts',(-3.09553900209,-2.4511656681074,11.4287692348011));
#24910=CARTESIAN_POINT('Ctrl Pts',(-3.6393581823996,-1.76438488268918,11.3932381955639));
#24911=CARTESIAN_POINT('Ctrl Pts',(-3.93197409656805,-0.878691784660489,
11.3577071563268));
#24912=CARTESIAN_POINT('Ctrl Pts',(-3.93845364011251,0.00310220437029302,
11.3221761170896));
#24913=CARTESIAN_POINT('Ctrl Pts',(-3.93886953396072,0.00324640498314072,
11.1778238829104));
#24914=CARTESIAN_POINT('Ctrl Pts',(-3.9319114080084,-0.895584744841287,
11.2140510883126));
#24915=CARTESIAN_POINT('Ctrl Pts',(-3.62672875965172,-1.79868808138705,
11.2502782937149));
#24916=CARTESIAN_POINT('Ctrl Pts',(-3.06311856673542,-2.49158288893653,
11.2865054991171));
#24917=CARTESIAN_POINT('Ctrl Pts',(-2.23874530081967,-3.50505631900356,
11.3394937878453));
#24918=CARTESIAN_POINT('Ctrl Pts',(-0.861494527015975,-4.06881155882777,
11.3924820765736));
#24919=CARTESIAN_POINT('Ctrl Pts',(0.436898299346125,-3.92425795818127,
11.4454703653018));
#24920=CARTESIAN_POINT('Ctrl Pts',(1.73529112570822,-3.77970435753476,11.4984586540301));
#24921=CARTESIAN_POINT('Ctrl Pts',(2.95482600462875,-2.92684191641753,11.5514469427583));
#24922=CARTESIAN_POINT('Ctrl Pts',(3.53611067677546,-1.75687276941591,11.6044352314866));
#24923=CARTESIAN_POINT('Ctrl Pts',(4.11739534892219,-0.586903622414244,
11.6574235202148));
#24924=CARTESIAN_POINT('Ctrl Pts',(4.06042981429509,0.900172230471804,11.7104118089431));
#24925=CARTESIAN_POINT('Ctrl Pts',(3.39134377174076,2.02224332566476,11.7634000976713));
#24926=CARTESIAN_POINT('Ctrl Pts',(2.72225772918646,3.14431442085768,11.8163883863996));
#24927=CARTESIAN_POINT('Ctrl Pts',(1.44105117870494,3.90138075835749,11.8693766751278));
#24928=CARTESIAN_POINT('Ctrl Pts',(0.135404751111381,3.94618121729058,11.9223649638561));
#24929=CARTESIAN_POINT('Ctrl Pts',(-1.17024167648218,3.99098167622367,11.9753532525843));
#24930=CARTESIAN_POINT('Ctrl Pts',(-2.50032798118779,3.32351625659005,12.0283415413126));
#24931=CARTESIAN_POINT('Ctrl Pts',(-3.24475272518949,2.24994675463574,12.0813298300408));
#24932=CARTESIAN_POINT('Ctrl Pts',(-3.69662968598688,1.59827399972424,12.1134945143307));
#24933=CARTESIAN_POINT('Ctrl Pts',(-3.93270958942814,0.796965223217272,
12.1456591986205));
#24934=CARTESIAN_POINT('Ctrl Pts',(-3.93670434321626,-0.00217448122624482,
12.1778238829104));
#24935=CARTESIAN_POINT('Origin',(0.,0.,0.));
#24936=CARTESIAN_POINT('',(-3.94733077553239,-0.00192598462593618,13.3221761170896));
#24937=CARTESIAN_POINT('',(-3.94682996399265,-0.00229165249276323,13.1778238829104));
#24938=CARTESIAN_POINT('',(-3.942,-4.82755768223887E-16,0.));
#24939=CARTESIAN_POINT('Ctrl Pts',(-3.94733077553239,-0.00192598462593618,
13.3221761170896));
#24940=CARTESIAN_POINT('Ctrl Pts',(-3.94013816129704,1.1955636687552,13.273644253101));
#24941=CARTESIAN_POINT('Ctrl Pts',(-3.356565432248,2.39912123530496,13.2251123891123));
#24942=CARTESIAN_POINT('Ctrl Pts',(-2.40836516771617,3.12895382914166,13.1765805251237));
#24943=CARTESIAN_POINT('Ctrl Pts',(-1.37357164668001,3.92543751280327,13.123616546629));
#24944=CARTESIAN_POINT('Ctrl Pts',(0.0954887653771007,4.15772060523228,
13.0706525681344));
#24945=CARTESIAN_POINT('Ctrl Pts',(1.32553410510171,3.71934593472844,13.0176885896398));
#24946=CARTESIAN_POINT('Ctrl Pts',(2.55557944482628,3.28097126422461,12.9647246111452));
#24947=CARTESIAN_POINT('Ctrl Pts',(3.54660971221836,2.17193883078797,12.9117606326505));
#24948=CARTESIAN_POINT('Ctrl Pts',(3.84442792620346,0.900526938073336,12.8587966541559));
#24949=CARTESIAN_POINT('Ctrl Pts',(4.14224614018855,-0.370884954641299,
12.8058326756613));
#24950=CARTESIAN_POINT('Ctrl Pts',(3.74685230076666,-1.80467630663392,12.7528686971667));
#24951=CARTESIAN_POINT('Ctrl Pts',(2.83945852033214,-2.74372924270635,12.699904718672));
#24952=CARTESIAN_POINT('Ctrl Pts',(1.93206473989763,-3.68278217877878,12.6469407401774));
#24953=CARTESIAN_POINT('Ctrl Pts',(0.512671018450501,-4.127096698931,12.5939767616828));
#24954=CARTESIAN_POINT('Ctrl Pts',(-0.768203316346435,-3.8730399572846,
12.5410127831882));
#24955=CARTESIAN_POINT('Ctrl Pts',(-2.04907765114337,-3.6189832156382,12.4880488046935));
#24956=CARTESIAN_POINT('Ctrl Pts',(-3.19143259929011,-2.66655521219318,
12.4350848261989));
#24957=CARTESIAN_POINT('Ctrl Pts',(-3.67171788605172,-1.45226120626306,
12.3821208477043));
#24958=CARTESIAN_POINT('Ctrl Pts',(-3.85291381676684,-0.994147791942479,
12.3621392708327));
#24959=CARTESIAN_POINT('Ctrl Pts',(-3.93987696773182,-0.498762829361246,
12.3421576939612));
#24960=CARTESIAN_POINT('Ctrl Pts',(-3.93708098219134,-0.00243404615490106,
12.3221761170896));
#24961=CARTESIAN_POINT('Ctrl Pts',(-3.93670434321626,-0.00217448122624482,
12.1778238829104));
#24962=CARTESIAN_POINT('Ctrl Pts',(-3.93929057014649,-0.519542192545187,
12.1986474873488));
#24963=CARTESIAN_POINT('Ctrl Pts',(-3.84460194542603,-1.03600077131728,
12.2194710917872));
#24964=CARTESIAN_POINT('Ctrl Pts',(-3.64821869509448,-1.51035790430073,
12.2402946962256));
#24965=CARTESIAN_POINT('Ctrl Pts',(-3.14849673769996,-2.71741947700787,
12.2932829849538));
#24966=CARTESIAN_POINT('Ctrl Pts',(-1.99028963961311,-3.65186903814713,
12.3462712736821));
#24967=CARTESIAN_POINT('Ctrl Pts',(-0.704859028994106,-3.8850810024459,
12.3992595624103));
#24968=CARTESIAN_POINT('Ctrl Pts',(0.580571581624919,-4.11829296674466,
12.4522478511386));
#24969=CARTESIAN_POINT('Ctrl Pts',(1.99322570477611,-3.6502673342029,12.5052361398668));
#24970=CARTESIAN_POINT('Ctrl Pts',(2.88512861233689,-2.6956842427472,12.5582244285951));
#24971=CARTESIAN_POINT('Ctrl Pts',(3.77703151989765,-1.74110115129151,12.6112127173233));
#24972=CARTESIAN_POINT('Ctrl Pts',(4.148183211868,-0.299960600921891,12.6642010060516));
#24973=CARTESIAN_POINT('Ctrl Pts',(3.82833896043004,0.966696152042594,12.7171892947798));
#24974=CARTESIAN_POINT('Ctrl Pts',(3.50849470899208,2.23335290500708,12.7701775835081));
#24975=CARTESIAN_POINT('Ctrl Pts',(2.4976545141458,3.32552586056643,12.8231658722363));
#24976=CARTESIAN_POINT('Ctrl Pts',(1.259483819326,3.74224279746471,12.8761541609646));
#24977=CARTESIAN_POINT('Ctrl Pts',(0.0213131245061955,4.158959734363,12.9291424496928));
#24978=CARTESIAN_POINT('Ctrl Pts',(-1.44418807028713,3.90022065260022,12.9821307384211));
#24979=CARTESIAN_POINT('Ctrl Pts',(-2.46480444872359,3.08470738901973,13.0351190271493));
#24980=CARTESIAN_POINT('Ctrl Pts',(-3.38102522484729,2.35261038265819,13.082687312403));
#24981=CARTESIAN_POINT('Ctrl Pts',(-3.93871824071251,1.17181521210322,13.1302555976567));
#24982=CARTESIAN_POINT('Ctrl Pts',(-3.94682996399265,-0.00229165249276323,
13.1778238829104));
#24983=CARTESIAN_POINT('Origin',(0.,0.,0.));
#24984=CARTESIAN_POINT('',(-3.9429197498326,0.0035503728418125,14.3221761170896));
#24985=CARTESIAN_POINT('',(-3.94377660893062,0.00343048778150908,14.1778238829104));
#24986=CARTESIAN_POINT('',(-3.942,-4.82755768223887E-16,0.));
#24987=CARTESIAN_POINT('Ctrl Pts',(-3.9429197498326,0.0035503728418125,
14.3221761170896));
#24988=CARTESIAN_POINT('Ctrl Pts',(-3.94546599449794,0.278662013094457,
14.31105876923));
#24989=CARTESIAN_POINT('Ctrl Pts',(-3.91912941936741,0.553289499978031,
14.2999414213704));
#24990=CARTESIAN_POINT('Ctrl Pts',(-3.86210967795079,0.821391308358944,
14.2888240735108));
#24991=CARTESIAN_POINT('Ctrl Pts',(-3.59046284308573,2.09865083039248,14.2358600950161));
#24992=CARTESIAN_POINT('Ctrl Pts',(-2.62241565120338,3.22780031721448,14.1828961165215));
#24993=CARTESIAN_POINT('Ctrl Pts',(-1.40163175876062,3.69134166107696,14.1299321380269));
#24994=CARTESIAN_POINT('Ctrl Pts',(-0.18084786631787,4.15488300493943,14.0769681595322));
#24995=CARTESIAN_POINT('Ctrl Pts',(1.29267272668526,3.95281620584241,14.0240041810376));
#24996=CARTESIAN_POINT('Ctrl Pts',(2.34360392082064,3.17775007014128,13.971040202543));
#24997=CARTESIAN_POINT('Ctrl Pts',(3.39453511495603,2.40268393444014,13.9180762240484));
#24998=CARTESIAN_POINT('Ctrl Pts',(4.02287691022366,1.05461846213484,13.8651122455537));
#24999=CARTESIAN_POINT('Ctrl Pts',(3.9406553103857,-0.24861731777516,13.8121482670591));
#25000=CARTESIAN_POINT('Ctrl Pts',(3.85843371054775,-1.55185309768514,13.7591842885645));
#25001=CARTESIAN_POINT('Ctrl Pts',(3.06564871560427,-2.81025918519985,13.7062203100699));
#25002=CARTESIAN_POINT('Ctrl Pts',(1.92563993605177,-3.44709815390442,13.6532563315753));
#25003=CARTESIAN_POINT('Ctrl Pts',(0.7856311564993,-4.08393712260898,13.6002923530807));
#25004=CARTESIAN_POINT('Ctrl Pts',(-0.701601407662154,-4.09920897250343,
13.547328374586));
#25005=CARTESIAN_POINT('Ctrl Pts',(-1.85444735256939,-3.48591449443573,
13.4943643960914));
#25006=CARTESIAN_POINT('Ctrl Pts',(-3.00729329747666,-2.87262001636802,
13.4414004175968));
#25007=CARTESIAN_POINT('Ctrl Pts',(-3.82575262312968,-1.63075921033812,
13.3884364391021));
#25008=CARTESIAN_POINT('Ctrl Pts',(-3.93471897094859,-0.329486669876098,
13.3354724606075));
#25009=CARTESIAN_POINT('Ctrl Pts',(-3.94383745759853,-0.22059400231727,
13.3310403461016));
#25010=CARTESIAN_POINT('Ctrl Pts',(-3.94798763243564,-0.111285296783124,
13.3266082315956));
#25011=CARTESIAN_POINT('Ctrl Pts',(-3.94733077553239,-0.00192598462593618,
13.3221761170896));
#25012=CARTESIAN_POINT('Ctrl Pts',(-3.94682996399265,-0.00229165249276323,
13.1778238829104));
#25013=CARTESIAN_POINT('Ctrl Pts',(-3.94775422620073,-0.13607119177326,
13.183243886385));
#25014=CARTESIAN_POINT('Ctrl Pts',(-3.94154345388817,-0.269763898960769,
13.1886638898595));
#25015=CARTESIAN_POINT('Ctrl Pts',(-3.92791502810543,-0.402696136440426,
13.1940838933341));
#25016=CARTESIAN_POINT('Ctrl Pts',(-3.79467766697122,-1.70229895292184,
13.2470721820623));
#25017=CARTESIAN_POINT('Ctrl Pts',(-2.95247138262324,-2.92921714048647,
13.3000604707906));
#25018=CARTESIAN_POINT('Ctrl Pts',(-1.78761040384536,-3.52067176691954,
13.3530487595188));
#25019=CARTESIAN_POINT('Ctrl Pts',(-0.622749425067479,-4.1121263933526,
13.4060370482471));
#25020=CARTESIAN_POINT('Ctrl Pts',(0.864766248140306,-4.0681174586541,13.4590253369753));
#25021=CARTESIAN_POINT('Ctrl Pts',(1.99262340964458,-3.4088315584166,13.5120136257036));
#25022=CARTESIAN_POINT('Ctrl Pts',(3.12048057114885,-2.7495456581791,13.5650019144318));
#25023=CARTESIAN_POINT('Ctrl Pts',(3.8886792209496,-1.4749827924026,13.6179902031601));
#25024=CARTESIAN_POINT('Ctrl Pts',(3.94485192310407,-0.169776179432411,
13.6709784918883));
#25025=CARTESIAN_POINT('Ctrl Pts',(4.00102462525853,1.13543043353777,13.7239667806165));
#25026=CARTESIAN_POINT('Ctrl Pts',(3.34517137976671,2.47128079370165,13.7769550693448));
#25027=CARTESIAN_POINT('Ctrl Pts',(2.27812755848019,3.2250295306576,13.829943358073));
#25028=CARTESIAN_POINT('Ctrl Pts',(1.21108373719365,3.97877826761357,13.8829316468013));
#25029=CARTESIAN_POINT('Ctrl Pts',(-0.267150659887593,4.15042538136161,
13.9359199355295));
#25030=CARTESIAN_POINT('Ctrl Pts',(-1.47851968414005,3.66123752164906,13.9889082242578));
#25031=CARTESIAN_POINT('Ctrl Pts',(-2.68988870839249,3.17204966193652,14.041896512986));
#25032=CARTESIAN_POINT('Ctrl Pts',(-3.63439235981614,2.02202682876341,14.0948848017143));
#25033=CARTESIAN_POINT('Ctrl Pts',(-3.87879331109071,0.738676584276535,
14.1478730904425));
#25034=CARTESIAN_POINT('Ctrl Pts',(-3.92484123568096,0.496878772227051,
14.1578566879318));
#25035=CARTESIAN_POINT('Ctrl Pts',(-3.9460363164428,0.250347989813759,14.1678402854211));
#25036=CARTESIAN_POINT('Ctrl Pts',(-3.94377660893062,0.00343048778150908,
14.1778238829104));
#25037=CARTESIAN_POINT('Origin',(0.,0.,0.));
#25038=CARTESIAN_POINT('',(-3.935515150562,-7.56757525427476E-5,15.3221761170896));
#25039=CARTESIAN_POINT('',(-3.93554762371472,0.000453016733568931,15.1778238829104));
#25040=CARTESIAN_POINT('',(-3.942,-4.82755768223887E-16,0.));
#25041=CARTESIAN_POINT('Ctrl Pts',(-3.935515150562,-7.56757525427476E-5,
15.3221761170896));
#25042=CARTESIAN_POINT('Ctrl Pts',(-3.93540179088204,0.662968867054025,
15.2955093068644));
#25043=CARTESIAN_POINT('Ctrl Pts',(-3.77682343808938,1.32606434282809,15.2688424966392));
#25044=CARTESIAN_POINT('Ctrl Pts',(-3.46008318945363,1.90220902322252,15.242175686414));
#25045=CARTESIAN_POINT('Ctrl Pts',(-2.83099318673311,3.04651215526165,15.1892117079193));
#25046=CARTESIAN_POINT('Ctrl Pts',(-1.57799465489921,3.84781647231203,15.1362477294247));
#25047=CARTESIAN_POINT('Ctrl Pts',(-0.275346694985541,3.93887789142153,
15.0832837509301));
#25048=CARTESIAN_POINT('Ctrl Pts',(1.02730126492813,4.02993931053103,15.0303197724355));
#25049=CARTESIAN_POINT('Ctrl Pts',(2.37959865292158,3.41075783169958,14.9773557939409));
#25050=CARTESIAN_POINT('Ctrl Pts',(3.16177691968707,2.36510920595707,14.9243918154462));
#25051=CARTESIAN_POINT('Ctrl Pts',(3.94395518645256,1.31946058021456,14.8714278369516));
#25052=CARTESIAN_POINT('Ctrl Pts',(4.15601433199016,-0.152655192438981,
14.818463858457));
#25053=CARTESIAN_POINT('Ctrl Pts',(3.70076597882895,-1.37655585281198,14.7654998799624));
#25054=CARTESIAN_POINT('Ctrl Pts',(3.24551762566774,-2.60045651318499,14.7125359014677));
#25055=CARTESIAN_POINT('Ctrl Pts',(2.1229617738077,-3.57614206127742,14.6595719229731));
#25056=CARTESIAN_POINT('Ctrl Pts',(0.847574616134508,-3.85644812178943,
14.6066079444785));
#25057=CARTESIAN_POINT('Ctrl Pts',(-0.427812541538684,-4.13675418230144,
14.5536439659839));
#25058=CARTESIAN_POINT('Ctrl Pts',(-1.85603100502504,-3.72168075523303,
14.5006799874892));
#25059=CARTESIAN_POINT('Ctrl Pts',(-2.78251699784433,-2.80145926307632,
14.4477160089946));
#25060=CARTESIAN_POINT('Ctrl Pts',(-3.5145299287451,-2.07439588945562,14.4058693783596));
#25061=CARTESIAN_POINT('Ctrl Pts',(-3.93333547115731,-1.0319929364451,14.3640227477246));
#25062=CARTESIAN_POINT('Ctrl Pts',(-3.9429197498326,0.0035503728418125,
14.3221761170896));
#25063=CARTESIAN_POINT('Ctrl Pts',(-3.94377660893062,0.00343048778150908,
14.1778238829104));
#25064=CARTESIAN_POINT('Ctrl Pts',(-3.93404284072175,-1.06017518620376,
14.2208285741494));
#25065=CARTESIAN_POINT('Ctrl Pts',(-3.48910890040614,-2.13095638625906,
14.2638332653883));
#25066=CARTESIAN_POINT('Ctrl Pts',(-2.72071532173612,-2.86153608825589,
14.3068379566273));
#25067=CARTESIAN_POINT('Ctrl Pts',(-1.77393812998146,-3.7617208605008,14.3598262453555));
#25068=CARTESIAN_POINT('Ctrl Pts',(-0.336085495346666,-4.14541274918995,
14.4128145340838));
#25069=CARTESIAN_POINT('Ctrl Pts',(0.933309470178012,-3.83661492453915,
14.465802822812));
#25070=CARTESIAN_POINT('Ctrl Pts',(2.20270443570267,-3.52781709988836,14.5187911115403));
#25071=CARTESIAN_POINT('Ctrl Pts',(3.30364173211722,-2.5265295618976,14.5717794002685));
#25072=CARTESIAN_POINT('Ctrl Pts',(3.73112899530853,-1.29203601601831,14.6247676889968));
#25073=CARTESIAN_POINT('Ctrl Pts',(4.15861625849985,-0.0575424701390118,
14.677755977725));
#25074=CARTESIAN_POINT('Ctrl Pts',(3.91265348846795,1.41015708362883,14.7307442664533));
#25075=CARTESIAN_POINT('Ctrl Pts',(3.10606211575817,2.43783895681654,14.7837325551815));
#25076=CARTESIAN_POINT('Ctrl Pts',(2.29947074304839,3.46552083000428,14.8367208439098));
#25077=CARTESIAN_POINT('Ctrl Pts',(0.932250767660721,4.05318502261185,14.889709132638));
#25078=CARTESIAN_POINT('Ctrl Pts',(-0.368463413303181,3.93127401224813,
14.9426974213663));
#25079=CARTESIAN_POINT('Ctrl Pts',(-1.66917759426705,3.80936300188441,14.9956857100945));
#25080=CARTESIAN_POINT('Ctrl Pts',(-2.90338598080718,2.9778767885494,15.0486739988228));
#25081=CARTESIAN_POINT('Ctrl Pts',(-3.50496567659063,1.81821237820066,15.101662287551));
#25082=CARTESIAN_POINT('Ctrl Pts',(-3.79318829122445,1.26260601250841,15.1270494860042));
#25083=CARTESIAN_POINT('Ctrl Pts',(-3.93619350756073,0.631667647738924,
15.1524366844573));
#25084=CARTESIAN_POINT('Ctrl Pts',(-3.93554762371472,0.000453016733568931,
15.1778238829104));
#25085=CARTESIAN_POINT('Origin',(0.,0.,0.));
#25086=CARTESIAN_POINT('',(-3.94319808732824,-0.00351593218956836,16.3221761170896));
#25087=CARTESIAN_POINT('',(-3.94210945089404,-0.00361990150021516,16.1778238829104));
#25088=CARTESIAN_POINT('',(-3.942,-4.82755768223887E-16,0.));
#25089=CARTESIAN_POINT('Ctrl Pts',(-3.94319808732824,-0.00351593218956836,
16.3221761170896));
#25090=CARTESIAN_POINT('Ctrl Pts',(-3.93355225073649,1.04098512265698,16.2799598444988));
#25091=CARTESIAN_POINT('Ctrl Pts',(-3.50650185007344,2.09245600266764,16.237743571908));
#25092=CARTESIAN_POINT('Ctrl Pts',(-2.76293020390983,2.82077853336478,16.1955272993172));
#25093=CARTESIAN_POINT('Ctrl Pts',(-1.83005502901329,3.73452236922869,16.1425633208226));
#25094=CARTESIAN_POINT('Ctrl Pts',(-0.398979196739877,4.13963456552086,
16.089599342328));
#25095=CARTESIAN_POINT('Ctrl Pts',(0.87442396179839,3.85044901031056,16.0366353638333));
#25096=CARTESIAN_POINT('Ctrl Pts',(2.14782712033666,3.56126345510026,15.9836713853387));
#25097=CARTESIAN_POINT('Ctrl Pts',(3.26355760513978,2.57778014838748,15.9307074068441));
#25098=CARTESIAN_POINT('Ctrl Pts',(3.7102673428296,1.35073723969577,15.8777434283495));
#25099=CARTESIAN_POINT('Ctrl Pts',(4.15697708051941,0.123694331004073,15.8247794498548));
#25100=CARTESIAN_POINT('Ctrl Pts',(3.93466607109594,-1.34690817966655,15.7718154713602));
#25101=CARTESIAN_POINT('Ctrl Pts',(3.14522120203587,-2.38708157301605,15.7188514928656));
#25102=CARTESIAN_POINT('Ctrl Pts',(2.3557763329758,-3.42725496636555,15.665887514371));
#25103=CARTESIAN_POINT('Ctrl Pts',(0.999197604279134,-4.03699924239392,
15.6129235358763));
#25104=CARTESIAN_POINT('Ctrl Pts',(-0.302784262564327,-3.93686379448313,
15.5599595573817));
#25105=CARTESIAN_POINT('Ctrl Pts',(-1.60476612940779,-3.83672834657235,
15.5069955788871));
#25106=CARTESIAN_POINT('Ctrl Pts',(-2.85215113439804,-3.02671317472241,
15.4540316003925));
#25107=CARTESIAN_POINT('Ctrl Pts',(-3.47325290008964,-1.8780546152835,15.4010676218978));
#25108=CARTESIAN_POINT('Ctrl Pts',(-3.78163641109193,-1.30773364846388,
15.3747704536284));
#25109=CARTESIAN_POINT('Ctrl Pts',(-3.9356269389069,-0.653929427477854,
15.348473285359));
#25110=CARTESIAN_POINT('Ctrl Pts',(-3.935515150562,-7.56757525427476E-5,
15.3221761170896));
#25111=CARTESIAN_POINT('Ctrl Pts',(-3.93554762371472,0.000453016733568931,
15.1778238829104));
#25112=CARTESIAN_POINT('Ctrl Pts',(-3.93484541553788,-0.685806715529583,
15.2054249731855));
#25113=CARTESIAN_POINT('Ctrl Pts',(-3.76434547901772,-1.37239299857592,
15.2330260634607));
#25114=CARTESIAN_POINT('Ctrl Pts',(-3.42606065206783,-1.96285227530577,
15.2606271537358));
#25115=CARTESIAN_POINT('Ctrl Pts',(-2.77662492673475,-3.09640991110095,
15.313615442464));
#25116=CARTESIAN_POINT('Ctrl Pts',(-1.5088024710418,-3.87568257532879,15.3666037311923));
#25117=CARTESIAN_POINT('Ctrl Pts',(-0.204134723598678,-3.94322325781103,
15.4195920199205));
#25118=CARTESIAN_POINT('Ctrl Pts',(1.10053302384446,-4.01076394029327,15.4725803086488));
#25119=CARTESIAN_POINT('Ctrl Pts',(2.44204606303776,-3.36657264102987,15.525568597377));
#25120=CARTESIAN_POINT('Ctrl Pts',(3.2050615916644,-2.30613547736428,15.5785568861053));
#25121=CARTESIAN_POINT('Ctrl Pts',(3.96807712029102,-1.24569831369873,15.6315451748335));
#25122=CARTESIAN_POINT('Ctrl Pts',(4.15259513835105,0.230984714368973,15.6845334635618));
#25123=CARTESIAN_POINT('Ctrl Pts',(3.67397850032763,1.44656926050946,15.73752175229));
#25124=CARTESIAN_POINT('Ctrl Pts',(3.1953618623042,2.66215380664994,15.7905100410183));
#25125=CARTESIAN_POINT('Ctrl Pts',(2.05361056819728,3.6166398708632,15.8434983297465));
#25126=CARTESIAN_POINT('Ctrl Pts',(0.772438082086977,3.87221126175501,15.8964866184748));
#25127=CARTESIAN_POINT('Ctrl Pts',(-0.508734404023323,4.12778265264681,
15.949474907203));
#25128=CARTESIAN_POINT('Ctrl Pts',(-1.92932808213704,3.68443937021718,16.0024631959313));
#25129=CARTESIAN_POINT('Ctrl Pts',(-2.83772640488938,2.74553992819521,16.0554514846595));
#25130=CARTESIAN_POINT('Ctrl Pts',(-3.53701854402849,2.02276778870165,16.0962422840765));
#25131=CARTESIAN_POINT('Ctrl Pts',(-3.93278162022236,1.00632704174549,16.1370330834934));
#25132=CARTESIAN_POINT('Ctrl Pts',(-3.94210945089404,-0.00361990150021516,
16.1778238829104));
#25133=CARTESIAN_POINT('Origin',(0.,0.,0.));
#25134=CARTESIAN_POINT('',(-3.94714763575412,0.00206509481356407,17.3221761170896));
#25135=CARTESIAN_POINT('',(-3.94786894067556,0.00143683566665543,17.1778238829104));
#25136=CARTESIAN_POINT('',(-3.942,-4.82755768223887E-16,0.));
#25137=CARTESIAN_POINT('Ctrl Pts',(-3.94714763575412,0.00206509481356407,
17.3221761170896));
#25138=CARTESIAN_POINT('Ctrl Pts',(-3.94790115726501,0.120559580499713,
17.3173743606278));
#25139=CARTESIAN_POINT('Ctrl Pts',(-3.94302847934562,0.238991236972465,
17.3125726041661));
#25140=CARTESIAN_POINT('Ctrl Pts',(-3.93232775304421,0.356893945881719,
17.3077708477043));
#25141=CARTESIAN_POINT('Ctrl Pts',(-3.81429739431669,1.6573756735258,17.2548068692097));
#25142=CARTESIAN_POINT('Ctrl Pts',(-2.98720523271932,2.89350369502107,17.201842890715));
#25143=CARTESIAN_POINT('Ctrl Pts',(-1.83011412357382,3.49875079716524,17.1488789122204));
#25144=CARTESIAN_POINT('Ctrl Pts',(-0.67302301442832,4.10399789930941,17.0959149337258));
#25145=CARTESIAN_POINT('Ctrl Pts',(0.814067042265299,4.07836408210249,17.0429509552312));
#25146=CARTESIAN_POINT('Ctrl Pts',(1.94961095493928,3.43359752597032,16.9899869767366));
#25147=CARTESIAN_POINT('Ctrl Pts',(3.08515486761327,2.78883096983815,16.9370229982419));
#25148=CARTESIAN_POINT('Ctrl Pts',(3.86915263626762,1.52493167478073,16.8840590197473));
#25149=CARTESIAN_POINT('Ctrl Pts',(3.94229190545934,0.221154647517415,16.8310950412527));
#25150=CARTESIAN_POINT('Ctrl Pts',(4.01543117465106,-1.08262237974594,16.7781310627581));
#25151=CARTESIAN_POINT('Ctrl Pts',(3.37771194438013,-2.42627713921516,16.7251670842634));
#25152=CARTESIAN_POINT('Ctrl Pts',(2.32140596324251,-3.19400206634104,16.6722031057688));
#25153=CARTESIAN_POINT('Ctrl Pts',(1.26509998210492,-3.96172699346691,16.6192391272742));
#25154=CARTESIAN_POINT('Ctrl Pts',(-0.209792749899407,-4.15352208824943,
16.5662751487796));
#25155=CARTESIAN_POINT('Ctrl Pts',(-1.42731727122521,-3.68148614736372,
16.5133111702849));
#25156=CARTESIAN_POINT('Ctrl Pts',(-2.64484179255099,-3.20945020647802,
16.4603471917903));
#25157=CARTESIAN_POINT('Ctrl Pts',(-3.60499810319833,-2.07358322992414,
16.4073832132957));
#25158=CARTESIAN_POINT('Ctrl Pts',(-3.86773899976216,-0.794462003929412,
16.3544192348011));
#25159=CARTESIAN_POINT('Ctrl Pts',(-3.92105564940663,-0.534896556939351,
16.3436715288973));
#25160=CARTESIAN_POINT('Ctrl Pts',(-3.94565379003534,-0.269432117224103,
16.3329238229934));
#25161=CARTESIAN_POINT('Ctrl Pts',(-3.94319808732824,-0.00351593218956836,
16.3221761170896));
#25162=CARTESIAN_POINT('Ctrl Pts',(-3.94210945089404,-0.00361990150021516,
16.1778238829104));
#25163=CARTESIAN_POINT('Ctrl Pts',(-3.94489871015204,-0.305619794154464,
16.1900213722217));
#25164=CARTESIAN_POINT('Ctrl Pts',(-3.91313437834161,-0.607039035223508,
16.202218861533));
#25165=CARTESIAN_POINT('Ctrl Pts',(-3.84459973154587,-0.899851960334574,
16.2144163508443));
#25166=CARTESIAN_POINT('Ctrl Pts',(-3.54687176805904,-2.17188880522799,
16.2674046395725));
#25167=CARTESIAN_POINT('Ctrl Pts',(-2.55521287369446,-3.2815068934005,16.3203929283008));
#25168=CARTESIAN_POINT('Ctrl Pts',(-1.32449016131116,-3.71973204127804,
16.373381217029));
#25169=CARTESIAN_POINT('Ctrl Pts',(-0.0937674489278181,-4.15795718915558,
16.4263695057573));
#25170=CARTESIAN_POINT('Ctrl Pts',(1.37601908147424,-3.9247893967381,16.4793577944855));
#25171=CARTESIAN_POINT('Ctrl Pts',(2.4106884596013,-3.12718112636055,16.5323460832138));
#25172=CARTESIAN_POINT('Ctrl Pts',(3.44535783772833,-2.32957285598302,16.585334371942));
#25173=CARTESIAN_POINT('Ctrl Pts',(4.04491006358037,-0.967524107645474,
16.6383226606703));
#25174=CARTESIAN_POINT('Ctrl Pts',(3.93433465569921,0.334202727823592,16.6913109493985));
#25175=CARTESIAN_POINT('Ctrl Pts',(3.82375924781804,1.63592956329268,16.7442992381268));
#25176=CARTESIAN_POINT('Ctrl Pts',(3.00305620620361,2.87733448589332,16.797287526855));
#25177=CARTESIAN_POINT('Ctrl Pts',(1.84867637012666,3.48899359770921,16.8502758155833));
#25178=CARTESIAN_POINT('Ctrl Pts',(0.694296534049695,4.10065270952511,16.9032641043115));
#25179=CARTESIAN_POINT('Ctrl Pts',(-0.793760096489806,4.08256601055629,
16.9562523930398));
#25180=CARTESIAN_POINT('Ctrl Pts',(-1.93293218195181,3.44302974519471,17.009240681768));
#25181=CARTESIAN_POINT('Ctrl Pts',(-3.0721042674138,2.80349347983313,17.0622289704962));
#25182=CARTESIAN_POINT('Ctrl Pts',(-3.86239180779829,1.54250764807881,17.1152172592245));
#25183=CARTESIAN_POINT('Ctrl Pts',(-3.94129534500935,0.238477776172487,
17.1682055479527));
#25184=CARTESIAN_POINT('Ctrl Pts',(-3.94606948578935,0.159576089253736,
17.1714116596053));
#25185=CARTESIAN_POINT('Ctrl Pts',(-3.9482392631182,0.0805168189138495,
17.1746177712579));
#25186=CARTESIAN_POINT('Ctrl Pts',(-3.94786894067556,0.00143683566665543,
17.1778238829104));
#25187=CARTESIAN_POINT('Origin',(0.,0.,0.));
#25188=CARTESIAN_POINT('',(-3.93691309430117,0.00231896033839218,18.3221761170896));
#25189=CARTESIAN_POINT('',(-3.93777174659584,0.00283174072808758,18.1778238829104));
#25190=CARTESIAN_POINT('',(-3.942,-4.82755768223887E-16,0.));
#25191=CARTESIAN_POINT('Ctrl Pts',(-3.93691309430117,0.00231896033839218,
18.3221761170896));
#25192=CARTESIAN_POINT('Ctrl Pts',(-3.93961914157867,0.507883428428715,
18.3018248982623));
#25193=CARTESIAN_POINT('Ctrl Pts',(-3.84930447301574,1.01251781158405,18.2814736794349));
#25194=CARTESIAN_POINT('Ctrl Pts',(-3.66151008646525,1.47780876052409,18.2611224606075));
#25195=CARTESIAN_POINT('Ctrl Pts',(-3.17277582759625,2.68872688893964,18.2081584821129));
#25196=CARTESIAN_POINT('Ctrl Pts',(-2.02381253743022,3.63317238083008,18.1551945036183));
#25197=CARTESIAN_POINT('Ctrl Pts',(-0.741199145924524,3.87829842483136,
18.1022305251237));
#25198=CARTESIAN_POINT('Ctrl Pts',(0.541414245581171,4.12342446883263,18.049266546629));
#25199=CARTESIAN_POINT('Ctrl Pts',(1.95767773842654,3.66923106494473,17.9963025681344));
#25200=CARTESIAN_POINT('Ctrl Pts',(2.8585066133837,2.72387862930978,17.9433385896398));
#25201=CARTESIAN_POINT('Ctrl Pts',(3.75933548834084,1.77852619367486,17.8903746111452));
#25202=CARTESIAN_POINT('Ctrl Pts',(4.14472974540982,0.342014726292911,17.8374106326505));
#25203=CARTESIAN_POINT('Ctrl Pts',(3.83806015958749,-0.927291247319836,
17.7844466541559));
#25204=CARTESIAN_POINT('Ctrl Pts',(3.53139057376515,-2.19659722093258,17.7314826756613));
#25205=CARTESIAN_POINT('Ctrl Pts',(2.53265714505146,-3.29869770077617,17.6785186971667));
#25206=CARTESIAN_POINT('Ctrl Pts',(1.29958727405717,-3.72849135215269,17.625554718672));
#25207=CARTESIAN_POINT('Ctrl Pts',(0.0665174030628353,-4.15828500352923,
17.5725907401774));
#25208=CARTESIAN_POINT('Ctrl Pts',(-1.40088891021208,-3.91577182643871,
17.5196267616828));
#25209=CARTESIAN_POINT('Ctrl Pts',(-2.43010778892075,-3.11209752099697,
17.4666627831882));
#25210=CARTESIAN_POINT('Ctrl Pts',(-3.36601686459191,-2.38128496799525,
17.4185005611553));
#25211=CARTESIAN_POINT('Ctrl Pts',(-3.93958972010326,-1.18644951952042,
17.3703383391225));
#25212=CARTESIAN_POINT('Ctrl Pts',(-3.94714763575412,0.00206509481356407,
17.3221761170896));
#25213=CARTESIAN_POINT('Ctrl Pts',(-3.94786894067556,0.00143683566665543,
17.1778238829104));
#25214=CARTESIAN_POINT('Ctrl Pts',(-3.94211884229706,-1.22645980543112,
17.2276060599861));
#25215=CARTESIAN_POINT('Ctrl Pts',(-3.32396017207549,-2.45935025115224,
17.2773882370618));
#25216=CARTESIAN_POINT('Ctrl Pts',(-2.33396838579359,-3.18485042355784,
17.3271704141375));
#25217=CARTESIAN_POINT('Ctrl Pts',(-1.28021835532917,-3.95707483932351,
17.3801587028657));
#25218=CARTESIAN_POINT('Ctrl Pts',(0.194801239637294,-4.15444975879655,
17.433146991594));
#25219=CARTESIAN_POINT('Ctrl Pts',(1.41450905809659,-3.68644066422928,17.4861352803222));
#25220=CARTESIAN_POINT('Ctrl Pts',(2.63421687655591,-3.21843156966201,17.5391235690505));
#25221=CARTESIAN_POINT('Ctrl Pts',(3.59861291850804,-2.08503846105438,17.5921118577787));
#25222=CARTESIAN_POINT('Ctrl Pts',(3.86533535394433,-0.806140960297021,
17.645100146507));
#25223=CARTESIAN_POINT('Ctrl Pts',(4.13205778938061,0.472756540460342,17.6980884352352));
#25224=CARTESIAN_POINT('Ctrl Pts',(3.70110661830104,1.89715843336744,17.7510767239635));
#25225=CARTESIAN_POINT('Ctrl Pts',(2.77015617820835,2.81370136913189,17.8040650126917));
#25226=CARTESIAN_POINT('Ctrl Pts',(1.83920573811566,3.73024430489631,17.85705330142));
#25227=CARTESIAN_POINT('Ctrl Pts',(0.408256029009864,4.13892828351809,17.9100415901482));
#25228=CARTESIAN_POINT('Ctrl Pts',(-0.866326161571161,3.85229277549071,
17.9630298788765));
#25229=CARTESIAN_POINT('Ctrl Pts',(-2.14090835215219,3.56565726746332,18.0160181676047));
#25230=CARTESIAN_POINT('Ctrl Pts',(-3.25912302420844,2.58370227278676,18.069006456333));
#25231=CARTESIAN_POINT('Ctrl Pts',(-3.70805280027739,1.35684379228987,18.1219947450612));
#25232=CARTESIAN_POINT('Ctrl Pts',(-3.86571884909867,0.925965870186712,
18.1406044576776));
#25233=CARTESIAN_POINT('Ctrl Pts',(-3.94083233343714,0.464880467044514,
18.159214170294));
#25234=CARTESIAN_POINT('Ctrl Pts',(-3.93777174659584,0.00283174072808758,
18.1778238829104));
#25235=CARTESIAN_POINT('Origin',(0.,0.,0.));
#25236=CARTESIAN_POINT('',(-3.93868067607543,-0.00317875339515938,19.3221761170896));
#25237=CARTESIAN_POINT('',(-3.93757571821786,-0.00273443803236162,19.1778238829104));
#25238=CARTESIAN_POINT('',(-3.942,-4.82755768223887E-16,0.));
#25239=CARTESIAN_POINT('Ctrl Pts',(-3.93868067607543,-0.00317875339515938,
19.3221761170896));
#25240=CARTESIAN_POINT('Ctrl Pts',(-3.93194593082782,0.887659399123926,
19.2862754358966));
#25241=CARTESIAN_POINT('Ctrl Pts',(-3.63268362464169,1.78259416274328,19.2503747547037));
#25242=CARTESIAN_POINT('Ctrl Pts',(-3.07838529125365,2.47267443157326,19.2144740735107));
#25243=CARTESIAN_POINT('Ctrl Pts',(-2.26063353742526,3.4907441534662,19.1615100950161));
#25244=CARTESIAN_POINT('Ctrl Pts',(-0.887799511314515,4.06295099197559,
19.1085461165215));
#25245=CARTESIAN_POINT('Ctrl Pts',(0.410936134697139,3.92704804390779,19.0555821380269));
#25246=CARTESIAN_POINT('Ctrl Pts',(1.70967178070872,3.79114509584001,19.0026181595322));
#25247=CARTESIAN_POINT('Ctrl Pts',(2.93430904662124,2.94713236119515,18.9496541810376));
#25248=CARTESIAN_POINT('Ctrl Pts',(3.52358702306116,1.78182752725689,18.896690202543));
#25249=CARTESIAN_POINT('Ctrl Pts',(4.11286499950109,0.616522693318613,18.8437262240484));
#25250=CARTESIAN_POINT('Ctrl Pts',(4.06678368646841,-0.870074239913033,
18.7907622455538));
#25251=CARTESIAN_POINT('Ctrl Pts',(3.40646251285886,-1.99664418323714,18.7377982670591));
#25252=CARTESIAN_POINT('Ctrl Pts',(2.74614133924929,-3.1232141265613,18.6848342885645));
#25253=CARTESIAN_POINT('Ctrl Pts',(1.47158030506274,-3.88975707997784,18.6318703100699));
#25254=CARTESIAN_POINT('Ctrl Pts',(0.166920776077049,-3.94496036741581,
18.5789063315753));
#25255=CARTESIAN_POINT('Ctrl Pts',(-1.1377387529086,-4.00016365485379,18.5259423530806));
#25256=CARTESIAN_POINT('Ctrl Pts',(-2.47249677669342,-3.34402727631325,
18.472978374586));
#25257=CARTESIAN_POINT('Ctrl Pts',(-3.22562317479983,-2.27726370457266,
18.4200143960914));
#25258=CARTESIAN_POINT('Ctrl Pts',(-3.689363454866,-1.62040021025458,18.3874016364241));
#25259=CARTESIAN_POINT('Ctrl Pts',(-3.93257666264772,-0.807846398012042,
18.3547888767569));
#25260=CARTESIAN_POINT('Ctrl Pts',(-3.93691309430117,0.00231896033839218,
18.3221761170896));
#25261=CARTESIAN_POINT('Ctrl Pts',(-3.93777174659584,0.00283174072808758,
18.1778238829104));
#25262=CARTESIAN_POINT('Ctrl Pts',(-3.93211778407426,-0.850732074710112,
18.2122024590223));
#25263=CARTESIAN_POINT('Ctrl Pts',(-3.65968019788323,-1.70758341046428,
18.2465810351341));
#25264=CARTESIAN_POINT('Ctrl Pts',(-3.14806281812505,-2.38335501750349,
18.280959611246));
#25265=CARTESIAN_POINT('Ctrl Pts',(-2.3594981798221,-3.42493338048278,18.3339478999742));
#25266=CARTESIAN_POINT('Ctrl Pts',(-1.00272402313454,-4.03632814012413,
18.3869361887025));
#25267=CARTESIAN_POINT('Ctrl Pts',(0.299916680013111,-3.93709672618929,
18.4399244774307));
#25268=CARTESIAN_POINT('Ctrl Pts',(1.60255738316074,-3.83786531225445,18.492912766159));
#25269=CARTESIAN_POINT('Ctrl Pts',(2.85106463276846,-3.02800772474346,18.5459010548872));
#25270=CARTESIAN_POINT('Ctrl Pts',(3.47275674238136,-1.8790000677396,18.5988893436155));
#25271=CARTESIAN_POINT('Ctrl Pts',(4.09444885199426,-0.729992410735758,
18.6518776323437));
#25272=CARTESIAN_POINT('Ctrl Pts',(4.08932582161236,0.758165315760947,18.704865921072));
#25273=CARTESIAN_POINT('Ctrl Pts',(3.45973755002874,1.90286540019034,18.7578542098002));
#25274=CARTESIAN_POINT('Ctrl Pts',(2.83014927844509,3.04756548461977,18.8108424985285));
#25275=CARTESIAN_POINT('Ctrl Pts',(1.57609576565968,3.84880792698187,18.8638307872567));
#25276=CARTESIAN_POINT('Ctrl Pts',(0.272802730892003,3.93906833100647,18.916819075985));
#25277=CARTESIAN_POINT('Ctrl Pts',(-1.03049030387567,4.02932873503108,18.9698073647132));
#25278=CARTESIAN_POINT('Ctrl Pts',(-2.3830228606256,3.4086071007182,19.0227956534415));
#25279=CARTESIAN_POINT('Ctrl Pts',(-3.16439756014476,2.36162417155469,19.0757839421697));
#25280=CARTESIAN_POINT('Ctrl Pts',(-3.66596391218726,1.68956324002662,19.10979725575));
#25281=CARTESIAN_POINT('Ctrl Pts',(-3.93219107470607,0.841866122485371,
19.1438105693302));
#25282=CARTESIAN_POINT('Ctrl Pts',(-3.93757571821786,-0.00273443803236162,
19.1778238829104));
#25283=CARTESIAN_POINT('Origin',(0.,0.,0.));
#25284=CARTESIAN_POINT('',(-3.94834041879863,-0.000694519400761262,20.3221761170896));
#25285=CARTESIAN_POINT('',(-3.94772619292891,-0.00158826883248112,20.1778238829104));
#25286=CARTESIAN_POINT('',(-3.942,-4.82755768223887E-16,0.));
#25287=CARTESIAN_POINT('Ctrl Pts',(-3.94834041879863,-0.000694519400761262,
20.3221761170896));
#25288=CARTESIAN_POINT('Ctrl Pts',(-3.94525718695861,1.26793825937276,20.270725973531));
#25289=CARTESIAN_POINT('Ctrl Pts',(-3.27892645249503,2.53935361509062,20.2192758299725));
#25290=CARTESIAN_POINT('Ctrl Pts',(-2.23269077785256,3.25663426508529,20.167825686414));
#25291=CARTESIAN_POINT('Ctrl Pts',(-1.15567135789659,3.9950197056954,20.1148617079193));
#25292=CARTESIAN_POINT('Ctrl Pts',(0.323938040913112,4.14618172311401,20.0618977294247));
#25293=CARTESIAN_POINT('Ctrl Pts',(1.52802077187684,3.64084157388599,20.0089337509301));
#25294=CARTESIAN_POINT('Ctrl Pts',(2.73210350284056,3.13550142465798,19.9559697724355));
#25295=CARTESIAN_POINT('Ctrl Pts',(3.66065956595831,1.97365910878334,19.9030057939409));
#25296=CARTESIAN_POINT('Ctrl Pts',(3.88812440006945,0.687796115025536,19.8500418154462));
#25297=CARTESIAN_POINT('Ctrl Pts',(4.11558923418059,-0.598066878732264,
19.7970778369516));
#25298=CARTESIAN_POINT('Ctrl Pts',(3.64196283928513,-2.00795055037323,19.744113858457));
#25299=CARTESIAN_POINT('Ctrl Pts',(2.68431192455269,-2.89569410291512,19.6911498799624));
#25300=CARTESIAN_POINT('Ctrl Pts',(1.72666100982023,-3.78343765545704,19.6381859014677));
#25301=CARTESIAN_POINT('Ctrl Pts',(0.284985575250775,-4.14904108889985,
19.5852219229731));
#25302=CARTESIAN_POINT('Ctrl Pts',(-0.979983166843207,-3.82494546870956,
19.5322579444785));
#25303=CARTESIAN_POINT('Ctrl Pts',(-2.24495190893719,-3.50084984851927,
19.4792939659839));
#25304=CARTESIAN_POINT('Ctrl Pts',(-3.3332139585557,-2.48705517469588,19.4263299874892));
#25305=CARTESIAN_POINT('Ctrl Pts',(-3.74601024259189,-1.24819153514592,
19.3733660089946));
#25306=CARTESIAN_POINT('Ctrl Pts',(-3.87899998240626,-0.849069354397836,
19.3563027116929));
#25307=CARTESIAN_POINT('Ctrl Pts',(-3.94188164487581,-0.426586770708422,
19.3392394143913));
#25308=CARTESIAN_POINT('Ctrl Pts',(-3.93868067607543,-0.00317875339515938,
19.3221761170896));
#25309=CARTESIAN_POINT('Ctrl Pts',(-3.93757571821786,-0.00273443803236162,
19.1778238829104));
#25310=CARTESIAN_POINT('Ctrl Pts',(-3.9405796442122,-0.473910955663478,
19.1967988580584));
#25311=CARTESIAN_POINT('Ctrl Pts',(-3.86240471339523,-0.944123769370189,
19.2157738332064));
#25312=CARTESIAN_POINT('Ctrl Pts',(-3.69862306761181,-1.38234150992047,
19.2347488083545));
#25313=CARTESIAN_POINT('Ctrl Pts',(-3.24125703327134,-2.60608003821792,
19.2877370970827));
#25314=CARTESIAN_POINT('Ctrl Pts',(-2.11630812230202,-3.58031287079873,
19.340725385811));
#25315=CARTESIAN_POINT('Ctrl Pts',(-0.839782661227222,-3.85816610946462,
19.3937136745392));
#25316=CARTESIAN_POINT('Ctrl Pts',(0.436742799847613,-4.13601934813052,
19.4467019632675));
#25317=CARTESIAN_POINT('Ctrl Pts',(1.86484481102796,-3.71749299288145,19.4996902519957));
#25318=CARTESIAN_POINT('Ctrl Pts',(2.78946280422149,-2.79456220367197,19.552678540724));
#25319=CARTESIAN_POINT('Ctrl Pts',(3.714080797415,-1.8716314144625,19.6056668294522));
#25320=CARTESIAN_POINT('Ctrl Pts',(4.13521477262173,-0.444296191292658,
19.6586551181805));
#25321=CARTESIAN_POINT('Ctrl Pts',(3.85969347255442,0.832734618130101,19.7116434069087));
#25322=CARTESIAN_POINT('Ctrl Pts',(3.5841721724871,2.10976542755288,19.764631695637));
#25323=CARTESIAN_POINT('Ctrl Pts',(2.6119955971457,3.23649182322855,19.8176199843652));
#25324=CARTESIAN_POINT('Ctrl Pts',(1.38909445367046,3.69609215863147,19.8706082730935));
#25325=CARTESIAN_POINT('Ctrl Pts',(0.166193310195227,4.1556924940344,19.9235965618217));
#25326=CARTESIAN_POINT('Ctrl Pts',(-1.30743240141386,3.94816676916459,19.97658485055));
#25327=CARTESIAN_POINT('Ctrl Pts',(-2.35584070483748,3.16870560636289,20.0295731392782));
#25328=CARTESIAN_POINT('Ctrl Pts',(-3.33358701031412,2.44177958936821,20.0789900538223));
#25329=CARTESIAN_POINT('Ctrl Pts',(-3.94150300763008,1.21741613169822,20.1284069683663));
#25330=CARTESIAN_POINT('Ctrl Pts',(-3.94772619292891,-0.00158826883248112,
20.1778238829104));
#25331=CARTESIAN_POINT('Origin',(0.,0.,0.));
#25332=CARTESIAN_POINT('',(-3.94074044801927,0.00358039056613663,21.3221761170896));
#25333=CARTESIAN_POINT('',(-3.94238528018782,0.00360576479228953,21.1778238829104));
#25334=CARTESIAN_POINT('',(-3.942,-4.82755768223887E-16,0.));
#25335=CARTESIAN_POINT('Ctrl Pts',(-3.94074044801927,0.00358039056613663,
21.3221761170896));
#25336=CARTESIAN_POINT('Ctrl Pts',(-3.94382356658785,0.35139917714199,21.3081404896601));
#25337=CARTESIAN_POINT('Ctrl Pts',(-3.90159553870986,0.69848167363253,21.2941048622306));
#25338=CARTESIAN_POINT('Ctrl Pts',(-3.81110742902655,1.03248974691214,21.2800692348011));
#25339=CARTESIAN_POINT('Ctrl Pts',(-3.46964707612424,2.29288202357064,21.2271052563065));
#25340=CARTESIAN_POINT('Ctrl Pts',(-2.44098286072968,3.36709985140295,21.1741412778118));
#25341=CARTESIAN_POINT('Ctrl Pts',(-1.19655973690358,3.76282070551412,21.1211772993172));
#25342=CARTESIAN_POINT('Ctrl Pts',(0.0478633869225303,4.15854155962529,
21.0682133208226));
#25343=CARTESIAN_POINT('Ctrl Pts',(1.50804541918014,3.87576544001532,21.0152493423279));
#25344=CARTESIAN_POINT('Ctrl Pts',(2.51477344786687,3.04409088599763,20.9622853638333));
#25345=CARTESIAN_POINT('Ctrl Pts',(3.52150147655357,2.21241633197998,20.9093213853387));
#25346=CARTESIAN_POINT('Ctrl Pts',(4.07477550166942,0.831843343554564,20.8563574068441));
#25347=CARTESIAN_POINT('Ctrl Pts',(3.92102566715379,-0.464900607518139,
20.8033934283495));
#25348=CARTESIAN_POINT('Ctrl Pts',(3.76727583263815,-1.76164455859092,20.7504294498548));
#25349=CARTESIAN_POINT('Ctrl Pts',(2.90650213849103,-2.97455947231102,20.6974654713602));
#25350=CARTESIAN_POINT('Ctrl Pts',(1.73320395728241,-3.54775688148229,20.6445014928656));
#25351=CARTESIAN_POINT('Ctrl Pts',(0.559905776073817,-4.12095429065355,
20.5915375143709));
#25352=CARTESIAN_POINT('Ctrl Pts',(-0.925916892196226,-4.05443419527599,
20.5385735358763));
#25353=CARTESIAN_POINT('Ctrl Pts',(-2.04329981292238,-3.37868328145881,
20.4856095573817));
#25354=CARTESIAN_POINT('Ctrl Pts',(-3.16068273364853,-2.70293236764162,
20.4326455788871));
#25355=CARTESIAN_POINT('Ctrl Pts',(-3.90962590683076,-1.41795063538484,
20.3796816003925));
#25356=CARTESIAN_POINT('Ctrl Pts',(-3.94688277287076,-0.11265533735563,
20.3267176218978));
#25357=CARTESIAN_POINT('Ctrl Pts',(-3.94794766163145,-0.0753469311478099,
20.3252037869617));
#25358=CARTESIAN_POINT('Ctrl Pts',(-3.94843113776951,-0.0380219297583325,
20.3236899520257));
#25359=CARTESIAN_POINT('Ctrl Pts',(-3.94834041879863,-0.000694519400761262,
20.3221761170896));
#25360=CARTESIAN_POINT('Ctrl Pts',(-3.94772619292891,-0.00158826883248112,
20.1778238829104));
#25361=CARTESIAN_POINT('Ctrl Pts',(-3.94817594426456,-0.0896860565358013,
20.1813952570946));
#25362=CARTESIAN_POINT('Ctrl Pts',(-3.9454830581488,-0.177755853920253,
20.1849666312788));
#25363=CARTESIAN_POINT('Ctrl Pts',(-3.93956001409796,-0.265607871813588,
20.188538005463));
#25364=CARTESIAN_POINT('Ctrl Pts',(-3.85168012469672,-1.56906358645505,
20.2415262941912));
#25365=CARTESIAN_POINT('Ctrl Pts',(-3.05272945065598,-2.82457841500438,
20.2945145829195));
#25366=CARTESIAN_POINT('Ctrl Pts',(-1.90918116982076,-3.45625634279478,
20.3475028716477));
#25367=CARTESIAN_POINT('Ctrl Pts',(-0.765632888985623,-4.08793427058512,
20.4004911603759));
#25368=CARTESIAN_POINT('Ctrl Pts',(0.722512998643886,-4.09577529761664,
20.4534794491042));
#25369=CARTESIAN_POINT('Ctrl Pts',(1.87265421179595,-3.47618279865318,20.5064677378324));
#25370=CARTESIAN_POINT('Ctrl Pts',(3.0227954249481,-2.85659029968967,20.5594560265607));
#25371=CARTESIAN_POINT('Ctrl Pts',(3.8349319636227,-1.60956427473106,20.6124443152889));
#25372=CARTESIAN_POINT('Ctrl Pts',(3.9365423847422,-0.307106982824769,20.6654326040172));
#25373=CARTESIAN_POINT('Ctrl Pts',(4.03815280586171,0.995350309081448,20.7184208927454));
#25374=CARTESIAN_POINT('Ctrl Pts',(3.4292371094262,2.35323886793535,20.7714091814737));
#25375=CARTESIAN_POINT('Ctrl Pts',(2.38910073600262,3.14370455348999,20.8243974702019));
#25376=CARTESIAN_POINT('Ctrl Pts',(1.348964362579,3.93417023904466,20.8773857589302));
#25377=CARTESIAN_POINT('Ctrl Pts',(-0.12239268783275,4.15721305130006,20.9303740476584));
#25378=CARTESIAN_POINT('Ctrl Pts',(-1.35006905738725,3.71052478612394,20.9833623363867));
#25379=CARTESIAN_POINT('Ctrl Pts',(-2.57774542694174,3.26383652094782,21.0363506251149));
#25380=CARTESIAN_POINT('Ctrl Pts',(-3.56174111563901,2.14741717834018,21.0893389138432));
#25381=CARTESIAN_POINT('Ctrl Pts',(-3.85070407192177,0.873360631535526,
21.1423272025715));
#25382=CARTESIAN_POINT('Ctrl Pts',(-3.91522918325707,0.588865201437585,
21.1541594293511));
#25383=CARTESIAN_POINT('Ctrl Pts',(-3.94509829421553,0.296509601950098,
21.1659916561308));
#25384=CARTESIAN_POINT('Ctrl Pts',(-3.94238528018782,0.00360576479228953,
21.1778238829104));
#25385=CARTESIAN_POINT('Origin',(0.,0.,0.));
#25386=CARTESIAN_POINT('',(-3.93587951376728,-0.00124481178566893,22.3221761170896));
#25387=CARTESIAN_POINT('',(-3.93552176014147,-0.00030393483444853,22.1778238829104));
#25388=CARTESIAN_POINT('',(-3.942,-4.82755768223887E-16,0.));
#25389=CARTESIAN_POINT('Ctrl Pts',(-3.93587951376728,-0.00124481178566893,
22.3221761170896));
#25390=CARTESIAN_POINT('Ctrl Pts',(-3.9337992464037,0.734189273701127,22.2925910272945));
#25391=CARTESIAN_POINT('Ctrl Pts',(-3.73627980596971,1.47066093628887,22.2630059374994));
#25392=CARTESIAN_POINT('Ctrl Pts',(-3.35026562609245,2.08956860583238,22.2334208477043));
#25393=CARTESIAN_POINT('Ctrl Pts',(-2.65921324588212,3.19755282108702,22.1804568692097));
#25394=CARTESIAN_POINT('Ctrl Pts',(-1.36405277538343,3.92875538432108,22.1274928907151));
#25395=CARTESIAN_POINT('Ctrl Pts',(-0.0583683106578484,3.94805897547177,
22.0745289122204));
#25396=CARTESIAN_POINT('Ctrl Pts',(1.2473161540677,3.96736256662245,22.0215649337258));
#25397=CARTESIAN_POINT('Ctrl Pts',(2.56352461302015,3.27476718568979,21.9686009552312));
#25398=CARTESIAN_POINT('Ctrl Pts',(3.28702932421304,2.18769549882087,21.9156369767366));
#25399=CARTESIAN_POINT('Ctrl Pts',(4.01053403540591,1.10062381195199,21.8626729982419));
#25400=CARTESIAN_POINT('Ctrl Pts',(4.14133499883926,-0.380924180853135,
21.8097090197473));
#25401=CARTESIAN_POINT('Ctrl Pts',(3.6194845960222,-1.57794374981529,21.7567450412527));
#25402=CARTESIAN_POINT('Ctrl Pts',(3.09763419320511,-2.77496331877751,21.7037810627581));
#25403=CARTESIAN_POINT('Ctrl Pts',(1.92313242413752,-3.68745446389673,21.6508170842634));
#25404=CARTESIAN_POINT('Ctrl Pts',(0.634262969967227,-3.89721509840628,
21.5978531057688));
#25405=CARTESIAN_POINT('Ctrl Pts',(-0.654606484203027,-4.10697573291583,
21.5448891272742));
#25406=CARTESIAN_POINT('Ctrl Pts',(-2.05784362347597,-3.61400585681575,
21.4919251487796));
#25407=CARTESIAN_POINT('Ctrl Pts',(-2.93233394790743,-2.64423755602338,
21.4389611702849));
#25408=CARTESIAN_POINT('Ctrl Pts',(-3.57508147783416,-1.93146102491564,
21.4000328192198));
#25409=CARTESIAN_POINT('Ctrl Pts',(-3.93218930040467,-0.961108355901809,
21.3611044681547));
#25410=CARTESIAN_POINT('Ctrl Pts',(-3.94074044801927,0.00358039056613663,
21.3221761170896));
#25411=CARTESIAN_POINT('Ctrl Pts',(-3.94238528018782,0.00360576479228953,
21.1778238829104));
#25412=CARTESIAN_POINT('Ctrl Pts',(-3.93294859718036,-1.0152023337623,21.218979944859));
#25413=CARTESIAN_POINT('Ctrl Pts',(-3.52931423770067,-2.04064333351309,
21.2601360068076));
#25414=CARTESIAN_POINT('Ctrl Pts',(-2.81875615331693,-2.76501254901743,
21.3012920687562));
#25415=CARTESIAN_POINT('Ctrl Pts',(-1.90391505456104,-3.69763543176414,
21.3542803574844));
#25416=CARTESIAN_POINT('Ctrl Pts',(-0.480302633180845,-4.13118744625593,
21.4072686462127));
#25417=CARTESIAN_POINT('Ctrl Pts',(0.799079880925017,-3.86680126221775,
21.4602569349409));
#25418=CARTESIAN_POINT('Ctrl Pts',(2.07846239503088,-3.60241507817958,21.5132452236692));
#25419=CARTESIAN_POINT('Ctrl Pts',(3.21361500186243,-2.64009069561159,21.5662335123974));
#25420=CARTESIAN_POINT('Ctrl Pts',(3.68385102080785,-1.42123969585553,21.6192218011257));
#25421=CARTESIAN_POINT('Ctrl Pts',(4.15408703975328,-0.202388696099407,
21.6722100898539));
#25422=CARTESIAN_POINT('Ctrl Pts',(3.95940647081237,1.27298892084472,21.7251983785822));
#25423=CARTESIAN_POINT('Ctrl Pts',(3.18910793065139,2.32814760557936,21.7781866673104));
#25424=CARTESIAN_POINT('Ctrl Pts',(2.41880939049046,3.38330629031394,21.8311749560387));
#25425=CARTESIAN_POINT('Ctrl Pts',(1.07289287910942,4.01824604283911,21.8841632447669));
#25426=CARTESIAN_POINT('Ctrl Pts',(-0.231278918613751,3.94172434024104,
21.9371515334952));
#25427=CARTESIAN_POINT('Ctrl Pts',(-1.53545071633696,3.86520263764296,21.9901398222234));
#25428=CARTESIAN_POINT('Ctrl Pts',(-2.79787780040235,3.07721947992169,22.0431281109517));
#25429=CARTESIAN_POINT('Ctrl Pts',(-3.43949362875525,1.93921737114795,22.0961163996799));
#25430=CARTESIAN_POINT('Ctrl Pts',(-3.76928231599023,1.35428756589898,22.1233522274234));
#25431=CARTESIAN_POINT('Ctrl Pts',(-3.93505699138564,0.676885190519015,
22.1505880551669));
#25432=CARTESIAN_POINT('Ctrl Pts',(-3.93552176014147,-0.00030393483444853,
22.1778238829104));
#25433=CARTESIAN_POINT('Origin',(0.,0.,0.));
#25434=CARTESIAN_POINT('',(-3.94525314071248,-0.00295827654940184,23.3221761170896));
#25435=CARTESIAN_POINT('',(-3.94350653563855,-0.00347714007584369,23.1778238829104));
#25436=CARTESIAN_POINT('',(-3.942,-4.82755768223887E-16,0.));
#25437=CARTESIAN_POINT('Ctrl Pts',(-3.94525314071248,-0.00295827654940184,
23.3221761170896));
#25438=CARTESIAN_POINT('Ctrl Pts',(-3.93582062597525,1.11220231279806,23.2770415649289));
#25439=CARTESIAN_POINT('Ctrl Pts',(-3.44025122786987,2.23463092251658,23.2319070127682));
#25440=CARTESIAN_POINT('Ctrl Pts',(-2.60368934111206,2.9683990932166,23.1867724606075));
#25441=CARTESIAN_POINT('Ctrl Pts',(-1.62201025804696,3.82945298103697,23.1338084821129));
#25442=CARTESIAN_POINT('Ctrl Pts',(-0.170774803008089,4.15531037113838,
23.0808445036183));
#25443=CARTESIAN_POINT('Ctrl Pts',(1.08481479710351,3.79655919604497,23.0278805251236));
#25444=CARTESIAN_POINT('Ctrl Pts',(2.34040439721512,3.43780802095157,22.974916546629));
#25445=CARTESIAN_POINT('Ctrl Pts',(3.40034814239945,2.39444828066336,22.9219525681344));
#25446=CARTESIAN_POINT('Ctrl Pts',(3.77891236751962,1.14469612557038,22.8689885896398));
#25447=CARTESIAN_POINT('Ctrl Pts',(4.15747659263979,-0.105056029522605,
22.8160246111452));
#25448=CARTESIAN_POINT('Ctrl Pts',(3.85466129769578,-1.56120059942036,22.7630606326505));
#25449=CARTESIAN_POINT('Ctrl Pts',(3.00922455792002,-2.55639398676302,22.7100966541559));
#25450=CARTESIAN_POINT('Ctrl Pts',(2.16378781814425,-3.55158737410568,22.6571326756613));
#25451=CARTESIAN_POINT('Ctrl Pts',(0.77572963353673,-4.08582957889326,22.6041686971666));
#25452=CARTESIAN_POINT('Ctrl Pts',(-0.518779131279689,-3.91426327466899,
22.551204718672));
#25453=CARTESIAN_POINT('Ctrl Pts',(-1.81328789609611,-3.74269697044473,
22.4982407401774));
#25454=CARTESIAN_POINT('Ctrl Pts',(-3.01424724112142,-2.86532215720863,
22.4452767616828));
#25455=CARTESIAN_POINT('Ctrl Pts',(-3.57125476867308,-1.684251816953,22.3923127831882));
#25456=CARTESIAN_POINT('Ctrl Pts',(-3.81712408139379,-1.16291424345579,
22.3689338944886));
#25457=CARTESIAN_POINT('Ctrl Pts',(-3.9375233938263,-0.582403488318747,
22.3455550057891));
#25458=CARTESIAN_POINT('Ctrl Pts',(-3.93587951376728,-0.00124481178566893,
22.3221761170896));
#25459=CARTESIAN_POINT('Ctrl Pts',(-3.93552176014147,-0.00030393483444853,
22.1778238829104));
#25460=CARTESIAN_POINT('Ctrl Pts',(-3.93596121582331,-0.640610765021898,
22.2035763438952));
#25461=CARTESIAN_POINT('Ctrl Pts',(-3.78860721752551,-1.28072694143294,
22.2293288048799));
#25462=CARTESIAN_POINT('Ctrl Pts',(-3.49236428582461,-1.84230088118771,
22.2550812658647));
#25463=CARTESIAN_POINT('Ctrl Pts',(-2.88281454190065,-2.99779596492355,
22.3080695545929));
#25464=CARTESIAN_POINT('Ctrl Pts',(-1.64291048141232,-3.82076507256913,
22.3610578433212));
#25465=CARTESIAN_POINT('Ctrl Pts',(-0.341387846963322,-3.93371775192091,
22.4140461320494));
#25466=CARTESIAN_POINT('Ctrl Pts',(0.96013478748571,-4.04667043127269,22.4670344207777));
#25467=CARTESIAN_POINT('Ctrl Pts',(2.3232759958954,-3.44960668233064,22.5200227095059));
#25468=CARTESIAN_POINT('Ctrl Pts',(3.12277281794346,-2.41639589080571,22.5730109982342));
#25469=CARTESIAN_POINT('Ctrl Pts',(3.92226963999152,-1.38318509928078,22.6259992869624));
#25470=CARTESIAN_POINT('Ctrl Pts',(4.15812207567794,0.0861727348270178,
22.6789875756907));
#25471=CARTESIAN_POINT('Ctrl Pts',(3.72214521454942,1.31769395259273,22.7319758644189));
#25472=CARTESIAN_POINT('Ctrl Pts',(3.28616835342092,2.5492151703584,22.7849641531472));
#25473=CARTESIAN_POINT('Ctrl Pts',(2.17836219547751,3.54289977178199,22.8379524418754));
#25474=CARTESIAN_POINT('Ctrl Pts',(0.906871753871591,3.84295018391872,22.8909407306037));
#25475=CARTESIAN_POINT('Ctrl Pts',(-0.364618687734369,4.14300059605545,
22.9439290193319));
#25476=CARTESIAN_POINT('Ctrl Pts',(-1.79979341300285,3.74941681890528,22.9969173080602));
#25477=CARTESIAN_POINT('Ctrl Pts',(-2.74035137198678,2.84273547234742,23.0499055967884));
#25478=CARTESIAN_POINT('Ctrl Pts',(-3.49721397313409,2.11313322315816,23.0925450254957));
#25479=CARTESIAN_POINT('Ctrl Pts',(-3.9337951138205,1.05128255440302,23.1351844542031));
#25480=CARTESIAN_POINT('Ctrl Pts',(-3.94350653563855,-0.00347714007584369,
23.1778238829104));
#25481=CARTESIAN_POINT('Origin',(0.,0.,-1.84858989190503));
#25482=CARTESIAN_POINT('',(-3.37453254114594,-0.00253033205341837,23.651410108095));
#25483=CARTESIAN_POINT('',(-3.37610896110192,0.00188753811008129,23.848589891905));
#25484=CARTESIAN_POINT('',(-3.37175,2.08693528006523E-13,-1.84858989190503));
#25485=CARTESIAN_POINT('',(-3.33611311329475,0.488924695431507,24.62825));
#25486=CARTESIAN_POINT('Ctrl Pts',(-3.37453254114594,-0.00253033205341877,
23.651410108095));
#25487=CARTESIAN_POINT('Ctrl Pts',(-3.37593208671392,-0.167991834513083,
23.6592395344289));
#25488=CARTESIAN_POINT('Ctrl Pts',(-3.28964411790747,-1.45130369571974,
23.7200329392575));
#25489=CARTESIAN_POINT('Ctrl Pts',(-1.64345961820725,-3.63211696072943,
23.8337903225806));
#25490=CARTESIAN_POINT('Ctrl Pts',(2.163389782855,-3.34808861530533,23.9926822580645));
#25491=CARTESIAN_POINT('Ctrl Pts',(3.98513370400483,0.0032270738820094,
24.1515741935484));
#25492=CARTESIAN_POINT('Ctrl Pts',(2.15811323746268,3.35470758430291,24.3104661290323));
#25493=CARTESIAN_POINT('Ctrl Pts',(-1.65524532662936,3.62504834974875,24.4693580645161));
#25494=CARTESIAN_POINT('Ctrl Pts',(-3.1734075349997,1.59912472915632,24.5752860215054));
#25495=CARTESIAN_POINT('Ctrl Pts',(-3.33611311329483,0.488924695430968,
24.62825));
#25496=CARTESIAN_POINT('',(-0.624728334461187,3.31336876465952,24.62825));
#25497=CARTESIAN_POINT('Origin',(0.,0.,24.62825));
#25498=CARTESIAN_POINT('Ctrl Pts',(-3.37610896110192,0.00188753811008135,
23.848589891905));
#25499=CARTESIAN_POINT('Ctrl Pts',(-3.36932955763165,-1.01002015324007,
23.8965234396903));
#25500=CARTESIAN_POINT('Ctrl Pts',(-2.34697770975975,-3.15243101165571,
23.997445276204));
#25501=CARTESIAN_POINT('Ctrl Pts',(1.29650641132588,-3.76899081084458,24.1513554014457));
#25502=CARTESIAN_POINT('Ctrl Pts',(3.87454091099827,-0.951014904317504,
24.3103202676305));
#25503=CARTESIAN_POINT('Ctrl Pts',(2.88961752940844,2.74513957150359,24.4692851338152));
#25504=CARTESIAN_POINT('Ctrl Pts',(0.478408881098333,3.52136284087264,24.5752617112718));
#25505=CARTESIAN_POINT('Ctrl Pts',(-0.624728334461281,3.3133687646595,24.62825));
#25506=CARTESIAN_POINT('Origin',(0.,0.,-1.84858989190503));
#25507=CARTESIAN_POINT('',(-3.36651490374044,-0.00106473722420811,22.651410108095));
#25508=CARTESIAN_POINT('',(-3.37303860008607,-0.00297413674536479,22.848589891905));
#25509=CARTESIAN_POINT('',(-3.37175,2.08693528006523E-13,-1.84858989190503));
#25510=CARTESIAN_POINT('Ctrl Pts',(-3.36651490374044,-0.00106473722420751,
22.651410108095));
#25511=CARTESIAN_POINT('Ctrl Pts',(-3.36792097999337,-0.498152958330381,
22.6747889967945));
#25512=CARTESIAN_POINT('Ctrl Pts',(-3.03163608822923,-2.11956584279889,
22.7511318639887));
#25513=CARTESIAN_POINT('Ctrl Pts',(-0.52374905937927,-3.95173187129016,
22.8804387096774));
#25514=CARTESIAN_POINT('Ctrl Pts',(3.03803570770629,-2.58085580280275,23.0393306451613));
#25515=CARTESIAN_POINT('Ctrl Pts',(3.81506574631169,1.15563997615671,23.1982225806452));
#25516=CARTESIAN_POINT('Ctrl Pts',(1.095229123157,3.83292171460177,23.357114516129));
#25517=CARTESIAN_POINT('Ctrl Pts',(-2.44517403763626,3.03796695389969,23.508177025279));
#25518=CARTESIAN_POINT('Ctrl Pts',(-3.36646453466052,0.951311047229191,
23.6062755559343));
#25519=CARTESIAN_POINT('Ctrl Pts',(-3.37453254114594,-0.00253033205341877,
23.651410108095));
#25520=CARTESIAN_POINT('Ctrl Pts',(-3.37303860008607,-0.00297413674536527,
22.848589891905));
#25521=CARTESIAN_POINT('Ctrl Pts',(-3.3750546565899,-0.221938484280555,
22.8589387519259));
#25522=CARTESIAN_POINT('Ctrl Pts',(-3.25576106932785,-1.5598586434856,22.9222759006751));
#25523=CARTESIAN_POINT('Ctrl Pts',(-1.46739644894177,-3.70704069007233,
23.0386013381526));
#25524=CARTESIAN_POINT('Ctrl Pts',(2.32262200499063,-3.24046036848089,23.1975662043372));
#25525=CARTESIAN_POINT('Ctrl Pts',(3.98198637087808,0.198816238648098,23.3565310705221));
#25526=CARTESIAN_POINT('Ctrl Pts',(1.98816433058814,3.45581133218519,23.5154959367067));
#25527=CARTESIAN_POINT('Ctrl Pts',(-1.82925354411967,3.5422830008711,23.6744608028915));
#25528=CARTESIAN_POINT('Ctrl Pts',(-3.3238940749889,1.33320070540347,23.7854921212909));
#25529=CARTESIAN_POINT('Ctrl Pts',(-3.37682387017652,0.108596335481547,
23.8435351509621));
#25530=CARTESIAN_POINT('Ctrl Pts',(-3.37610896110192,0.00188753811008135,
23.848589891905));
#25531=CARTESIAN_POINT('Origin',(0.,0.,-1.84858989190503));
#25532=CARTESIAN_POINT('',(-3.37067265489827,0.00306245101284196,21.651410108095));
#25533=CARTESIAN_POINT('',(-3.36620890277955,-0.000259967599581801,21.848589891905));
#25534=CARTESIAN_POINT('',(-3.37175,2.08693528006523E-13,-1.84858989190503));
#25535=CARTESIAN_POINT('Ctrl Pts',(-3.37067265489827,0.00306245101284172,
21.651410108095));
#25536=CARTESIAN_POINT('Ctrl Pts',(-3.36335851690506,-0.822074352869367,
21.6903384591601));
#25537=CARTESIAN_POINT('Ctrl Pts',(-2.64233179033033,-2.78128712935246,
21.7822307887199));
#25538=CARTESIAN_POINT('Ctrl Pts',(0.640333691332285,-3.93451715048184,
21.9270870967742));
#25539=CARTESIAN_POINT('Ctrl Pts',(3.6541284705207,-1.59304681672573,22.0859790322581));
#25540=CARTESIAN_POINT('Ctrl Pts',(3.31849061020388,2.20863464806944,22.2448709677419));
#25541=CARTESIAN_POINT('Ctrl Pts',(-0.058926339166703,3.98584809986529,
22.4037629032258));
#25542=CARTESIAN_POINT('Ctrl Pts',(-2.89333741463138,2.3856381715614,22.5392759500101));
#25543=CARTESIAN_POINT('Ctrl Pts',(-3.36473556800141,0.627981401218202,
22.6218250182999));
#25544=CARTESIAN_POINT('Ctrl Pts',(-3.36651490374044,-0.00106473722420751,
22.651410108095));
#25545=CARTESIAN_POINT('Ctrl Pts',(-3.36620890277955,-0.00025996759958187,
21.848589891905));
#25546=CARTESIAN_POINT('Ctrl Pts',(-3.36658478677126,-0.547939966251195,
21.8743423528898));
#25547=CARTESIAN_POINT('Ctrl Pts',(-2.98121161418831,-2.22202824736231,
21.9530831026028));
#25548=CARTESIAN_POINT('Ctrl Pts',(-0.344707483447601,-3.97197126386073,
22.0848121410441));
#25549=CARTESIAN_POINT('Ctrl Pts',(3.15313982968432,-2.43989387002868,22.2437770072288));
#25550=CARTESIAN_POINT('Ctrl Pts',(3.75834184644668,1.33050740634341,22.4027418734136));
#25551=CARTESIAN_POINT('Ctrl Pts',(0.915689325102905,3.88032175554439,22.5617067395983));
#25552=CARTESIAN_POINT('Ctrl Pts',(-2.52724878310966,2.93612690507347,22.7103227457621));
#25553=CARTESIAN_POINT('Ctrl Pts',(-3.36473203323799,0.899203945410642,
22.8059504631977));
#25554=CARTESIAN_POINT('Ctrl Pts',(-3.37303860008607,-0.00297413674536527,
22.848589891905));
#25555=CARTESIAN_POINT('Origin',(0.,0.,-1.84858989190503));
#25556=CARTESIAN_POINT('',(-3.37717321336486,-0.000594050174885632,20.651410108095));
#25557=CARTESIAN_POINT('',(-3.37207954552848,0.0030841546013495,20.848589891905));
#25558=CARTESIAN_POINT('',(-3.37175,2.08693528006523E-13,-1.84858989190503));
#25559=CARTESIAN_POINT('Ctrl Pts',(-3.37717321336486,-0.000594050174885286,
20.651410108095));
#25560=CARTESIAN_POINT('Ctrl Pts',(-3.37725080892297,-0.0325216746987667,
20.6529239430311));
#25561=CARTESIAN_POINT('Ctrl Pts',(-3.36236902703727,-1.18141504466881,
20.7074017564618));
#25562=CARTESIAN_POINT('Ctrl Pts',(-2.06285714434356,-3.41102216294582,
20.8148435483871));
#25563=CARTESIAN_POINT('Ctrl Pts',(1.74979322227715,-3.58171404391184,20.9737354838709));
#25564=CARTESIAN_POINT('Ctrl Pts',(3.95855555351044,-0.46935037546761,21.1326274193549));
#25565=CARTESIAN_POINT('Ctrl Pts',(2.53884345747981,3.07322723010567,21.2915193548387));
#25566=CARTESIAN_POINT('Ctrl Pts',(-1.20801252978399,3.79883634829061,21.4504112903226));
#25567=CARTESIAN_POINT('Ctrl Pts',(-3.20089281760442,1.71770287259066,21.5703748747413));
#25568=CARTESIAN_POINT('Ctrl Pts',(-3.3733097693157,0.300565747216989,21.6373744806655));
#25569=CARTESIAN_POINT('Ctrl Pts',(-3.37067265489827,0.00306245101284172,
21.651410108095));
#25570=CARTESIAN_POINT('Ctrl Pts',(-3.37207954552848,0.00308415460134954,
20.848589891905));
#25571=CARTESIAN_POINT('Ctrl Pts',(-3.36400797375518,-0.868343092050458,
20.8897459538536));
#25572=CARTESIAN_POINT('Ctrl Pts',(-2.57426217007386,-2.87470778191459,
20.9838903045305));
#25573=CARTESIAN_POINT('Ctrl Pts',(0.806850527235046,-3.9044039261228,21.1310229439355));
#25574=CARTESIAN_POINT('Ctrl Pts',(3.71967457752779,-1.43506051902692,21.2899878101203));
#25575=CARTESIAN_POINT('Ctrl Pts',(3.22012038549849,2.35078763921597,21.448952676305));
#25576=CARTESIAN_POINT('Ctrl Pts',(-0.233528014234224,3.98005560769136,
21.6079175424898));
#25577=CARTESIAN_POINT('Ctrl Pts',(-2.94815289437509,2.2856379957105,21.7411299476898));
#25578=CARTESIAN_POINT('Ctrl Pts',(-3.36581136750493,0.578966930779549,
21.8213540641615));
#25579=CARTESIAN_POINT('Ctrl Pts',(-3.36620890277955,-0.00025996759958187,
21.848589891905));
#25580=CARTESIAN_POINT('Origin',(0.,0.,-1.84858989190503));
#25581=CARTESIAN_POINT('',(-3.36891084971013,-0.00271891470300727,19.651410108095));
#25582=CARTESIAN_POINT('',(-3.37664784145308,-0.00135850975013785,19.848589891905));
#25583=CARTESIAN_POINT('',(-3.37175,2.08693528006523E-13,-1.84858989190503));
#25584=CARTESIAN_POINT('Ctrl Pts',(-3.36891084971013,-0.00271891470300756,
19.651410108095));
#25585=CARTESIAN_POINT('Ctrl Pts',(-3.3716487661365,-0.364876698157186,
19.6684734053967));
#25586=CARTESIAN_POINT('Ctrl Pts',(-3.15091588331813,-1.84791316659487,
19.738500681193));
#25587=CARTESIAN_POINT('Ctrl Pts',(-0.989363022110038,-3.86155572506565,
19.8614919354839));
#25588=CARTESIAN_POINT('Ctrl Pts',(2.71000466929749,-2.92341008068914,20.0203838709678));
#25589=CARTESIAN_POINT('Ctrl Pts',(3.92533937020224,0.694379317983201,20.1792758064516));
#25590=CARTESIAN_POINT('Ctrl Pts',(1.54264613898669,3.6756896897871,20.3381677419355));
#25591=CARTESIAN_POINT('Ctrl Pts',(-2.21788792003282,3.29150051432633,20.4955458424833));
#25592=CARTESIAN_POINT('Ctrl Pts',(-3.37453600206181,1.08451822071036,20.5999599645364));
#25593=CARTESIAN_POINT('Ctrl Pts',(-3.37717321336486,-0.000594050174885286,
20.651410108095));
#25594=CARTESIAN_POINT('Ctrl Pts',(-3.37664784145308,-0.0013585097501378,
19.848589891905));
#25595=CARTESIAN_POINT('Ctrl Pts',(-3.37703253172857,-0.0767120652268113,
19.8521612660892));
#25596=CARTESIAN_POINT('Ctrl Pts',(-3.3405547692736,-1.26970315744226,19.9087209290016));
#25597=CARTESIAN_POINT('Ctrl Pts',(-1.92774697870435,-3.4898666651324,20.0182688806423));
#25598=CARTESIAN_POINT('Ctrl Pts',(1.89086481476229,-3.50998689564495,20.1772337468271));
#25599=CARTESIAN_POINT('Ctrl Pts',(3.97482324267393,-0.310093440809367,
20.3361986130118));
#25600=CARTESIAN_POINT('Ctrl Pts',(2.41233351706024,3.17427546962878,20.4951634791965));
#25601=CARTESIAN_POINT('Ctrl Pts',(-1.36319778790607,3.74660773920425,20.6541283453813));
#25602=CARTESIAN_POINT('Ctrl Pts',(-3.23443909431523,1.62353950510727,20.7719371496175));
#25603=CARTESIAN_POINT('Ctrl Pts',(-3.37440009475423,0.25361650187097,20.8367576651254));
#25604=CARTESIAN_POINT('Ctrl Pts',(-3.37207954552848,0.00308415460134954,
20.848589891905));
#25605=CARTESIAN_POINT('Origin',(0.,0.,-1.84858989190503));
#25606=CARTESIAN_POINT('',(-3.36739896644089,0.00198349937115513,18.651410108095));
#25607=CARTESIAN_POINT('',(-3.36796573513472,-0.00233887403243982,18.848589891905));
#25608=CARTESIAN_POINT('',(-3.37175,2.08693528006523E-13,-1.84858989190503));
#25609=CARTESIAN_POINT('Ctrl Pts',(-3.36739896644089,0.00198349937115483,
18.651410108095));
#25610=CARTESIAN_POINT('Ctrl Pts',(-3.36368984329845,-0.690983280694315,
18.6840228677623));
#25611=CARTESIAN_POINT('Ctrl Pts',(-2.81781374229535,-2.51470704523694,
18.7695996059241));
#25612=CARTESIAN_POINT('Ctrl Pts',(0.168518449156949,-3.98271933982683,
18.9081403225806));
#25613=CARTESIAN_POINT('Ctrl Pts',(3.43906728250426,-2.01575495384355,19.0670322580645));
#25614=CARTESIAN_POINT('Ctrl Pts',(3.55731284355299,1.79888219198906,19.2259241935484));
#25615=CARTESIAN_POINT('Ctrl Pts',(0.41486938743375,3.96463556949202,19.3848161290323));
#25616=CARTESIAN_POINT('Ctrl Pts',(-2.72954745140897,2.65402060505441,19.5266447672144));
#25617=CARTESIAN_POINT('Ctrl Pts',(-3.36315035318836,0.75925052739643,19.615509426902));
#25618=CARTESIAN_POINT('Ctrl Pts',(-3.36891084971013,-0.00271891470300756,
19.651410108095));
#25619=CARTESIAN_POINT('Ctrl Pts',(-3.36796573513472,-0.00233887403243996,
18.848589891905));
#25620=CARTESIAN_POINT('Ctrl Pts',(-3.37053511298134,-0.405354963155371,
18.867564867053));
#25621=CARTESIAN_POINT('Ctrl Pts',(-3.11694291466331,-1.93068155902232,
18.9395281309293));
#25622=CARTESIAN_POINT('Ctrl Pts',(-0.847949117405149,-3.89568479841959,
19.0644796835338));
#25623=CARTESIAN_POINT('Ctrl Pts',(2.81658890100978,-2.82173788950715,19.2234445497186));
#25624=CARTESIAN_POINT('Ctrl Pts',(3.89722701433046,0.840832535700663,19.3824094159033));
#25625=CARTESIAN_POINT('Ctrl Pts',(1.40260268563389,3.73203476143841,19.5413742820881));
#25626=CARTESIAN_POINT('Ctrl Pts',(-2.29379652508948,3.21148336255172,19.6967677740886));
#25627=CARTESIAN_POINT('Ctrl Pts',(-3.37132490258154,1.04130462761393,19.799172977361));
#25628=CARTESIAN_POINT('Ctrl Pts',(-3.37664784145308,-0.0013585097501378,
19.848589891905));
#25629=CARTESIAN_POINT('Origin',(0.,0.,-1.84858989190503));
#25630=CARTESIAN_POINT('',(-3.3761529784003,0.00176635805113218,17.651410108095));
#25631=CARTESIAN_POINT('',(-3.36813340603362,0.00242210091315795,17.848589891905));
#25632=CARTESIAN_POINT('',(-3.37175,2.08693528006523E-13,-1.84858989190503));
#25633=CARTESIAN_POINT('Ctrl Pts',(-3.3761529784003,0.00176635805113214,
17.651410108095));
#25634=CARTESIAN_POINT('Ctrl Pts',(-3.36968839136432,-1.01481764775316,
17.6995723301278));
#25635=CARTESIAN_POINT('Ctrl Pts',(-2.33957623769215,-3.16069067030928,
17.8006985306553));
#25636=CARTESIAN_POINT('Ctrl Pts',(1.31202620257783,-3.7641784032229,17.9547887096774));
#25637=CARTESIAN_POINT('Ctrl Pts',(3.87479594250582,-0.936166764781103,
18.1136806451613));
#25638=CARTESIAN_POINT('Ctrl Pts',(2.88586665310525,2.74995008464444,18.2725725806452));
#25639=CARTESIAN_POINT('Ctrl Pts',(-0.748293493014444,3.91541934610488,
18.431464516129));
#25640=CARTESIAN_POINT('Ctrl Pts',(-3.09142162050251,1.98937278233,18.5577436919457));
#25641=CARTESIAN_POINT('Ctrl Pts',(-3.36971355672701,0.434412975597321,
18.6310588892676));
#25642=CARTESIAN_POINT('Ctrl Pts',(-3.36739896644089,0.00198349937115483,
18.651410108095));
#25643=CARTESIAN_POINT('Ctrl Pts',(-3.36813340603362,0.00242210091315778,
17.848589891905));
#25644=CARTESIAN_POINT('Ctrl Pts',(-3.36329734613199,-0.727665112355139,
17.8829684680169));
#25645=CARTESIAN_POINT('Ctrl Pts',(-2.77110248260437,-2.59019431375764,
17.970335332857));
#25646=CARTESIAN_POINT('Ctrl Pts',(0.302833216085013,-3.97538297495793,
18.1106904864254));
#25647=CARTESIAN_POINT('Ctrl Pts',(3.5065275226793,-1.89727238082542,18.2696553526101));
#25648=CARTESIAN_POINT('Ctrl Pts',(3.49338172535042,1.92136979140851,18.4286202187948));
#25649=CARTESIAN_POINT('Ctrl Pts',(0.275455597698851,3.97737375262188,18.5875850849796));
#25650=CARTESIAN_POINT('Ctrl Pts',(-2.78089559275923,2.57471376007135,18.7275749760163));
#25651=CARTESIAN_POINT('Ctrl Pts',(-3.36336003453583,0.720081709408907,
18.8145765783248));
#25652=CARTESIAN_POINT('Ctrl Pts',(-3.36796573513472,-0.00233887403243996,
18.848589891905));
#25653=CARTESIAN_POINT('Origin',(0.,0.,-1.84858989190503));
#25654=CARTESIAN_POINT('',(-3.37277477193024,-0.0030073171892592,16.651410108095));
#25655=CARTESIAN_POINT('',(-3.37676993930056,0.00122898291704077,16.848589891905));
#25656=CARTESIAN_POINT('',(-3.37175,2.08693528006523E-13,-1.84858989190503));
#25657=CARTESIAN_POINT('Ctrl Pts',(-3.37277477193024,-0.0030073171892591,
16.651410108095));
#25658=CARTESIAN_POINT('Ctrl Pts',(-3.3748752325093,-0.230456048008689,
16.6621578139988));
#25659=CARTESIAN_POINT('Ctrl Pts',(-3.25015286697033,-1.5764664391,16.7258694983973));
#25660=CARTESIAN_POINT('Ctrl Pts',(-1.44097876042837,-3.71672329068694,
16.8425451612903));
#25661=CARTESIAN_POINT('Ctrl Pts',(2.34362517346463,-3.22457328244272,17.0014370967742));
#25662=CARTESIAN_POINT('Ctrl Pts',(3.980025336833,0.223271417131382,17.1603290322581));
#25663=CARTESIAN_POINT('Ctrl Pts',(1.96827154957251,3.46646201691059,17.3192209677419));
#25664=CARTESIAN_POINT('Ctrl Pts',(-1.84763096082072,3.53223889907763,17.4781129032258));
#25665=CARTESIAN_POINT('Ctrl Pts',(-3.32665838484882,1.32176305576882,17.5888426166768));
#25666=CARTESIAN_POINT('Ctrl Pts',(-3.3767974954359,0.103119423021283,17.6466083516332));
#25667=CARTESIAN_POINT('Ctrl Pts',(-3.3761529784003,0.00176635805113214,
17.651410108095));
#25668=CARTESIAN_POINT('Ctrl Pts',(-3.37676993930056,0.00122898291704094,
16.848589891905));
#25669=CARTESIAN_POINT('Ctrl Pts',(-3.37185165056191,-1.0490400428621,16.8983720689807));
#25670=CARTESIAN_POINT('Ctrl Pts',(-2.28032799824397,-3.22603625281427,
17.0011425347847));
#25671=CARTESIAN_POINT('Ctrl Pts',(1.42826443406275,-3.7222894112013,17.1569012893169));
#25672=CARTESIAN_POINT('Ctrl Pts',(3.90292376012977,-0.813980268166524,
17.3158661555016));
#25673=CARTESIAN_POINT('Ctrl Pts',(2.79709452794753,2.84106317354542,17.4748310216864));
#25674=CARTESIAN_POINT('Ctrl Pts',(-0.87475073969136,3.88975434928213,17.6337958878711));
#25675=CARTESIAN_POINT('Ctrl Pts',(-3.12356865319579,1.91496539554474,17.758382177944));
#25676=CARTESIAN_POINT('Ctrl Pts',(-3.37075124816507,0.397630825661392,
17.8299801792886));
#25677=CARTESIAN_POINT('Ctrl Pts',(-3.36813340603362,0.00242210091315778,
17.848589891905));
#25678=CARTESIAN_POINT('Origin',(0.,0.,-1.84858989190503));
#25679=CARTESIAN_POINT('',(-3.36620324934232,-6.47284927745773E-5,15.651410108095));
#25680=CARTESIAN_POINT('',(-3.37184361771993,-0.00309624629213801,15.848589891905));
#25681=CARTESIAN_POINT('',(-3.37175,2.08693528006523E-13,-1.84858989190503));
#25682=CARTESIAN_POINT('Ctrl Pts',(-3.36620324934232,-6.47284927745434E-5,
15.651410108095));
#25683=CARTESIAN_POINT('Ctrl Pts',(-3.36629886637731,-0.559331950050314,
15.6777072763644));
#25684=CARTESIAN_POINT('Ctrl Pts',(-2.969304704679,-2.24486717295088,15.7569684231284));
#25685=CARTESIAN_POINT('Ctrl Pts',(-0.30568234557457,-3.97454527098943,
15.8891935483871));
#25686=CARTESIAN_POINT('Ctrl Pts',(3.17532551476257,-2.40992939374543,16.048085483871));
#25687=CARTESIAN_POINT('Ctrl Pts',(3.74577996379122,1.36366574731522,16.2069774193548));
#25688=CARTESIAN_POINT('Ctrl Pts',(0.882793462927545,3.88730337243608,16.3658693548387));
#25689=CARTESIAN_POINT('Ctrl Pts',(-2.54098403241842,2.91809266432718,16.5140135844188));
#25690=CARTESIAN_POINT('Ctrl Pts',(-3.36452430274498,0.890396140872364,
16.6091938355042));
#25691=CARTESIAN_POINT('Ctrl Pts',(-3.37277477193024,-0.0030073171892591,
16.651410108095));
#25692=CARTESIAN_POINT('Ctrl Pts',(-3.37184361771993,-0.00309624629213769,
15.848589891905));
#25693=CARTESIAN_POINT('Ctrl Pts',(-3.37422938253555,-0.261408813023958,
15.8607873812163));
#25694=CARTESIAN_POINT('Ctrl Pts',(-3.22903130121081,-1.63922767409008,
15.9259731592558));
#25695=CARTESIAN_POINT('Ctrl Pts',(-1.33737014962086,-3.75590452983738,
16.0441472260236));
#25696=CARTESIAN_POINT('Ctrl Pts',(2.43413116992486,-3.15759136082396,16.2031120922084));
#25697=CARTESIAN_POINT('Ctrl Pts',(3.97259404474729,0.337452678146523,16.3620769583931));
#25698=CARTESIAN_POINT('Ctrl Pts',(1.86665380078734,3.52292227310739,16.5210418245779));
#25699=CARTESIAN_POINT('Ctrl Pts',(-1.95172895721992,3.47651144567355,16.6800066907626));
#25700=CARTESIAN_POINT('Ctrl Pts',(-3.34455787065121,1.25410828714709,16.7891893798717));
#25701=CARTESIAN_POINT('Ctrl Pts',(-3.37708669087234,0.0688692501706657,
16.8453837802525));
#25702=CARTESIAN_POINT('Ctrl Pts',(-3.37676993930056,0.00122898291704094,
16.848589891905));
#25703=CARTESIAN_POINT('Origin',(0.,0.,-1.84858989190503));
#25704=CARTESIAN_POINT('',(-3.37253669875649,0.00303677565441225,14.651410108095));
#25705=CARTESIAN_POINT('',(-3.36623102492646,0.000387483300791081,14.848589891905));
#25706=CARTESIAN_POINT('',(-3.37175,2.08693528006523E-13,-1.84858989190503));
#25707=CARTESIAN_POINT('Ctrl Pts',(-3.37253669875649,0.00303677565441206,
14.651410108095));
#25708=CARTESIAN_POINT('Ctrl Pts',(-3.36433888251516,-0.882704764956481,
14.69325673873));
#25709=CARTESIAN_POINT('Ctrl Pts',(-2.55272847437535,-2.90279523765218,
14.7880673478596));
#25710=CARTESIAN_POINT('Ctrl Pts',(0.8556871302199,-3.8933599040824,14.9358419354839));
#25711=CARTESIAN_POINT('Ctrl Pts',(3.73618765800463,-1.38973148187494,15.0947338709677));
#25712=CARTESIAN_POINT('Ctrl Pts',(3.19203969455987,2.38774671937678,15.2536258064516));
#25713=CARTESIAN_POINT('Ctrl Pts',(-0.277982160818163,3.97657864574653,
15.4125177419355));
#25714=CARTESIAN_POINT('Ctrl Pts',(-2.9610712487067,2.26071800063538,15.54511250915));
#25715=CARTESIAN_POINT('Ctrl Pts',(-3.3661062882817,0.567063743655371,15.6247432978698));
#25716=CARTESIAN_POINT('Ctrl Pts',(-3.36620324934232,-6.47284927745434E-5,
15.651410108095));
#25717=CARTESIAN_POINT('Ctrl Pts',(-3.36623102492646,0.000387483300790976,
14.848589891905));
#25718=CARTESIAN_POINT('Ctrl Pts',(-3.36563039823437,-0.58659786734821,
14.8761909821801));
#25719=CARTESIAN_POINT('Ctrl Pts',(-2.93982168940875,-2.30128717837213,
14.9567803611835));
#25720=CARTESIAN_POINT('Ctrl Pts',(-0.206119829211681,-3.98156908396121,
15.0903580289152));
#25721=CARTESIAN_POINT('Ctrl Pts',(3.23622917375625,-2.32856146349605,15.2493228950999));
#25722=CARTESIAN_POINT('Ctrl Pts',(3.70970605913983,1.46063640552025,15.4082877612846));
#25723=CARTESIAN_POINT('Ctrl Pts',(0.779949646731194,3.90986653262151,15.5672526274694));
#25724=CARTESIAN_POINT('Ctrl Pts',(-2.58561751919903,2.85952988987219,15.7140200043429));
#25725=CARTESIAN_POINT('Ctrl Pts',(-3.36386515169579,0.8607517004072,15.8077990924881));
#25726=CARTESIAN_POINT('Ctrl Pts',(-3.37184361771993,-0.00309624629213769,
15.848589891905));
#25727=CARTESIAN_POINT('Origin',(0.,0.,-1.84858989190503));
#25728=CARTESIAN_POINT('',(-3.37630962516523,-0.00164737155311467,13.651410108095));
#25729=CARTESIAN_POINT('',(-3.37326960455653,0.00293423317535069,13.848589891905));
#25730=CARTESIAN_POINT('',(-3.37175,2.08693528006523E-13,-1.84858989190503));
#25731=CARTESIAN_POINT('Ctrl Pts',(-3.37630962516523,-0.00164737155311456,
13.651410108095));
#25732=CARTESIAN_POINT('Ctrl Pts',(-3.3768714611022,-0.0951867578458431,
13.6558422226009));
#25733=CARTESIAN_POINT('Ctrl Pts',(-3.33090125004588,-1.30596569148795,
13.7132383156015));
#25734=CARTESIAN_POINT('Ctrl Pts',(-1.87219709398698,-3.51927973437849,
13.8235983870968));
#25735=CARTESIAN_POINT('Ctrl Pts',(1.94407109338865,-3.48009186536664,13.9824903225806));
#25736=CARTESIAN_POINT('Ctrl Pts',(3.97837307717912,-0.25099694483561,14.1413822580645));
#25737=CARTESIAN_POINT('Ctrl Pts',(2.36603559757979,3.20816573115008,14.3002741935484));
#25738=CARTESIAN_POINT('Ctrl Pts',(-1.41504740048591,3.7266731359107,14.4591661290323));
#25739=CARTESIAN_POINT('Ctrl Pts',(-3.24486867351568,1.59233323105557,14.5762114338811));
#25740=CARTESIAN_POINT('Ctrl Pts',(-3.37471460348768,0.238350746486947,
14.6402927602354));
#25741=CARTESIAN_POINT('Ctrl Pts',(-3.37253669875649,0.00303677565441206,
14.651410108095));
#25742=CARTESIAN_POINT('Ctrl Pts',(-3.37326960455653,0.00293423317535065,
13.848589891905));
#25743=CARTESIAN_POINT('Ctrl Pts',(-3.36494392394814,-0.906810168463347,
13.891594583144));
#25744=CARTESIAN_POINT('Ctrl Pts',(-2.51545460624217,-2.95119723051152,
13.9875875631112));
#25745=CARTESIAN_POINT('Ctrl Pts',(0.942385426660244,-3.87392403926152,
14.1365688318067));
#25746=CARTESIAN_POINT('Ctrl Pts',(3.76741231340739,-1.30460040439068,14.2955336979914));
#25747=CARTESIAN_POINT('Ctrl Pts',(3.1362669786623,2.46154569181692,14.4544985641762));
#25748=CARTESIAN_POINT('Ctrl Pts',(-0.372046531241306,3.96950363810656,
14.6134634303609));
#25749=CARTESIAN_POINT('Ctrl Pts',(-2.98916250729706,2.20635255558199,14.7448272062705));
#25750=CARTESIAN_POINT('Ctrl Pts',(-3.36678347516941,0.540290560949759,
14.8232026934519));
#25751=CARTESIAN_POINT('Ctrl Pts',(-3.36623102492646,0.000387483300790976,
14.848589891905));
#25752=CARTESIAN_POINT('Origin',(0.,0.,-1.84858989190503));
#25753=CARTESIAN_POINT('',(-3.36754256765694,-0.00208193686516585,12.651410108095));
#25754=CARTESIAN_POINT('',(-3.3758812610584,-0.00196014188030613,12.848589891905));
#25755=CARTESIAN_POINT('',(-3.37175,2.08693528006523E-13,-1.84858989190503));
#25756=CARTESIAN_POINT('Ctrl Pts',(-3.36754256765694,-0.00208193686516537,
12.651410108095));
#25757=CARTESIAN_POINT('Ctrl Pts',(-3.36993408573054,-0.426611763038696,
12.6713916849665));
#25758=CARTESIAN_POINT('Ctrl Pts',(-3.09838828538505,-1.97347045721629,
12.7443372403327));
#25759=CARTESIAN_POINT('Ctrl Pts',(-0.775556132376715,-3.9101105474236,
12.8702467741936));
#25760=CARTESIAN_POINT('Ctrl Pts',(2.86663624227273,-2.76999069710151,13.0291387096774));
#25761=CARTESIAN_POINT('Ctrl Pts',(3.88122465785174,0.909146282412278,13.1880306451613));
#25762=CARTESIAN_POINT('Ctrl Pts',(1.33822138229676,3.75494545093591,13.3469225806451));
#25763=CARTESIAN_POINT('Ctrl Pts',(-2.32626682514693,3.17552839905125,13.5013824016231));
#25764=CARTESIAN_POINT('Ctrl Pts',(-3.37015749501604,1.02261334351231,13.6028782441063));
#25765=CARTESIAN_POINT('Ctrl Pts',(-3.37630962516523,-0.00164737155311456,
13.651410108095));
#25766=CARTESIAN_POINT('Ctrl Pts',(-3.3758812610584,-0.00196014188030577,
12.848589891905));
#25767=CARTESIAN_POINT('Ctrl Pts',(-3.37667181942981,-0.11638712350615,
12.8540098953796));
#25768=CARTESIAN_POINT('Ctrl Pts',(-3.31942395404611,-1.34870119310656,
12.9124181875824));
#25769=CARTESIAN_POINT('Ctrl Pts',(-1.80499399926681,-3.5549084962852,13.0238147685134));
#25770=CARTESIAN_POINT('Ctrl Pts',(2.01200065152342,-3.44198069904803,13.1827796346982));
#25771=CARTESIAN_POINT('Ctrl Pts',(3.98321358718988,-0.171427165804589,
13.3417445008829));
#25772=CARTESIAN_POINT('Ctrl Pts',(2.30028118194861,3.25639129072706,13.5007093670677));
#25773=CARTESIAN_POINT('Ctrl Pts',(-1.49289753065309,3.69684118097057,13.6596742332524));
#25774=CARTESIAN_POINT('Ctrl Pts',(-3.26085313565002,1.54418744509758,13.7756344081982));
#25775=CARTESIAN_POINT('Ctrl Pts',(-3.37520242261949,0.214132631825097,
13.8386062944157));
#25776=CARTESIAN_POINT('Ctrl Pts',(-3.37326960455653,0.00293423317535065,
13.848589891905));
#25777=CARTESIAN_POINT('Origin',(0.,0.,-1.84858989190503));
#25778=CARTESIAN_POINT('',(-3.36871665678573,0.00265343926576773,11.651410108095));
#25779=CARTESIAN_POINT('',(-3.36722041330275,-0.00185992061757206,11.848589891905));
#25780=CARTESIAN_POINT('',(-3.37175,2.08693528006523E-13,-1.84858989190503));
#25781=CARTESIAN_POINT('Ctrl Pts',(-3.36871665678573,0.00265343926576761,
11.651410108095));
#25782=CARTESIAN_POINT('Ctrl Pts',(-3.36317444447066,-0.751580168678052,
11.6869411473321));
#25783=CARTESIAN_POINT('Ctrl Pts',(-2.7398020033052,-2.63841079513441,11.7754361650639));
#25784=CARTESIAN_POINT('Ctrl Pts',(0.38723559847199,-3.96742994882286,11.9168951612903));
#25785=CARTESIAN_POINT('Ctrl Pts',(3.54469272874429,-1.82362421192741,12.0757870967742));
#25786=CARTESIAN_POINT('Ctrl Pts',(3.45302863798842,1.9917442187119,12.2346790322581));
#25787=CARTESIAN_POINT('Ctrl Pts',(0.196264076456207,3.98144850774605,12.3935709677419));
#25788=CARTESIAN_POINT('Ctrl Pts',(-2.80821900811,2.53041799939006,12.5324813263542));
#25789=CARTESIAN_POINT('Ctrl Pts',(-3.36359503087846,0.698664221349558,
12.6184277064719));
#25790=CARTESIAN_POINT('Ctrl Pts',(-3.36754256765694,-0.00208193686516537,
12.651410108095));
#25791=CARTESIAN_POINT('Ctrl Pts',(-3.36722041330275,-0.00185992061757217,
11.848589891905));
#25792=CARTESIAN_POINT('Ctrl Pts',(-3.36943251646156,-0.444385182068521,
11.8694134963434));
#25793=CARTESIAN_POINT('Ctrl Pts',(-3.08234983495276,-2.01021544013623,
11.9432253895101));
#25794=CARTESIAN_POINT('Ctrl Pts',(-0.711713421966334,-3.92286142494773,
12.0700255714049));
#25795=CARTESIAN_POINT('Ctrl Pts',(2.91318501009988,-2.72189839106446,12.2289904375897));
#25796=CARTESIAN_POINT('Ctrl Pts',(3.86556759564105,0.976096776902648,12.3879553037744));
#25797=CARTESIAN_POINT('Ctrl Pts',(1.27173165426137,3.77863419159615,12.5469201699592));
#25798=CARTESIAN_POINT('Ctrl Pts',(-2.36055670961755,3.13734167043916,12.7004650326694));
#25799=CARTESIAN_POINT('Ctrl Pts',(-3.36894298024411,1.00230034028648,12.8010216066513));
#25800=CARTESIAN_POINT('Ctrl Pts',(-3.3758812610584,-0.00196014188030577,
12.848589891905));
#25801=CARTESIAN_POINT('Origin',(0.,0.,-1.84858989190503));
#25802=CARTESIAN_POINT('',(-3.37710546106046,0.000736094683953019,10.651410108095));
#25803=CARTESIAN_POINT('',(-3.36907238740032,0.00277677980771746,10.848589891905));
#25804=CARTESIAN_POINT('',(-3.37175,2.08693528006523E-13,-1.84858989190503));
#25805=CARTESIAN_POINT('Ctrl Pts',(-3.37710546106046,0.000736094683952996,
10.651410108095));
#25806=CARTESIAN_POINT('Ctrl Pts',(-3.37391321273993,-1.07663815669567,
10.7024906096977));
#25807=CARTESIAN_POINT('Ctrl Pts',(-2.23194165802167,-3.27693130018453,
10.8065350897951));
#25808=CARTESIAN_POINT('Ctrl Pts',(1.51699821428175,-3.68634890174633,10.9635435483871));
#25809=CARTESIAN_POINT('Ctrl Pts',(3.92040597926993,-0.721712384018116,
11.122435483871));
#25810=CARTESIAN_POINT('Ctrl Pts',(2.73030783639792,2.90445707939446,11.2813274193548));
#25811=CARTESIAN_POINT('Ctrl Pts',(-0.962433500126168,3.86835540835836,
11.4402193548387));
#25812=CARTESIAN_POINT('Ctrl Pts',(-3.1445024192473,1.86381595651157,11.5635802510854));
#25813=CARTESIAN_POINT('Ctrl Pts',(-3.37143588630209,0.372710407919653,
11.6339771688375));
#25814=CARTESIAN_POINT('Ctrl Pts',(-3.36871665678573,0.00265343926576761,
11.651410108095));
#25815=CARTESIAN_POINT('Ctrl Pts',(-3.36907238740032,0.00277677980771742,
10.848589891905));
#25816=CARTESIAN_POINT('Ctrl Pts',(-3.36312082444251,-0.766029392039194,
10.8848170973072));
#25817=CARTESIAN_POINT('Ctrl Pts',(-2.72027913252513,-2.66834094208117,
10.9740325914377));
#25818=CARTESIAN_POINT('Ctrl Pts',(0.441146911493231,-3.96241935650807,
11.1162363742964));
#25819=CARTESIAN_POINT('Ctrl Pts',(3.57049754163045,-1.77395745708877,11.2752012404812));
#25820=CARTESIAN_POINT('Ctrl Pts',(3.42432285260543,2.04190860605321,11.4341661066659));
#25821=CARTESIAN_POINT('Ctrl Pts',(0.136721492950909,3.98455580808139,11.5931309728507));
#25822=CARTESIAN_POINT('Ctrl Pts',(-2.82921667119627,2.49618535096433,11.7312722345971));
#25823=CARTESIAN_POINT('Ctrl Pts',(-3.36380354088135,0.681676177418306,
11.8164252076152));
#25824=CARTESIAN_POINT('Ctrl Pts',(-3.36722041330275,-0.00185992061757217,
11.848589891905));
#25825=CARTESIAN_POINT('Origin',(0.,0.,-1.84858989190503));
#25826=CARTESIAN_POINT('',(-3.37090359896229,-0.00307926823583696,9.65141010809498));
#25827=CARTESIAN_POINT('',(-3.37720911693329,0.000534521222638907,9.84858989190502));
#25828=CARTESIAN_POINT('',(-3.37175,2.08693528006523E-13,-1.84858989190503));
#25829=CARTESIAN_POINT('Ctrl Pts',(-3.37090359896229,-0.0030792682358368,
9.65141010809498));
#25830=CARTESIAN_POINT('Ctrl Pts',(-3.37349992290045,-0.292697043198134,
9.6650760935687));
#25831=CARTESIAN_POINT('Ctrl Pts',(-3.20668744219234,-1.70181407180786,
9.73170605753704));
#25832=CARTESIAN_POINT('Ctrl Pts',(-1.23445173354738,-3.79032725830928,
9.85129999999999));
#25833=CARTESIAN_POINT('Ctrl Pts',(2.51736903674626,-3.09084210861242,10.0101919354839));
#25834=CARTESIAN_POINT('Ctrl Pts',(3.96172967315432,0.441757630821415,10.1690838709677));
#25835=CARTESIAN_POINT('Ctrl Pts',(1.77470645260886,3.56943536355667,10.3279758064516));
#25836=CARTESIAN_POINT('Ctrl Pts',(-2.03904067252446,3.42531238624034,10.4868677419355));
#25837=CARTESIAN_POINT('Ctrl Pts',(-3.35858003390563,1.1971743885357,10.5946791758166));
#25838=CARTESIAN_POINT('Ctrl Pts',(-3.37722316793013,0.0404618108125119,
10.6495266312031));
#25839=CARTESIAN_POINT('Ctrl Pts',(-3.37710546106046,0.000736094683952996,
10.651410108095));
#25840=CARTESIAN_POINT('Ctrl Pts',(-3.37720911693329,0.000534521222638742,
9.84858989190502));
#25841=CARTESIAN_POINT('Ctrl Pts',(-3.37481325646777,-1.08835732049462,
9.90022069827108));
#25842=CARTESIAN_POINT('Ctrl Pts',(-2.21074657312113,-3.29916896326091,
10.0048397933654));
#25843=CARTESIAN_POINT('Ctrl Pts',(1.55707745747673,-3.67027077281332,10.1624471771879));
#25844=CARTESIAN_POINT('Ctrl Pts',(3.928912558612,-0.677512997019795,10.3214120433727));
#25845=CARTESIAN_POINT('Ctrl Pts',(2.69641733534343,2.93678588051791,10.4803769095574));
#25846=CARTESIAN_POINT('Ctrl Pts',(-1.00973405207762,3.8569177977272,10.6393417757422));
#25847=CARTESIAN_POINT('Ctrl Pts',(-3.15606037844699,1.83542847981608,10.7620794365247));
#25848=CARTESIAN_POINT('Ctrl Pts',(-3.37182597111036,0.358476982592217,
10.831828808579));
#25849=CARTESIAN_POINT('Ctrl Pts',(-3.36907238740032,0.00277677980771742,
10.848589891905));
#25850=CARTESIAN_POINT('Origin',(0.,0.,-1.84858989190503));
#25851=CARTESIAN_POINT('',(-3.36644585084492,0.000942668595409863,8.65141010809498));
#25852=CARTESIAN_POINT('',(-3.37066808100933,-0.00306963188584058,8.84858989190501));
#25853=CARTESIAN_POINT('',(-3.37175,2.08693528006523E-13,-1.84858989190503));
#25854=CARTESIAN_POINT('Ctrl Pts',(-3.36644585084492,0.000942668595410034,
8.65141010809498));
#25855=CARTESIAN_POINT('Ctrl Pts',(-3.36489256340397,-0.620276501159167,
8.68062555593429));
#25856=CARTESIAN_POINT('Ctrl Pts',(-2.90218694538986,-2.36984060140867,
8.76280498226821));
#25857=CARTESIAN_POINT('Ctrl Pts',(-0.086697347329244,-3.9853400579507,
8.89794838709678));
#25858=CARTESIAN_POINT('Ctrl Pts',(3.30302181201077,-2.23170309784288,9.05684032258065));
#25859=CARTESIAN_POINT('Ctrl Pts',(3.66513912143678,1.56754809433529,9.21573225806451));
#25860=CARTESIAN_POINT('Ctrl Pts',(0.667732148006428,3.92995999802278,9.3746241935484));
#25861=CARTESIAN_POINT('Ctrl Pts',(-2.63128595375923,2.79674582771393,9.51985014355854));
#25862=CARTESIAN_POINT('Ctrl Pts',(-3.36343759366045,0.829747410900375,
9.61211211507407));
#25863=CARTESIAN_POINT('Ctrl Pts',(-3.37090359896229,-0.0030792682358368,
9.65141010809498));
#25864=CARTESIAN_POINT('Ctrl Pts',(-3.37066808100933,-0.0030696318858409,
8.84858989190502));
#25865=CARTESIAN_POINT('Ctrl Pts',(-3.37331082414,-0.300796169438093,8.86263601050667));
#25866=CARTESIAN_POINT('Ctrl Pts',(-3.20068977672434,-1.71866740211794,
8.92967041783657));
#25867=CARTESIAN_POINT('Ctrl Pts',(-1.20570712414377,-3.80021684712055,
9.04969311389473));
#25868=CARTESIAN_POINT('Ctrl Pts',(2.54266018034211,-3.07087234538534,9.20865798007948));
#25869=CARTESIAN_POINT('Ctrl Pts',(3.95842601916979,0.47564819468749,9.36762284626423));
#25870=CARTESIAN_POINT('Ctrl Pts',(1.74278629094578,3.58581562527152,9.52658771244896));
#25871=CARTESIAN_POINT('Ctrl Pts',(-2.07166160205713,3.40640513751843,9.68555257863373));
#25872=CARTESIAN_POINT('Ctrl Pts',(-3.36396169301834,1.17525404838138,9.7928866384524));
#25873=CARTESIAN_POINT('Ctrl Pts',(-3.377272109138,0.0291637752183697,9.84723240954283));
#25874=CARTESIAN_POINT('Ctrl Pts',(-3.37720911693329,0.000534521222638742,
9.84858989190502));
#25875=CARTESIAN_POINT('Origin',(0.,0.,-1.84858989190503));
#25876=CARTESIAN_POINT('',(-3.37436653161969,0.00264543560195785,7.65141010809498));
#25877=CARTESIAN_POINT('',(-3.36647579863201,0.00101859643942465,7.84858989190502));
#25878=CARTESIAN_POINT('',(-3.37175,2.08693528006523E-13,-1.84858989190503));
#25879=CARTESIAN_POINT('Ctrl Pts',(-3.37436653161969,0.00264543560195811,
7.65141010809498));
#25880=CARTESIAN_POINT('Ctrl Pts',(-3.36621424622869,-0.943539301975876,
7.69617501829988));
#25881=CARTESIAN_POINT('Ctrl Pts',(-2.45755376938072,-3.02292340440546,
7.7939039069994));
#25882=CARTESIAN_POINT('Ctrl Pts',(1.06845185659111,-3.84042477308012,7.94459677419355));
#25883=CARTESIAN_POINT('Ctrl Pts',(3.80694458147109,-1.18221180891932,8.10348870967742));
#25884=CARTESIAN_POINT('Ctrl Pts',(3.0559319039131,2.55963513145653,8.2623806451613));
#25885=CARTESIAN_POINT('Ctrl Pts',(-0.49619611955484,3.95528016940384,8.42127258064515));
#25886=CARTESIAN_POINT('Ctrl Pts',(-3.02400139141134,2.13545120331948,8.55094906828973));
#25887=CARTESIAN_POINT('Ctrl Pts',(-3.36770848062251,0.505916700748885,
8.62766157743967));
#25888=CARTESIAN_POINT('Ctrl Pts',(-3.36644585084492,0.000942668595410034,
8.65141010809498));
#25889=CARTESIAN_POINT('Ctrl Pts',(-3.36647579863201,0.00101859643942433,
7.84858989190502));
#25890=CARTESIAN_POINT('Ctrl Pts',(-3.36478428770786,-0.625167485996831,
7.87803961147051));
#25891=CARTESIAN_POINT('Ctrl Pts',(-2.8964828528491,-2.38038813746449,7.96047761976425));
#25892=CARTESIAN_POINT('Ctrl Pts',(-0.0672816548149041,-3.98633301836102,
8.09590391678625));
#25893=CARTESIAN_POINT('Ctrl Pts',(3.31538886833258,-2.21440159096907,8.25486878297098));
#25894=CARTESIAN_POINT('Ctrl Pts',(3.65656725922866,1.58899138861319,8.41383364915575));
#25895=CARTESIAN_POINT('Ctrl Pts',(0.643261156248369,3.93466553079316,8.57279851534047));
#25896=CARTESIAN_POINT('Ctrl Pts',(-2.64176562949924,2.78241271369441,8.71771726292358));
#25897=CARTESIAN_POINT('Ctrl Pts',(-3.36334120619684,0.822362489639698,
8.80964772177842));
#25898=CARTESIAN_POINT('Ctrl Pts',(-3.37066808100933,-0.0030696318858409,
8.84858989190502));
#25899=CARTESIAN_POINT('Origin',(0.,0.,-1.84858989190503));
#25900=CARTESIAN_POINT('',(-3.3748606436688,-0.00246557707590639,6.65141010809498));
#25901=CARTESIAN_POINT('',(-3.37441250761161,0.00263846066578283,6.84858989190502));
#25902=CARTESIAN_POINT('',(-3.37175,2.08693528006523E-13,-1.84858989190503));
#25903=CARTESIAN_POINT('Ctrl Pts',(-3.3748606436688,-0.00246557707590626,
6.65141010809497));
#25904=CARTESIAN_POINT('Ctrl Pts',(-3.37613613582624,-0.157769830059076,
6.65876050217084));
#25905=CARTESIAN_POINT('Ctrl Pts',(-3.29579272315184,-1.43080711580639,
6.71907487474133));
#25906=CARTESIAN_POINT('Ctrl Pts',(-1.67587337027072,-3.61689096522939,
6.83235322580646));
#25907=CARTESIAN_POINT('Ctrl Pts',(2.13246786040229,-3.36794189853266,6.99124516129032));
#25908=CARTESIAN_POINT('Ctrl Pts',(3.98615544163244,-0.0318842074478251,
7.15013709677419));
#25909=CARTESIAN_POINT('Ctrl Pts',(2.18607012156152,3.33339905069232,7.30902903225807));
#25910=CARTESIAN_POINT('Ctrl Pts',(-1.61780152532516,3.64323620318475,7.46792096774193));
#25911=CARTESIAN_POINT('Ctrl Pts',(-3.28487995770484,1.46716325720085,7.58204799302091));
#25912=CARTESIAN_POINT('Ctrl Pts',(-3.37585969097893,0.175947096268433,
7.64321103980526));
#25913=CARTESIAN_POINT('Ctrl Pts',(-3.37436653161969,0.00264543560195811,
7.65141010809498));
#25914=CARTESIAN_POINT('Ctrl Pts',(-3.37441250761161,0.00263846066578258,
6.84858989190502));
#25915=CARTESIAN_POINT('Ctrl Pts',(-3.36625911376211,-0.945381294583835,
6.89344321243435));
#25916=CARTESIAN_POINT('Ctrl Pts',(-2.45439078883877,-3.02709322103295,
6.99128482169193));
#25917=CARTESIAN_POINT('Ctrl Pts',(1.07677617223565,-3.83874078693202,7.14211471967776));
#25918=CARTESIAN_POINT('Ctrl Pts',(3.81057598656871,-1.17255635469506,7.3010795858625));
#25919=CARTESIAN_POINT('Ctrl Pts',(3.04860581952888,2.56931514444696,7.46004445204726));
#25920=CARTESIAN_POINT('Ctrl Pts',(-0.510113381387115,3.95413228059959,
7.619009318232));
#25921=CARTESIAN_POINT('Ctrl Pts',(-3.02827174132543,2.12695452322279,7.74852446485126));
#25922=CARTESIAN_POINT('Ctrl Pts',(-3.36782778932888,0.501516551178981,
7.82505132274226));
#25923=CARTESIAN_POINT('Ctrl Pts',(-3.36647579863201,0.00101859643942433,
7.84858989190502));
#25924=CARTESIAN_POINT('Origin',(0.,0.,-1.84858989190503));
#25925=CARTESIAN_POINT('',(-3.36661890683212,-0.00122158962200572,5.65141010809498));
#25926=CARTESIAN_POINT('',(-3.37491538366506,-0.00245188971244759,5.84858989190502));
#25927=CARTESIAN_POINT('',(-3.37175,2.08693528006523E-13,-1.84858989190503));
#25928=CARTESIAN_POINT('Ctrl Pts',(-3.36661890683212,-0.00122158962200539,
5.65141010809498));
#25929=CARTESIAN_POINT('Ctrl Pts',(-3.36820126338182,-0.488087448628749,
5.67430996453643));
#25930=CARTESIAN_POINT('Ctrl Pts',(-3.04142339082007,-2.09897775501084,
5.75017379947252));
#25931=CARTESIAN_POINT('Ctrl Pts',(-0.559403071098495,-3.94683670951677,
5.87900161290323));
#25932=CARTESIAN_POINT('Ctrl Pts',(3.01459581839321,-2.60819168376593,6.03789354838709));
#25933=CARTESIAN_POINT('Ctrl Pts',(3.82536866943663,1.12116294553142,6.19678548387097));
#25934=CARTESIAN_POINT('Ctrl Pts',(1.12974830864147,3.82284194895142,6.35567741935484));
#25935=CARTESIAN_POINT('Ctrl Pts',(-2.42881219485455,3.0575629803579,6.50721896076285));
#25936=CARTESIAN_POINT('Ctrl Pts',(-3.3669454531908,0.961290050298803,6.60579652367622));
#25937=CARTESIAN_POINT('Ctrl Pts',(-3.3748606436688,-0.00246557707590626,
6.65141010809497));
#25938=CARTESIAN_POINT('Ctrl Pts',(-3.37491538366506,-0.00245188971244781,
5.84858989190502));
#25939=CARTESIAN_POINT('Ctrl Pts',(-3.37617143803668,-0.156022125643285,
5.85585852466994));
#25940=CARTESIAN_POINT('Ctrl Pts',(-3.29681403413222,-1.42781289481916,
5.91611544616311));
#25941=CARTESIAN_POINT('Ctrl Pts',(-1.68004955900417,-3.61563427819245,
6.02936065638453));
#25942=CARTESIAN_POINT('Ctrl Pts',(2.13069369871068,-3.3697955600636,6.18832552256926));
#25943=CARTESIAN_POINT('Ctrl Pts',(3.98676787287831,-0.032552759256669,
6.34729038875402));
#25944=CARTESIAN_POINT('Ctrl Pts',(2.18543605335013,3.3345534950076,6.50625525493876));
#25945=CARTESIAN_POINT('Ctrl Pts',(-1.62078473268592,3.64258625218979,6.66522012112352));
#25946=CARTESIAN_POINT('Ctrl Pts',(-3.2856992999535,1.4649244081245,6.77933166677893));
#25947=CARTESIAN_POINT('Ctrl Pts',(-3.37589127437617,0.174579143538081,
6.8404549237061));
#25948=CARTESIAN_POINT('Ctrl Pts',(-3.37441250761161,0.00263846066578258,
6.84858989190502));
#25949=CARTESIAN_POINT('Origin',(0.,0.,-1.84858989190503));
#25950=CARTESIAN_POINT('',(-3.37037732776107,0.00303222645661923,4.65141010809497));
#25951=CARTESIAN_POINT('',(-3.36666513788771,-0.00130109466394523,4.84858989190502));
#25952=CARTESIAN_POINT('',(-3.37175,2.08693528006523E-13,-1.84858989190503));
#25953=CARTESIAN_POINT('Ctrl Pts',(-3.37037732776107,0.00303222645661912,
4.65141010809497));
#25954=CARTESIAN_POINT('Ctrl Pts',(-3.36327434274459,-0.812132332425157,
4.68985942690203));
#25955=CARTESIAN_POINT('Ctrl Pts',(-2.65651681547025,-2.76122659154967,
4.7812727242037));
#25956=CARTESIAN_POINT('Ctrl Pts',(0.604781303071069,-3.94013849796468,
4.92565));
#25957=CARTESIAN_POINT('Ctrl Pts',(3.63959495745868,-1.6259767381985,5.08454193548388));
#25958=CARTESIAN_POINT('Ctrl Pts',(3.3382985122726,2.17858092584818,5.24343387096774));
#25959=CARTESIAN_POINT('Ctrl Pts',(-0.0229349622598251,3.98621697792136,
5.40232580645161));
#25960=CARTESIAN_POINT('Ctrl Pts',(-2.88174731779988,2.40610117021057,5.53831788549402));
#25961=CARTESIAN_POINT('Ctrl Pts',(-3.36454150689018,0.637961221244742,
5.62134598604181));
#25962=CARTESIAN_POINT('Ctrl Pts',(-3.36661890683212,-0.00122158962200539,
5.65141010809498));
#25963=CARTESIAN_POINT('Ctrl Pts',(-3.36666513788771,-0.00130109466394548,
4.84858989190502));
#25964=CARTESIAN_POINT('Ctrl Pts',(-3.36833385037662,-0.483310565759833,
4.87126212563378));
#25965=CARTESIAN_POINT('Ctrl Pts',(-3.04595737613669,-2.0897168735396,4.94692264809078));
#25966=CARTESIAN_POINT('Ctrl Pts',(-0.574613628296617,-3.94527526701846,
5.07557145927603));
#25967=CARTESIAN_POINT('Ctrl Pts',(3.0062441927532,-2.61875420913902,5.2345363254608));
#25968=CARTESIAN_POINT('Ctrl Pts',(3.8292149534867,1.11017592945447,5.39350119164552));
#25969=CARTESIAN_POINT('Ctrl Pts',(1.13931660104628,3.82064594498541,5.55246605783029));
#25970=CARTESIAN_POINT('Ctrl Pts',(-2.42498889622798,3.06243800957472,5.7041622912501));
#25971=CARTESIAN_POINT('Ctrl Pts',(-3.36701480929308,0.963503961964746,
5.80287023594169));
#25972=CARTESIAN_POINT('Ctrl Pts',(-3.37491538366506,-0.00245188971244781,
5.84858989190502));
#25973=CARTESIAN_POINT('Origin',(0.,0.,-1.84858989190503));
#25974=CARTESIAN_POINT('',(-3.37724050405987,-0.000407706007126927,3.65141010809498));
#25975=CARTESIAN_POINT('',(-3.37013695473896,0.00300786229786701,3.84858989190502));
#25976=CARTESIAN_POINT('',(-3.37175,2.08693528006523E-13,-1.84858989190503));
#25977=CARTESIAN_POINT('Ctrl Pts',(-3.37724050405987,-0.000407706007126926,
3.65141010809498));
#25978=CARTESIAN_POINT('Ctrl Pts',(-3.37727770925144,-0.0222311044065494,
3.652444910773));
#25979=CARTESIAN_POINT('Ctrl Pts',(-3.36719553771294,-1.16099931030625,
3.70644369194564));
#25980=CARTESIAN_POINT('Ctrl Pts',(-2.09357261161725,-3.39225669930255,
3.8134064516129));
#25981=CARTESIAN_POINT('Ctrl Pts',(1.71738108280889,-3.59736765289132,3.97229838709678));
#25982=CARTESIAN_POINT('Ctrl Pts',(3.95415621068438,-0.505074716519562,
4.13119032258065));
#25983=CARTESIAN_POINT('Ctrl Pts',(2.56648943634972,3.05017766348832,4.29008225806451));
#25984=CARTESIAN_POINT('Ctrl Pts',(-1.17366200413909,3.8095891259482,4.44897419354839));
#25985=CARTESIAN_POINT('Ctrl Pts',(-3.19328501843251,1.73829700144105,4.56941681022521));
#25986=CARTESIAN_POINT('Ctrl Pts',(-3.37305871233378,0.310757734440618,
4.6368954484074));
#25987=CARTESIAN_POINT('Ctrl Pts',(-3.37037732776107,0.00303222645661912,
4.65141010809497));
#25988=CARTESIAN_POINT('Ctrl Pts',(-3.37013695473896,0.00300786229786694,
3.84858989190502));
#25989=CARTESIAN_POINT('Ctrl Pts',(-3.36320369751902,-0.804384073785939,
3.88666572659761));
#25990=CARTESIAN_POINT('Ctrl Pts',(-2.66732523950674,-2.7461115272218,3.97772985001845));
#25991=CARTESIAN_POINT('Ctrl Pts',(0.57892500607099,-3.94464492605495,4.12178226216755));
#25992=CARTESIAN_POINT('Ctrl Pts',(3.63013258458704,-1.64848875417016,4.2807471283523));
#25993=CARTESIAN_POINT('Ctrl Pts',(3.35110647594949,2.15996831943484,4.43971199453705));
#25994=CARTESIAN_POINT('Ctrl Pts',(-0.00217860669321579,3.9869001753454,
4.59867686072179));
#25995=CARTESIAN_POINT('Ctrl Pts',(-2.87549058156321,2.41739184906724,4.73496949317778));
#25996=CARTESIAN_POINT('Ctrl Pts',(-3.36443382798691,0.643215268868607,
4.81827383690552));
#25997=CARTESIAN_POINT('Ctrl Pts',(-3.36666513788771,-0.00130109466394548,
4.84858989190502));
#25998=CARTESIAN_POINT('Origin',(0.,0.,-1.84858989190503));
#25999=CARTESIAN_POINT('',(-3.36917031630593,-0.00279652979204336,2.65141010809498));
#26000=CARTESIAN_POINT('',(-3.37729882489346,-0.000194430141600699,2.84858989190502));
#26001=CARTESIAN_POINT('',(-3.37175,2.08693528006523E-13,-1.84858989190503));
#26002=CARTESIAN_POINT('Ctrl Pts',(-3.36917031630593,-0.00279652979204365,
2.65141010809498));
#26003=CARTESIAN_POINT('Ctrl Pts',(-3.37192195751912,-0.354718783760072,
2.66799437313859));
#26004=CARTESIAN_POINT('Ctrl Pts',(-3.15912528101716,-1.82730552094877,
2.73754261667682));
#26005=CARTESIAN_POINT('Ctrl Pts',(-1.02419029239979,-3.85246484135621,
2.86005483870968));
#26006=CARTESIAN_POINT('Ctrl Pts',(2.68349747959669,-2.94776072747231,3.01894677419354));
#26007=CARTESIAN_POINT('Ctrl Pts',(3.9314491981565,0.658907486316316,3.17783870967743));
#26008=CARTESIAN_POINT('Ctrl Pts',(1.57577260497388,3.66161063015511,3.33673064516129));
#26009=CARTESIAN_POINT('Ctrl Pts',(-2.19953367602677,3.310326581852,3.49458777796714));
#26010=CARTESIAN_POINT('Ctrl Pts',(-3.37537344768752,1.09474900016628,3.59948093227837));
#26011=CARTESIAN_POINT('Ctrl Pts',(-3.37724050405987,-0.000407706007126926,
3.65141010809498));
#26012=CARTESIAN_POINT('Ctrl Pts',(-3.37729882489346,-0.000194430141600942,
2.84858989190502));
#26013=CARTESIAN_POINT('Ctrl Pts',(-3.37730745906329,-0.0105519609168573,
2.8490810388332));
#26014=CARTESIAN_POINT('Ctrl Pts',(-3.3725690581147,-1.13834260190552,2.90256047448963));
#26015=CARTESIAN_POINT('Ctrl Pts',(-2.12700963248002,-3.37212213291773,
3.00902819887431));
#26016=CARTESIAN_POINT('Ctrl Pts',(1.68400001564517,-3.61379602896036,3.16799306505907));
#26017=CARTESIAN_POINT('Ctrl Pts',(3.95013122707835,-0.540223147458982,
3.32695793124381));
#26018=CARTESIAN_POINT('Ctrl Pts',(2.59246639543577,3.02894300530038,3.48592279742856));
#26019=CARTESIAN_POINT('Ctrl Pts',(-1.14349143614182,3.81939852540782,3.6448876636133));
#26020=CARTESIAN_POINT('Ctrl Pts',(-3.18684176799334,1.75591563149786,3.76577669510546));
#26021=CARTESIAN_POINT('Ctrl Pts',(-3.37285237464884,0.31922404594331,3.83367743786936));
#26022=CARTESIAN_POINT('Ctrl Pts',(-3.37013695473896,0.00300786229786694,
3.84858989190502));
#26023=CARTESIAN_POINT('Origin',(0.,0.,-1.84858989190503));
#26024=CARTESIAN_POINT('',(-3.36722314734446,0.00185482314707379,1.65141010809497));
#26025=CARTESIAN_POINT('',(-3.3695578818617,-0.00290129534754852,1.84858989190502));
#26026=CARTESIAN_POINT('',(-3.37175,2.08693528006523E-13,-1.84858989190503));
#26027=CARTESIAN_POINT('Ctrl Pts',(-3.36722314734446,0.00185482314707382,
1.65141010809497));
#26028=CARTESIAN_POINT('Ctrl Pts',(-3.36382382620938,-0.68102387856646,
1.68354383550418));
#26029=CARTESIAN_POINT('Ctrl Pts',(-2.83012682104856,-2.49433668358649,
1.768641541408));
#26030=CARTESIAN_POINT('Ctrl Pts',(0.13255069832671,-3.98407441119242,1.90670322580645));
#26031=CARTESIAN_POINT('Ctrl Pts',(3.42072557595435,-2.04672776701011,2.06559516129032));
#26032=CARTESIAN_POINT('Ctrl Pts',(3.57341090601276,1.76668952717683,2.2244870967742));
#26033=CARTESIAN_POINT('Ctrl Pts',(0.45065073371557,3.96072731387378,2.38337903225806));
#26034=CARTESIAN_POINT('Ctrl Pts',(-2.71613180302817,2.67422828685271,2.52568670269832));
#26035=CARTESIAN_POINT('Ctrl Pts',(-3.36313423821671,0.769190092631348,
2.61503039464396));
#26036=CARTESIAN_POINT('Ctrl Pts',(-3.36917031630593,-0.00279652979204365,
2.65141010809498));
#26037=CARTESIAN_POINT('Ctrl Pts',(-3.3695578818617,-0.00290129534754862,
1.84858989190502));
#26038=CARTESIAN_POINT('Ctrl Pts',(-3.37231432811694,-0.34009370411539,
1.86448463979704));
#26039=CARTESIAN_POINT('Ctrl Pts',(-3.1706964344189,-1.79816219768021,1.93336767641731));
#26040=CARTESIAN_POINT('Ctrl Pts',(-1.07258002819951,-3.83991470812214,
2.05523900176583));
#26041=CARTESIAN_POINT('Ctrl Pts',(2.6481020123777,-2.98042525524821,2.21420386795058));
#26042=CARTESIAN_POINT('Ctrl Pts',(3.9394520872816,0.613266379946328,2.37316873413532));
#26043=CARTESIAN_POINT('Ctrl Pts',(1.61680281711694,3.64435532093595,2.53213360032008));
#26044=CARTESIAN_POINT('Ctrl Pts',(-2.17732013669245,3.33312768965276,2.69060731957663));
#26045=CARTESIAN_POINT('Ctrl Pts',(-3.37637594578823,1.10688927659692,2.79609275010495));
#26046=CARTESIAN_POINT('Ctrl Pts',(-3.37729882489346,-0.000194430141600942,
2.84858989190502));
#26047=CARTESIAN_POINT('Origin',(0.,0.,-1.84858989190503));
#26048=CARTESIAN_POINT('',(-3.37589447807987,0.00214364281095937,0.651410108094974));
#26049=CARTESIAN_POINT('',(-3.36692593843476,0.00163208592380837,0.848589891905015));
#26050=CARTESIAN_POINT('',(-3.37175,2.08693528006523E-13,-1.84858989190503));
#26051=CARTESIAN_POINT('Ctrl Pts',(-3.37589447807987,0.0021436428109594,
0.651410108094974));
#26052=CARTESIAN_POINT('Ctrl Pts',(-3.36905382598057,-1.00443485423249,
0.699093297869767));
#26053=CARTESIAN_POINT('Ctrl Pts',(-2.35675364226999,-3.1417842761117,0.799740466139185));
#26054=CARTESIAN_POINT('Ctrl Pts',(1.27802196869812,-3.77566833700333,0.953351612903227));
#26055=CARTESIAN_POINT('Ctrl Pts',(3.86616524359544,-0.97122229991515,1.1122435483871));
#26056=CARTESIAN_POINT('Ctrl Pts',(2.91058978102209,2.72383605033175,1.27113548387097));
#26057=CARTESIAN_POINT('Ctrl Pts',(-0.71291441141164,3.92198718064885,1.43002741935484));
#26058=CARTESIAN_POINT('Ctrl Pts',(-3.08228566582866,2.00998594685298,1.55678562742951));
#26059=CARTESIAN_POINT('Ctrl Pts',(-3.36942671096663,0.444521639742584,
1.63057985700955));
#26060=CARTESIAN_POINT('Ctrl Pts',(-3.36722314734446,0.00185482314707382,
1.65141010809497));
#26061=CARTESIAN_POINT('Ctrl Pts',(-3.36692593843476,0.00163208592380858,
0.848589891905015));
#26062=CARTESIAN_POINT('Ctrl Pts',(-3.36407240691806,-0.663645509172373,
0.879888240760876));
#26063=CARTESIAN_POINT('Ctrl Pts',(-2.85117022634889,-2.45933226824664,
0.964174878344985));
#26064=CARTESIAN_POINT('Ctrl Pts',(0.0716483833591926,-3.98622915634864,
1.10144980465734));
#26065=CARTESIAN_POINT('Ctrl Pts',(3.39051798866077,-2.09756782602768,1.26041467084209));
#26066=CARTESIAN_POINT('Ctrl Pts',(3.59899177492058,1.71542482386315,1.41937953702684));
#26067=CARTESIAN_POINT('Ctrl Pts',(0.505790215469384,3.95468340129096,1.57834440321159));
#26068=CARTESIAN_POINT('Ctrl Pts',(-2.69572995999776,2.70483870003466,1.72141452150431));
#26069=CARTESIAN_POINT('Ctrl Pts',(-3.36312516884065,0.784003943368042,
1.81149635106879));
#26070=CARTESIAN_POINT('Ctrl Pts',(-3.3695578818617,-0.00290129534754862,
1.84858989190502));
#26071=CARTESIAN_POINT('Origin',(0.,0.,24.5));
#26072=CARTESIAN_POINT('',(-3.87097280197699,0.00213832761144025,24.1339652975667));
#26073=CARTESIAN_POINT('Ctrl Pts',(-0.624728334461281,3.3133687646595,24.62825));
#26074=CARTESIAN_POINT('Ctrl Pts',(-0.520138250042208,3.33634852849099,
24.625046902956));
#26075=CARTESIAN_POINT('Ctrl Pts',(-0.414648098080521,3.35389705620374,
24.6218539025135));
#26076=CARTESIAN_POINT('Ctrl Pts',(-0.308613703672553,3.36622114122732,
24.6186673709615));
#26077=CARTESIAN_POINT('Ctrl Pts',(-0.199986616426575,3.37884656778403,
24.6154029241484));
#26078=CARTESIAN_POINT('Ctrl Pts',(-0.0907876447210383,3.38598894312879,
24.6121452664408));
#26079=CARTESIAN_POINT('Ctrl Pts',(0.018614620750679,3.38781780937344,24.6088904974597));
#26080=CARTESIAN_POINT('Ctrl Pts',(0.0805633655032933,3.38885340006882,
24.6070474930945));
#26081=CARTESIAN_POINT('Ctrl Pts',(0.142577487054791,3.38818433590453,24.6052054149592));
#26082=CARTESIAN_POINT('Ctrl Pts',(0.204590631758452,3.38583417858992,24.6033635549037));
#26083=CARTESIAN_POINT('Ctrl Pts',(0.254638036250335,3.38393749564785,24.6018770907733));
#26084=CARTESIAN_POINT('Ctrl Pts',(0.304684819171919,3.38094577981049,24.600390768683));
#26085=CARTESIAN_POINT('Ctrl Pts',(0.354695913393206,3.3768690300029,24.5989042163964));
#26086=CARTESIAN_POINT('Ctrl Pts',(0.372494580510141,3.37541813767843,24.5983751607996));
#26087=CARTESIAN_POINT('Ctrl Pts',(0.39028796136771,3.37382978973891,24.5978460986132));
#26088=CARTESIAN_POINT('Ctrl Pts',(0.408061433233138,3.37210587416845,24.5973174010591));
#26089=CARTESIAN_POINT('Ctrl Pts',(0.519404457290808,3.36130629745725,24.5940053422263));
#26090=CARTESIAN_POINT('Ctrl Pts',(0.630100011901245,3.34518038635334,24.5907036020021));
#26091=CARTESIAN_POINT('Ctrl Pts',(0.739763436768937,3.32391000487198,24.5874081616821));
#26092=CARTESIAN_POINT('Ctrl Pts',(0.850257666159321,3.3024784800636,24.5840877552741));
#26093=CARTESIAN_POINT('Ctrl Pts',(0.95970493776685,3.27582407416606,24.5807737445874));
#26094=CARTESIAN_POINT('Ctrl Pts',(1.06770973553523,3.24407969544398,24.5774620188875));
#26095=CARTESIAN_POINT('Ctrl Pts',(1.1361584697924,3.22396149154746,24.5753631914553));
#26096=CARTESIAN_POINT('Ctrl Pts',(1.20402775637168,3.20179785912252,24.5732652817816));
#26097=CARTESIAN_POINT('Ctrl Pts',(1.27121405220256,3.17761217468148,24.5711672434934));
#26098=CARTESIAN_POINT('Ctrl Pts',(1.29774075436021,3.16806310757318,24.5703388894951));
#26099=CARTESIAN_POINT('Ctrl Pts',(1.32416095392457,3.15819874582631,24.5695105154476));
#26100=CARTESIAN_POINT('Ctrl Pts',(1.35046812449935,3.14802019412801,24.5686820569498));
#26101=CARTESIAN_POINT('Ctrl Pts',(1.36653976589062,3.14180188827438,24.5681759330454));
#26102=CARTESIAN_POINT('Ctrl Pts',(1.38256076287534,3.13546957145725,24.5676700437565));
#26103=CARTESIAN_POINT('Ctrl Pts',(1.39852700263983,3.12902498441374,24.5671644619047));
#26104=CARTESIAN_POINT('Ctrl Pts',(1.5038400459978,3.08651659892363,24.5638296526902));
#26105=CARTESIAN_POINT('Ctrl Pts',(1.60681042310701,3.03911282071154,24.5605069879339));
#26106=CARTESIAN_POINT('Ctrl Pts',(1.70704837153172,2.98697613057657,24.5571923886324));
#26107=CARTESIAN_POINT('Ctrl Pts',(1.80670371564138,2.935142469994,24.5538970544882));
#26108=CARTESIAN_POINT('Ctrl Pts',(1.90365915425284,2.87863046313165,24.5506096923149));
#26109=CARTESIAN_POINT('Ctrl Pts',(1.99751737945406,2.81755070396422,24.5473262938205));
#26110=CARTESIAN_POINT('Ctrl Pts',(2.09219867451912,2.7559353187613,24.5440141022572));
#26111=CARTESIAN_POINT('Ctrl Pts',(2.18372913512715,2.68967155408011,24.5407059441949));
#26112=CARTESIAN_POINT('Ctrl Pts',(2.271672791588,2.61882611527755,24.5373977049647));
#26113=CARTESIAN_POINT('Ctrl Pts',(2.31564461981842,2.58340339587627,24.5357435853496));
#26114=CARTESIAN_POINT('Ctrl Pts',(2.3587192214935,2.54683454512376,24.5340894454425));
#26115=CARTESIAN_POINT('Ctrl Pts',(2.40083835867941,2.50912376524234,24.5324347709098));
#26116=CARTESIAN_POINT('Ctrl Pts',(2.4199270309962,2.49203298969322,24.5316848614374));
#26117=CARTESIAN_POINT('Ctrl Pts',(2.43881941610424,2.47470762973993,24.5309348421549));
#26118=CARTESIAN_POINT('Ctrl Pts',(2.45750989027674,2.45714789797131,24.5301846651845));
#26119=CARTESIAN_POINT('Ctrl Pts',(2.47259728190695,2.4429732682819,24.5295791046386));
#26120=CARTESIAN_POINT('Ctrl Pts',(2.48755582869293,2.42864311414144,24.5289733271752));
#26121=CARTESIAN_POINT('Ctrl Pts',(2.50236326380812,2.41417672018039,24.528368102554));
#26122=CARTESIAN_POINT('Ctrl Pts',(2.5096874370137,2.40702123550619,24.5280687414615));
#26123=CARTESIAN_POINT('Ctrl Pts',(2.51697555679688,2.39983158202503,24.5277694793085));
#26124=CARTESIAN_POINT('Ctrl Pts',(2.52422733942721,2.39260786015533,24.5274703131481));
#26125=CARTESIAN_POINT('Ctrl Pts',(2.60073745914298,2.31639379621843,24.5243139528543));
#26126=CARTESIAN_POINT('Ctrl Pts',(2.67320522179129,2.23639118372509,24.5211682778273));
#26127=CARTESIAN_POINT('Ctrl Pts',(2.74161153441807,2.15302978874429,24.5180298269183));
#26128=CARTESIAN_POINT('Ctrl Pts',(2.81186762190031,2.06741421857952,24.5148065091695));
#26129=CARTESIAN_POINT('Ctrl Pts',(2.87784002551868,1.97825519814193,24.511590811516));
#26130=CARTESIAN_POINT('Ctrl Pts',(2.93947332195402,1.88597569204873,24.5083789843694));
#26131=CARTESIAN_POINT('Ctrl Pts',(3.00543439044467,1.78721649574186,24.5049416288708));
#26132=CARTESIAN_POINT('Ctrl Pts',(3.06642646008642,1.68488265861663,24.5015087065221));
#26133=CARTESIAN_POINT('Ctrl Pts',(3.12233208000985,1.57945276379857,24.4980756211074));
#26134=CARTESIAN_POINT('Ctrl Pts',(3.14679078872635,1.53332718481566,24.4965736462384));
#26135=CARTESIAN_POINT('Ctrl Pts',(3.1702752276744,1.48660856181708,24.4950716401576));
#26136=CARTESIAN_POINT('Ctrl Pts',(3.19277220676191,1.43933527974668,24.4935692179767));
#26137=CARTESIAN_POINT('Ctrl Pts',(3.20843753613705,1.40641745858516,24.4925230358101));
#26138=CARTESIAN_POINT('Ctrl Pts',(3.2236240268298,1.3732306769969,24.4914766518865));
#26139=CARTESIAN_POINT('Ctrl Pts',(3.23832660560595,1.33978769663366,24.4904299362547));
#26140=CARTESIAN_POINT('Ctrl Pts',(3.24466706730076,1.32536546913318,24.489978541947));
#26141=CARTESIAN_POINT('Ctrl Pts',(3.25091694288974,1.31089679039211,24.489527124135));
#26142=CARTESIAN_POINT('Ctrl Pts',(3.25707117071328,1.29639411279135,24.4890760252508));
#26143=CARTESIAN_POINT('Ctrl Pts',(3.30189883440903,1.19075597705509,24.4857902013176));
#26144=CARTESIAN_POINT('Ctrl Pts',(3.34172661274634,1.08315538243838,24.4825162404531));
#26145=CARTESIAN_POINT('Ctrl Pts',(3.37649898345667,0.974036565393082,24.4792502460069));
#26146=CARTESIAN_POINT('Ctrl Pts',(3.41163056334322,0.863790517745426,24.4759505128437));
#26147=CARTESIAN_POINT('Ctrl Pts',(3.44160210056879,0.751993878752548,24.47265891154));
#26148=CARTESIAN_POINT('Ctrl Pts',(3.46631080319639,0.639077130310462,24.4693714234329));
#26149=CARTESIAN_POINT('Ctrl Pts',(3.4909156460234,0.526635012655473,24.4660977538522));
#26150=CARTESIAN_POINT('Ctrl Pts',(3.51030206328578,0.41308129028903,24.4628281629622));
#26151=CARTESIAN_POINT('Ctrl Pts',(3.5243192195213,0.298826837120347,24.4595586825629));
#26152=CARTESIAN_POINT('Ctrl Pts',(3.5361116521245,0.202706203521802,24.4568081155714));
#26153=CARTESIAN_POINT('Ctrl Pts',(3.54410317841348,0.106089103613188,24.4540576267811));
#26154=CARTESIAN_POINT('Ctrl Pts',(3.54817462918724,0.00921931232785102,
24.451304853408));
#26155=CARTESIAN_POINT('Ctrl Pts',(3.54887956636703,-0.00755287067786807,
24.4508282340391));
#26156=CARTESIAN_POINT('Ctrl Pts',(3.54946687335721,-0.0243333324170402,
24.4503515260614));
#26157=CARTESIAN_POINT('Ctrl Pts',(3.5499355914206,-0.0411046474494315,
24.4498751757144));
#26158=CARTESIAN_POINT('Ctrl Pts',(3.55318741783251,-0.157459039234995,
24.4465703987905));
#26159=CARTESIAN_POINT('Ctrl Pts',(3.55074422185484,-0.273556149324447,
24.4432776009626));
#26160=CARTESIAN_POINT('Ctrl Pts',(3.54250561679224,-0.388968852721143,
24.4399928190226));
#26161=CARTESIAN_POINT('Ctrl Pts',(3.53438980253945,-0.502661408204027,
24.4367569945253));
#26162=CARTESIAN_POINT('Ctrl Pts',(3.52065018301948,-0.615690678667281,
24.4335289487538));
#26163=CARTESIAN_POINT('Ctrl Pts',(3.50114108221864,-0.727654569046081,
24.430304893079));
#26164=CARTESIAN_POINT('Ctrl Pts',(3.49384800416623,-0.769509977961124,
24.42909964585));
#26165=CARTESIAN_POINT('Ctrl Pts',(3.48574813528587,-0.811216498584334,
24.427894956231));
#26166=CARTESIAN_POINT('Ctrl Pts',(3.47683197850714,-0.852752977896645,
24.4266906262961));
#26167=CARTESIAN_POINT('Ctrl Pts',(3.4529871352566,-0.963835685722627,24.4234698374258));
#26168=CARTESIAN_POINT('Ctrl Pts',(3.42330774908946,-1.07370337125384,24.4202516210517));
#26169=CARTESIAN_POINT('Ctrl Pts',(3.38809113649622,-1.1820724034292,24.4170321914123));
#26170=CARTESIAN_POINT('Ctrl Pts',(3.37495661955853,-1.22249011495268,24.4158314611315));
#26171=CARTESIAN_POINT('Ctrl Pts',(3.36105136220375,-1.26269920199182,24.4146305620831));
#26172=CARTESIAN_POINT('Ctrl Pts',(3.34638908048464,-1.30268427759558,24.4134292978622));
#26173=CARTESIAN_POINT('Ctrl Pts',(3.33893812623189,-1.32300355496479,24.4128188495754));
#26174=CARTESIAN_POINT('Ctrl Pts',(3.33129166525305,-1.3432649771586,24.412208306987));
#26175=CARTESIAN_POINT('Ctrl Pts',(3.32345141301749,-1.36346647925837,24.411597644323));
#26176=CARTESIAN_POINT('Ctrl Pts',(3.31733644758331,-1.37922253956704,24.4111213610389));
#26177=CARTESIAN_POINT('Ctrl Pts',(3.31110676245958,-1.39493393196613,24.4106452528772));
#26178=CARTESIAN_POINT('Ctrl Pts',(3.30476515852903,-1.41059588192003,24.4101694268982));
#26179=CARTESIAN_POINT('Ctrl Pts',(3.26241982156158,-1.51517676644526,24.4069921531923));
#26180=CARTESIAN_POINT('Ctrl Pts',(3.21506671129281,-1.61761018296196,24.4038257550006));
#26181=CARTESIAN_POINT('Ctrl Pts',(3.16305493267433,-1.71764249367417,24.4006667076014));
#26182=CARTESIAN_POINT('Ctrl Pts',(3.10936292149889,-1.82090633289145,24.3974056076588));
#26183=CARTESIAN_POINT('Ctrl Pts',(3.05070610897566,-1.92161214375833,24.3941523411125));
#26184=CARTESIAN_POINT('Ctrl Pts',(2.98741482167415,-2.01946701686137,24.3909030304897));
#26185=CARTESIAN_POINT('Ctrl Pts',(2.92378476042904,-2.11784566950304,24.3876363275557));
#26186=CARTESIAN_POINT('Ctrl Pts',(2.85546994313465,-2.2133435033276,24.3843736230076));
#26187=CARTESIAN_POINT('Ctrl Pts',(2.78275913579883,-2.30563818528626,24.3811109767752));
#26188=CARTESIAN_POINT('Ctrl Pts',(2.73115118701869,-2.37114618050358,24.3787952484011));
#26189=CARTESIAN_POINT('Ctrl Pts',(2.67732765960473,-2.4350400215934,24.3764795494049));
#26190=CARTESIAN_POINT('Ctrl Pts',(2.62137984513178,-2.49719390809692,24.3741624709621));
#26191=CARTESIAN_POINT('Ctrl Pts',(2.60733587761121,-2.51279571795411,24.3735808401209));
#26192=CARTESIAN_POINT('Ctrl Pts',(2.59315801395097,-2.52828784255011,24.3729991223601));
#26193=CARTESIAN_POINT('Ctrl Pts',(2.5788476135988,-2.54366818796195,24.3724172953964));
#26194=CARTESIAN_POINT('Ctrl Pts',(2.56780240058981,-2.55553921791534,24.3719682232117));
#26195=CARTESIAN_POINT('Ctrl Pts',(2.55668178857907,-2.56733978704972,24.3715192315499));
#26196=CARTESIAN_POINT('Ctrl Pts',(2.54549189058683,-2.5790635828598,24.3710705218887));
#26197=CARTESIAN_POINT('Ctrl Pts',(2.46377857881438,-2.6646756396319,24.367793856412));
#26198=CARTESIAN_POINT('Ctrl Pts',(2.37828958660479,-2.74628708545935,24.3645287774285));
#26199=CARTESIAN_POINT('Ctrl Pts',(2.28935576945552,-2.82360475294287,24.3612714210233));
#26200=CARTESIAN_POINT('Ctrl Pts',(2.2004312170102,-2.9009143658379,24.358014403954));
#26201=CARTESIAN_POINT('Ctrl Pts',(2.10806196086699,-2.97393178300944,24.354765107854));
#26202=CARTESIAN_POINT('Ctrl Pts',(2.01253765634337,-3.04233309530011,24.3515196700154));
#26203=CARTESIAN_POINT('Ctrl Pts',(1.91831994223422,-3.10979880801304,24.3483186235807));
#26204=CARTESIAN_POINT('Ctrl Pts',(1.82103227216761,-3.17277441103138,24.345121330582));
#26205=CARTESIAN_POINT('Ctrl Pts',(1.72092180235263,-3.23090982550694,24.3419240846569));
#26206=CARTESIAN_POINT('Ctrl Pts',(1.63731823238491,-3.27945947471638,24.3392540225356));
#26207=CARTESIAN_POINT('Ctrl Pts',(1.55174530961941,-3.32463302100756,24.3365839932441));
#26208=CARTESIAN_POINT('Ctrl Pts',(1.46433480530475,-3.3662006160568,24.3339118381243));
#26209=CARTESIAN_POINT('Ctrl Pts',(1.44360953039847,-3.37605640903435,24.3332782626761));
#26210=CARTESIAN_POINT('Ctrl Pts',(1.42277595537401,-3.38571149112601,24.3326444189594));
#26211=CARTESIAN_POINT('Ctrl Pts',(1.40186473452666,-3.39514984035219,24.3320111514667));
#26212=CARTESIAN_POINT('Ctrl Pts',(1.33458120918284,-3.42551848377093,24.3299735626666));
#26213=CARTESIAN_POINT('Ctrl Pts',(1.2664465713012,-3.45366766831798,24.3279404681835));
#26214=CARTESIAN_POINT('Ctrl Pts',(1.19753254997869,-3.47952152342011,24.3259109394442));
#26215=CARTESIAN_POINT('Ctrl Pts',(1.09102290473056,-3.51947979145293,24.3227742136821));
#26216=CARTESIAN_POINT('Ctrl Pts',(0.982652679880705,-3.55395790982246,
24.3196460054332));
#26217=CARTESIAN_POINT('Ctrl Pts',(0.872822247400536,-3.58310705179026,
24.3165228865437));
#26218=CARTESIAN_POINT('Ctrl Pts',(0.760371906501168,-3.61295152091583,
24.3133252683986));
#26219=CARTESIAN_POINT('Ctrl Pts',(0.646390155341705,-3.6372098459968,24.3101329853132));
#26220=CARTESIAN_POINT('Ctrl Pts',(0.53128616178814,-3.6559936831665,24.3069423579087));
#26221=CARTESIAN_POINT('Ctrl Pts',(0.41453738712084,-3.67504593240137,24.3037061379619));
#26222=CARTESIAN_POINT('Ctrl Pts',(0.296633230443278,-3.68846615738096,
24.3004716213517));
#26223=CARTESIAN_POINT('Ctrl Pts',(0.177991630975357,-3.69631848981734,
24.2972349687049));
#26224=CARTESIAN_POINT('Ctrl Pts',(0.142360760405031,-3.69867673045107,
24.2962629255763));
#26225=CARTESIAN_POINT('Ctrl Pts',(0.1066633636693,-3.70053242315808,24.2952906897893));
#26226=CARTESIAN_POINT('Ctrl Pts',(0.0709107847277581,-3.70188639298558,
24.2943181573453));
#26227=CARTESIAN_POINT('Ctrl Pts',(0.0511417931589634,-3.70263505556873,
24.2937804063283));
#26228=CARTESIAN_POINT('Ctrl Pts',(0.0313540742527653,-3.70323026849973,
24.2932425143369));
#26229=CARTESIAN_POINT('Ctrl Pts',(0.0115717980804544,-3.70367187863094,
24.2927050676203));
#26230=CARTESIAN_POINT('Ctrl Pts',(-0.107433551546183,-3.70632849749549,
24.2894719192276));
#26231=CARTESIAN_POINT('Ctrl Pts',(-0.226418918411982,-3.7034386910525,
24.2862500321799));
#26232=CARTESIAN_POINT('Ctrl Pts',(-0.344959013740293,-3.6951464558983,
24.2830356970017));
#26233=CARTESIAN_POINT('Ctrl Pts',(-0.464907323931171,-3.68675571189142,
24.2797831766461));
#26234=CARTESIAN_POINT('Ctrl Pts',(-0.584400592051045,-3.67283340149898,
24.2765383886529));
#26235=CARTESIAN_POINT('Ctrl Pts',(-0.703006950795025,-3.65347561626452,
24.2732974897681));
#26236=CARTESIAN_POINT('Ctrl Pts',(-0.821420460393264,-3.63414930600648,
24.2700618604539));
#26237=CARTESIAN_POINT('Ctrl Pts',(-0.938950841911184,-3.6094050645999,
24.2668301076113));
#26238=CARTESIAN_POINT('Ctrl Pts',(-1.05516365811085,-3.57928709699041,
24.2635984067028));
#26239=CARTESIAN_POINT('Ctrl Pts',(-1.11307514573956,-3.56427862920126,
24.261987976689));
#26240=CARTESIAN_POINT('Ctrl Pts',(-1.17065929149193,-3.5479349386455,24.2603775595719));
#26241=CARTESIAN_POINT('Ctrl Pts',(-1.22786083460473,-3.53025684653982,
24.258766682079));
#26242=CARTESIAN_POINT('Ctrl Pts',(-1.27025654792723,-3.5171544845367,24.2575727579877));
#26243=CARTESIAN_POINT('Ctrl Pts',(-1.31244206756123,-3.50331904033182,
24.256378581001));
#26244=CARTESIAN_POINT('Ctrl Pts',(-1.35439435742328,-3.48874976896511,
24.2551839584315));
#26245=CARTESIAN_POINT('Ctrl Pts',(-1.37450122726203,-3.48176701679641,
24.2546114003997));
#26246=CARTESIAN_POINT('Ctrl Pts',(-1.39455787836581,-3.47461436152618,
24.2540386428268));
#26247=CARTESIAN_POINT('Ctrl Pts',(-1.4145370881139,-3.46730094250551,24.2534663728415));
#26248=CARTESIAN_POINT('Ctrl Pts',(-1.52840519986039,-3.42561935325375,
24.2502048172814));
#26249=CARTESIAN_POINT('Ctrl Pts',(-1.63991365982444,-3.37866812586214,
24.2469546926609));
#26250=CARTESIAN_POINT('Ctrl Pts',(-1.74863318528068,-3.32654324532194,
24.2437121916767));
#26251=CARTESIAN_POINT('Ctrl Pts',(-1.85558872732241,-3.27526409533814,
24.2405223005429));
#26252=CARTESIAN_POINT('Ctrl Pts',(-1.95984592910298,-3.2189775652086,24.2373397876639));
#26253=CARTESIAN_POINT('Ctrl Pts',(-2.06098377301333,-3.15772709883281,
24.2341610280672));
#26254=CARTESIAN_POINT('Ctrl Pts',(-2.15682437201784,-3.09968471667599,
24.2311487607293));
#26255=CARTESIAN_POINT('Ctrl Pts',(-2.24986433245661,-3.03718433413316,
24.2281398638026));
#26256=CARTESIAN_POINT('Ctrl Pts',(-2.33972491633012,-2.97022484402709,
24.2251312525923));
#26257=CARTESIAN_POINT('Ctrl Pts',(-2.39708388099203,-2.9274838906389,24.2232108241167));
#26258=CARTESIAN_POINT('Ctrl Pts',(-2.45314695486067,-2.88292530873872,
24.2212905120536));
#26259=CARTESIAN_POINT('Ctrl Pts',(-2.50788173230019,-2.8366336564438,24.2193695141552));
#26260=CARTESIAN_POINT('Ctrl Pts',(-2.53563831690701,-2.81315866990653,
24.2183953558013));
#26261=CARTESIAN_POINT('Ctrl Pts',(-2.56305323963533,-2.78923792330051,
24.2174210210771));
#26262=CARTESIAN_POINT('Ctrl Pts',(-2.59012178635459,-2.76488197889541,
24.2164464053624));
#26263=CARTESIAN_POINT('Ctrl Pts',(-2.60345465688749,-2.75288522647173,
24.2159663491083));
#26264=CARTESIAN_POINT('Ctrl Pts',(-2.61670472847459,-2.74078173073675,
24.2154861793416));
#26265=CARTESIAN_POINT('Ctrl Pts',(-2.62986751863965,-2.72857633888938,
24.2150060254729));
#26266=CARTESIAN_POINT('Ctrl Pts',(-2.71508215755265,-2.6495598047031,24.2118975554583));
#26267=CARTESIAN_POINT('Ctrl Pts',(-2.79636860051037,-2.56653035928709,
24.2087997059384));
#26268=CARTESIAN_POINT('Ctrl Pts',(-2.87364584295152,-2.47991615691849,
24.2057091871955));
#26269=CARTESIAN_POINT('Ctrl Pts',(-2.95372207710542,-2.39016477694134,
24.2025067294641));
#26270=CARTESIAN_POINT('Ctrl Pts',(-3.02949395217132,-2.29656378485085,
24.1993121431703));
#26271=CARTESIAN_POINT('Ctrl Pts',(-3.10083927390671,-2.19954365518354,
24.1961217680305));
#26272=CARTESIAN_POINT('Ctrl Pts',(-3.1729388167544,-2.1014978853154,24.1928976661062));
#26273=CARTESIAN_POINT('Ctrl Pts',(-3.24051817780072,-1.99995957525359,
24.1896778648424));
#26274=CARTESIAN_POINT('Ctrl Pts',(-3.30341172612255,-1.89533643715524,
24.1864585866407));
#26275=CARTESIAN_POINT('Ctrl Pts',(-3.34638934220069,-1.82384336382643,
24.1842587282087));
#26276=CARTESIAN_POINT('Ctrl Pts',(-3.38717808530971,-1.7509090628703,24.1820591140217));
#26277=CARTESIAN_POINT('Ctrl Pts',(-3.42571297641979,-1.67665668248674,
24.1798585386985));
#26278=CARTESIAN_POINT('Ctrl Pts',(-3.445014281687,-1.63946524845605,24.1787563174426));
#26279=CARTESIAN_POINT('Ctrl Pts',(-3.46374997985981,-1.60194306216562,
24.1776538550573));
#26280=CARTESIAN_POINT('Ctrl Pts',(-3.48191088985649,-1.56410523444394,
24.1765510000744));
#26281=CARTESIAN_POINT('Ctrl Pts',(-3.49096642636183,-1.54523823767566,
24.1760010858047));
#26282=CARTESIAN_POINT('Ctrl Pts',(-3.4998801459806,-1.52629016625364,24.1754509999921));
#26283=CARTESIAN_POINT('Ctrl Pts',(-3.50864077925426,-1.5072853111527,24.174901369431));
#26284=CARTESIAN_POINT('Ctrl Pts',(-3.56003841051657,-1.39578600463474,
24.171676749928));
#26285=CARTESIAN_POINT('Ctrl Pts',(-3.60624692934267,-1.28217850112835,
24.1684632179365));
#26286=CARTESIAN_POINT('Ctrl Pts',(-3.6471387300781,-1.1668916502069,24.1652570948759));
#26287=CARTESIAN_POINT('Ctrl Pts',(-3.6882879122029,-1.05087916017607,24.1620307918185));
#26288=CARTESIAN_POINT('Ctrl Pts',(-3.72405366249247,-0.933165324275529,
24.1588119912523));
#26289=CARTESIAN_POINT('Ctrl Pts',(-3.75426180619985,-0.814159485558989,
24.1555969446976));
#26290=CARTESIAN_POINT('Ctrl Pts',(-3.7841716362032,-0.696328862138458,
24.1524136476093));
#26291=CARTESIAN_POINT('Ctrl Pts',(-3.80863339059432,-0.577230809008665,
24.1492340307549));
#26292=CARTESIAN_POINT('Ctrl Pts',(-3.8274295805391,-0.457247749762826,
24.1460544556133));
#26293=CARTESIAN_POINT('Ctrl Pts',(-3.83933667583213,-0.381240339527709,
24.1440402439932));
#26294=CARTESIAN_POINT('Ctrl Pts',(-3.84896918346273,-0.304877515113294,
24.1420260491124));
#26295=CARTESIAN_POINT('Ctrl Pts',(-3.85626072121049,-0.2282555949368,24.14001094599));
#26296=CARTESIAN_POINT('Ctrl Pts',(-3.85942265273046,-0.195028959773208,
24.1391371086324));
#26297=CARTESIAN_POINT('Ctrl Pts',(-3.86214425712046,-0.161753603333563,
24.1382631004825));
#26298=CARTESIAN_POINT('Ctrl Pts',(-3.86441958153066,-0.128437410079632,
24.1373888461123));
#26299=CARTESIAN_POINT('Ctrl Pts',(-3.86591347492261,-0.106563236566722,
24.1368148432051));
#26300=CARTESIAN_POINT('Ctrl Pts',(-3.86721509040623,-0.0846675012688186,
24.1362406305225));
#26301=CARTESIAN_POINT('Ctrl Pts',(-3.86832155925171,-0.0627797067798542,
24.1356669009074));
#26302=CARTESIAN_POINT('Ctrl Pts',(-3.86941608558997,-0.0411281549512009,
24.1350993637576));
#26303=CARTESIAN_POINT('Ctrl Pts',(-3.87032006240666,-0.0194794249965481,
24.1345321693282));
#26304=CARTESIAN_POINT('Ctrl Pts',(-3.87103266938659,0.00216425178203038,
24.1339652975667));
#26305=CARTESIAN_POINT('',(0.349572399382967,3.92005776261121,24.058));
#26306=CARTESIAN_POINT('Ctrl Pts',(0.349418900843753,3.91916189049795,24.058));
#26307=CARTESIAN_POINT('Ctrl Pts',(0.226012228632792,3.91828850060595,24.0696807256992));
#26308=CARTESIAN_POINT('Ctrl Pts',(0.102952431902507,3.91191927543051,24.0813859465783));
#26309=CARTESIAN_POINT('Ctrl Pts',(-0.0193397180673949,3.90006603014558,
24.0931306202039));
#26310=CARTESIAN_POINT('Ctrl Pts',(-0.140580622517234,3.88831467750876,
24.1047743344831));
#26311=CARTESIAN_POINT('Ctrl Pts',(-0.261067870571708,3.87117297838718,
24.1164568261384));
#26312=CARTESIAN_POINT('Ctrl Pts',(-0.380377476123202,3.84860347157658,
24.1281926703091));
#26313=CARTESIAN_POINT('Ctrl Pts',(-0.496161715673067,3.82670084964599,
24.1395817431879));
#26314=CARTESIAN_POINT('Ctrl Pts',(-0.610837511562959,3.79968611836398,
24.1510210622381));
#26315=CARTESIAN_POINT('Ctrl Pts',(-0.723993462162786,3.76748283972913,
24.1625239483983));
#26316=CARTESIAN_POINT('Ctrl Pts',(-0.796757989013667,3.74677463728383,
24.1699208379514));
#26317=CARTESIAN_POINT('Ctrl Pts',(-0.868893538246561,3.72392009045816,
24.177344013056));
#26318=CARTESIAN_POINT('Ctrl Pts',(-0.940283456718533,3.69889010045098,
24.1847970158196));
#26319=CARTESIAN_POINT('Ctrl Pts',(-0.958852956027486,3.69237945592175,
24.1867356443071));
#26320=CARTESIAN_POINT('Ctrl Pts',(-0.977371972215163,3.6857215872702,24.188676290909));
#26321=CARTESIAN_POINT('Ctrl Pts',(-0.995838377017294,3.67891590798256,
24.1906190179632));
#26322=CARTESIAN_POINT('Ctrl Pts',(-1.01171569758055,3.67306441967942,24.1922893647652));
#26323=CARTESIAN_POINT('Ctrl Pts',(-1.0275456693922,3.66710676559807,24.1939603606721));
#26324=CARTESIAN_POINT('Ctrl Pts',(-1.04332469128769,3.6610438482036,24.1956317888384));
#26325=CARTESIAN_POINT('Ctrl Pts',(-1.15165978098886,3.619417269311,24.2071074253844));
#26326=CARTESIAN_POINT('Ctrl Pts',(-1.25763328276278,3.57281828211811,24.2186074516257));
#26327=CARTESIAN_POINT('Ctrl Pts',(-1.36087067794145,3.52121736057027,24.2301462409952));
#26328=CARTESIAN_POINT('Ctrl Pts',(-1.42681061365643,3.48825874665126,24.2375163129341));
#26329=CARTESIAN_POINT('Ctrl Pts',(-1.49163388388109,3.45325861360399,24.2449021988746));
#26330=CARTESIAN_POINT('Ctrl Pts',(-1.55523660610354,3.41620000588947,24.2523076441887));
#26331=CARTESIAN_POINT('Ctrl Pts',(-1.65681419035516,3.35701505726094,24.2641346103786));
#26332=CARTESIAN_POINT('Ctrl Pts',(-1.75528075449242,3.2925810923405,24.276011464936));
#26333=CARTESIAN_POINT('Ctrl Pts',(-1.8504118158475,3.22325698482629,24.2879534645915));
#26334=CARTESIAN_POINT('Ctrl Pts',(-1.94589009699015,3.15367985057672,24.2999390514679));
#26335=CARTESIAN_POINT('Ctrl Pts',(-2.03800893445419,3.07917596454707,24.3119902598576));
#26336=CARTESIAN_POINT('Ctrl Pts',(-2.12649675572721,3.00008130698686,24.3241225141588));
#26337=CARTESIAN_POINT('Ctrl Pts',(-2.15464819134299,2.97491820399908,24.3279822585951));
#26338=CARTESIAN_POINT('Ctrl Pts',(-2.18243175770649,2.94929030687597,24.3318502058895));
#26339=CARTESIAN_POINT('Ctrl Pts',(-2.20983765373967,2.92320808164845,24.3357268527022));
#26340=CARTESIAN_POINT('Ctrl Pts',(-2.22035441337321,2.91319926846847,24.3372144801333));
#26341=CARTESIAN_POINT('Ctrl Pts',(-2.23081386252428,2.90312511161636,24.3387031532638));
#26342=CARTESIAN_POINT('Ctrl Pts',(-2.24120927897093,2.89299245114185,24.3401919995702));
#26343=CARTESIAN_POINT('Ctrl Pts',(-2.32385350748897,2.81243714948096,24.3520284233442));
#26344=CARTESIAN_POINT('Ctrl Pts',(-2.40257000364209,2.72807711715171,24.3638921677319));
#26345=CARTESIAN_POINT('Ctrl Pts',(-2.47717616028223,2.64027648475023,24.3757991858546));
#26346=CARTESIAN_POINT('Ctrl Pts',(-2.55187618325755,2.55236538527792,24.3877211848877));
#26347=CARTESIAN_POINT('Ctrl Pts',(-2.62245590857137,2.46100416174114,24.3996865666148));
#26348=CARTESIAN_POINT('Ctrl Pts',(-2.68868744355177,2.36653097722017,24.4117113444476));
#26349=CARTESIAN_POINT('Ctrl Pts',(-2.75414075468922,2.27316785733437,24.4235948305405));
#26350=CARTESIAN_POINT('Ctrl Pts',(-2.81534772258566,2.17676464445494,24.4355363251252));
#26351=CARTESIAN_POINT('Ctrl Pts',(-2.8720401475082,2.07763370148774,24.4475512837449));
#26352=CARTESIAN_POINT('Ctrl Pts',(-2.90668546327039,2.01705377699881,24.4548937467957));
#26353=CARTESIAN_POINT('Ctrl Pts',(-2.93964383947717,1.95545494636204,24.462263645402));
#26354=CARTESIAN_POINT('Ctrl Pts',(-2.97084438937695,1.89290785453322,24.4696645068668));
#26355=CARTESIAN_POINT('Ctrl Pts',(-2.98845779797902,1.85759862156167,24.4738424587748));
#26356=CARTESIAN_POINT('Ctrl Pts',(-3.00551087593063,1.82198719162217,24.4780302780973));
#26357=CARTESIAN_POINT('Ctrl Pts',(-3.02198977071177,1.78608635326393,24.4822285994141));
#26358=CARTESIAN_POINT('Ctrl Pts',(-3.02877383007556,1.77130663521446,24.4839569714572));
#26359=CARTESIAN_POINT('Ctrl Pts',(-3.03545687173813,1.75648588102819,24.4856861859929));
#26360=CARTESIAN_POINT('Ctrl Pts',(-3.04203688563128,1.74162824455868,24.4874159221199));
#26361=CARTESIAN_POINT('Ctrl Pts',(-3.08710741956134,1.63985921800425,24.4992639412984));
#26362=CARTESIAN_POINT('Ctrl Pts',(-3.12737033179139,1.53631268431983,24.5111420689289));
#26363=CARTESIAN_POINT('Ctrl Pts',(-3.16262066493997,1.43129464400087,24.5230664886917));
#26364=CARTESIAN_POINT('Ctrl Pts',(-3.19738804194613,1.32771543001649,24.534827534913));
#26365=CARTESIAN_POINT('Ctrl Pts',(-3.22727942618041,1.22270400117247,24.5466336134818));
#26366=CARTESIAN_POINT('Ctrl Pts',(-3.2520488351859,1.1165476391786,24.5585002519648));
#26367=CARTESIAN_POINT('Ctrl Pts',(-3.27606482816892,1.01362025628536,24.5700059405533));
#26368=CARTESIAN_POINT('Ctrl Pts',(-3.29526569753493,0.909615922196257,
24.5815685609605));
#26369=CARTESIAN_POINT('Ctrl Pts',(-3.3093795070715,0.804800410213191,24.5932022664991));
#26370=CARTESIAN_POINT('Ctrl Pts',(-3.32346107752391,0.700224320202117,
24.6048093980635));
#26371=CARTESIAN_POINT('Ctrl Pts',(-3.33247901104835,0.594840172393064,
24.6164872903817));
#26372=CARTESIAN_POINT('Ctrl Pts',(-3.33611311329483,0.488924695430968,
24.62825));
#26373=CARTESIAN_POINT('',(-2.87185821835411,2.69480181882395,24.058));
#26374=CARTESIAN_POINT('Origin',(0.,0.,24.058));
#26375=CARTESIAN_POINT('Ctrl Pts',(-3.87103266938659,0.00216425178203038,
24.1339652975667));
#26376=CARTESIAN_POINT('Ctrl Pts',(-3.87507260628243,0.124867355795072,
24.1307515679672));
#26377=CARTESIAN_POINT('Ctrl Pts',(-3.87296594485587,0.247407050622043,
24.1275482085216));
#26378=CARTESIAN_POINT('Ctrl Pts',(-3.86453408452217,0.369385378863034,
24.1243515657403));
#26379=CARTESIAN_POINT('Ctrl Pts',(-3.85627040623579,0.488930725038259,
24.1212186832571));
#26380=CARTESIAN_POINT('Ctrl Pts',(-3.84193179212873,0.607937675272044,
24.1180922521689));
#26381=CARTESIAN_POINT('Ctrl Pts',(-3.82181791447054,0.726086832854309,
24.1149688332722));
#26382=CARTESIAN_POINT('Ctrl Pts',(-3.80134858411548,0.846323923823187,
24.1117902172779));
#26383=CARTESIAN_POINT('Ctrl Pts',(-3.77489779988944,0.965673358591756,
24.1086147208788));
#26384=CARTESIAN_POINT('Ctrl Pts',(-3.74272692791689,1.08379247292844,24.1054387192973));
#26385=CARTESIAN_POINT('Ctrl Pts',(-3.72259049299425,1.15772574589009,24.1034507921682));
#26386=CARTESIAN_POINT('Ctrl Pts',(-3.70021198877918,1.23117684933353,24.1014626671201));
#26387=CARTESIAN_POINT('Ctrl Pts',(-3.67564568396927,1.30405861901184,24.099473455278));
#26388=CARTESIAN_POINT('Ctrl Pts',(-3.66863540268018,1.32485628110409,24.0989058105034));
#26389=CARTESIAN_POINT('Ctrl Pts',(-3.66144692163609,1.3456075617141,24.0983380772297));
#26390=CARTESIAN_POINT('Ctrl Pts',(-3.65408139767167,1.36631038395308,24.097770234802));
#26391=CARTESIAN_POINT('Ctrl Pts',(-3.64822216373193,1.38277936556212,24.0973185192633));
#26392=CARTESIAN_POINT('Ctrl Pts',(-3.64225062386782,1.39921823302553,24.0968667189574));
#26393=CARTESIAN_POINT('Ctrl Pts',(-3.63617302699739,1.41561112341376,24.0964152327823));
#26394=CARTESIAN_POINT('Ctrl Pts',(-3.59274946073352,1.53273599648544,24.0931894281991));
#26395=CARTESIAN_POINT('Ctrl Pts',(-3.54385270980084,1.6476965516567,24.0899746657265));
#26396=CARTESIAN_POINT('Ctrl Pts',(-3.48981414813695,1.76015005122282,24.0867672641288));
#26397=CARTESIAN_POINT('Ctrl Pts',(-3.43581118825365,1.87252946397587,24.0835619756371));
#26398=CARTESIAN_POINT('Ctrl Pts',(-3.37667270383973,1.98240587688454,24.0803640383244));
#26399=CARTESIAN_POINT('Ctrl Pts',(-3.31267597495322,2.08942561654219,24.0771697782258));
#26400=CARTESIAN_POINT('Ctrl Pts',(-3.24861596071611,2.19655118632369,24.0739723593741));
#26401=CARTESIAN_POINT('Ctrl Pts',(-3.17968763174453,2.30081519811777,24.0707786250127));
#26402=CARTESIAN_POINT('Ctrl Pts',(-3.10612258128374,2.40183988004365,24.0675848902668));
#26403=CARTESIAN_POINT('Ctrl Pts',(-3.03255753082295,2.50286456196954,24.0643911555208));
#26404=CARTESIAN_POINT('Ctrl Pts',(-2.95435530373159,2.60065069905013,24.0611974203902));
#26405=CARTESIAN_POINT('Ctrl Pts',(-2.87170785494336,2.69478584831407,24.058));
#26406=CARTESIAN_POINT('',(-3.,-3.67394039744206E-16,25.));
#26407=CARTESIAN_POINT('',(-3.5,-4.28626379701574E-16,24.5));
#26408=CARTESIAN_POINT('Origin',(0.,0.,25.));
#26409=CARTESIAN_POINT('Ctrl Pts',(2.28870316125076,-3.20954854141214,-0.329233991005384));
#26410=CARTESIAN_POINT('Ctrl Pts',(3.35678472141098,-2.44790820113649,-0.27627001251076));
#26411=CARTESIAN_POINT('Ctrl Pts',(4.65420965805454,0.212376298523761,-0.170342055521513));
#26412=CARTESIAN_POINT('Ctrl Pts',(2.33824086975704,4.03501766412881,-0.011450120037642));
#26413=CARTESIAN_POINT('Ctrl Pts',(-2.12304297015552,4.14730362817999,0.147441815446229));
#26414=CARTESIAN_POINT('Ctrl Pts',(-4.6372363620278,0.464007918031343,0.3063337509301));
#26415=CARTESIAN_POINT('Ctrl Pts',(-2.9014296726223,-3.64766420030675,0.46522568641397));
#26416=CARTESIAN_POINT('Ctrl Pts',(1.49416848835415,-4.41423135892847,0.624117621897843));
#26417=CARTESIAN_POINT('Ctrl Pts',(4.52003362949604,-1.13548107251883,0.783009557381712));
#26418=CARTESIAN_POINT('Ctrl Pts',(3.40284567859094,3.18450706915039,0.941901492865584));
#26419=CARTESIAN_POINT('Ctrl Pts',(-0.833486649302243,4.58529649769934,
1.10079342834945));
#26420=CARTESIAN_POINT('Ctrl Pts',(-4.30580977810473,1.78325097864793,1.25968536383333));
#26421=CARTESIAN_POINT('Ctrl Pts',(-3.83137142736725,-2.65341337269076,
1.4185772993172));
#26422=CARTESIAN_POINT('Ctrl Pts',(0.154968444518143,-4.65788428232239,
1.57746923480107));
#26423=CARTESIAN_POINT('Ctrl Pts',(3.99925861063605,-2.3928822888867,1.73636117028494));
#26424=CARTESIAN_POINT('Ctrl Pts',(4.17776697308586,2.065482350747,1.89525310576881));
#26425=CARTESIAN_POINT('Ctrl Pts',(0.526867410782717,4.63058858791146,2.05414504125268));
#26426=CARTESIAN_POINT('Ctrl Pts',(-3.60696666633743,2.95122682044694,2.21303697673655));
#26427=CARTESIAN_POINT('Ctrl Pts',(-4.43459848935502,-1.43327725922984,
2.37192891222043));
#26428=CARTESIAN_POINT('Ctrl Pts',(-1.19740732042406,-4.50401613542707,
2.53082084770429));
#26429=CARTESIAN_POINT('Ctrl Pts',(3.13734620436576,-3.44630319202068,2.68971278318817));
#26430=CARTESIAN_POINT('Ctrl Pts',(4.59635878672289,0.770345758451563,2.84860471867204));
#26431=CARTESIAN_POINT('Ctrl Pts',(1.84227644659507,4.28088354832699,3.00749665415591));
#26432=CARTESIAN_POINT('Ctrl Pts',(-2.60046551010954,3.86749606027826,3.16638858963978));
#26433=CARTESIAN_POINT('Ctrl Pts',(-4.65957980074616,-0.0908992967115246,
3.32528052512365));
#26434=CARTESIAN_POINT('Ctrl Pts',(-2.44764980647886,-3.96597491173744,
3.48417246060752));
#26435=CARTESIAN_POINT('Ctrl Pts',(2.00783457505236,-4.20577542454142,3.64306439609139));
#26436=CARTESIAN_POINT('Ctrl Pts',(4.62290614147485,-0.590495894571063,
3.80195633157526));
#26437=CARTESIAN_POINT('Ctrl Pts',(3.00054907928836,3.56604147682096,3.96084826705914));
#26438=CARTESIAN_POINT('Ctrl Pts',(-1.37215855870585,4.45388902928383,4.119740202543));
#26439=CARTESIAN_POINT('Ctrl Pts',(-4.48712403609106,1.2592317017741,4.27863213802688));
#26440=CARTESIAN_POINT('Ctrl Pts',(-3.48912090296361,-3.08965724931931,
4.43752407351074));
#26441=CARTESIAN_POINT('Ctrl Pts',(0.707065439817984,-4.60651767152865,
4.59641600899462));
#26442=CARTESIAN_POINT('Ctrl Pts',(4.25514445682574,-1.9009713952631,4.75530794447848));
#26443=CARTESIAN_POINT('Ctrl Pts',(3.90289100181761,2.54703522197484,4.91419987996237));
#26444=CARTESIAN_POINT('Ctrl Pts',(-0.0268138566703869,4.6603892124167,
5.07309181544622));
#26445=CARTESIAN_POINT('Ctrl Pts',(-3.93194071153866,2.50195700103508,5.23198375093011));
#26446=CARTESIAN_POINT('Ctrl Pts',(-4.23298874115587,-1.9498084293931,5.39087568641397));
#26447=CARTESIAN_POINT('Ctrl Pts',(-0.654012576931896,-4.61434872363465,
5.54976762189785));
#26448=CARTESIAN_POINT('Ctrl Pts',(3.52444182282379,-3.04930425369769,5.70865955738171));
#26449=CARTESIAN_POINT('Ctrl Pts',(4.47233730108079,1.31078055350635,5.86755149286558));
#26450=CARTESIAN_POINT('Ctrl Pts',(1.32081792323409,4.46938324690933,6.02644342834946));
#26451=CARTESIAN_POINT('Ctrl Pts',(-3.04138397969982,3.531278816819,6.18533536383333));
#26452=CARTESIAN_POINT('Ctrl Pts',(-4.61580539333909,-0.643651431219671,
6.3442272993172));
#26453=CARTESIAN_POINT('Ctrl Pts',(-1.95930683639269,-4.22860063318286,
6.50311923480107));
#26454=CARTESIAN_POINT('Ctrl Pts',(2.4931232462982,-3.93754785023079,6.66201117028494));
#26455=CARTESIAN_POINT('Ctrl Pts',(4.66031726875216,-0.037276650332675,
6.82090310576881));
#26456=CARTESIAN_POINT('Ctrl Pts',(2.55579103409072,3.8971629147562,6.97979504125268));
#26457=CARTESIAN_POINT('Ctrl Pts',(-1.89141354276916,4.25940153123874,7.13868697673655));
#26458=CARTESIAN_POINT('Ctrl Pts',(-4.60491865684703,0.717405574212831,
7.29757891222042));
#26459=CARTESIAN_POINT('Ctrl Pts',(-3.09748275458741,-3.48217563875277,
7.45647084770429));
#26460=CARTESIAN_POINT('Ctrl Pts',(1.24915465816929,-4.48993978067229,7.61536278318817));
#26461=CARTESIAN_POINT('Ctrl Pts',(4.45079722404066,-1.38215435627192,7.77425471867203));
#26462=CARTESIAN_POINT('Ctrl Pts',(3.57276890790401,2.99253553442627,7.93314665415592));
#26463=CARTESIAN_POINT('Ctrl Pts',(-0.580115697571088,4.62422019063984,
8.09203858963977));
#26464=CARTESIAN_POINT('Ctrl Pts',(-4.20125711178304,2.01727174044104,8.25093052512366));
#26465=CARTESIAN_POINT('Ctrl Pts',(-3.97146004374031,-2.43873978010442,
8.40982246060752));
#26466=CARTESIAN_POINT('Ctrl Pts',(-0.101360107710164,-4.65936398263266,
8.56871439609139));
#26467=CARTESIAN_POINT('Ctrl Pts',(3.86164810052541,-2.60914172512687,8.72760633157527));
#26468=CARTESIAN_POINT('Ctrl Pts',(4.28500879860717,1.83266095881065,8.88649826705913));
#26469=CARTESIAN_POINT('Ctrl Pts',(0.78066289832912,4.59461772438818,9.04539020254301));
#26470=CARTESIAN_POINT('Ctrl Pts',(-3.43925091813584,3.14507547066701,9.20428213802687));
#26471=CARTESIAN_POINT('Ctrl Pts',(-4.50669313898401,-1.18729252719113,
9.36317407351076));
#26472=CARTESIAN_POINT('Ctrl Pts',(-1.44322940124376,-4.431369482392,9.52206600899461));
#26473=CARTESIAN_POINT('Ctrl Pts',(2.94312115158416,-3.61358332976944,9.6809579444785));
#26474=CARTESIAN_POINT('Ctrl Pts',(4.63176047203213,0.516470254526036,9.83984987996235));
#26475=CARTESIAN_POINT('Ctrl Pts',(2.07485514530555,4.17311906373262,9.99874181544625));
#26476=CARTESIAN_POINT('Ctrl Pts',(-2.3838951082054,4.00462116899514,10.1576337509301));
#26477=CARTESIAN_POINT('Ctrl Pts',(-4.65752953433707,0.165424396228235,
10.316525686414));
#26478=CARTESIAN_POINT('Ctrl Pts',(-2.6619989846541,-3.82540298528012,10.4754176218978));
#26479=CARTESIAN_POINT('Ctrl Pts',(1.77356178859607,-4.30980570050686,10.6343095573817));
#26480=CARTESIAN_POINT('Ctrl Pts',(4.58344787433293,-0.843772586282874,
10.7932014928656));
#26481=CARTESIAN_POINT('Ctrl Pts',(3.19207340137333,3.39567577874192,10.9520934283495));
#26482=CARTESIAN_POINT('Ctrl Pts',(-1.12520585971602,4.52259420768106,11.1109853638333));
#26483=CARTESIAN_POINT('Ctrl Pts',(-4.41110369606797,1.50403150785647,11.2698772993172));
#26484=CARTESIAN_POINT('Ctrl Pts',(-3.65371436373851,-2.89315017624395,
11.4287692348011));
#26485=CARTESIAN_POINT('Ctrl Pts',(0.452727138482009,-4.63842481152508,
11.5876611702849));
#26486=CARTESIAN_POINT('Ctrl Pts',(4.14419181039819,-2.13204616101957,11.7465531057688));
#26487=CARTESIAN_POINT('Ctrl Pts',(4.03702495468236,2.32859960262844,11.9054450412527));
#26488=CARTESIAN_POINT('Ctrl Pts',(0.229457400278859,4.65481427078963,12.0643369767365));
#26489=CARTESIAN_POINT('Ctrl Pts',(-3.78843442356625,2.7143528164975,12.2232289122204));
#26490=CARTESIAN_POINT('Ctrl Pts',(-4.33378754743687,-1.71412720874813,
12.3821208477043));
#26491=CARTESIAN_POINT('Ctrl Pts',(-0.906722702996628,-4.57141121908323,
12.5410127831882));
#26492=CARTESIAN_POINT('Ctrl Pts',(3.35145846134476,-3.23846765862655,12.699904718672));
#26493=CARTESIAN_POINT('Ctrl Pts',(4.53763997961045,1.06290639735133,12.8587966541559));
#26494=CARTESIAN_POINT('Ctrl Pts',(1.56454917743418,4.39000369766127,13.0176885896398));
#26495=CARTESIAN_POINT('Ctrl Pts',(-2.84263205873703,3.69315442037428,13.1765805251236));
#26496=CARTESIAN_POINT('Ctrl Pts',(-4.6442119487827,-0.388898404308158,
13.3354724606075));
#26497=CARTESIAN_POINT('Ctrl Pts',(-2.1888339718237,-4.11448082239789,13.4943643960914));
#26498=CARTESIAN_POINT('Ctrl Pts',(2.27286372066084,-4.06866527271454,13.6532563315753));
#26499=CARTESIAN_POINT('Ctrl Pts',(4.65121870549125,-0.293447010170337,
13.8121482670591));
#26500=CARTESIAN_POINT('Ctrl Pts',(2.76619331968842,3.75074940674537,13.971040202543));
#26501=CARTESIAN_POINT('Ctrl Pts',(-1.65436845932101,4.35694980403646,14.1299321380269));
#26502=CARTESIAN_POINT('Ctrl Pts',(-4.55851003496805,0.969501343570532,
14.2888240735108));
#26503=CARTESIAN_POINT('Ctrl Pts',(-3.28424946851144,-3.30660732816461,
14.4477160089946));
#26504=CARTESIAN_POINT('Ctrl Pts',(1.00040592194765,-4.55182760936985,14.6066079444785));
#26505=CARTESIAN_POINT('Ctrl Pts',(4.36807347752778,-1.62477096509257,14.7654998799624));
#26506=CARTESIAN_POINT('Ctrl Pts',(3.73189604091493,2.79157635286821,14.9243918154462));
#26507=CARTESIAN_POINT('Ctrl Pts',(-0.324996123065272,4.64912078936244,
15.0832837509301));
#26508=CARTESIAN_POINT('Ctrl Pts',(-4.08399171856711,2.24520783821119,15.242175686414));
#26509=CARTESIAN_POINT('Ctrl Pts',(-4.09953613938831,-2.21669800287246,
15.4010676218978));
#26510=CARTESIAN_POINT('Ctrl Pts',(-0.357381124417536,-4.64674351842229,
15.5599595573817));
#26511=CARTESIAN_POINT('Ctrl Pts',(3.71235506167248,-2.81751069033718,15.7188514928656));
#26512=CARTESIAN_POINT('Ctrl Pts',(4.37928808994288,1.59429684167472,15.8777434283495));
#26513=CARTESIAN_POINT('Ctrl Pts',(1.03209663553355,4.54474676181302,16.0366353638333));
#26514=CARTESIAN_POINT('Ctrl Pts',(-3.26113086128664,3.32941017293654,16.1955272993172));
#26515=CARTESIAN_POINT('Ctrl Pts',(-4.56515441384568,-0.937716253370267,
16.3544192348011));
#26516=CARTESIAN_POINT('Ctrl Pts',(-1.68468548190361,-4.34531718303195,
16.5133111702849));
#26517=CARTESIAN_POINT('Ctrl Pts',(2.7399927141092,-3.76993189868439,16.6722031057688));
#26518=CARTESIAN_POINT('Ctrl Pts',(4.65315040492198,0.261032379723303,16.8310950412527));
#26519=CARTESIAN_POINT('Ctrl Pts',(2.30115709895892,4.05273026489556,16.9899869767366));
#26520=CARTESIAN_POINT('Ctrl Pts',(-2.16011307112194,4.12963171651633,17.1488789122204));
#26521=CARTESIAN_POINT('Ctrl Pts',(-4.64138955591407,0.421247652030533,
17.3077708477043));
#26522=CARTESIAN_POINT('Ctrl Pts',(-2.86829522348703,-3.67325864934817,
17.4666627831881));
#26523=CARTESIAN_POINT('Ctrl Pts',(1.53392371633779,-4.40079818061975,17.6255547186721));
#26524=CARTESIAN_POINT('Ctrl Pts',(4.53012400247882,-1.09449674108904,17.7844466541559));
#26525=CARTESIAN_POINT('Ctrl Pts',(3.37394123127184,3.21503766105686,17.9433385896398));
#26526=CARTESIAN_POINT('Ctrl Pts',(-0.874849247264209,4.57761787272052,
18.1022305251236));
#26527=CARTESIAN_POINT('Ctrl Pts',(-4.32173911776226,1.7442813970492,18.2611224606075));
#26528=CARTESIAN_POINT('Ctrl Pts',(-3.80725480047823,-2.68789089777271,
18.4200143960914));
#26529=CARTESIAN_POINT('Ctrl Pts',(0.197019270876202,-4.65630003339433,
18.5789063315753));
#26530=CARTESIAN_POINT('Ctrl Pts',(4.02070237343572,-2.35667117314485,18.7377982670591));
#26531=CARTESIAN_POINT('Ctrl Pts',(4.15894631253379,2.10311962655031,18.896690202543));
#26532=CARTESIAN_POINT('Ctrl Pts',(0.485034514796087,4.63515783048493,19.0555821380269));
#26533=CARTESIAN_POINT('Ctrl Pts',(-3.63346756353596,2.9185373149568,19.2144740735107));
#26534=CARTESIAN_POINT('Ctrl Pts',(-4.42147600817412,-1.47326050087259,
19.3733660089946));
#26535=CARTESIAN_POINT('Ctrl Pts',(-1.15668985931864,-4.51464452234266,
19.5322579444785));
#26536=CARTESIAN_POINT('Ctrl Pts',(3.16833644438965,-3.41783422201423,19.6911498799624));
#26537=CARTESIAN_POINT('Ctrl Pts',(4.58921562907606,0.811816792908698,19.8500418154462));
#26538=CARTESIAN_POINT('Ctrl Pts',(1.80354743972281,4.29734374053261,20.0089337509301));
#26539=CARTESIAN_POINT('Ctrl Pts',(-2.63528075670629,3.84385768827679,20.167825686414));
#26540=CARTESIAN_POINT('Ctrl Pts',(-4.65856908001299,-0.132968903128038,
20.3267176218978));
#26541=CARTESIAN_POINT('Ctrl Pts',(-2.41173956046629,-3.98791409989842,
20.4856095573818));
#26542=CARTESIAN_POINT('Ctrl Pts',(2.04572844434392,-4.18747438603111,20.6445014928655));
#26543=CARTESIAN_POINT('Ctrl Pts',(4.62804952678526,-0.548729644870818,
20.8033934283495));
#26544=CARTESIAN_POINT('Ctrl Pts',(2.96822745143777,3.59298932040533,20.9622853638333));
#26545=CARTESIAN_POINT('Ctrl Pts',(-1.4123186453351,4.44131767923527,21.1211772993172));
#26546=CARTESIAN_POINT('Ctrl Pts',(-4.49831129151882,1.21866419573831,21.2800692348011));
#26547=CARTESIAN_POINT('Ctrl Pts',(-3.46108076274892,-3.12103598071567,
21.438961170285));
#26548=CARTESIAN_POINT('Ctrl Pts',(0.748630655069918,-4.59994560901591,
21.5978531057688));
#26549=CARTESIAN_POINT('Ctrl Pts',(4.2721359622726,-1.86247217365839,21.7567450412527));
#26550=CARTESIAN_POINT('Ctrl Pts',(3.8797330719726,2.58217180475713,21.9156369767366));
#26551=CARTESIAN_POINT('Ctrl Pts',(-0.0688923048847857,4.65995794755513,
22.0745289122204));
#26552=CARTESIAN_POINT('Ctrl Pts',(-3.95437371638077,2.46635025785298,22.2334208477043));
#26553=CARTESIAN_POINT('Ctrl Pts',(-4.21520658614674,-1.98794734397253,
22.3923127831882));
#26554=CARTESIAN_POINT('Ctrl Pts',(-0.612328551070793,-4.62007178368083,
22.551204718672));
#26555=CARTESIAN_POINT('Ctrl Pts',(3.55184600275178,-3.01734516931811,22.7100966541559));
#26556=CARTESIAN_POINT('Ctrl Pts',(4.46029188758379,1.35108854037515,22.8689885896398));
#26557=CARTESIAN_POINT('Ctrl Pts',(1.28046065203078,4.48116776123978,23.0278805251236));
#26558=CARTESIAN_POINT('Ctrl Pts',(-3.07324571308582,3.50359559093557,23.1867724606075));
#26559=CARTESIAN_POINT('Ctrl Pts',(-4.60961384635985,-0.685155565682453,
23.3456643960914));
#26560=CARTESIAN_POINT('Ctrl Pts',(-1.9214110817744,-4.24640173773129,23.5045563315753));
#26561=CARTESIAN_POINT('Ctrl Pts',(2.52927486439223,-3.91433686410129,23.6634482670591));
#26562=CARTESIAN_POINT('Ctrl Pts',(4.65912272890548,0.00377285541425606,
23.822340202543));
#26563=CARTESIAN_POINT('Ctrl Pts',(2.52310591890791,3.92207527169042,23.9812321380269));
#26564=CARTESIAN_POINT('Ctrl Pts',(-1.93519005785514,4.23813764208779,24.1401240735107));
#26565=CARTESIAN_POINT('Ctrl Pts',(-3.71011270200011,1.86957801804229,24.2460520305));
#26566=CARTESIAN_POINT('Ctrl Pts',(-3.90033599543508,0.571614487844223,
24.2990160089946));
#26567=CARTESIAN_POINT('Ctrl Pts',(2.17834184062643,-3.05478403475391,-0.219489327336923));
#26568=CARTESIAN_POINT('Ctrl Pts',(3.19492048266714,-2.32987000971945,-0.166525348842299));
#26569=CARTESIAN_POINT('Ctrl Pts',(4.42978355814708,0.202135508380576,-0.0605973918530519));
#26570=CARTESIAN_POINT('Ctrl Pts',(2.22549083965568,3.84044901682883,0.0982945436308193));
#26571=CARTESIAN_POINT('Ctrl Pts',(-2.02066978786809,3.94732054903492,0.25718647911469));
#26572=CARTESIAN_POINT('Ctrl Pts',(-4.41362871485661,0.441633445237732,
0.416078414598561));
#26573=CARTESIAN_POINT('Ctrl Pts',(-2.76152266511234,-3.4717737462035,0.574970350082432));
#26574=CARTESIAN_POINT('Ctrl Pts',(1.42211964846881,-4.20137701828676,0.733862285566304));
#26575=CARTESIAN_POINT('Ctrl Pts',(4.30207750086251,-1.08072814831761,0.892754221050174));
#26576=CARTESIAN_POINT('Ctrl Pts',(3.23876037940132,3.03095006287751,1.05164615653404));
#26577=CARTESIAN_POINT('Ctrl Pts',(-0.793295903338713,4.36419339201584,
1.21053809201792));
#26578=CARTESIAN_POINT('Ctrl Pts',(-4.09818352865738,1.69726257423614,1.36943002750179));
#26579=CARTESIAN_POINT('Ctrl Pts',(-3.64662260642559,-2.52546571703568,
1.52832196298566));
#26580=CARTESIAN_POINT('Ctrl Pts',(0.147495862454333,-4.43328099194573,
1.68721389846953));
#26581=CARTESIAN_POINT('Ctrl Pts',(3.80641426574215,-2.27749744826117,1.8461058339534));
#26582=CARTESIAN_POINT('Ctrl Pts',(3.97631495072816,1.96588474289028,2.00499776943727));
#26583=CARTESIAN_POINT('Ctrl Pts',(0.501461851760338,4.40730149656556,2.16388970492114));
#26584=CARTESIAN_POINT('Ctrl Pts',(-3.43303864828577,2.80891859328985,2.32278164040501));
#26585=CARTESIAN_POINT('Ctrl Pts',(-4.22076204520191,-1.36416459585457,
2.48167357588889));
#26586=CARTESIAN_POINT('Ctrl Pts',(-1.13966831108264,-4.28683237073678,
2.64056551137275));
#26587=CARTESIAN_POINT('Ctrl Pts',(2.98606329610941,-3.28012237050456,2.79945744685663));
#26588=CARTESIAN_POINT('Ctrl Pts',(4.37472225720076,0.733199667739815,2.9583493823405));
#26589=CARTESIAN_POINT('Ctrl Pts',(1.75344183272134,4.07445924226969,3.11724131782437));
#26590=CARTESIAN_POINT('Ctrl Pts',(-2.47507100164175,3.68100530868232,3.27613325330824));
#26591=CARTESIAN_POINT('Ctrl Pts',(-4.43489475243097,-0.0865161304718975,
3.43502518879211));
#26592=CARTESIAN_POINT('Ctrl Pts',(-2.32962407485832,-3.77473550759247,
3.59391712427598));
#26593=CARTESIAN_POINT('Ctrl Pts',(1.91101674430454,-4.00297283399139,3.75280905975985));
#26594=CARTESIAN_POINT('Ctrl Pts',(4.39998949787803,-0.562022168553895,
3.91170099524372));
#26595=CARTESIAN_POINT('Ctrl Pts',(2.85586253164215,3.39408687237674,4.07059293072759));
#26596=CARTESIAN_POINT('Ctrl Pts',(-1.30599304051693,4.23912239483862,4.22948486621146));
#26597=CARTESIAN_POINT('Ctrl Pts',(-4.27075480883071,1.19851151930018,4.38837680169534));
#26598=CARTESIAN_POINT('Ctrl Pts',(-3.32087541041203,-2.94067390360441,
4.5472687371792));
#26599=CARTESIAN_POINT('Ctrl Pts',(0.672970727569009,-4.38439128034066,
4.70616067266308));
#26600=CARTESIAN_POINT('Ctrl Pts',(4.04996129037005,-1.8093065095749,4.86505260814695));
#26601=CARTESIAN_POINT('Ctrl Pts',(3.7146935053026,2.42421712326595,5.02394454363082));
#26602=CARTESIAN_POINT('Ctrl Pts',(-0.0255208918668632,4.43566513425159,
5.18283647911469));
#26603=CARTESIAN_POINT('Ctrl Pts',(-3.7423424373331,2.38131257520723,5.34172841459856));
#26604=CARTESIAN_POINT('Ctrl Pts',(-4.02887392383437,-1.85578862076283,
5.50062035008243));
#26605=CARTESIAN_POINT('Ctrl Pts',(-0.622476074987428,-4.39184471892869,
5.6595122855663));
#26606=CARTESIAN_POINT('Ctrl Pts',(3.35449315468027,-2.90226673038711,5.81840422105018));
#26607=CARTESIAN_POINT('Ctrl Pts',(4.25668109053274,1.24757468418137,5.97729615653404));
#26608=CARTESIAN_POINT('Ctrl Pts',(1.25712805170321,4.25386948092336,6.13618809201792));
#26609=CARTESIAN_POINT('Ctrl Pts',(-2.89472837218891,3.36100046866316,6.29508002750178));
#26610=CARTESIAN_POINT('Ctrl Pts',(-4.3932311479855,-0.61261454396674,6.45397196298565));
#26611=CARTESIAN_POINT('Ctrl Pts',(-1.86482901435204,-4.0246974105317,6.61286389846953));
#26612=CARTESIAN_POINT('Ctrl Pts',(2.37290478433289,-3.74767919966474,6.77175583395341));
#26613=CARTESIAN_POINT('Ctrl Pts',(4.43559665971225,-0.0354791693710577,
6.93064776943726));
#26614=CARTESIAN_POINT('Ctrl Pts',(2.43255072991432,3.7092416267349,7.08953970492115));
#26615=CARTESIAN_POINT('Ctrl Pts',(-1.80020953695449,4.05401308855407,7.248431640405));
#26616=CARTESIAN_POINT('Ctrl Pts',(-4.38286937018484,0.682812260438543,
7.40732357588889));
#26617=CARTESIAN_POINT('Ctrl Pts',(-2.94812206282321,-3.31426504700587,
7.56621551137276));
#26618=CARTESIAN_POINT('Ctrl Pts',(1.18892039097656,-4.27343477814157,7.72510744685661));
#26619=CARTESIAN_POINT('Ctrl Pts',(4.23617967651747,-1.31550684048772,7.88399938234051));
#26620=CARTESIAN_POINT('Ctrl Pts',(3.40048990657371,2.84823540010302,8.04289131782437));
#26621=CARTESIAN_POINT('Ctrl Pts',(-0.552142504899003,4.40124018356118,
8.20178325330824));
#26622=CARTESIAN_POINT('Ctrl Pts',(-3.99867239438119,1.91999884935475,8.36067518879212));
#26623=CARTESIAN_POINT('Ctrl Pts',(-3.7799561464003,-2.3211436901666,8.51956712427598));
#26624=CARTESIAN_POINT('Ctrl Pts',(-0.0964725209165242,-4.43468934107201,
8.67845905975986));
#26625=CARTESIAN_POINT('Ctrl Pts',(3.67543933768719,-2.48332884936554,8.83735099524372));
#26626=CARTESIAN_POINT('Ctrl Pts',(4.0783855728837,1.74429000398553,8.9962429307276));
#26627=CARTESIAN_POINT('Ctrl Pts',(0.743019314888223,4.37306514893305,9.15513486621146));
#26628=CARTESIAN_POINT('Ctrl Pts',(-3.2734101574334,2.99341985700662,9.31402680169534));
#26629=CARTESIAN_POINT('Ctrl Pts',(-4.28938028911884,-1.13004125341886,
9.4729187371792));
#26630=CARTESIAN_POINT('Ctrl Pts',(-1.37363684534497,-4.2176887410311,9.63181067266308));
#26631=CARTESIAN_POINT('Ctrl Pts',(2.80120377997153,-3.43933625605043,9.79070260814695));
#26632=CARTESIAN_POINT('Ctrl Pts',(4.40841687240619,0.491566046624494,9.94959454363082));
#26633=CARTESIAN_POINT('Ctrl Pts',(1.97480558107332,3.97189116367397,10.1084864791147));
#26634=CARTESIAN_POINT('Ctrl Pts',(-2.26894362964508,3.81151824141021,10.2673784145986));
#26635=CARTESIAN_POINT('Ctrl Pts',(-4.43294334991667,0.157447627925427,
10.4262703500824));
#26636=CARTESIAN_POINT('Ctrl Pts',(-2.53363733058688,-3.6409419627572,10.5851622855663));
#26637=CARTESIAN_POINT('Ctrl Pts',(1.68804059715796,-4.10198676758668,10.7440542210502));
#26638=CARTESIAN_POINT('Ctrl Pts',(4.36243390931193,-0.803085852194621,
10.902946156534));
#26639=CARTESIAN_POINT('Ctrl Pts',(3.03815154638153,3.23193621229276,11.0618380920179));
#26640=CARTESIAN_POINT('Ctrl Pts',(-1.07094840651941,4.30451460790682,11.2207300275018));
#26641=CARTESIAN_POINT('Ctrl Pts',(-4.19840017140343,1.43150707293723,11.3796219629857));
#26642=CARTESIAN_POINT('Ctrl Pts',(-3.47753217061135,-2.75364240624537,
11.5385138984695));
#26643=CARTESIAN_POINT('Ctrl Pts',(0.430896625145342,-4.41475985729101,
11.6974058339534));
#26644=CARTESIAN_POINT('Ctrl Pts',(3.94435878318021,-2.02923884465551,11.8562977694373));
#26645=CARTESIAN_POINT('Ctrl Pts',(3.84235951578439,2.21631447465625,12.0151897049212));
#26646=CARTESIAN_POINT('Ctrl Pts',(0.218392959004639,4.43035901644177,12.174081640405));
#26647=CARTESIAN_POINT('Ctrl Pts',(-3.60575602596446,2.58346665941922,12.3329735758889));
#26648=CARTESIAN_POINT('Ctrl Pts',(-4.12481220928992,-1.63147195415751,
12.4918655113728));
#26649=CARTESIAN_POINT('Ctrl Pts',(-0.86300051278999,-4.35097766186335,
12.6507574468566));
#26650=CARTESIAN_POINT('Ctrl Pts',(3.18985105498742,-3.08230867145154,12.8096493823405));
#26651=CARTESIAN_POINT('Ctrl Pts',(4.31883487235755,1.01165302570498,12.9685413178244));
#26652=CARTESIAN_POINT('Ctrl Pts',(1.48910657905504,4.17831761541948,13.1274332533082));
#26653=CARTESIAN_POINT('Ctrl Pts',(-2.70556027356073,3.51507042678234,13.2863251887921));
#26654=CARTESIAN_POINT('Ctrl Pts',(-4.42026793865305,-0.3701457140446,13.445217124276));
#26655=CARTESIAN_POINT('Ctrl Pts',(-2.08328834587812,-3.91608045972475,
13.6041090597598));
#26656=CARTESIAN_POINT('Ctrl Pts',(2.16326617823678,-3.87247413693191,13.7630009952437));
#26657=CARTESIAN_POINT('Ctrl Pts',(4.4269368293872,-0.279296988392094,13.9218929307276));
#26658=CARTESIAN_POINT('Ctrl Pts',(2.63280741231888,3.56988818154694,14.0807848662115));
#26659=CARTESIAN_POINT('Ctrl Pts',(-1.57459477304264,4.14685758132787,14.2396768016953));
#26660=CARTESIAN_POINT('Ctrl Pts',(-4.33869857315167,0.922751965829036,
14.3985687371792));
#26661=CARTESIAN_POINT('Ctrl Pts',(-3.12588288137982,-3.14716264451114,
14.5574606726631));
#26662=CARTESIAN_POINT('Ctrl Pts',(0.952166324705068,-4.33233837427404,
14.716352608147));
#26663=CARTESIAN_POINT('Ctrl Pts',(4.15744487102007,-1.54642447068669,14.8752445436308));
#26664=CARTESIAN_POINT('Ctrl Pts',(3.55194392546324,2.65696647503773,15.0341364791147));
#26665=CARTESIAN_POINT('Ctrl Pts',(-0.309324802316237,4.4249400748238,15.1930284145986));
#26666=CARTESIAN_POINT('Ctrl Pts',(-3.88706154120257,2.13694386309366,15.3519203500824));
#26667=CARTESIAN_POINT('Ctrl Pts',(-3.90185640968376,-2.10980877268997,
15.5108122855663));
#26668=CARTESIAN_POINT('Ctrl Pts',(-0.340148198136544,-4.42267743594467,
15.6697042210502));
#26669=CARTESIAN_POINT('Ctrl Pts',(3.53334521270251,-2.68165025813993,15.8285961565341));
#26670=CARTESIAN_POINT('Ctrl Pts',(4.168118714559,1.51741981022156,15.9874880920179));
#26671=CARTESIAN_POINT('Ctrl Pts',(0.982328911331549,4.32559896535404,16.1463800275018));
#26672=CARTESIAN_POINT('Ctrl Pts',(-3.10387905394275,3.16886593556829,16.3052719629857));
#26673=CARTESIAN_POINT('Ctrl Pts',(-4.3450225599225,-0.892499553430768,
16.4641638984695));
#26674=CARTESIAN_POINT('Ctrl Pts',(-1.60344990807853,-4.13578588558361,
16.6230558339534));
#26675=CARTESIAN_POINT('Ctrl Pts',(2.60787020056101,-3.5881456932705,16.7819477694373));
#26676=CARTESIAN_POINT('Ctrl Pts',(4.42877538222566,0.248445392192659,16.9408397049211));
#26677=CARTESIAN_POINT('Ctrl Pts',(2.19019524916345,3.85730751556724,17.099731640405));
#26678=CARTESIAN_POINT('Ctrl Pts',(-2.0559523676882,3.9305007773701,17.2586235758889));
#26679=CARTESIAN_POINT('Ctrl Pts',(-4.41758164163537,0.400935080275903,
17.4175155113728));
#26680=CARTESIAN_POINT('Ctrl Pts',(-2.72998595989888,-3.49613403030616,
17.5764074468566));
#26681=CARTESIAN_POINT('Ctrl Pts',(1.4599578784178,-4.18859158815413,17.7352993823405));
#26682=CARTESIAN_POINT('Ctrl Pts',(4.31168131582116,-1.04172008231973,17.8941913178244));
#26683=CARTESIAN_POINT('Ctrl Pts',(3.2112497052163,3.06000846891939,18.0530832533082));
#26684=CARTESIAN_POINT('Ctrl Pts',(-0.832663995847618,4.35688503051531,
18.2119751887921));
#26685=CARTESIAN_POINT('Ctrl Pts',(-4.11334475517948,1.66017210678477,18.370867124276));
#26686=CARTESIAN_POINT('Ctrl Pts',(-3.62366888385615,-2.55828073504186,
18.5297590597599));
#26687=CARTESIAN_POINT('Ctrl Pts',(0.187518996969786,-4.4317731355385,18.6886509952437));
#26688=CARTESIAN_POINT('Ctrl Pts',(3.82682400979189,-2.24303243337775,18.8475429307276));
#26689=CARTESIAN_POINT('Ctrl Pts',(3.95840182287352,2.00170714836323,19.0064348662115));
#26690=CARTESIAN_POINT('Ctrl Pts',(0.461646139008639,4.41165041015396,19.1653268016953));
#26691=CARTESIAN_POINT('Ctrl Pts',(-3.45826167159393,2.77780537652842,19.3242187371792));
#26692=CARTESIAN_POINT('Ctrl Pts',(-4.20827233037425,-1.40221984463863,
19.4831106726631));
#26693=CARTESIAN_POINT('Ctrl Pts',(-1.10091424691577,-4.29694825658366,
19.6420026081469));
#26694=CARTESIAN_POINT('Ctrl Pts',(3.01555918602559,-3.25302617490586,19.8008945436308));
#26695=CARTESIAN_POINT('Ctrl Pts',(4.36792354278479,0.772670967933531,19.9597864791147));
#26696=CARTESIAN_POINT('Ctrl Pts',(1.71658033947744,4.09012572361745,20.1186784145985));
#26697=CARTESIAN_POINT('Ctrl Pts',(-2.5082074562233,3.65850677953844,20.2775703500824));
#26698=CARTESIAN_POINT('Ctrl Pts',(-4.43393276867548,-0.126557139470934,
20.4364622855663));
#26699=CARTESIAN_POINT('Ctrl Pts',(-2.29544542175872,-3.79561678758089,
20.5953542210502));
#26700=CARTESIAN_POINT('Ctrl Pts',(1.94708337032167,-3.98555427199136,20.7542461565341));
#26701=CARTESIAN_POINT('Ctrl Pts',(4.40488486902698,-0.52226988840308,20.9131380920179));
#26702=CARTESIAN_POINT('Ctrl Pts',(2.82509945345179,3.41973529030544,21.0720300275018));
#26703=CARTESIAN_POINT('Ctrl Pts',(-1.34421660681807,4.22715723558706,21.2309219629857));
#26704=CARTESIAN_POINT('Ctrl Pts',(-4.28140261453686,1.15990017936594,21.3898138984695));
#26705=CARTESIAN_POINT('Ctrl Pts',(-3.29418736642239,-2.97053955182989,
21.5487058339534));
#26706=CARTESIAN_POINT('Ctrl Pts',(0.712531667157375,-4.37813612283788,
21.7075977694373));
#26707=CARTESIAN_POINT('Ctrl Pts',(4.06613346502197,-1.7726637213475,21.8664897049211));
#26708=CARTESIAN_POINT('Ctrl Pts',(3.69265225138302,2.45765941919457,22.025381640405));
#26709=CARTESIAN_POINT('Ctrl Pts',(-0.0655703163120924,4.43525466499184,
22.1842735758889));
#26710=CARTESIAN_POINT('Ctrl Pts',(-3.76369372215058,2.34742279002442,22.3431655113728));
#26711=CARTESIAN_POINT('Ctrl Pts',(-4.0119492247608,-1.89208847597824,22.5020574468566));
#26712=CARTESIAN_POINT('Ctrl Pts',(-0.582802053840284,-4.39729181288394,
22.6609493823405));
#26713=CARTESIAN_POINT('Ctrl Pts',(3.38057590440328,-2.87184871381299,22.8198413178244));
#26714=CARTESIAN_POINT('Ctrl Pts',(4.24521650715976,1.285939018969,22.9787332533082));
#26715=CARTESIAN_POINT('Ctrl Pts',(1.21871680907285,4.26508574569377,23.1376251887921));
#26716=CARTESIAN_POINT('Ctrl Pts',(-2.92505373203667,3.33465212858728,23.296517124276));
#26717=CARTESIAN_POINT('Ctrl Pts',(-4.38733815754819,-0.652117348083053,
23.4554090597599));
#26718=CARTESIAN_POINT('Ctrl Pts',(-1.82876059391868,-4.04164014539733,
23.6143009952437));
#26719=CARTESIAN_POINT('Ctrl Pts',(2.40731317054649,-3.72558744783597,23.7731929307276));
#26720=CARTESIAN_POINT('Ctrl Pts',(4.43445972060527,0.00359092823684341,
23.9320848662115));
#26721=CARTESIAN_POINT('Ctrl Pts',(2.4014416917595,3.73295270922791,24.0909768016953));
#26722=CARTESIAN_POINT('Ctrl Pts',(-1.84187514744654,4.03377454464145,24.2498687371792));
#26723=CARTESIAN_POINT('Ctrl Pts',(-3.53121097966664,1.77942692174697,24.3557966941685));
#26724=CARTESIAN_POINT('Ctrl Pts',(-3.71226170138833,0.544051223706471,
24.4087606726631));
#26725=CARTESIAN_POINT('Ctrl Pts',(2.06798052000209,-2.90001952809568,-0.109744663668461));
#26726=CARTESIAN_POINT('Ctrl Pts',(3.0330562439233,-2.2118318183024,-0.0567806851738377));
#26727=CARTESIAN_POINT('Ctrl Pts',(4.20535745823963,0.191894718237391,0.0491472718154096));
#26728=CARTESIAN_POINT('Ctrl Pts',(2.1127408095543,3.64588036952885,0.20803920729928));
#26729=CARTESIAN_POINT('Ctrl Pts',(-1.91829660558064,3.74733746988985,0.366931142783152));
#26730=CARTESIAN_POINT('Ctrl Pts',(-4.19002106768543,0.419258972444119,
0.525823078267022));
#26731=CARTESIAN_POINT('Ctrl Pts',(-2.62161565760238,-3.29588329210025,
0.684715013750895));
#26732=CARTESIAN_POINT('Ctrl Pts',(1.35007080858346,-3.98852267764505,0.843606949234764));
#26733=CARTESIAN_POINT('Ctrl Pts',(4.08412137222898,-1.02597522411638,1.00249888471864));
#26734=CARTESIAN_POINT('Ctrl Pts',(3.07467508021171,2.87739305660463,1.16139082020251));
#26735=CARTESIAN_POINT('Ctrl Pts',(-0.753105157375175,4.14309028633234,
1.32028275568638));
#26736=CARTESIAN_POINT('Ctrl Pts',(-3.89055727921005,1.61127416982435,1.47917469117025));
#26737=CARTESIAN_POINT('Ctrl Pts',(-3.46187378548392,-2.39751806138059,
1.63806662665412));
#26738=CARTESIAN_POINT('Ctrl Pts',(0.14002328039052,-4.20867770156907,1.79695856213799));
#26739=CARTESIAN_POINT('Ctrl Pts',(3.61356992084825,-2.16211260763564,1.95585049762186));
#26740=CARTESIAN_POINT('Ctrl Pts',(3.77486292837046,1.86628713503355,2.11474243310573));
#26741=CARTESIAN_POINT('Ctrl Pts',(0.476056292737952,4.18401440521967,2.27363436858961));
#26742=CARTESIAN_POINT('Ctrl Pts',(-3.2591106302341,2.66661036613276,2.43252630407347));
#26743=CARTESIAN_POINT('Ctrl Pts',(-4.0069256010488,-1.2950519324793,2.59141823955734));
#26744=CARTESIAN_POINT('Ctrl Pts',(-1.08192930174121,-4.0696486060465,2.75031017504122));
#26745=CARTESIAN_POINT('Ctrl Pts',(2.83478038785305,-3.11394154898843,2.90920211052509));
#26746=CARTESIAN_POINT('Ctrl Pts',(4.15308572767863,0.696053577028067,3.06809404600896));
#26747=CARTESIAN_POINT('Ctrl Pts',(1.66460721884761,3.8680349362124,3.22698598149283));
#26748=CARTESIAN_POINT('Ctrl Pts',(-2.34967649317396,3.49451455708637,3.3858779169767));
#26749=CARTESIAN_POINT('Ctrl Pts',(-4.21020970411577,-0.0821329642322605,
3.54476985246057));
#26750=CARTESIAN_POINT('Ctrl Pts',(-2.21159834323779,-3.58349610344751,
3.70366178794445));
#26751=CARTESIAN_POINT('Ctrl Pts',(1.81419891355671,-3.80017024344135,3.86255372342831));
#26752=CARTESIAN_POINT('Ctrl Pts',(4.1770728542812,-0.53354844253673,4.02144565891219));
#26753=CARTESIAN_POINT('Ctrl Pts',(2.71117598399594,3.22213226793253,4.18033759439605));
#26754=CARTESIAN_POINT('Ctrl Pts',(-1.23982752232801,4.02435576039341,4.33922952987993));
#26755=CARTESIAN_POINT('Ctrl Pts',(-4.05438558157035,1.13779133682627,4.4981214653638));
#26756=CARTESIAN_POINT('Ctrl Pts',(-3.15262991786046,-2.79169055788951,
4.65701340084767));
#26757=CARTESIAN_POINT('Ctrl Pts',(0.638876015320037,-4.16226488915267,
4.81590533633154));
#26758=CARTESIAN_POINT('Ctrl Pts',(3.84477812391437,-1.7176416238867,4.97479727181542));
#26759=CARTESIAN_POINT('Ctrl Pts',(3.5264960087876,2.30139902455706,5.13368920729927));
#26760=CARTESIAN_POINT('Ctrl Pts',(-0.0242279270633424,4.21094105608648,
5.29258114278316));
#26761=CARTESIAN_POINT('Ctrl Pts',(-3.55274416312754,2.26066814937938,5.45147307826701));
#26762=CARTESIAN_POINT('Ctrl Pts',(-3.82475910651287,-1.76176881213256,
5.61036501375091));
#26763=CARTESIAN_POINT('Ctrl Pts',(-0.590939573042961,-4.16934071422273,
5.76925694923476));
#26764=CARTESIAN_POINT('Ctrl Pts',(3.18454448653674,-2.75522920707652,5.92814888471864));
#26765=CARTESIAN_POINT('Ctrl Pts',(4.04102487998468,1.1843688148564,6.0870408202025));
#26766=CARTESIAN_POINT('Ctrl Pts',(1.19343818017234,4.03835571493739,6.24593275568638));
#26767=CARTESIAN_POINT('Ctrl Pts',(-2.74807276467801,3.19072212050733,6.40482469117025));
#26768=CARTESIAN_POINT('Ctrl Pts',(-4.17065690263191,-0.581577656713809,
6.56371662665412));
#26769=CARTESIAN_POINT('Ctrl Pts',(-1.77035119231138,-3.82079418788054,
6.72260856213799));
#26770=CARTESIAN_POINT('Ctrl Pts',(2.25268632236759,-3.5578105490987,6.88150049762186));
#26771=CARTESIAN_POINT('Ctrl Pts',(4.21087605067235,-0.033681688409442,
7.04039243310573));
#26772=CARTESIAN_POINT('Ctrl Pts',(2.30931042573792,3.52132033871361,7.19928436858961));
#26773=CARTESIAN_POINT('Ctrl Pts',(-1.70900553113983,3.84862464586941,7.35817630407347));
#26774=CARTESIAN_POINT('Ctrl Pts',(-4.16082008352265,0.648218946664257,
7.51706823955734));
#26775=CARTESIAN_POINT('Ctrl Pts',(-2.79876137105901,-3.14635445525897,
7.67596017504123));
#26776=CARTESIAN_POINT('Ctrl Pts',(1.12868612378383,-4.05692977561084,7.83485211052507));
#26777=CARTESIAN_POINT('Ctrl Pts',(4.02156212899428,-1.24885932470353,7.99374404600897));
#26778=CARTESIAN_POINT('Ctrl Pts',(3.2282109052434,2.70393526577978,8.15263598149282));
#26779=CARTESIAN_POINT('Ctrl Pts',(-0.524169312226923,4.1782601764825,8.3115279169767));
#26780=CARTESIAN_POINT('Ctrl Pts',(-3.79608767697933,1.82272595826847,8.47041985246058));
#26781=CARTESIAN_POINT('Ctrl Pts',(-3.5884522490603,-2.20354760022878,8.62931178794444));
#26782=CARTESIAN_POINT('Ctrl Pts',(-0.0915849341228856,-4.21001469951135,
8.78820372342831));
#26783=CARTESIAN_POINT('Ctrl Pts',(3.48923057484898,-2.35751597360421,8.94709565891219));
#26784=CARTESIAN_POINT('Ctrl Pts',(3.87176234716024,1.65591904916041,9.10598759439605));
#26785=CARTESIAN_POINT('Ctrl Pts',(0.705375731447328,4.15151257347791,9.26487952987993));
#26786=CARTESIAN_POINT('Ctrl Pts',(-3.10756939673095,2.84176424334623,9.42377146536379));
#26787=CARTESIAN_POINT('Ctrl Pts',(-4.07206743925366,-1.07278997964659,
9.58266340084768));
#26788=CARTESIAN_POINT('Ctrl Pts',(-1.30404428944617,-4.00400799967019,
9.74155533633153));
#26789=CARTESIAN_POINT('Ctrl Pts',(2.65928640835889,-3.26508918233143,9.90044727181542));
#26790=CARTESIAN_POINT('Ctrl Pts',(4.18507327278026,0.466661838722957,10.0593392072993));
#26791=CARTESIAN_POINT('Ctrl Pts',(1.87475601684109,3.77066326361532,10.2182311427832));
#26792=CARTESIAN_POINT('Ctrl Pts',(-2.15399215108477,3.61841531382528,10.377123078267));
#26793=CARTESIAN_POINT('Ctrl Pts',(-4.20835716549627,0.149470859622617,
10.5360150137509));
#26794=CARTESIAN_POINT('Ctrl Pts',(-2.40527567651967,-3.45648094023428,
10.6949069492348));
#26795=CARTESIAN_POINT('Ctrl Pts',(1.60251940571986,-3.89416783466651,10.8537988847186));
#26796=CARTESIAN_POINT('Ctrl Pts',(4.14141994429093,-0.762399118106369,
11.0126908202025));
#26797=CARTESIAN_POINT('Ctrl Pts',(2.88422969138973,3.06819664584361,11.1715827556864));
#26798=CARTESIAN_POINT('Ctrl Pts',(-1.01669095332279,4.08643500813259,11.3304746911703));
#26799=CARTESIAN_POINT('Ctrl Pts',(-3.98569664673889,1.35898263801798,11.4893666266541));
#26800=CARTESIAN_POINT('Ctrl Pts',(-3.30134997748419,-2.61413463624678,
11.648258562138));
#26801=CARTESIAN_POINT('Ctrl Pts',(0.409066111808665,-4.19109490305693,
11.8071504976218));
#26802=CARTESIAN_POINT('Ctrl Pts',(3.74452575596225,-1.92643152829146,11.9660424331058));
#26803=CARTESIAN_POINT('Ctrl Pts',(3.6476940768864,2.10402934668408,12.1249343685896));
#26804=CARTESIAN_POINT('Ctrl Pts',(0.207328517730425,4.20590376209391,12.2838263040735));
#26805=CARTESIAN_POINT('Ctrl Pts',(-3.42307762836267,2.45258050234096,12.4427182395573));
#26806=CARTESIAN_POINT('Ctrl Pts',(-3.91583687114297,-1.54881669956688,
12.6016101750412));
#26807=CARTESIAN_POINT('Ctrl Pts',(-0.819278322583353,-4.13054410464348,
12.7605021105251));
#26808=CARTESIAN_POINT('Ctrl Pts',(3.02824364863007,-2.92614968427652,12.919394046009));
#26809=CARTESIAN_POINT('Ctrl Pts',(4.10002976510464,0.960399654058624,13.0782859814928));
#26810=CARTESIAN_POINT('Ctrl Pts',(1.4136639806759,3.9666315331777,13.2371779169767));
#26811=CARTESIAN_POINT('Ctrl Pts',(-2.56848848838443,3.33698643319039,13.3960698524606));
#26812=CARTESIAN_POINT('Ctrl Pts',(-4.19632392852339,-0.351393023781037,
13.5549617879445));
#26813=CARTESIAN_POINT('Ctrl Pts',(-1.97774271993255,-3.71768009705162,
13.7138537234283));
#26814=CARTESIAN_POINT('Ctrl Pts',(2.05366863581272,-3.67628300114927,13.8727456589122));
#26815=CARTESIAN_POINT('Ctrl Pts',(4.20265495328316,-0.265146966613851,
14.0316375943961));
#26816=CARTESIAN_POINT('Ctrl Pts',(2.49942150494934,3.38902695634851,14.1905295298799));
#26817=CARTESIAN_POINT('Ctrl Pts',(-1.49482108676428,3.93676535861929,14.3494214653638));
#26818=CARTESIAN_POINT('Ctrl Pts',(-4.11888711133529,0.876002588087538,
14.5083134008477));
#26819=CARTESIAN_POINT('Ctrl Pts',(-2.96751629424819,-2.98771796085767,
14.6672053363315));
#26820=CARTESIAN_POINT('Ctrl Pts',(0.903926727462482,-4.11284913917822,
14.8260972718154));
#26821=CARTESIAN_POINT('Ctrl Pts',(3.94681626451235,-1.46807797628081,14.9849892072993));
#26822=CARTESIAN_POINT('Ctrl Pts',(3.37199181001155,2.52235659720725,15.1438811427832));
#26823=CARTESIAN_POINT('Ctrl Pts',(-0.293653481567197,4.20075936028517,
15.302773078267));
#26824=CARTESIAN_POINT('Ctrl Pts',(-3.69013136383804,2.02867988797614,15.4616650137509));
#26825=CARTESIAN_POINT('Ctrl Pts',(-3.7041766799792,-2.00291954250747,15.6205569492348));
#26826=CARTESIAN_POINT('Ctrl Pts',(-0.322915271855557,-4.19861135346705,
15.7794488847186));
#26827=CARTESIAN_POINT('Ctrl Pts',(3.35433536373254,-2.54578982594268,15.9383408202025));
#26828=CARTESIAN_POINT('Ctrl Pts',(3.95694933917511,1.44054277876839,16.0972327556863));
#26829=CARTESIAN_POINT('Ctrl Pts',(0.932561187129547,4.10645116889506,16.2561246911703));
#26830=CARTESIAN_POINT('Ctrl Pts',(-2.94662724659887,3.00832169820004,16.4150166266541));
#26831=CARTESIAN_POINT('Ctrl Pts',(-4.12489070599933,-0.847282853491266,
16.573908562138));
#26832=CARTESIAN_POINT('Ctrl Pts',(-1.52221433425345,-3.92625458813528,
16.7328004976219));
#26833=CARTESIAN_POINT('Ctrl Pts',(2.47574768701282,-3.40635948785661,16.8916924331057));
#26834=CARTESIAN_POINT('Ctrl Pts',(4.20440035952933,0.235858404662022,17.0505843685896));
#26835=CARTESIAN_POINT('Ctrl Pts',(2.07923339936798,3.66188476623891,17.2094763040735));
#26836=CARTESIAN_POINT('Ctrl Pts',(-1.95179166425446,3.73136983822386,17.3683682395573));
#26837=CARTESIAN_POINT('Ctrl Pts',(-4.19377372735666,0.380622508521273,
17.5272601750413));
#26838=CARTESIAN_POINT('Ctrl Pts',(-2.59167669631074,-3.31900941126415,
17.6861521105251));
#26839=CARTESIAN_POINT('Ctrl Pts',(1.38599204049781,-3.97638499568851,17.845044046009));
#26840=CARTESIAN_POINT('Ctrl Pts',(4.09323862916349,-0.988943423550422,
18.0039359814928));
#26841=CARTESIAN_POINT('Ctrl Pts',(3.04855817916078,2.90497927678192,18.1628279169767));
#26842=CARTESIAN_POINT('Ctrl Pts',(-0.79047874443103,4.13615218831009,18.3217198524606));
#26843=CARTESIAN_POINT('Ctrl Pts',(-3.9049503925967,1.57606281652034,18.4806117879444));
#26844=CARTESIAN_POINT('Ctrl Pts',(-3.44008296723408,-2.42867057231101,
18.6395037234283));
#26845=CARTESIAN_POINT('Ctrl Pts',(0.178018723063364,-4.20724623768266,
18.7983956589122));
#26846=CARTESIAN_POINT('Ctrl Pts',(3.63294564614808,-2.12939369361065,18.9572875943961));
#26847=CARTESIAN_POINT('Ctrl Pts',(3.75785733321325,1.90029467017615,19.1161795298799));
#26848=CARTESIAN_POINT('Ctrl Pts',(0.438257763221198,4.18814298982299,19.2750714653638));
#26849=CARTESIAN_POINT('Ctrl Pts',(-3.2830557796519,2.63707343810004,19.4339634008477));
#26850=CARTESIAN_POINT('Ctrl Pts',(-3.99506865257438,-1.33117918840468,
19.5928553363316));
#26851=CARTESIAN_POINT('Ctrl Pts',(-1.04513863451291,-4.07925199082465,
19.7517472718154));
#26852=CARTESIAN_POINT('Ctrl Pts',(2.86278192766154,-3.08821812779751,19.9106392072993));
#26853=CARTESIAN_POINT('Ctrl Pts',(4.14663145649351,0.733525142958367,20.0695311427831));
#26854=CARTESIAN_POINT('Ctrl Pts',(1.62961323923206,3.88290770670228,20.228423078267));
#26855=CARTESIAN_POINT('Ctrl Pts',(-2.3811341557403,3.47315587080009,20.3873150137509));
#26856=CARTESIAN_POINT('Ctrl Pts',(-4.20929645733797,-0.120145375813829,
20.5462069492348));
#26857=CARTESIAN_POINT('Ctrl Pts',(-2.17915128305114,-3.60331947526336,
20.7050988847187));
#26858=CARTESIAN_POINT('Ctrl Pts',(1.8484382962994,-3.78363415795159,20.8639908202025));
#26859=CARTESIAN_POINT('Ctrl Pts',(4.18172021126871,-0.495810131935346,
21.0228827556864));
#26860=CARTESIAN_POINT('Ctrl Pts',(2.6819714554658,3.24648126020556,21.1817746911702));
#26861=CARTESIAN_POINT('Ctrl Pts',(-1.27611456830103,4.01299679193883,21.3406666266541));
#26862=CARTESIAN_POINT('Ctrl Pts',(-4.0644939375549,1.10113616299357,21.499558562138));
#26863=CARTESIAN_POINT('Ctrl Pts',(-3.12729397009587,-2.82004312294412,
21.6584504976218));
#26864=CARTESIAN_POINT('Ctrl Pts',(0.676432679244829,-4.15632663665986,
21.8173424331058));
#26865=CARTESIAN_POINT('Ctrl Pts',(3.86013096777133,-1.68285526903662,21.9762343685896));
#26866=CARTESIAN_POINT('Ctrl Pts',(3.50557143079345,2.33314703363201,22.1351263040735));
#26867=CARTESIAN_POINT('Ctrl Pts',(-0.062248327739398,4.21055138242857,
22.2940182395573));
#26868=CARTESIAN_POINT('Ctrl Pts',(-3.57301372792039,2.22849532219585,22.4529101750413));
#26869=CARTESIAN_POINT('Ctrl Pts',(-3.80869186337486,-1.79622960798394,
22.6118021105251));
#26870=CARTESIAN_POINT('Ctrl Pts',(-0.553275556609776,-4.17451184208706,
22.770694046009));
#26871=CARTESIAN_POINT('Ctrl Pts',(3.20930580605478,-2.72635225830787,22.9295859814928));
#26872=CARTESIAN_POINT('Ctrl Pts',(4.03014112673573,1.22078949756286,23.0884779169767));
#26873=CARTESIAN_POINT('Ctrl Pts',(1.15697296611493,4.04900373014777,23.2473698524606));
#26874=CARTESIAN_POINT('Ctrl Pts',(-2.77686175098751,3.16570866623898,23.4062617879444));
#26875=CARTESIAN_POINT('Ctrl Pts',(-4.16506246873653,-0.619079130483647,
23.5651537234284));
#26876=CARTESIAN_POINT('Ctrl Pts',(-1.73611010606296,-3.83687855306338,
23.7240456589121));
#26877=CARTESIAN_POINT('Ctrl Pts',(2.28535147670074,-3.53683803157065,23.8829375943961));
#26878=CARTESIAN_POINT('Ctrl Pts',(4.20979671230505,0.00340900105942339,
24.0418295298799));
#26879=CARTESIAN_POINT('Ctrl Pts',(2.27977746461109,3.54383014676541,24.2007214653638));
#26880=CARTESIAN_POINT('Ctrl Pts',(-1.74856023703795,3.82941144719509,24.3596134008477));
#26881=CARTESIAN_POINT('Ctrl Pts',(-3.35230925733317,1.68927582545165,24.4655413578369));
#26882=CARTESIAN_POINT('Ctrl Pts',(-3.52418740734158,0.51648795956872,24.5185053363315));
#26883=CARTESIAN_POINT('Ctrl Pts',(1.95761919937776,-2.74525502143746,0.));
#26884=CARTESIAN_POINT('Ctrl Pts',(2.87119200517945,-2.09379362688536,0.0529639784946237));
#26885=CARTESIAN_POINT('Ctrl Pts',(3.98093135833217,0.181653928094203,0.158891935483871));
#26886=CARTESIAN_POINT('Ctrl Pts',(1.99999077945293,3.45131172222888,0.317783870967742));
#26887=CARTESIAN_POINT('Ctrl Pts',(-1.81592342329319,3.54735439074478,0.476675806451613));
#26888=CARTESIAN_POINT('Ctrl Pts',(-3.96641342051426,0.396884499650513,
0.635567741935484));
#26889=CARTESIAN_POINT('Ctrl Pts',(-2.48170865009243,-3.119992837997,0.794459677419355));
#26890=CARTESIAN_POINT('Ctrl Pts',(1.27802196869812,-3.77566833700333,0.953351612903227));
#26891=CARTESIAN_POINT('Ctrl Pts',(3.86616524359544,-0.97122229991515,1.1122435483871));
#26892=CARTESIAN_POINT('Ctrl Pts',(2.91058978102209,2.72383605033175,1.27113548387097));
#26893=CARTESIAN_POINT('Ctrl Pts',(-0.71291441141164,3.92198718064885,1.43002741935484));
#26894=CARTESIAN_POINT('Ctrl Pts',(-3.6829310297627,1.52528576541256,1.58891935483871));
#26895=CARTESIAN_POINT('Ctrl Pts',(-3.27712496454226,-2.26957040572551,
1.74781129032258));
#26896=CARTESIAN_POINT('Ctrl Pts',(0.13255069832671,-3.98407441119242,1.90670322580645));
#26897=CARTESIAN_POINT('Ctrl Pts',(3.42072557595435,-2.04672776701011,2.06559516129032));
#26898=CARTESIAN_POINT('Ctrl Pts',(3.57341090601276,1.76668952717683,2.2244870967742));
#26899=CARTESIAN_POINT('Ctrl Pts',(0.45065073371557,3.96072731387378,2.38337903225806));
#26900=CARTESIAN_POINT('Ctrl Pts',(-3.08518261218244,2.52430213897566,2.54227096774194));
#26901=CARTESIAN_POINT('Ctrl Pts',(-3.79308915689569,-1.22593926910403,
2.70116290322581));
#26902=CARTESIAN_POINT('Ctrl Pts',(-1.02419029239979,-3.85246484135621,
2.86005483870968));
#26903=CARTESIAN_POINT('Ctrl Pts',(2.68349747959669,-2.94776072747231,3.01894677419354));
#26904=CARTESIAN_POINT('Ctrl Pts',(3.9314491981565,0.658907486316316,3.17783870967743));
#26905=CARTESIAN_POINT('Ctrl Pts',(1.57577260497388,3.66161063015511,3.33673064516129));
#26906=CARTESIAN_POINT('Ctrl Pts',(-2.22428198470617,3.30802380549044,3.49562258064516));
#26907=CARTESIAN_POINT('Ctrl Pts',(-3.98552465580058,-0.07774979799263,
3.65451451612903));
#26908=CARTESIAN_POINT('Ctrl Pts',(-2.09357261161725,-3.39225669930255,
3.8134064516129));
#26909=CARTESIAN_POINT('Ctrl Pts',(1.71738108280889,-3.59736765289132,3.97229838709678));
#26910=CARTESIAN_POINT('Ctrl Pts',(3.95415621068438,-0.505074716519562,
4.13119032258065));
#26911=CARTESIAN_POINT('Ctrl Pts',(2.56648943634972,3.05017766348832,4.29008225806451));
#26912=CARTESIAN_POINT('Ctrl Pts',(-1.17366200413909,3.8095891259482,4.44897419354839));
#26913=CARTESIAN_POINT('Ctrl Pts',(-3.83801635431,1.07707115435234,4.60786612903225));
#26914=CARTESIAN_POINT('Ctrl Pts',(-2.98438442530889,-2.6427072121746,4.76675806451613));
#26915=CARTESIAN_POINT('Ctrl Pts',(0.604781303071069,-3.94013849796468,
4.92565));
#26916=CARTESIAN_POINT('Ctrl Pts',(3.63959495745868,-1.6259767381985,5.08454193548388));
#26917=CARTESIAN_POINT('Ctrl Pts',(3.3382985122726,2.17858092584818,5.24343387096774));
#26918=CARTESIAN_POINT('Ctrl Pts',(-0.0229349622598251,3.98621697792136,
5.40232580645161));
#26919=CARTESIAN_POINT('Ctrl Pts',(-3.36314588892197,2.14002372355154,5.56121774193549));
#26920=CARTESIAN_POINT('Ctrl Pts',(-3.62064428919136,-1.6677490035023,5.72010967741935));
#26921=CARTESIAN_POINT('Ctrl Pts',(-0.559403071098495,-3.94683670951677,
5.87900161290323));
#26922=CARTESIAN_POINT('Ctrl Pts',(3.01459581839321,-2.60819168376593,6.03789354838709));
#26923=CARTESIAN_POINT('Ctrl Pts',(3.82536866943663,1.12116294553142,6.19678548387097));
#26924=CARTESIAN_POINT('Ctrl Pts',(1.12974830864147,3.82284194895142,6.35567741935484));
#26925=CARTESIAN_POINT('Ctrl Pts',(-2.60141715716711,3.02044377235149,6.51456935483871));
#26926=CARTESIAN_POINT('Ctrl Pts',(-3.94808265727831,-0.550540769460877,
6.67346129032257));
#26927=CARTESIAN_POINT('Ctrl Pts',(-1.67587337027072,-3.61689096522939,
6.83235322580646));
#26928=CARTESIAN_POINT('Ctrl Pts',(2.13246786040229,-3.36794189853266,6.99124516129032));
#26929=CARTESIAN_POINT('Ctrl Pts',(3.98615544163244,-0.0318842074478251,
7.15013709677419));
#26930=CARTESIAN_POINT('Ctrl Pts',(2.18607012156152,3.33339905069232,7.30902903225807));
#26931=CARTESIAN_POINT('Ctrl Pts',(-1.61780152532516,3.64323620318475,7.46792096774193));
#26932=CARTESIAN_POINT('Ctrl Pts',(-3.93877079686046,0.613625632889965,
7.62681290322582));
#26933=CARTESIAN_POINT('Ctrl Pts',(-2.64940067929482,-2.97844386351206,
7.78570483870967));
#26934=CARTESIAN_POINT('Ctrl Pts',(1.06845185659111,-3.84042477308012,7.94459677419355));
#26935=CARTESIAN_POINT('Ctrl Pts',(3.80694458147109,-1.18221180891932,8.10348870967742));
#26936=CARTESIAN_POINT('Ctrl Pts',(3.0559319039131,2.55963513145653,8.2623806451613));
#26937=CARTESIAN_POINT('Ctrl Pts',(-0.49619611955484,3.95528016940384,8.42127258064515));
#26938=CARTESIAN_POINT('Ctrl Pts',(-3.59350295957747,1.72545306718219,8.58016451612905));
#26939=CARTESIAN_POINT('Ctrl Pts',(-3.39694835172031,-2.08595151029096,
8.7390564516129));
#26940=CARTESIAN_POINT('Ctrl Pts',(-0.086697347329244,-3.9853400579507,
8.89794838709678));
#26941=CARTESIAN_POINT('Ctrl Pts',(3.30302181201077,-2.23170309784288,9.05684032258065));
#26942=CARTESIAN_POINT('Ctrl Pts',(3.66513912143678,1.56754809433529,9.21573225806451));
#26943=CARTESIAN_POINT('Ctrl Pts',(0.667732148006428,3.92995999802278,9.3746241935484));
#26944=CARTESIAN_POINT('Ctrl Pts',(-2.94172863602851,2.69010862968584,9.53351612903225));
#26945=CARTESIAN_POINT('Ctrl Pts',(-3.85475458938848,-1.01553870587432,
9.69240806451614));
#26946=CARTESIAN_POINT('Ctrl Pts',(-1.23445173354738,-3.79032725830928,
9.85129999999999));
#26947=CARTESIAN_POINT('Ctrl Pts',(2.51736903674626,-3.09084210861242,10.0101919354839));
#26948=CARTESIAN_POINT('Ctrl Pts',(3.96172967315432,0.441757630821415,10.1690838709677));
#26949=CARTESIAN_POINT('Ctrl Pts',(1.77470645260886,3.56943536355667,10.3279758064516));
#26950=CARTESIAN_POINT('Ctrl Pts',(-2.03904067252446,3.42531238624034,10.4868677419355));
#26951=CARTESIAN_POINT('Ctrl Pts',(-3.98377098107586,0.14149409131981,10.6457596774194));
#26952=CARTESIAN_POINT('Ctrl Pts',(-2.27691402245245,-3.27201991771136,
10.8046516129032));
#26953=CARTESIAN_POINT('Ctrl Pts',(1.51699821428175,-3.68634890174633,10.9635435483871));
#26954=CARTESIAN_POINT('Ctrl Pts',(3.92040597926993,-0.721712384018116,
11.122435483871));
#26955=CARTESIAN_POINT('Ctrl Pts',(2.73030783639792,2.90445707939446,11.2813274193548));
#26956=CARTESIAN_POINT('Ctrl Pts',(-0.962433500126168,3.86835540835836,
11.4402193548387));
#26957=CARTESIAN_POINT('Ctrl Pts',(-3.77299312207436,1.28645820309873,11.5991112903226));
#26958=CARTESIAN_POINT('Ctrl Pts',(-3.12516778435703,-2.4746268662482,11.7580032258064));
#26959=CARTESIAN_POINT('Ctrl Pts',(0.38723559847199,-3.96742994882286,11.9168951612903));
#26960=CARTESIAN_POINT('Ctrl Pts',(3.54469272874429,-1.82362421192741,12.0757870967742));
#26961=CARTESIAN_POINT('Ctrl Pts',(3.45302863798842,1.9917442187119,12.2346790322581));
#26962=CARTESIAN_POINT('Ctrl Pts',(0.196264076456207,3.98144850774605,12.3935709677419));
#26963=CARTESIAN_POINT('Ctrl Pts',(-3.24039923076088,2.32169434526269,12.5524629032258));
#26964=CARTESIAN_POINT('Ctrl Pts',(-3.70686153299603,-1.46616144497625,
12.7113548387097));
#26965=CARTESIAN_POINT('Ctrl Pts',(-0.775556132376715,-3.9101105474236,
12.8702467741936));
#26966=CARTESIAN_POINT('Ctrl Pts',(2.86663624227273,-2.76999069710151,13.0291387096774));
#26967=CARTESIAN_POINT('Ctrl Pts',(3.88122465785174,0.909146282412278,13.1880306451613));
#26968=CARTESIAN_POINT('Ctrl Pts',(1.33822138229676,3.75494545093591,13.3469225806451));
#26969=CARTESIAN_POINT('Ctrl Pts',(-2.43141670320813,3.15890243959844,13.5058145161291));
#26970=CARTESIAN_POINT('Ctrl Pts',(-3.97237991839373,-0.332640333517474,
13.6647064516129));
#26971=CARTESIAN_POINT('Ctrl Pts',(-1.87219709398698,-3.51927973437849,
13.8235983870968));
#26972=CARTESIAN_POINT('Ctrl Pts',(1.94407109338865,-3.48009186536664,13.9824903225806));
#26973=CARTESIAN_POINT('Ctrl Pts',(3.97837307717912,-0.25099694483561,14.1413822580645));
#26974=CARTESIAN_POINT('Ctrl Pts',(2.36603559757979,3.20816573115008,14.3002741935484));
#26975=CARTESIAN_POINT('Ctrl Pts',(-1.41504740048591,3.7266731359107,14.4591661290323));
#26976=CARTESIAN_POINT('Ctrl Pts',(-3.8990756495189,0.82925321034604,14.6180580645161));
#26977=CARTESIAN_POINT('Ctrl Pts',(-2.80914970711657,-2.8282732772042,14.77695));
#26978=CARTESIAN_POINT('Ctrl Pts',(0.8556871302199,-3.8933599040824,14.9358419354839));
#26979=CARTESIAN_POINT('Ctrl Pts',(3.73618765800463,-1.38973148187494,15.0947338709677));
#26980=CARTESIAN_POINT('Ctrl Pts',(3.19203969455987,2.38774671937678,15.2536258064516));
#26981=CARTESIAN_POINT('Ctrl Pts',(-0.277982160818163,3.97657864574653,
15.4125177419355));
#26982=CARTESIAN_POINT('Ctrl Pts',(-3.4932011864735,1.92041591285862,15.5714096774194));
#26983=CARTESIAN_POINT('Ctrl Pts',(-3.50649695027464,-1.89603031232498,
15.7303016129032));
#26984=CARTESIAN_POINT('Ctrl Pts',(-0.30568234557457,-3.97454527098943,
15.8891935483871));
#26985=CARTESIAN_POINT('Ctrl Pts',(3.17532551476257,-2.40992939374543,16.048085483871));
#26986=CARTESIAN_POINT('Ctrl Pts',(3.74577996379122,1.36366574731522,16.2069774193548));
#26987=CARTESIAN_POINT('Ctrl Pts',(0.882793462927545,3.88730337243608,16.3658693548387));
#26988=CARTESIAN_POINT('Ctrl Pts',(-2.78937543925498,2.84777746083178,16.5247612903226));
#26989=CARTESIAN_POINT('Ctrl Pts',(-3.90475885207616,-0.802066153551767,
16.6836532258065));
#26990=CARTESIAN_POINT('Ctrl Pts',(-1.44097876042837,-3.71672329068694,
16.8425451612903));
#26991=CARTESIAN_POINT('Ctrl Pts',(2.34362517346463,-3.22457328244272,17.0014370967742));
#26992=CARTESIAN_POINT('Ctrl Pts',(3.980025336833,0.223271417131382,17.1603290322581));
#26993=CARTESIAN_POINT('Ctrl Pts',(1.96827154957251,3.46646201691059,17.3192209677419));
#26994=CARTESIAN_POINT('Ctrl Pts',(-1.84763096082072,3.53223889907763,17.4781129032258));
#26995=CARTESIAN_POINT('Ctrl Pts',(-3.96996581307795,0.360309936766638,
17.6370048387097));
#26996=CARTESIAN_POINT('Ctrl Pts',(-2.4533674327226,-3.14188479222213,17.7958967741935));
#26997=CARTESIAN_POINT('Ctrl Pts',(1.31202620257783,-3.7641784032229,17.9547887096774));
#26998=CARTESIAN_POINT('Ctrl Pts',(3.87479594250582,-0.936166764781103,
18.1136806451613));
#26999=CARTESIAN_POINT('Ctrl Pts',(2.88586665310525,2.74995008464444,18.2725725806452));
#27000=CARTESIAN_POINT('Ctrl Pts',(-0.748293493014444,3.91541934610488,
18.431464516129));
#27001=CARTESIAN_POINT('Ctrl Pts',(-3.69655603001392,1.49195352625591,18.5903564516129));
#27002=CARTESIAN_POINT('Ctrl Pts',(-3.25649705061201,-2.29906040958017,
18.7492483870968));
#27003=CARTESIAN_POINT('Ctrl Pts',(0.168518449156949,-3.98271933982683,
18.9081403225806));
#27004=CARTESIAN_POINT('Ctrl Pts',(3.43906728250426,-2.01575495384355,19.0670322580645));
#27005=CARTESIAN_POINT('Ctrl Pts',(3.55731284355299,1.79888219198906,19.2259241935484));
#27006=CARTESIAN_POINT('Ctrl Pts',(0.41486938743375,3.96463556949202,19.3848161290323));
#27007=CARTESIAN_POINT('Ctrl Pts',(-3.10784988770987,2.49634149967166,19.5437080645161));
#27008=CARTESIAN_POINT('Ctrl Pts',(-3.78186497477451,-1.26013853217073,
19.7026));
#27009=CARTESIAN_POINT('Ctrl Pts',(-0.989363022110038,-3.86155572506565,
19.8614919354839));
#27010=CARTESIAN_POINT('Ctrl Pts',(2.71000466929749,-2.92341008068914,20.0203838709678));
#27011=CARTESIAN_POINT('Ctrl Pts',(3.92533937020224,0.694379317983201,20.1792758064516));
#27012=CARTESIAN_POINT('Ctrl Pts',(1.54264613898669,3.6756896897871,20.3381677419355));
#27013=CARTESIAN_POINT('Ctrl Pts',(-2.25406085525731,3.28780496206174,20.4970596774194));
#27014=CARTESIAN_POINT('Ctrl Pts',(-3.98466014600046,-0.113733612156729,
20.6559516129032));
#27015=CARTESIAN_POINT('Ctrl Pts',(-2.06285714434356,-3.41102216294582,
20.8148435483871));
#27016=CARTESIAN_POINT('Ctrl Pts',(1.74979322227715,-3.58171404391184,20.9737354838709));
#27017=CARTESIAN_POINT('Ctrl Pts',(3.95855555351044,-0.46935037546761,21.1326274193549));
#27018=CARTESIAN_POINT('Ctrl Pts',(2.53884345747981,3.07322723010567,21.2915193548387));
#27019=CARTESIAN_POINT('Ctrl Pts',(-1.20801252978399,3.79883634829061,21.4504112903226));
#27020=CARTESIAN_POINT('Ctrl Pts',(-3.84758526057294,1.0423721466212,21.6093032258064));
#27021=CARTESIAN_POINT('Ctrl Pts',(-2.96040057376934,-2.66954669405833,
21.7681951612904));
#27022=CARTESIAN_POINT('Ctrl Pts',(0.640333691332285,-3.93451715048184,
21.9270870967742));
#27023=CARTESIAN_POINT('Ctrl Pts',(3.6541284705207,-1.59304681672573,22.0859790322581));
#27024=CARTESIAN_POINT('Ctrl Pts',(3.31849061020388,2.20863464806944,22.2448709677419));
#27025=CARTESIAN_POINT('Ctrl Pts',(-0.058926339166703,3.98584809986529,
22.4037629032258));
#27026=CARTESIAN_POINT('Ctrl Pts',(-3.3823337336902,2.1095678543673,22.5626548387097));
#27027=CARTESIAN_POINT('Ctrl Pts',(-3.60543450198892,-1.70037073998966,
22.7215467741936));
#27028=CARTESIAN_POINT('Ctrl Pts',(-0.52374905937927,-3.95173187129016,
22.8804387096774));
#27029=CARTESIAN_POINT('Ctrl Pts',(3.03803570770629,-2.58085580280275,23.0393306451613));
#27030=CARTESIAN_POINT('Ctrl Pts',(3.81506574631169,1.15563997615671,23.1982225806452));
#27031=CARTESIAN_POINT('Ctrl Pts',(1.095229123157,3.83292171460177,23.357114516129));
#27032=CARTESIAN_POINT('Ctrl Pts',(-2.62866976993836,2.99676520389069,23.5160064516129));
#27033=CARTESIAN_POINT('Ctrl Pts',(-3.94278677992486,-0.586040912884242,
23.6748983870968));
#27034=CARTESIAN_POINT('Ctrl Pts',(-1.64345961820725,-3.63211696072943,
23.8337903225806));
#27035=CARTESIAN_POINT('Ctrl Pts',(2.163389782855,-3.34808861530533,23.9926822580645));
#27036=CARTESIAN_POINT('Ctrl Pts',(3.98513370400483,0.0032270738820094,
24.1515741935484));
#27037=CARTESIAN_POINT('Ctrl Pts',(2.15811323746268,3.35470758430291,24.3104661290323));
#27038=CARTESIAN_POINT('Ctrl Pts',(-1.65524532662936,3.62504834974875,24.4693580645161));
#27039=CARTESIAN_POINT('Ctrl Pts',(-3.1734075349997,1.59912472915632,24.5752860215054));
#27040=CARTESIAN_POINT('Ctrl Pts',(-3.33611311329483,0.488924695430968,
24.62825));
#27041=CARTESIAN_POINT('',(1.95761919937778,-2.74525502143744,0.));
#27042=CARTESIAN_POINT('Ctrl Pts',(1.95761919937776,-2.74525502143746,0.));
#27043=CARTESIAN_POINT('Ctrl Pts',(2.87119200517945,-2.09379362688536,0.0529639784946237));
#27044=CARTESIAN_POINT('Ctrl Pts',(3.98093135833217,0.181653928094203,0.158891935483871));
#27045=CARTESIAN_POINT('Ctrl Pts',(1.99999077945293,3.45131172222888,0.317783870967742));
#27046=CARTESIAN_POINT('Ctrl Pts',(-1.81592342329319,3.54735439074478,0.476675806451613));
#27047=CARTESIAN_POINT('Ctrl Pts',(-3.32105516281529,1.34233496093003,0.58788455216069));
#27048=CARTESIAN_POINT('Ctrl Pts',(-3.3766520624322,0.1136195821916,0.646129319375144));
#27049=CARTESIAN_POINT('Ctrl Pts',(-3.37589447807987,0.0021436428109594,
0.651410108094974));
#27050=CARTESIAN_POINT('Ctrl Pts',(1.73118107496478,3.54876586530513,2.39391839684799E-16));
#27051=CARTESIAN_POINT('Ctrl Pts',(1.81301063452785,3.50205269354806,2.06920727311338E-16));
#27052=CARTESIAN_POINT('Ctrl Pts',(1.89292240658196,3.4522795469799,5.6760153975772E-16));
#27053=CARTESIAN_POINT('Ctrl Pts',(1.97072352421092,3.39943606703627,2.9316826744008E-16));
#27054=CARTESIAN_POINT('Ctrl Pts',(2.07158749034463,3.33092801556019,-4.87384004076243E-17));
#27055=CARTESIAN_POINT('Ctrl Pts',(2.16890551010069,3.25726040082769,-6.1331688516479E-17));
#27056=CARTESIAN_POINT('Ctrl Pts',(2.26249391432527,3.17884397520376,-1.04083408558608E-17));
#27057=CARTESIAN_POINT('Ctrl Pts',(2.31703211703773,3.13314717171513,1.92670006623856E-17));
#27058=CARTESIAN_POINT('Ctrl Pts',(2.37030307443948,3.08583698417059,-9.57318163015451E-16));
#27059=CARTESIAN_POINT('Ctrl Pts',(2.42226407127706,3.03698980450436,-1.02695629777827E-15));
#27060=CARTESIAN_POINT('Ctrl Pts',(2.45441149625484,3.00676884764696,-1.07004028094122E-15));
#27061=CARTESIAN_POINT('Ctrl Pts',(2.48605741280453,2.97595951290433,-8.19532942944583E-16));
#27062=CARTESIAN_POINT('Ctrl Pts',(2.51719072732778,2.9445793777147,-8.39606162372775E-16));
#27063=CARTESIAN_POINT('Ctrl Pts',(2.53181221876951,2.92984196908534,-8.49033375972473E-16));
#27064=CARTESIAN_POINT('Ctrl Pts',(2.54632072268487,2.91497845934833,-6.96615474306211E-16));
#27065=CARTESIAN_POINT('Ctrl Pts',(2.56070494112922,2.90000148244637,-7.07767178198537E-16));
#27066=CARTESIAN_POINT('Ctrl Pts',(2.64790074151672,2.80921243517189,-7.75367774667319E-16));
#27067=CARTESIAN_POINT('Ctrl Pts',(2.73062866917384,2.71416182380689,-8.593918943852E-16));
#27068=CARTESIAN_POINT('Ctrl Pts',(2.80868748257388,2.61529981528879,-7.7715611723761E-16));
#27069=CARTESIAN_POINT('Ctrl Pts',(2.87698894429891,2.52879555783546,-7.05199812233468E-16));
#27070=CARTESIAN_POINT('Ctrl Pts',(2.94171511816388,2.43937213712426,-7.20848724153807E-16));
#27071=CARTESIAN_POINT('Ctrl Pts',(3.00269897791456,2.3473133317077,-6.24500451351651E-16));
#27072=CARTESIAN_POINT('Ctrl Pts',(3.02937941655548,2.30703760433796,-5.82348082000707E-16));
#27073=CARTESIAN_POINT('Ctrl Pts',(3.05534314365639,2.26625728440317,-1.08606649764317E-16));
#27074=CARTESIAN_POINT('Ctrl Pts',(3.08057418911428,2.22499554197223,-6.93889390390723E-17));
#27075=CARTESIAN_POINT('Ctrl Pts',(3.09523937783659,2.20101273710704,-4.6594198725879E-17));
#27076=CARTESIAN_POINT('Ctrl Pts',(3.10965701779078,2.17686728558595,-1.5350788780052E-16));
#27077=CARTESIAN_POINT('Ctrl Pts',(3.12382377516257,2.1525637049523,-1.66533453693773E-16));
#27078=CARTESIAN_POINT('Ctrl Pts',(3.1333468514065,2.13622652592816,-1.75289406369904E-16));
#27079=CARTESIAN_POINT('Ctrl Pts',(3.14275743380374,2.11981622896702,-6.17919290773945E-16));
#27080=CARTESIAN_POINT('Ctrl Pts',(3.15204614385832,2.10334928089744,-6.10622663543836E-16));
#27081=CARTESIAN_POINT('Ctrl Pts',(3.21133027918083,1.99825085797653,-5.64052770246931E-16));
#27082=CARTESIAN_POINT('Ctrl Pts',(3.26572921710173,1.89071971149897,-2.93721959998899E-16));
#27083=CARTESIAN_POINT('Ctrl Pts',(3.3150665440347,1.78114320161924,-3.46944695195361E-16));
#27084=CARTESIAN_POINT('Ctrl Pts',(3.36416434269629,1.67209867580975,-3.99909038813826E-16));
#27085=CARTESIAN_POINT('Ctrl Pts',(3.40824985101865,1.5610277430108,-6.74639111044964E-16));
#27086=CARTESIAN_POINT('Ctrl Pts',(3.44710068203266,1.44829560050515,-7.21644966006352E-16));
#27087=CARTESIAN_POINT('Ctrl Pts',(3.48485757303191,1.33873770674576,-7.67327256340457E-16));
#27088=CARTESIAN_POINT('Ctrl Pts',(3.51767049623361,1.22761008128266,-7.45739296926402E-16));
#27089=CARTESIAN_POINT('Ctrl Pts',(3.54528704260767,1.11524410687019,-6.10622663543836E-16));
#27090=CARTESIAN_POINT('Ctrl Pts',(3.56429882714017,1.03788911593903,-5.17605662582399E-16));
#27091=CARTESIAN_POINT('Ctrl Pts',(3.58084694549942,0.959947166702576,1.01128139593754E-16));
#27092=CARTESIAN_POINT('Ctrl Pts',(3.59483483174014,0.881527990398642,1.38777878078145E-16));
#27093=CARTESIAN_POINT('Ctrl Pts',(3.60174616248926,0.842781545425996,1.5738038819335E-16));
#27094=CARTESIAN_POINT('Ctrl Pts',(3.60803228263339,0.803918629301433,-8.2431208915498E-16));
#27095=CARTESIAN_POINT('Ctrl Pts',(3.6136804381616,0.764952740225288,-8.60422844084496E-16));
#27096=CARTESIAN_POINT('Ctrl Pts',(3.61598402562173,0.749060590478247,-8.75150533826084E-16));
#27097=CARTESIAN_POINT('Ctrl Pts',(3.6181800809526,0.733160977259198,-9.56453568707426E-16));
#27098=CARTESIAN_POINT('Ctrl Pts',(3.62026800126996,0.71725566677106,-9.43689570931383E-16));
#27099=CARTESIAN_POINT('Ctrl Pts',(3.63517124652415,0.603726074153541,-8.52582172005361E-16));
#27100=CARTESIAN_POINT('Ctrl Pts',(3.64457137343043,0.489891978911761,1.54068630345449E-16));
#27101=CARTESIAN_POINT('Ctrl Pts',(3.64826597516095,0.3760806489335,1.38777878078145E-16));
#27102=CARTESIAN_POINT('Ctrl Pts',(3.65049038519446,0.307558225463841,1.29571770019922E-16));
#27103=CARTESIAN_POINT('Ctrl Pts',(3.65064564728474,0.239043959798587,2.28153843810054E-16));
#27104=CARTESIAN_POINT('Ctrl Pts',(3.64867842117138,0.170609648189261,1.38777878078145E-16));
#27105=CARTESIAN_POINT('Ctrl Pts',(3.64536397368567,0.0553092612588858,
-9.22057312926959E-18));
#27106=CARTESIAN_POINT('Ctrl Pts',(3.63602703897368,-0.0597651999246838,
-3.71059406415836E-16));
#27107=CARTESIAN_POINT('Ctrl Pts',(3.62088618085986,-0.174255990612961,
-4.44089209850063E-16));
#27108=CARTESIAN_POINT('Ctrl Pts',(3.60564019443288,-0.289541731204713,
-5.17626084943432E-16));
#27109=CARTESIAN_POINT('Ctrl Pts',(3.58450894234823,-0.404236478340693,
2.06881119674206E-16));
#27110=CARTESIAN_POINT('Ctrl Pts',(3.55766829556208,-0.517952337059044,
1.66533453693773E-16));
#27111=CARTESIAN_POINT('Ctrl Pts',(3.55209090522836,-0.541582085487224,
1.58149353116006E-16));
#27112=CARTESIAN_POINT('Ctrl Pts',(3.54626683911464,-0.565169464342046,
2.72822796152711E-16));
#27113=CARTESIAN_POINT('Ctrl Pts',(3.54019745029697,-0.588710821151176,
2.77555756156289E-16));
#27114=CARTESIAN_POINT('Ctrl Pts',(3.53607649256559,-0.604694792398417,
2.80769313353732E-16));
#27115=CARTESIAN_POINT('Ctrl Pts',(3.53184170988113,-0.62066020100356,-1.61867697048363E-17));
#27116=CARTESIAN_POINT('Ctrl Pts',(3.52749592285427,-0.636597072708719,
-2.77555756156289E-17));
#27117=CARTESIAN_POINT('Ctrl Pts',(3.49747618222011,-0.7466854760641,-1.07670341512578E-16));
#27118=CARTESIAN_POINT('Ctrl Pts',(3.46222700262188,-0.855189606000695,
-1.99543722780696E-16));
#27119=CARTESIAN_POINT('Ctrl Pts',(3.42199607778626,-0.961778490999782,
-2.77555756156289E-16));
#27120=CARTESIAN_POINT('Ctrl Pts',(3.38156991618782,-1.0688846414842,-3.55946374337476E-16));
#27121=CARTESIAN_POINT('Ctrl Pts',(3.33611303054141,-1.17405769074672,1.35240542225809E-16));
#27122=CARTESIAN_POINT('Ctrl Pts',(3.28582849960376,-1.27693996092432,1.11022302462516E-16));
#27123=CARTESIAN_POINT('Ctrl Pts',(3.23598893769955,-1.3789118233987,8.70183704900679E-17));
#27124=CARTESIAN_POINT('Ctrl Pts',(3.18140622212873,-1.47863395215989,2.26466381867324E-16));
#27125=CARTESIAN_POINT('Ctrl Pts',(3.1222390297712,-1.57572584500942,2.22044604925031E-16));
#27126=CARTESIAN_POINT('Ctrl Pts',(3.08604888850041,-1.6351129678129,2.19339985594059E-16));
#27127=CARTESIAN_POINT('Ctrl Pts',(3.04814284654775,-1.69351537716898,-1.98475779326559E-16));
#27128=CARTESIAN_POINT('Ctrl Pts',(3.00855126708734,-1.75083831899302,-2.22044604925031E-16));
#27129=CARTESIAN_POINT('Ctrl Pts',(2.9875142347103,-1.78129693164588,-2.34567928166019E-16));
#27130=CARTESIAN_POINT('Ctrl Pts',(2.96600124729196,-1.81145066683922,-9.64459754115302E-17));
#27131=CARTESIAN_POINT('Ctrl Pts',(2.94401641708542,-1.8412845286552,-1.11022302462516E-16));
#27132=CARTESIAN_POINT('Ctrl Pts',(2.93430327275808,-1.85446546309672,-1.17462287082754E-16));
#27133=CARTESIAN_POINT('Ctrl Pts',(2.92449763119146,-1.86758436264681,1.18006511135168E-16));
#27134=CARTESIAN_POINT('Ctrl Pts',(2.91460943608169,-1.8806275411502,1.11022302462516E-16));
#27135=CARTESIAN_POINT('Ctrl Pts',(2.8471863415804,-1.96956302907997,6.34001675707856E-17));
#27136=CARTESIAN_POINT('Ctrl Pts',(2.77582498992288,-2.05512251526362,-2.18484873575661E-16));
#27137=CARTESIAN_POINT('Ctrl Pts',(2.70071126790977,-2.13697549169768,-1.66533453693773E-16));
#27138=CARTESIAN_POINT('Ctrl Pts',(2.6265626894838,-2.21777673120304,-1.1524956270538E-16));
#27139=CARTESIAN_POINT('Ctrl Pts',(2.54875698937316,-2.29496666804747,3.16111469076589E-16));
#27140=CARTESIAN_POINT('Ctrl Pts',(2.46744030034225,-2.36818969290806,1.66533453693773E-16));
#27141=CARTESIAN_POINT('Ctrl Pts',(2.38865944095536,-2.43912928592605,2.1619971139621E-17));
#27142=CARTESIAN_POINT('Ctrl Pts',(2.30658261909198,-2.50634586230322,1.27495535944492E-16));
#27143=CARTESIAN_POINT('Ctrl Pts',(2.22131994895062,-2.56947408053004,1.66533453693773E-16));
#27144=CARTESIAN_POINT('Ctrl Pts',(2.13653932671254,-2.63224539197476,2.05350663525179E-16));
#27145=CARTESIAN_POINT('Ctrl Pts',(2.04860838319626,-2.69097492590926,9.78571983200637E-17));
#27146=CARTESIAN_POINT('Ctrl Pts',(1.95761919937776,-2.74525502143746,5.55111512312578E-17));
#27147=CARTESIAN_POINT('Ctrl Pts',(0.349418900843865,3.91916189049794,24.058));
#27148=CARTESIAN_POINT('Ctrl Pts',(0.983708099956935,3.86349481221817,24.0324107126756));
#27149=CARTESIAN_POINT('Ctrl Pts',(1.60505772607221,3.66267070559658,24.0068214253513));
#27150=CARTESIAN_POINT('Ctrl Pts',(2.13605939111367,3.32170193071062,23.9812321380269));
#27151=CARTESIAN_POINT('Ctrl Pts',(3.23511152224044,2.61597446626503,23.9282681595323));
#27152=CARTESIAN_POINT('Ctrl Pts',(3.94711712557296,1.30987366083964,23.8753041810376));
#27153=CARTESIAN_POINT('Ctrl Pts',(3.94814528315368,0.00380497154103099,
23.822340202543));
#27154=CARTESIAN_POINT('Ctrl Pts',(3.94917344073441,-1.30226371775762,23.7693762240484));
#27155=CARTESIAN_POINT('Ctrl Pts',(3.23922415256329,-2.60830029092949,23.7164122455538));
#27156=CARTESIAN_POINT('Ctrl Pts',(2.14246851744994,-3.3166627231204,23.6634482670591));
#27157=CARTESIAN_POINT('Ctrl Pts',(1.04571288233662,-4.0250251553113,23.6104842885645));
#27158=CARTESIAN_POINT('Ctrl Pts',(-0.437849099718904,-4.13571344652128,
23.5575203100699));
#27159=CARTESIAN_POINT('Ctrl Pts',(-1.62766388484424,-3.59751656345146,
23.5045563315753));
#27160=CARTESIAN_POINT('Ctrl Pts',(-2.81747866996957,-3.05931968038165,
23.4515923530806));
#27161=CARTESIAN_POINT('Ctrl Pts',(-3.71354625816471,-1.87223762303205,
23.398628374586));
#27162=CARTESIAN_POINT('Ctrl Pts',(-3.90551869671661,-0.580571401587583,
23.3456643960914));
#27163=CARTESIAN_POINT('Ctrl Pts',(-3.93389711745665,-0.389630203130338,
23.3378349697575));
#27164=CARTESIAN_POINT('Ctrl Pts',(-3.94688938557907,-0.196403592096446,
23.3300055434235));
#27165=CARTESIAN_POINT('Ctrl Pts',(-3.94525314071248,-0.00295827654940184,
23.3221761170896));
#27166=CARTESIAN_POINT('Origin',(0.,0.,-1.84858989190503));
#27167=CARTESIAN_POINT('',(-1.95761919937781,-2.74525502143742,0.));
#27168=CARTESIAN_POINT('Ctrl Pts',(-1.96186193197216,-2.74910310536277,
-1.68972908581866E-15));
#27169=CARTESIAN_POINT('Ctrl Pts',(-1.11318069597017,-3.34796943221813,
0.0492202025162847));
#27170=CARTESIAN_POINT('Ctrl Pts',(1.27289724729396,-3.73216471134832,0.15142869376082));
#27171=CARTESIAN_POINT('Ctrl Pts',(3.84885445708067,-1.03979978230375,0.306625473733605));
#27172=CARTESIAN_POINT('Ctrl Pts',(2.95737874714596,2.67433718082728,0.465590339918353));
#27173=CARTESIAN_POINT('Ctrl Pts',(-0.647631800440264,3.93376542742361,
0.624555206103101));
#27174=CARTESIAN_POINT('Ctrl Pts',(-3.06550566908991,2.04752208664245,0.752221723431987));
#27175=CARTESIAN_POINT('Ctrl Pts',(-3.36890345256199,0.462673372879177,
0.826899952032626));
#27176=CARTESIAN_POINT('Ctrl Pts',(-3.36692593843476,0.00163208592380858,
0.848589891905015));
#27177=CARTESIAN_POINT('Origin',(0.,0.,0.));
#27178=CARTESIAN_POINT('Ctrl Pts',(-1.47719995289048,3.03093687853778,-0.329233991005386));
#27179=CARTESIAN_POINT('Ctrl Pts',(-2.48630564145415,2.53912496184525,-0.276245702277136));
#27180=CARTESIAN_POINT('Ctrl Pts',(-3.95706612649723,0.476768711041013,
-0.170269124820638));
#27181=CARTESIAN_POINT('Ctrl Pts',(-2.54025446427213,-3.07629710463389,
-0.0113042586358904));
#27182=CARTESIAN_POINT('Ctrl Pts',(1.21035452671364,-3.79753374264191,0.147660607548857));
#27183=CARTESIAN_POINT('Ctrl Pts',(3.84885445708067,-1.03979978230375,0.306625473733605));
#27184=CARTESIAN_POINT('Ctrl Pts',(2.95737874714596,2.67433718082728,0.465590339918353));
#27185=CARTESIAN_POINT('Ctrl Pts',(-0.647631800440264,3.93376542742361,
0.624555206103101));
#27186=CARTESIAN_POINT('Ctrl Pts',(-3.65826453346399,1.58509620284767,0.783520072287847));
#27187=CARTESIAN_POINT('Ctrl Pts',(-3.31298624479799,-2.21807698161905,
0.942484938472596));
#27188=CARTESIAN_POINT('Ctrl Pts',(0.0716483833591926,-3.98622915634864,
1.10144980465734));
#27189=CARTESIAN_POINT('Ctrl Pts',(3.39051798866077,-2.09756782602768,1.26041467084209));
#27190=CARTESIAN_POINT('Ctrl Pts',(3.59899177492058,1.71542482386315,1.41937953702684));
#27191=CARTESIAN_POINT('Ctrl Pts',(0.505790215469384,3.95468340129096,1.57834440321159));
#27192=CARTESIAN_POINT('Ctrl Pts',(-3.05141119286119,2.56598394358578,1.73730926939633));
#27193=CARTESIAN_POINT('Ctrl Pts',(-3.80929264538726,-1.17672126473752,
1.89627413558108));
#27194=CARTESIAN_POINT('Ctrl Pts',(-1.07258002819951,-3.83991470812214,
2.05523900176583));
#27195=CARTESIAN_POINT('Ctrl Pts',(2.6481020123777,-2.98042525524821,2.21420386795058));
#27196=CARTESIAN_POINT('Ctrl Pts',(3.9394520872816,0.613266379946328,2.37316873413532));
#27197=CARTESIAN_POINT('Ctrl Pts',(1.61680281711694,3.64435532093595,2.53213360032008));
#27198=CARTESIAN_POINT('Ctrl Pts',(-2.18907900650795,3.33216312280983,2.69109846650482));
#27199=CARTESIAN_POINT('Ctrl Pts',(-3.98672992391563,-0.0369098299799313,
2.85006333268957));
#27200=CARTESIAN_POINT('Ctrl Pts',(-2.12700963248002,-3.37212213291773,
3.00902819887431));
#27201=CARTESIAN_POINT('Ctrl Pts',(1.68400001564517,-3.61379602896036,3.16799306505907));
#27202=CARTESIAN_POINT('Ctrl Pts',(3.95013122707835,-0.540223147458982,
3.32695793124381));
#27203=CARTESIAN_POINT('Ctrl Pts',(2.59246639543577,3.02894300530038,3.48592279742856));
#27204=CARTESIAN_POINT('Ctrl Pts',(-1.14349143614182,3.81939852540782,3.6448876636133));
#27205=CARTESIAN_POINT('Ctrl Pts',(-3.83042595833975,1.10599038526397,3.80385252979806));
#27206=CARTESIAN_POINT('Ctrl Pts',(-3.00338040757504,-2.62203811565132,
3.9628173959828));
#27207=CARTESIAN_POINT('Ctrl Pts',(0.57892500607099,-3.94464492605495,4.12178226216755));
#27208=CARTESIAN_POINT('Ctrl Pts',(3.63013258458704,-1.64848875417016,4.2807471283523));
#27209=CARTESIAN_POINT('Ctrl Pts',(3.35110647594949,2.15996831943484,4.43971199453705));
#27210=CARTESIAN_POINT('Ctrl Pts',(-0.00217860669321579,3.9869001753454,
4.59867686072179));
#27211=CARTESIAN_POINT('Ctrl Pts',(-3.35346506555395,2.15630466503255,4.75764172690654));
#27212=CARTESIAN_POINT('Ctrl Pts',(-3.6283288127004,-1.65245507692285,4.91660659309129));
#27213=CARTESIAN_POINT('Ctrl Pts',(-0.574613628296617,-3.94527526701846,
5.07557145927603));
#27214=CARTESIAN_POINT('Ctrl Pts',(3.0062441927532,-2.61875420913902,5.2345363254608));
#27215=CARTESIAN_POINT('Ctrl Pts',(3.8292149534867,1.11017592945447,5.39350119164552));
#27216=CARTESIAN_POINT('Ctrl Pts',(1.13931660104628,3.82064594498541,5.55246605783029));
#27217=CARTESIAN_POINT('Ctrl Pts',(-2.59577512563926,3.02610793784054,5.71143092401502));
#27218=CARTESIAN_POINT('Ctrl Pts',(-3.94953846664522,-0.544539856061292,
5.87039579019978));
#27219=CARTESIAN_POINT('Ctrl Pts',(-1.68004955900417,-3.61563427819245,
6.02936065638453));
#27220=CARTESIAN_POINT('Ctrl Pts',(2.13069369871068,-3.3697955600636,6.18832552256926));
#27221=CARTESIAN_POINT('Ctrl Pts',(3.98676787287831,-0.032552759256669,
6.34729038875402));
#27222=CARTESIAN_POINT('Ctrl Pts',(2.18543605335013,3.3345534950076,6.50625525493876));
#27223=CARTESIAN_POINT('Ctrl Pts',(-1.62078473268592,3.64258625218979,6.66522012112352));
#27224=CARTESIAN_POINT('Ctrl Pts',(-3.94011990490355,0.608960498992104,
6.82418498730826));
#27225=CARTESIAN_POINT('Ctrl Pts',(-2.64484328742837,-2.98331723745481,
6.98314985349301));
#27226=CARTESIAN_POINT('Ctrl Pts',(1.07677617223565,-3.83874078693202,7.14211471967776));
#27227=CARTESIAN_POINT('Ctrl Pts',(3.81057598656871,-1.17255635469506,7.3010795858625));
#27228=CARTESIAN_POINT('Ctrl Pts',(3.04860581952888,2.56931514444696,7.46004445204726));
#27229=CARTESIAN_POINT('Ctrl Pts',(-0.510113381387115,3.95413228059959,
7.619009318232));
#27230=CARTESIAN_POINT('Ctrl Pts',(-3.60086158473341,1.71148286638841,7.77797418441675));
#27231=CARTESIAN_POINT('Ctrl Pts',(-3.38822891354565,-2.10125738160825,
7.93693905060149));
#27232=CARTESIAN_POINT('Ctrl Pts',(-0.0672816548149041,-3.98633301836102,
8.09590391678625));
#27233=CARTESIAN_POINT('Ctrl Pts',(3.31538886833258,-2.21440159096907,8.25486878297098));
#27234=CARTESIAN_POINT('Ctrl Pts',(3.65656725922866,1.58899138861319,8.41383364915575));
#27235=CARTESIAN_POINT('Ctrl Pts',(0.643261156248369,3.93466553079316,8.57279851534047));
#27236=CARTESIAN_POINT('Ctrl Pts',(-2.96016388101437,2.67073165104392,8.73176338152524));
#27237=CARTESIAN_POINT('Ctrl Pts',(-3.84797530194499,-1.04329469948394,
8.89072824770997));
#27238=CARTESIAN_POINT('Ctrl Pts',(-1.20570712414377,-3.80021684712055,
9.04969311389473));
#27239=CARTESIAN_POINT('Ctrl Pts',(2.54266018034211,-3.07087234538534,9.20865798007948));
#27240=CARTESIAN_POINT('Ctrl Pts',(3.95842601916979,0.47564819468749,9.36762284626423));
#27241=CARTESIAN_POINT('Ctrl Pts',(1.74278629094578,3.58581562527152,9.52658771244896));
#27242=CARTESIAN_POINT('Ctrl Pts',(-2.07166160205713,3.40640513751843,9.68555257863373));
#27243=CARTESIAN_POINT('Ctrl Pts',(-3.98559564477585,0.102005444431573,
9.84451744481845));
#27244=CARTESIAN_POINT('Ctrl Pts',(-2.24319907973156,-3.29597263991092,
10.0034823110032));
#27245=CARTESIAN_POINT('Ctrl Pts',(1.55707745747673,-3.67027077281332,10.1624471771879));
#27246=CARTESIAN_POINT('Ctrl Pts',(3.928912558612,-0.677512997019795,10.3214120433727));
#27247=CARTESIAN_POINT('Ctrl Pts',(2.69641733534343,2.93678588051791,10.4803769095574));
#27248=CARTESIAN_POINT('Ctrl Pts',(-1.00973405207762,3.8569177977272,10.6393417757422));
#27249=CARTESIAN_POINT('Ctrl Pts',(-3.7895693127859,1.2387663936115,10.7983066419269));
#27250=CARTESIAN_POINT('Ctrl Pts',(-3.0929058256244,-2.51581225614482,10.9572715081117));
#27251=CARTESIAN_POINT('Ctrl Pts',(0.441146911493231,-3.96241935650807,
11.1162363742964));
#27252=CARTESIAN_POINT('Ctrl Pts',(3.57049754163045,-1.77395745708877,11.2752012404812));
#27253=CARTESIAN_POINT('Ctrl Pts',(3.42432285260543,2.04190860605321,11.4341661066659));
#27254=CARTESIAN_POINT('Ctrl Pts',(0.136721492950909,3.98455580808139,11.5931309728507));
#27255=CARTESIAN_POINT('Ctrl Pts',(-3.27630628322196,2.27182633422323,11.7520958390354));
#27256=CARTESIAN_POINT('Ctrl Pts',(-3.683695752997,-1.52504536119478,11.9110607052202));
#27257=CARTESIAN_POINT('Ctrl Pts',(-0.711713421966334,-3.92286142494773,
12.0700255714049));
#27258=CARTESIAN_POINT('Ctrl Pts',(2.91318501009988,-2.72189839106446,12.2289904375897));
#27259=CARTESIAN_POINT('Ctrl Pts',(3.86556759564105,0.976096776902648,12.3879553037744));
#27260=CARTESIAN_POINT('Ctrl Pts',(1.27173165426137,3.77863419159615,12.5469201699592));
#27261=CARTESIAN_POINT('Ctrl Pts',(-2.48877340931887,3.11470458814592,12.7058850361439));
#27262=CARTESIAN_POINT('Ctrl Pts',(-3.96611198956382,-0.406612150074322,
12.8648499023287));
#27263=CARTESIAN_POINT('Ctrl Pts',(-1.80499399926681,-3.5549084962852,13.0238147685134));
#27264=CARTESIAN_POINT('Ctrl Pts',(2.01200065152342,-3.44198069904803,13.1827796346982));
#27265=CARTESIAN_POINT('Ctrl Pts',(3.98321358718988,-0.171427165804589,
13.3417445008829));
#27266=CARTESIAN_POINT('Ctrl Pts',(2.30028118194861,3.25639129072706,13.5007093670677));
#27267=CARTESIAN_POINT('Ctrl Pts',(-1.49289753065309,3.69684118097057,13.6596742332524));
#27268=CARTESIAN_POINT('Ctrl Pts',(-3.91651258901516,0.74585983564986,13.8186390994372));
#27269=CARTESIAN_POINT('Ctrl Pts',(-2.74717288447362,-2.88936306080816,
13.9776039656219));
#27270=CARTESIAN_POINT('Ctrl Pts',(0.942385426660244,-3.87392403926152,
14.1365688318067));
#27271=CARTESIAN_POINT('Ctrl Pts',(3.76741231340739,-1.30460040439068,14.2955336979914));
#27272=CARTESIAN_POINT('Ctrl Pts',(3.1362669786623,2.46154569181692,14.4544985641762));
#27273=CARTESIAN_POINT('Ctrl Pts',(-0.372046531241306,3.96950363810656,
14.6134634303609));
#27274=CARTESIAN_POINT('Ctrl Pts',(-3.53904967227374,1.83589356214594,14.7724282965457));
#27275=CARTESIAN_POINT('Ctrl Pts',(-3.45937733680892,-1.98194000815431,
14.9313931627304));
#27276=CARTESIAN_POINT('Ctrl Pts',(-0.206119829211681,-3.98156908396121,
15.0903580289152));
#27277=CARTESIAN_POINT('Ctrl Pts',(3.23622917375625,-2.32856146349605,15.2493228950999));
#27278=CARTESIAN_POINT('Ctrl Pts',(3.70970605913983,1.46063640552025,15.4082877612846));
#27279=CARTESIAN_POINT('Ctrl Pts',(0.779949646731194,3.90986653262151,15.5672526274694));
#27280=CARTESIAN_POINT('Ctrl Pts',(-2.86532184046814,2.77223889751338,15.7262174936541));
#27281=CARTESIAN_POINT('Ctrl Pts',(-3.88198649442593,-0.908602559673156,
15.8851823598389));
#27282=CARTESIAN_POINT('Ctrl Pts',(-1.33737014962086,-3.75590452983738,
16.0441472260236));
#27283=CARTESIAN_POINT('Ctrl Pts',(2.43413116992486,-3.15759136082396,16.2031120922084));
#27284=CARTESIAN_POINT('Ctrl Pts',(3.97259404474729,0.337452678146523,16.3620769583931));
#27285=CARTESIAN_POINT('Ctrl Pts',(1.86665380078734,3.52292227310739,16.5210418245779));
#27286=CARTESIAN_POINT('Ctrl Pts',(-1.95172895721992,3.47651144567355,16.6800066907626));
#27287=CARTESIAN_POINT('Ctrl Pts',(-3.97962242319515,0.240796850378547,
16.8389715569474));
#27288=CARTESIAN_POINT('Ctrl Pts',(-2.35666503270154,-3.21582146239366,
16.9979364231321));
#27289=CARTESIAN_POINT('Ctrl Pts',(1.42826443406275,-3.7222894112013,17.1569012893169));
#27290=CARTESIAN_POINT('Ctrl Pts',(3.90292376012977,-0.813980268166524,
17.3158661555016));
#27291=CARTESIAN_POINT('Ctrl Pts',(2.79709452794753,2.84106317354542,17.4748310216864));
#27292=CARTESIAN_POINT('Ctrl Pts',(-0.87475073969136,3.88975434928213,17.6337958878711));
#27293=CARTESIAN_POINT('Ctrl Pts',(-3.74411171420101,1.37003840308681,17.7927607540559));
#27294=CARTESIAN_POINT('Ctrl Pts',(-3.1786761163436,-2.40653192410502,17.9517256202406));
#27295=CARTESIAN_POINT('Ctrl Pts',(0.302833216085013,-3.97538297495793,
18.1106904864254));
#27296=CARTESIAN_POINT('Ctrl Pts',(3.5065275226793,-1.89727238082542,18.2696553526101));
#27297=CARTESIAN_POINT('Ctrl Pts',(3.49338172535042,1.92136979140851,18.4286202187948));
#27298=CARTESIAN_POINT('Ctrl Pts',(0.275455597698851,3.97737375262188,18.5875850849796));
#27299=CARTESIAN_POINT('Ctrl Pts',(-3.19516970536172,2.38458975681184,18.7465499511644));
#27300=CARTESIAN_POINT('Ctrl Pts',(-3.73459028221552,-1.3957840729596,18.9055148173491));
#27301=CARTESIAN_POINT('Ctrl Pts',(-0.847949117405149,-3.89568479841959,
19.0644796835338));
#27302=CARTESIAN_POINT('Ctrl Pts',(2.81658890100978,-2.82173788950715,19.2234445497186));
#27303=CARTESIAN_POINT('Ctrl Pts',(3.89722701433046,0.840832535700663,19.3824094159033));
#27304=CARTESIAN_POINT('Ctrl Pts',(1.40260268563389,3.73203476143841,19.5413742820881));
#27305=CARTESIAN_POINT('Ctrl Pts',(-2.3787500488546,3.19951964512964,19.7003391482728));
#27306=CARTESIAN_POINT('Ctrl Pts',(-3.97787021705804,-0.268190772315832,
19.8593040144576));
#27307=CARTESIAN_POINT('Ctrl Pts',(-1.92774697870435,-3.4898666651324,20.0182688806423));
#27308=CARTESIAN_POINT('Ctrl Pts',(1.89086481476229,-3.50998689564495,20.1772337468271));
#27309=CARTESIAN_POINT('Ctrl Pts',(3.97482324267393,-0.310093440809367,
20.3361986130118));
#27310=CARTESIAN_POINT('Ctrl Pts',(2.41233351706024,3.17427546962878,20.4951634791965));
#27311=CARTESIAN_POINT('Ctrl Pts',(-1.36319778790607,3.74660773920425,20.6541283453813));
#27312=CARTESIAN_POINT('Ctrl Pts',(-3.88815019533756,0.881853615583829,
20.813093211566));
#27313=CARTESIAN_POINT('Ctrl Pts',(-2.84616711491744,-2.79190087828212,
20.9720580777508));
#27314=CARTESIAN_POINT('Ctrl Pts',(0.806850527235046,-3.9044039261228,21.1310229439355));
#27315=CARTESIAN_POINT('Ctrl Pts',(3.71967457752779,-1.43506051902692,21.2899878101203));
#27316=CARTESIAN_POINT('Ctrl Pts',(3.22012038549849,2.35078763921597,21.448952676305));
#27317=CARTESIAN_POINT('Ctrl Pts',(-0.233528014234224,3.98005560769136,
21.6079175424898));
#27318=CARTESIAN_POINT('Ctrl Pts',(-3.47294089147738,1.95807523322667,21.7668824086745));
#27319=CARTESIAN_POINT('Ctrl Pts',(-3.52632583653101,-1.86021624962628,
21.9258472748593));
#27320=CARTESIAN_POINT('Ctrl Pts',(-0.344707483447601,-3.97197126386073,
22.0848121410441));
#27321=CARTESIAN_POINT('Ctrl Pts',(3.15313982968432,-2.43989387002868,22.2437770072288));
#27322=CARTESIAN_POINT('Ctrl Pts',(3.75834184644668,1.33050740634341,22.4027418734136));
#27323=CARTESIAN_POINT('Ctrl Pts',(0.915689325102905,3.88032175554439,22.5617067395983));
#27324=CARTESIAN_POINT('Ctrl Pts',(-2.76699741760937,2.87037799557025,22.720671605783));
#27325=CARTESIAN_POINT('Ctrl Pts',(-3.91129134187434,-0.7728027958352,22.8796364719677));
#27326=CARTESIAN_POINT('Ctrl Pts',(-1.46739644894177,-3.70704069007233,
23.0386013381526));
#27327=CARTESIAN_POINT('Ctrl Pts',(2.32262200499063,-3.24046036848089,23.1975662043372));
#27328=CARTESIAN_POINT('Ctrl Pts',(3.98198637087808,0.198816238648098,23.3565310705221));
#27329=CARTESIAN_POINT('Ctrl Pts',(1.98816433058814,3.45581133218519,23.5154959367067));
#27330=CARTESIAN_POINT('Ctrl Pts',(-1.82925354411967,3.5422830008711,23.6744608028915));
#27331=CARTESIAN_POINT('Ctrl Pts',(-3.96914826399699,0.379513463839679,
23.8334256690762));
#27332=CARTESIAN_POINT('Ctrl Pts',(-2.46663759784563,-3.13218185614485,
23.992390535261));
#27333=CARTESIAN_POINT('Ctrl Pts',(1.29650641132588,-3.76899081084458,24.1513554014457));
#27334=CARTESIAN_POINT('Ctrl Pts',(3.87454091099827,-0.951014904317504,
24.3103202676305));
#27335=CARTESIAN_POINT('Ctrl Pts',(2.88961752940844,2.74513957150359,24.4692851338152));
#27336=CARTESIAN_POINT('Ctrl Pts',(0.478408881098333,3.52136284087264,24.5752617112718));
#27337=CARTESIAN_POINT('Ctrl Pts',(-0.624728334461281,3.3133687646595,24.62825));
#27338=CARTESIAN_POINT('Ctrl Pts',(-1.56047750639987,3.20180677844002,-0.219489327336924));
#27339=CARTESIAN_POINT('Ctrl Pts',(-2.62647180561611,2.68226882971724,-0.166501038608675));
#27340=CARTESIAN_POINT('Ctrl Pts',(-4.1801468173981,0.503646678216414,-0.0605244611521764));
#27341=CARTESIAN_POINT('Ctrl Pts',(-2.683462008154,-3.24972419975438,0.0984404050325707));
#27342=CARTESIAN_POINT('Ctrl Pts',(1.27858859595154,-4.01162075153852,0.257405271217319));
#27343=CARTESIAN_POINT('Ctrl Pts',(4.06583468536472,-1.09841878093043,0.416370137402066));
#27344=CARTESIAN_POINT('Ctrl Pts',(3.12410178716573,2.82510367472183,0.575335003586814));
#27345=CARTESIAN_POINT('Ctrl Pts',(-0.684142221260432,4.15553253500754,
0.734299869771561));
#27346=CARTESIAN_POINT('Ctrl Pts',(-3.86450020240029,1.67445643711512,0.89326473595631));
#27347=CARTESIAN_POINT('Ctrl Pts',(-3.49975675527435,-2.3431216813317,1.05222960214106));
#27348=CARTESIAN_POINT('Ctrl Pts',(0.0756875806712427,-4.21095392107594,
1.2111944683258));
#27349=CARTESIAN_POINT('Ctrl Pts',(3.58165937251524,-2.21581878895911,1.37015933451055));
#27350=CARTESIAN_POINT('Ctrl Pts',(3.80188592579657,1.81213236997502,1.5291242006953));
#27351=CARTESIAN_POINT('Ctrl Pts',(0.534304277936582,4.17762976540319,1.68808906688005));
#27352=CARTESIAN_POINT('Ctrl Pts',(-3.22343533786296,2.71064199393843,1.8470539330648));
#27353=CARTESIAN_POINT('Ctrl Pts',(-4.02404256565933,-1.24305924958384,
2.00601879924955));
#27354=CARTESIAN_POINT('Ctrl Pts',(-1.1330470222017,-4.05639095560061,2.16498366543429));
#27355=CARTESIAN_POINT('Ctrl Pts',(2.79738949143739,-3.14844754849901,2.32394853161904));
#27356=CARTESIAN_POINT('Ctrl Pts',(4.1615397818786,0.647839440737169,2.48291339780379));
#27357=CARTESIAN_POINT('Ctrl Pts',(1.70795052048174,3.84980685419155,2.64187826398853));
#27358=CARTESIAN_POINT('Ctrl Pts',(-2.31248893740054,3.52001473505691,2.80084313017328));
#27359=CARTESIAN_POINT('Ctrl Pts',(-4.21148291955221,-0.0389906317936465,
2.95980799635803));
#27360=CARTESIAN_POINT('Ctrl Pts',(-2.2469203853454,-3.56222644534663,3.11877286254278));
#27361=CARTESIAN_POINT('Ctrl Pts',(1.77893597955331,-3.81752477372836,3.27773772872752));
#27362=CARTESIAN_POINT('Ctrl Pts',(4.17282096111768,-0.570678375934639,
3.43670259491227));
#27363=CARTESIAN_POINT('Ctrl Pts',(2.73861740129298,3.19970050005065,3.59566746109702));
#27364=CARTESIAN_POINT('Ctrl Pts',(-1.20795608026431,4.03471816744471,3.75463232728177));
#27365=CARTESIAN_POINT('Ctrl Pts',(-4.04636727494025,1.16834089733205,3.91359719346651));
#27366=CARTESIAN_POINT('Ctrl Pts',(-3.17269680384994,-2.76985623536663,
4.07256205965127));
#27367=CARTESIAN_POINT('Ctrl Pts',(0.611562062467236,-4.1670253683656,4.23152692583601));
#27368=CARTESIAN_POINT('Ctrl Pts',(3.83478230717035,-1.74142276094858,4.39049179202076));
#27369=CARTESIAN_POINT('Ctrl Pts',(3.5400260249384,2.28173712733952,4.54945665820551));
#27370=CARTESIAN_POINT('Ctrl Pts',(-0.00230142624457838,4.21166276895315,
4.70842152439025));
#27371=CARTESIAN_POINT('Ctrl Pts',(-3.54251758068034,2.27786693341294,4.867386390575));
#27372=CARTESIAN_POINT('Ctrl Pts',(-3.83287684714762,-1.74561268623704,
5.02635125675975));
#27373=CARTESIAN_POINT('Ctrl Pts',(-0.607007629585367,-4.16769124497425,
5.18531612294449));
#27374=CARTESIAN_POINT('Ctrl Pts',(3.17572203570494,-2.76638719772175,5.34428098912925));
#27375=CARTESIAN_POINT('Ctrl Pts',(4.04508799935564,1.17276240272716,5.50324585531399));
#27376=CARTESIAN_POINT('Ctrl Pts',(1.20354588769234,4.03603591064399,5.66221072149874));
#27377=CARTESIAN_POINT('Ctrl Pts',(-2.74211266207147,3.19670560488322,5.82117558768349));
#27378=CARTESIAN_POINT('Ctrl Pts',(-4.17219478365215,-0.575238440171331,
5.98014045386823));
#27379=CARTESIAN_POINT('Ctrl Pts',(-1.77476281483295,-3.81946665476637,
6.13910532005299));
#27380=CARTESIAN_POINT('Ctrl Pts',(2.2508121418228,-3.55976871130813,6.29807018623772));
#27381=CARTESIAN_POINT('Ctrl Pts',(4.21152300789809,-0.0343879300103317,
6.45703505242249));
#27382=CARTESIAN_POINT('Ctrl Pts',(2.30864061175677,3.52253986514459,6.61599991860723));
#27383=CARTESIAN_POINT('Ctrl Pts',(-1.71215691763581,3.84793805370841,6.77496478479197));
#27384=CARTESIAN_POINT('Ctrl Pts',(-4.16224524790261,0.643290814560192,
6.93392965097673));
#27385=CARTESIAN_POINT('Ctrl Pts',(-2.79394705497301,-3.1515025669977,7.09289451716147));
#27386=CARTESIAN_POINT('Ctrl Pts',(1.13747972501166,-4.05515085428062,7.25185938334622));
#27387=CARTESIAN_POINT('Ctrl Pts',(4.02539825555276,-1.23865954159255,7.41082424953096));
#27388=CARTESIAN_POINT('Ctrl Pts',(3.22047181083767,2.71416099216412,7.56978911571571));
#27389=CARTESIAN_POINT('Ctrl Pts',(-0.538871163521626,4.1770475751313,7.72875398190046));
#27390=CARTESIAN_POINT('Ctrl Pts',(-3.80386114665173,1.80796818356375,7.8877188480852));
#27391=CARTESIAN_POINT('Ctrl Pts',(-3.57924125016108,-2.21971634425003,
8.04668371426996));
#27392=CARTESIAN_POINT('Ctrl Pts',(-0.0710746766045851,-4.21106363833782,
8.2056485804547));
#27393=CARTESIAN_POINT('Ctrl Pts',(3.50229482737133,-2.33923908952323,8.36461344663945));
#27394=CARTESIAN_POINT('Ctrl Pts',(3.86270724386325,1.6785712150492,8.5235783128242));
#27395=CARTESIAN_POINT('Ctrl Pts',(0.679525180800456,4.15648338195204,8.68254317900894));
#27396=CARTESIAN_POINT('Ctrl Pts',(-3.12704393372178,2.82129488220555,8.8415080451937));
#27397=CARTESIAN_POINT('Ctrl Pts',(-4.06490596761654,-1.10211072502764,
9.00047291137844));
#27398=CARTESIAN_POINT('Ctrl Pts',(-1.27367919478393,-4.0144551167699,9.15943777756319));
#27399=CARTESIAN_POINT('Ctrl Pts',(2.68600334712891,-3.24399361821161,9.31840264374794));
#27400=CARTESIAN_POINT('Ctrl Pts',(4.18158337439399,0.502462992445402,9.47736750993269));
#27401=CARTESIAN_POINT('Ctrl Pts',(1.84103634728762,3.7879669670882,9.63633237611743));
#27402=CARTESIAN_POINT('Ctrl Pts',(-2.18845209448917,3.59844216375801,9.79529724230219));
#27403=CARTESIAN_POINT('Ctrl Pts',(-4.21028469511404,0.107756029408409,
9.95426210848692));
#27404=CARTESIAN_POINT('Ctrl Pts',(-2.36966004463275,-3.48178400373378,
10.1132269746717));
#27405=CARTESIAN_POINT('Ctrl Pts',(1.64485812726998,-3.87718329679412,10.2721918408564));
#27406=CARTESIAN_POINT('Ctrl Pts',(4.15040608438235,-0.71570797851312,10.4311567070412));
#27407=CARTESIAN_POINT('Ctrl Pts',(2.84842860401989,3.1023479920194,10.5901215732259));
#27408=CARTESIAN_POINT('Ctrl Pts',(-1.06665808689608,4.07435259905726,10.7490864394107));
#27409=CARTESIAN_POINT('Ctrl Pts',(-4.00320732475952,1.30860218965774,10.9080513055954));
#27410=CARTESIAN_POINT('Ctrl Pts',(-3.26726924195739,-2.657641863823,11.0670161717801));
#27411=CARTESIAN_POINT('Ctrl Pts',(0.466016689924724,-4.18580183722271,
11.2259810379649));
#27412=CARTESIAN_POINT('Ctrl Pts',(3.77178532227006,-1.87396479649261,11.3849459041496));
#27413=CARTESIAN_POINT('Ctrl Pts',(3.61736999495961,2.15702176515476,11.5439107703344));
#27414=CARTESIAN_POINT('Ctrl Pts',(0.144429204708414,4.20918623734002,11.7028756365191));
#27415=CARTESIAN_POINT('Ctrl Pts',(-3.4610089507791,2.39990116846763,11.8618405027039));
#27416=CARTESIAN_POINT('Ctrl Pts',(-3.89136511392694,-1.61102021275272,
12.0208053688886));
#27417=CARTESIAN_POINT('Ctrl Pts',(-0.751836461819641,-4.14401381639395,
12.1797702350734));
#27418=CARTESIAN_POINT('Ctrl Pts',(3.07741661604235,-2.87534616126336,12.3387351012581));
#27419=CARTESIAN_POINT('Ctrl Pts',(4.08349003170681,1.03112450108435,12.4976999674429));
#27420=CARTESIAN_POINT('Ctrl Pts',(1.34342587594075,3.99165573310602,12.6566648336276));
#27421=CARTESIAN_POINT('Ctrl Pts',(-2.62907869457274,3.29029691570976,12.8156296998124));
#27422=CARTESIAN_POINT('Ctrl Pts',(-4.18970264348228,-0.429535021835278,
12.9745945659971));
#27423=CARTESIAN_POINT('Ctrl Pts',(-1.90675103226963,-3.75531744020717,
13.1335594321819));
#27424=CARTESIAN_POINT('Ctrl Pts',(2.12542774146498,-3.63602330735055,13.2925242983666));
#27425=CARTESIAN_POINT('Ctrl Pts',(4.2077683483767,-0.181091419411761,13.4514891645514));
#27426=CARTESIAN_POINT('Ctrl Pts',(2.42996016605737,3.43997124510655,13.6104540307361));
#27427=CARTESIAN_POINT('Ctrl Pts',(-1.577060039425,3.90525161901692,13.7694188969209));
#27428=CARTESIAN_POINT('Ctrl Pts',(-4.13730706309004,0.787907888963343,
13.9283837631056));
#27429=CARTESIAN_POINT('Ctrl Pts',(-2.90204551118784,-3.05225169780932,
14.0873486292903));
#27430=CARTESIAN_POINT('Ctrl Pts',(0.995512664202879,-4.09231757213405,
14.2463134954751));
#27431=CARTESIAN_POINT('Ctrl Pts',(3.97980121844884,-1.37814761089607,14.4052783616599));
#27432=CARTESIAN_POINT('Ctrl Pts',(3.3130748919202,2.60031600701019,14.5642432278446));
#27433=CARTESIAN_POINT('Ctrl Pts',(-0.393020756736522,4.19328549714417,
14.7232080940294));
#27434=CARTESIAN_POINT('Ctrl Pts',(-3.73856457063159,1.9393925665021,14.8821729602141));
#27435=CARTESIAN_POINT('Ctrl Pts',(-3.65440068534852,-2.09367242106057,
15.0411378263989));
#27436=CARTESIAN_POINT('Ctrl Pts',(-0.217739891257386,-4.20603113582635,
15.2001026925836));
#27437=CARTESIAN_POINT('Ctrl Pts',(3.41867248324782,-2.45983475625287,15.3590675587684));
#27438=CARTESIAN_POINT('Ctrl Pts',(3.91884175823025,1.5429801844924,15.5180324249531));
#27439=CARTESIAN_POINT('Ctrl Pts',(0.823919522517587,4.13028633343982,15.6769972911379));
#27440=CARTESIAN_POINT('Ctrl Pts',(-3.02685514706235,2.92852462760477,15.8359621573226));
#27441=CARTESIAN_POINT('Ctrl Pts',(-4.10083455042517,-0.95982527880059,
15.9949270235073));
#27442=CARTESIAN_POINT('Ctrl Pts',(-1.41276475952385,-3.96764468041594,
16.1538918896921));
#27443=CARTESIAN_POINT('Ctrl Pts',(2.57135598390867,-3.3356014419895,16.3128567558768));
#27444=CARTESIAN_POINT('Ctrl Pts',(4.196550126309,0.356476665661734,16.4718216220616));
#27445=CARTESIAN_POINT('Ctrl Pts',(1.97188692205462,3.72152798490289,16.6307864882463));
#27446=CARTESIAN_POINT('Ctrl Pts',(-2.06175821382304,3.67250073431153,16.7897513544311));
#27447=CARTESIAN_POINT('Ctrl Pts',(-4.20397473152436,0.254371839027192,
16.9487162206158));
#27448=CARTESIAN_POINT('Ctrl Pts',(-2.48952267189958,-3.39711428154593,
17.1076810868006));
#27449=CARTESIAN_POINT('Ctrl Pts',(1.50878323424311,-3.93213450022406,17.2666459529853));
#27450=CARTESIAN_POINT('Ctrl Pts',(4.1229521602399,-0.859868629593263,17.4256108191701));
#27451=CARTESIAN_POINT('Ctrl Pts',(2.95478150103885,3.00122889112179,17.5845756853548));
#27452=CARTESIAN_POINT('Ctrl Pts',(-0.924065053159552,4.10904032023471,
17.7435405515396));
#27453=CARTESIAN_POINT('Ctrl Pts',(-3.95518704155557,1.44727469476127,17.9025054177243));
#27454=CARTESIAN_POINT('Ctrl Pts',(-3.35787485639895,-2.54220082301716,
18.0614702839091));
#27455=CARTESIAN_POINT('Ctrl Pts',(0.319905521907667,-4.1994962832271,18.2204351500938));
#27456=CARTESIAN_POINT('Ctrl Pts',(3.70420897591159,-2.00423163296111,18.3794000162786));
#27457=CARTESIAN_POINT('Ctrl Pts',(3.69032208064376,2.02968754169158,18.5383648824633));
#27458=CARTESIAN_POINT('Ctrl Pts',(0.290984482757316,4.20159929152924,18.6973297486481));
#27459=CARTESIAN_POINT('Ctrl Pts',(-3.37529827603299,2.51902166000967,18.8562946148328));
#27460=CARTESIAN_POINT('Ctrl Pts',(-3.94512883622391,-1.47447178385209,
19.0152594810176));
#27461=CARTESIAN_POINT('Ctrl Pts',(-0.895752482047657,-4.11530510007291,
19.1742243472023));
#27462=CARTESIAN_POINT('Ctrl Pts',(2.9753748747426,-2.98081413888224,19.333189213387));
#27463=CARTESIAN_POINT('Ctrl Pts',(4.1169342588298,0.888234701092859,19.4921540795718));
#27464=CARTESIAN_POINT('Ctrl Pts',(1.48167479769069,3.94242924726034,19.6511189457566));
#27465=CARTESIAN_POINT('Ctrl Pts',(-2.5128527369107,3.37989344485135,19.8100838119413));
#27466=CARTESIAN_POINT('Ctrl Pts',(-4.20212374428449,-0.283310100845846,
19.9690486781261));
#27467=CARTESIAN_POINT('Ctrl Pts',(-2.03642424467465,-3.68660885793949,
20.1280135443108));
#27468=CARTESIAN_POINT('Ctrl Pts',(1.9974628385994,-3.70786337197934,20.2869784104955));
#27469=CARTESIAN_POINT('Ctrl Pts',(4.1989049958817,-0.327575043797077,20.4459432766802));
#27470=CARTESIAN_POINT('Ctrl Pts',(2.54832948237039,3.35322612201562,20.6049081428651));
#27471=CARTESIAN_POINT('Ctrl Pts',(-1.44004843801888,3.95782378065465,20.7638730090497));
#27472=CARTESIAN_POINT('Ctrl Pts',(-4.10734573167046,0.931568355633416,
20.9228378752345));
#27473=CARTESIAN_POINT('Ctrl Pts',(-3.00662056859199,-2.94929505794555,
21.0818027414192));
#27474=CARTESIAN_POINT('Ctrl Pts',(0.852336947556435,-4.12451577099776,
21.240767607604));
#27475=CARTESIAN_POINT('Ctrl Pts',(3.92937225458326,-1.51596245036574,21.3997324737888));
#27476=CARTESIAN_POINT('Ctrl Pts',(3.4016555576228,2.48331393874026,21.5586973399735));
#27477=CARTESIAN_POINT('Ctrl Pts',(-0.246693220246651,4.20443233691565,
21.7176622061583));
#27478=CARTESIAN_POINT('Ctrl Pts',(-3.66872888914082,2.0684622628846,21.876627072343));
#27479=CARTESIAN_POINT('Ctrl Pts',(-3.72512342515035,-1.96508645217684,
22.0355919385278));
#27480=CARTESIAN_POINT('Ctrl Pts',(-0.364140462606384,-4.19589223597873,
22.1945568047125));
#27481=CARTESIAN_POINT('Ctrl Pts',(3.33089895455792,-2.57744355781532,22.3535216708973));
#27482=CARTESIAN_POINT('Ctrl Pts',(3.97021940141924,1.4055151272072,22.512486537082));
#27483=CARTESIAN_POINT('Ctrl Pts',(0.967311562579962,4.09907596143147,22.6714514032667));
#27484=CARTESIAN_POINT('Ctrl Pts',(-2.92298765783001,3.03219634429854,22.8304162694515));
#27485=CARTESIAN_POINT('Ctrl Pts',(-4.13179146670604,-0.816369765937287,
22.9893811356362));
#27486=CARTESIAN_POINT('Ctrl Pts',(-1.5501213272205,-3.91602612824874,23.148346001821));
#27487=CARTESIAN_POINT('Ctrl Pts',(2.45356045914115,-3.42314221273843,23.3073108680058));
#27488=CARTESIAN_POINT('Ctrl Pts',(4.20647194740789,0.210024558767638,23.4662757341905));
#27489=CARTESIAN_POINT('Ctrl Pts',(2.10024764138301,3.65063364623366,23.6252406003752));
#27490=CARTESIAN_POINT('Ctrl Pts',(-1.93237821563391,3.74198017901762,23.78420546656));
#27491=CARTESIAN_POINT('Ctrl Pts',(-4.19291008872147,0.400908639713182,
23.9431703327447));
#27492=CARTESIAN_POINT('Ctrl Pts',(-2.60569497064129,-3.30875946949763,
24.1021351989295));
#27493=CARTESIAN_POINT('Ctrl Pts',(1.36959731674678,-3.98146870411307,24.2611000651142));
#27494=CARTESIAN_POINT('Ctrl Pts',(4.09296922018457,-1.00462863103577,24.420064931299));
#27495=CARTESIAN_POINT('Ctrl Pts',(3.05252051214689,2.89989756964007,24.5790297974837));
#27496=CARTESIAN_POINT('Ctrl Pts',(0.505379313311694,3.71988063924714,24.6850063749402));
#27497=CARTESIAN_POINT('Ctrl Pts',(-0.659947566089433,3.50016083979823,
24.7379946636685));
#27498=CARTESIAN_POINT('Ctrl Pts',(-1.64375505990927,3.37267667834226,-0.109744663668463));
#27499=CARTESIAN_POINT('Ctrl Pts',(-2.76663796977808,2.82541269758923,-0.0567563749402136));
#27500=CARTESIAN_POINT('Ctrl Pts',(-4.40322750829897,0.530524645391819,
0.0492202025162849));
#27501=CARTESIAN_POINT('Ctrl Pts',(-2.82666955203587,-3.42315129487488,
0.208185068701033));
#27502=CARTESIAN_POINT('Ctrl Pts',(1.34682266518943,-4.22570776043514,0.36714993488578));
#27503=CARTESIAN_POINT('Ctrl Pts',(4.28281491364878,-1.15703777955712,0.526114801070528));
#27504=CARTESIAN_POINT('Ctrl Pts',(3.29082482718549,2.97587016861638,0.685079667255276));
#27505=CARTESIAN_POINT('Ctrl Pts',(-0.720652642080601,4.37729964259146,
0.844044533440024));
#27506=CARTESIAN_POINT('Ctrl Pts',(-4.07073587133658,1.76381667138256,1.00300939962477));
#27507=CARTESIAN_POINT('Ctrl Pts',(-3.68652726575071,-2.46816638104435,
1.16197426580952));
#27508=CARTESIAN_POINT('Ctrl Pts',(0.0797267779832985,-4.43567868580324,
1.32093913199426));
#27509=CARTESIAN_POINT('Ctrl Pts',(3.7728007563697,-2.33406975189055,1.47990399817901));
#27510=CARTESIAN_POINT('Ctrl Pts',(4.00478007667258,1.90883991608689,1.63886886436376));
#27511=CARTESIAN_POINT('Ctrl Pts',(0.562818340403771,4.40057612951542,1.79783373054851));
#27512=CARTESIAN_POINT('Ctrl Pts',(-3.39545948286473,2.85530004429109,1.95679859673326));
#27513=CARTESIAN_POINT('Ctrl Pts',(-4.23879248593139,-1.30939723443016,
2.11576346291801));
#27514=CARTESIAN_POINT('Ctrl Pts',(-1.19351401620389,-4.27286720307909,
2.27472832910275));
#27515=CARTESIAN_POINT('Ctrl Pts',(2.94667697049707,-3.31646984174982,2.4336931952875));
#27516=CARTESIAN_POINT('Ctrl Pts',(4.3836274764756,0.682412501528009,2.59265806147225));
#27517=CARTESIAN_POINT('Ctrl Pts',(1.79909822384654,4.05525838744716,2.751622927657));
#27518=CARTESIAN_POINT('Ctrl Pts',(-2.43589886829313,3.70786634730399,2.91058779384175));
#27519=CARTESIAN_POINT('Ctrl Pts',(-4.43623591518879,-0.041071433607366,
3.06955266002649));
#27520=CARTESIAN_POINT('Ctrl Pts',(-2.36683113821078,-3.75233075777553,
3.22851752621124));
#27521=CARTESIAN_POINT('Ctrl Pts',(1.87387194346144,-4.02125351849637,3.38748239239599));
#27522=CARTESIAN_POINT('Ctrl Pts',(4.39551069515703,-0.601133604410289,
3.54644725858073));
#27523=CARTESIAN_POINT('Ctrl Pts',(2.88476840715019,3.37045799480092,3.70541212476548));
#27524=CARTESIAN_POINT('Ctrl Pts',(-1.27242072438679,4.25003780948162,3.86437699095023));
#27525=CARTESIAN_POINT('Ctrl Pts',(-4.26230859154076,1.23069140940013,4.02334185713497));
#27526=CARTESIAN_POINT('Ctrl Pts',(-3.34201320012482,-2.91767435508194,
4.18230672331973));
#27527=CARTESIAN_POINT('Ctrl Pts',(0.64419911886348,-4.38940581067625,4.34127158950447));
#27528=CARTESIAN_POINT('Ctrl Pts',(4.03943202975366,-1.834356767727,4.50023645568922));
#27529=CARTESIAN_POINT('Ctrl Pts',(3.72894557392732,2.40350593524421,4.65920132187397));
#27530=CARTESIAN_POINT('Ctrl Pts',(-0.00242424579594498,4.43642536256088,
4.81816618805872));
#27531=CARTESIAN_POINT('Ctrl Pts',(-3.73157009580673,2.39942920179332,4.97713105424346));
#27532=CARTESIAN_POINT('Ctrl Pts',(-4.03742488159485,-1.83877029555123,
5.13609592042822));
#27533=CARTESIAN_POINT('Ctrl Pts',(-0.639401630874114,-4.39010722293004,
5.29506078661295));
#27534=CARTESIAN_POINT('Ctrl Pts',(3.34519987865668,-2.91402018630447,5.45402565279771));
#27535=CARTESIAN_POINT('Ctrl Pts',(4.26096104522458,1.23534887599985,5.61299051898245));
#27536=CARTESIAN_POINT('Ctrl Pts',(1.26777517433839,4.25142587630257,5.77195538516721));
#27537=CARTESIAN_POINT('Ctrl Pts',(-2.88845019850368,3.3673032719259,5.93092025135195));
#27538=CARTESIAN_POINT('Ctrl Pts',(-4.39485110065909,-0.605937024281373,
6.0898851175367));
#27539=CARTESIAN_POINT('Ctrl Pts',(-1.86947607066172,-4.02329903134028,
6.24884998372145));
#27540=CARTESIAN_POINT('Ctrl Pts',(2.37093058493492,-3.74974186255266,6.40781484990618));
#27541=CARTESIAN_POINT('Ctrl Pts',(4.43627814291787,-0.0362231007639915,
6.56677971609095));
#27542=CARTESIAN_POINT('Ctrl Pts',(2.43184517016341,3.71052623528157,6.72574458227568));
#27543=CARTESIAN_POINT('Ctrl Pts',(-1.80352910258568,4.05328985522703,6.88470944846044));
#27544=CARTESIAN_POINT('Ctrl Pts',(-4.38437059090167,0.677621130128278,
7.04367431464518));
#27545=CARTESIAN_POINT('Ctrl Pts',(-2.94305082251765,-3.31968789654059,
7.20263918082993));
#27546=CARTESIAN_POINT('Ctrl Pts',(1.19818327778767,-4.27156092162922,7.36160404701468));
#27547=CARTESIAN_POINT('Ctrl Pts',(4.2402205245368,-1.30476272849002,7.52056891319943));
#27548=CARTESIAN_POINT('Ctrl Pts',(3.39233780214647,2.85900683988128,7.67953377938417));
#27549=CARTESIAN_POINT('Ctrl Pts',(-0.567628945656141,4.39996286966301,
7.83849864556892));
#27550=CARTESIAN_POINT('Ctrl Pts',(-4.00686070857005,1.90445350073909,7.99746351175367));
#27551=CARTESIAN_POINT('Ctrl Pts',(-3.77025358677652,-2.33817530689181,
8.15642837793842));
#27552=CARTESIAN_POINT('Ctrl Pts',(-0.0748676983942658,-4.43579425831462,
8.31539324412316));
#27553=CARTESIAN_POINT('Ctrl Pts',(3.68920078641008,-2.4640765880774,8.47435811030792));
#27554=CARTESIAN_POINT('Ctrl Pts',(4.06884722849785,1.76815104148521,8.63332297649266));
#27555=CARTESIAN_POINT('Ctrl Pts',(0.715789205352545,4.37830123311092,8.79228784267741));
#27556=CARTESIAN_POINT('Ctrl Pts',(-3.29392398642918,2.97185811336718,8.95125270886215));
#27557=CARTESIAN_POINT('Ctrl Pts',(-4.28183663328808,-1.16092675057133,
9.1102175750469));
#27558=CARTESIAN_POINT('Ctrl Pts',(-1.34165126542409,-4.22869338641924,
9.26918244123165));
#27559=CARTESIAN_POINT('Ctrl Pts',(2.82934651391571,-3.41711489103788,9.42814730741641));
#27560=CARTESIAN_POINT('Ctrl Pts',(4.40474072961818,0.529277790203311,9.58711217360113));
#27561=CARTESIAN_POINT('Ctrl Pts',(1.93928640362945,3.99011830890487,9.74607703978591));
#27562=CARTESIAN_POINT('Ctrl Pts',(-2.30524258692121,3.79047918999758,9.90504190597063));
#27563=CARTESIAN_POINT('Ctrl Pts',(-4.43497374545224,0.113506614385248,
10.0640067721554));
#27564=CARTESIAN_POINT('Ctrl Pts',(-2.49612100953394,-3.66759536755666,
10.2229716383401));
#27565=CARTESIAN_POINT('Ctrl Pts',(1.73263879706324,-4.08409582077491,10.3819365045249));
#27566=CARTESIAN_POINT('Ctrl Pts',(4.3718996101527,-0.753902960006452,10.5409013707096));
#27567=CARTESIAN_POINT('Ctrl Pts',(3.00043987269634,3.26791010352089,10.6998662368944));
#27568=CARTESIAN_POINT('Ctrl Pts',(-1.12358212171453,4.29178740038732,10.8588311030791));
#27569=CARTESIAN_POINT('Ctrl Pts',(-4.21684533673315,1.37843798570399,11.0177959692639));
#27570=CARTESIAN_POINT('Ctrl Pts',(-3.44163265829037,-2.79947147150118,
11.1767608354486));
#27571=CARTESIAN_POINT('Ctrl Pts',(0.490886468356214,-4.40918431793734,
11.3357257016334));
#27572=CARTESIAN_POINT('Ctrl Pts',(3.97307310290967,-1.97397213589646,11.4946905678181));
#27573=CARTESIAN_POINT('Ctrl Pts',(3.8104171373138,2.27213492425632,11.6536554340029));
#27574=CARTESIAN_POINT('Ctrl Pts',(0.152136916465922,4.43381666659865,11.8126203001876));
#27575=CARTESIAN_POINT('Ctrl Pts',(-3.64571161833625,2.52797600271203,11.9715851663724));
#27576=CARTESIAN_POINT('Ctrl Pts',(-4.09903447485687,-1.69699506431066,
12.1305500325571));
#27577=CARTESIAN_POINT('Ctrl Pts',(-0.791959501672948,-4.36516620784018,
12.2895148987418));
#27578=CARTESIAN_POINT('Ctrl Pts',(3.24164822198482,-3.02879393146226,12.4484797649266));
#27579=CARTESIAN_POINT('Ctrl Pts',(4.30141246777259,1.08615222526604,12.6074446311113));
#27580=CARTESIAN_POINT('Ctrl Pts',(1.41512009762014,4.2046772746159,12.7664094972961));
#27581=CARTESIAN_POINT('Ctrl Pts',(-2.76938397982661,3.4658892432736,12.9253743634808));
#27582=CARTESIAN_POINT('Ctrl Pts',(-4.41329329740075,-0.452457893596237,
13.0843392296656));
#27583=CARTESIAN_POINT('Ctrl Pts',(-2.00850806527244,-3.95572638412914,
13.2433040958503));
#27584=CARTESIAN_POINT('Ctrl Pts',(2.23885483140653,-3.83006591565308,13.4022689620351));
#27585=CARTESIAN_POINT('Ctrl Pts',(4.43232310956353,-0.19075567301893,13.5612338282198));
#27586=CARTESIAN_POINT('Ctrl Pts',(2.55963915016612,3.62355119948605,13.7201986944046));
#27587=CARTESIAN_POINT('Ctrl Pts',(-1.66122254819691,4.11366205706328,13.8791635605893));
#27588=CARTESIAN_POINT('Ctrl Pts',(-4.35810153716492,0.829955942276827,
14.0381284267741));
#27589=CARTESIAN_POINT('Ctrl Pts',(-3.05691813790205,-3.21514033481048,
14.1970932929588));
#27590=CARTESIAN_POINT('Ctrl Pts',(1.04863990174551,-4.31071110500657,14.3560581591436));
#27591=CARTESIAN_POINT('Ctrl Pts',(4.19219012349031,-1.45169481740146,14.5150230253283));
#27592=CARTESIAN_POINT('Ctrl Pts',(3.48988280517811,2.73908632220345,14.6739878915131));
#27593=CARTESIAN_POINT('Ctrl Pts',(-0.413994982231739,4.41706735618179,
14.8329527576978));
#27594=CARTESIAN_POINT('Ctrl Pts',(-3.93807946898943,2.04289157085825,14.9919176238826));
#27595=CARTESIAN_POINT('Ctrl Pts',(-3.84942403388813,-2.20540483396684,
15.1508824900673));
#27596=CARTESIAN_POINT('Ctrl Pts',(-0.229359953303091,-4.4304931876915,
15.3098473562521));
#27597=CARTESIAN_POINT('Ctrl Pts',(3.60111579273939,-2.5911080490097,15.4688122224368));
#27598=CARTESIAN_POINT('Ctrl Pts',(4.12797745732068,1.62532396346455,15.6277770886216));
#27599=CARTESIAN_POINT('Ctrl Pts',(0.867889398303981,4.35070613425814,15.7867419548063));
#27600=CARTESIAN_POINT('Ctrl Pts',(-3.18838845365656,3.08481035769615,15.9457068209911));
#27601=CARTESIAN_POINT('Ctrl Pts',(-4.31968260642442,-1.01104799792802,
16.1046716871758));
#27602=CARTESIAN_POINT('Ctrl Pts',(-1.48815936942683,-4.1793848309945,16.2636365533605));
#27603=CARTESIAN_POINT('Ctrl Pts',(2.70858079789248,-3.51361152315505,16.4226014195453));
#27604=CARTESIAN_POINT('Ctrl Pts',(4.42050620787071,0.375500653176939,16.5815662857301));
#27605=CARTESIAN_POINT('Ctrl Pts',(2.07712004332191,3.92013369669841,16.7405311519148));
#27606=CARTESIAN_POINT('Ctrl Pts',(-2.17178747042617,3.8684900229495,16.8994960180995));
#27607=CARTESIAN_POINT('Ctrl Pts',(-4.42832703985357,0.267946827675841,
17.0584608842843));
#27608=CARTESIAN_POINT('Ctrl Pts',(-2.62238031109761,-3.57840710069821,
17.217425750469));
#27609=CARTESIAN_POINT('Ctrl Pts',(1.58930203442347,-4.14197958924682,17.3763906166538));
#27610=CARTESIAN_POINT('Ctrl Pts',(4.34298056035004,-0.905756991020003,
17.5353554828385));
#27611=CARTESIAN_POINT('Ctrl Pts',(3.11246847413016,3.16139460869816,17.6943203490233));
#27612=CARTESIAN_POINT('Ctrl Pts',(-0.973379366627741,4.32832629118729,
17.853285215208));
#27613=CARTESIAN_POINT('Ctrl Pts',(-4.16626236891013,1.52451098643573,18.0122500813928));
#27614=CARTESIAN_POINT('Ctrl Pts',(-3.53707359645429,-2.67786972192929,
18.1712149475776));
#27615=CARTESIAN_POINT('Ctrl Pts',(0.336977827730321,-4.42360959149628,
18.3301798137622));
#27616=CARTESIAN_POINT('Ctrl Pts',(3.90189042914389,-2.11119088509681,18.489144679947));
#27617=CARTESIAN_POINT('Ctrl Pts',(3.88726243593711,2.13800529197465,18.6481095461317));
#27618=CARTESIAN_POINT('Ctrl Pts',(0.306513367815784,4.42582483043659,18.8070744123165));
#27619=CARTESIAN_POINT('Ctrl Pts',(-3.55542684670427,2.6534535632075,18.9660392785013));
#27620=CARTESIAN_POINT('Ctrl Pts',(-4.15566739023229,-1.5531594947446,19.125004144686));
#27621=CARTESIAN_POINT('Ctrl Pts',(-0.943555846690173,-4.33492540172624,
19.2839690108708));
#27622=CARTESIAN_POINT('Ctrl Pts',(3.13416084847543,-3.13989038825732,19.4429338770555));
#27623=CARTESIAN_POINT('Ctrl Pts',(4.33664150332913,0.935636866485059,19.6018987432403));
#27624=CARTESIAN_POINT('Ctrl Pts',(1.5607469097475,4.15282373308227,19.760863609425));
#27625=CARTESIAN_POINT('Ctrl Pts',(-2.6469554249668,3.56026724457307,19.9198284756097));
#27626=CARTESIAN_POINT('Ctrl Pts',(-4.42637727151094,-0.298429429375862,
20.0787933417945));
#27627=CARTESIAN_POINT('Ctrl Pts',(-2.14510151064494,-3.88335105074656,
20.2377582079792));
#27628=CARTESIAN_POINT('Ctrl Pts',(2.10406086243651,-3.90573984831374,20.396723074164));
#27629=CARTESIAN_POINT('Ctrl Pts',(4.42298674908946,-0.345056646784782,
20.5556879403487));
#27630=CARTESIAN_POINT('Ctrl Pts',(2.68432544768054,3.53217677440245,20.7146528065335));
#27631=CARTESIAN_POINT('Ctrl Pts',(-1.51689908813168,4.16903982210505,20.8736176727182));
#27632=CARTESIAN_POINT('Ctrl Pts',(-4.32654126800335,0.981283095682997,
21.032582538903));
#27633=CARTESIAN_POINT('Ctrl Pts',(-3.16707402226655,-3.10668923760898,
21.1915474050877));
#27634=CARTESIAN_POINT('Ctrl Pts',(0.897823367877824,-4.34462761587273,
21.3505122712725));
#27635=CARTESIAN_POINT('Ctrl Pts',(4.13906993163872,-1.59686438170456,21.5094771374572));
#27636=CARTESIAN_POINT('Ctrl Pts',(3.58319072974711,2.61584023826454,21.668442003642));
#27637=CARTESIAN_POINT('Ctrl Pts',(-0.25985842625908,4.42880906613994,21.8274068698267));
#27638=CARTESIAN_POINT('Ctrl Pts',(-3.86451688680425,2.17884929254253,21.9863717360115));
#27639=CARTESIAN_POINT('Ctrl Pts',(-3.92392101376968,-2.0699566547274,22.1453366021962));
#27640=CARTESIAN_POINT('Ctrl Pts',(-0.383573441765164,-4.41981320809673,
22.304301468381));
#27641=CARTESIAN_POINT('Ctrl Pts',(3.50865807943151,-2.71499324560195,22.4632663345657));
#27642=CARTESIAN_POINT('Ctrl Pts',(4.1820969563918,1.48052284807099,22.6222312007505));
#27643=CARTESIAN_POINT('Ctrl Pts',(1.01893380005702,4.31783016731854,22.7811960669352));
#27644=CARTESIAN_POINT('Ctrl Pts',(-3.07897789805066,3.19401469302683,22.9401609331199));
#27645=CARTESIAN_POINT('Ctrl Pts',(-4.35229159153774,-0.859936736039379,
23.0991257993047));
#27646=CARTESIAN_POINT('Ctrl Pts',(-1.63284620549922,-4.12501156642513,
23.2580906654894));
#27647=CARTESIAN_POINT('Ctrl Pts',(2.58449891329166,-3.60582405699598,23.4170555316742));
#27648=CARTESIAN_POINT('Ctrl Pts',(4.43095752393771,0.221232878887186,23.5760203978589));
#27649=CARTESIAN_POINT('Ctrl Pts',(2.21233095217787,3.84545596028211,23.7349852640437));
#27650=CARTESIAN_POINT('Ctrl Pts',(-2.03550288714815,3.94167735716416,23.8939501302284));
#27651=CARTESIAN_POINT('Ctrl Pts',(-4.41667191344595,0.422303815586678,
24.0529149964132));
#27652=CARTESIAN_POINT('Ctrl Pts',(-2.74475234343696,-3.48533708285041,
24.2118798625979));
#27653=CARTESIAN_POINT('Ctrl Pts',(1.44268822216767,-4.19394659738156,24.3708447287827));
#27654=CARTESIAN_POINT('Ctrl Pts',(4.31139752937088,-1.05824235775403,24.5298095949674));
#27655=CARTESIAN_POINT('Ctrl Pts',(3.21542349488533,3.05465556777655,24.6887744611522));
#27656=CARTESIAN_POINT('Ctrl Pts',(0.532349745525053,3.91839843762163,24.7947510386087));
#27657=CARTESIAN_POINT('Ctrl Pts',(-0.695166797717585,3.68695291493697,
24.8477393273369));
#27658=CARTESIAN_POINT('Ctrl Pts',(-1.72703261341866,3.5435465782445,-1.38777878078145E-15));
#27659=CARTESIAN_POINT('Ctrl Pts',(-2.90680413394004,2.96855656546122,0.0529882887282479));
#27660=CARTESIAN_POINT('Ctrl Pts',(-4.62630819919985,0.557402612567225,
0.158964866184747));
#27661=CARTESIAN_POINT('Ctrl Pts',(-2.96987709591773,-3.59657838999538,
0.317929732369494));
#27662=CARTESIAN_POINT('Ctrl Pts',(1.41505673442732,-4.43979476933175,0.476894598554242));
#27663=CARTESIAN_POINT('Ctrl Pts',(4.49979514193284,-1.21565677818381,0.635859464738989));
#27664=CARTESIAN_POINT('Ctrl Pts',(3.45754786720525,3.12663666251093,0.794824330923737));
#27665=CARTESIAN_POINT('Ctrl Pts',(-0.757163062900767,4.59906675017539,
0.953789197108486));
#27666=CARTESIAN_POINT('Ctrl Pts',(-4.27697154027288,1.85317690565,1.11275406329323));
#27667=CARTESIAN_POINT('Ctrl Pts',(-3.87329777622707,-2.593211080757,1.27171892947798));
#27668=CARTESIAN_POINT('Ctrl Pts',(0.0837659752953463,-4.66040345053054,
1.43068379566273));
#27669=CARTESIAN_POINT('Ctrl Pts',(3.96394214022417,-2.45232071482198,1.58964866184748));
#27670=CARTESIAN_POINT('Ctrl Pts',(4.20767422754857,2.00554746219876,1.74861352803222));
#27671=CARTESIAN_POINT('Ctrl Pts',(0.591332402870964,4.62352249362764,1.90757839421698));
#27672=CARTESIAN_POINT('Ctrl Pts',(-3.5674836278665,2.99995809464374,2.06654326040171));
#27673=CARTESIAN_POINT('Ctrl Pts',(-4.45354240620347,-1.37573521927647,
2.22550812658647));
#27674=CARTESIAN_POINT('Ctrl Pts',(-1.25398101020607,-4.48934345055757,
2.38447299277121));
#27675=CARTESIAN_POINT('Ctrl Pts',(3.09596444955676,-3.48449213500062,2.54343785895597));
#27676=CARTESIAN_POINT('Ctrl Pts',(4.60571517107261,0.716985562318844,2.70240272514071));
#27677=CARTESIAN_POINT('Ctrl Pts',(1.89024592721134,4.26070992070277,2.86136759132546));
#27678=CARTESIAN_POINT('Ctrl Pts',(-2.55930879918572,3.89571795955106,3.0203324575102));
#27679=CARTESIAN_POINT('Ctrl Pts',(-4.66098891082537,-0.0431522354210798,
3.17929732369495));
#27680=CARTESIAN_POINT('Ctrl Pts',(-2.48674189107617,-3.94243507020443,
3.3382621898797));
#27681=CARTESIAN_POINT('Ctrl Pts',(1.96880790736958,-4.22498226326438,3.49722705606445));
#27682=CARTESIAN_POINT('Ctrl Pts',(4.61820042919637,-0.631588832885941,
3.65619192224919));
#27683=CARTESIAN_POINT('Ctrl Pts',(3.0309194130074,3.54121548955118,3.81515678843395));
#27684=CARTESIAN_POINT('Ctrl Pts',(-1.33688536850928,4.46535745151852,3.97412165461869));
#27685=CARTESIAN_POINT('Ctrl Pts',(-4.47824990814127,1.29304192146821,4.13308652080344));
#27686=CARTESIAN_POINT('Ctrl Pts',(-3.51132959639971,-3.06549247479725,
4.29205138698818));
#27687=CARTESIAN_POINT('Ctrl Pts',(0.676836175259727,-4.61178625298691,
4.45101625317294));
#27688=CARTESIAN_POINT('Ctrl Pts',(4.24408175233697,-1.92729077450542,4.60998111935768));
#27689=CARTESIAN_POINT('Ctrl Pts',(3.91786512291623,2.52527474314889,4.76894598554243));
#27690=CARTESIAN_POINT('Ctrl Pts',(-0.00254706534730991,4.66118795616863,
4.92791085172718));
#27691=CARTESIAN_POINT('Ctrl Pts',(-3.92062261093312,2.52099147017371,5.08687571791192));
#27692=CARTESIAN_POINT('Ctrl Pts',(-4.24197291604209,-1.93192790486543,
5.24584058409668));
#27693=CARTESIAN_POINT('Ctrl Pts',(-0.671795632162863,-4.61252320088583,
5.40480545028142));
#27694=CARTESIAN_POINT('Ctrl Pts',(3.51467772160843,-3.0616531748872,5.56377031646618));
#27695=CARTESIAN_POINT('Ctrl Pts',(4.47683409109351,1.29793534927254,5.72273518265091));
#27696=CARTESIAN_POINT('Ctrl Pts',(1.33200446098445,4.46681584196115,5.88170004883567));
#27697=CARTESIAN_POINT('Ctrl Pts',(-3.03478773493588,3.53790093896858,6.04066491502041));
#27698=CARTESIAN_POINT('Ctrl Pts',(-4.61750741766603,-0.636635608391419,
6.19962978120516));
#27699=CARTESIAN_POINT('Ctrl Pts',(-1.96418932649049,-4.22713140791419,
6.35859464738991));
#27700=CARTESIAN_POINT('Ctrl Pts',(2.49104902804703,-3.93971501379719,6.51755951357465));
#27701=CARTESIAN_POINT('Ctrl Pts',(4.66103327793766,-0.0380582715176506,
6.6765243797594));
#27702=CARTESIAN_POINT('Ctrl Pts',(2.55504972857005,3.89851260541856,6.83548924594414));
#27703=CARTESIAN_POINT('Ctrl Pts',(-1.89490128753556,4.25864165674564,6.9944541121289));
#27704=CARTESIAN_POINT('Ctrl Pts',(-4.60649593390074,0.711951445696367,
7.15341897831364));
#27705=CARTESIAN_POINT('Ctrl Pts',(-3.09215459006229,-3.48787322608348,
7.3123838444984));
#27706=CARTESIAN_POINT('Ctrl Pts',(1.25888683056368,-4.48797098897782,7.47134871068314));
#27707=CARTESIAN_POINT('Ctrl Pts',(4.45504279352084,-1.3708659153875,7.63031357686789));
#27708=CARTESIAN_POINT('Ctrl Pts',(3.56420379345526,3.00385268759844,7.78927844305264));
#27709=CARTESIAN_POINT('Ctrl Pts',(-0.596386727790659,4.62287816419472,
7.94824330923738));
#27710=CARTESIAN_POINT('Ctrl Pts',(-4.20986027048837,2.00093881791443,8.10720817542214));
#27711=CARTESIAN_POINT('Ctrl Pts',(-3.96126592339197,-2.45663426953358,
8.26617304160689));
#27712=CARTESIAN_POINT('Ctrl Pts',(-0.0786607201839425,-4.66052487829143,
8.42513790779162));
#27713=CARTESIAN_POINT('Ctrl Pts',(3.87610674544883,-2.58891408663156,8.58410277397638));
#27714=CARTESIAN_POINT('Ctrl Pts',(4.27498721313245,1.85773086792121,8.74306764016112));
#27715=CARTESIAN_POINT('Ctrl Pts',(0.752053229904626,4.60011908426979,8.90203250634587));
#27716=CARTESIAN_POINT('Ctrl Pts',(-3.46080403913657,3.12242134452881,9.06099737253062));
#27717=CARTESIAN_POINT('Ctrl Pts',(-4.49876729895963,-1.21974277611503,
9.21996223871536));
#27718=CARTESIAN_POINT('Ctrl Pts',(-1.40962333606424,-4.44293165606859,
9.37892710490011));
#27719=CARTESIAN_POINT('Ctrl Pts',(2.97268968070251,-3.59023616386415,9.53789197108486));
#27720=CARTESIAN_POINT('Ctrl Pts',(4.62789808484238,0.556092587961218,9.69685683726961));
#27721=CARTESIAN_POINT('Ctrl Pts',(2.03753645997128,4.19226965072155,9.85582170345435));
#27722=CARTESIAN_POINT('Ctrl Pts',(-2.42203307935326,3.98251621623715,10.0147865696391));
#27723=CARTESIAN_POINT('Ctrl Pts',(-4.65966279579043,0.119257199362087,
10.1737514358238));
#27724=CARTESIAN_POINT('Ctrl Pts',(-2.62258197443514,-3.85340673137953,
10.3327163020086));
#27725=CARTESIAN_POINT('Ctrl Pts',(1.82041946685649,-4.2910083447557,10.4916811681933));
#27726=CARTESIAN_POINT('Ctrl Pts',(4.59339313592305,-0.792097941499782,
10.6506460343781));
#27727=CARTESIAN_POINT('Ctrl Pts',(3.15245114137279,3.43347221502238,10.8096109005628));
#27728=CARTESIAN_POINT('Ctrl Pts',(-1.18050615653299,4.50922220171738,10.9685757667476));
#27729=CARTESIAN_POINT('Ctrl Pts',(-4.43048334870678,1.44827378175024,11.1275406329323));
#27730=CARTESIAN_POINT('Ctrl Pts',(-3.61599607462336,-2.94130107917936,
11.2865054991171));
#27731=CARTESIAN_POINT('Ctrl Pts',(0.515756246787712,-4.63256679865198,
11.4454703653018));
#27732=CARTESIAN_POINT('Ctrl Pts',(4.17436088354928,-2.07397947530031,11.6044352314866));
#27733=CARTESIAN_POINT('Ctrl Pts',(4.00346427966798,2.38724808335786,11.7634000976713));
#27734=CARTESIAN_POINT('Ctrl Pts',(0.159844628223428,4.6584470958573,11.9223649638561));
#27735=CARTESIAN_POINT('Ctrl Pts',(-3.83041428589339,2.65605083695643,12.0813298300408));
#27736=CARTESIAN_POINT('Ctrl Pts',(-4.3067038357868,-1.7829699158686,12.2402946962256));
#27737=CARTESIAN_POINT('Ctrl Pts',(-0.832082541526254,-4.58631859928641,
12.3992595624103));
#27738=CARTESIAN_POINT('Ctrl Pts',(3.40587982792729,-3.18224170166115,12.5582244285951));
#27739=CARTESIAN_POINT('Ctrl Pts',(4.51933490383836,1.14117994944773,12.7171892947798));
#27740=CARTESIAN_POINT('Ctrl Pts',(1.48681431929952,4.41769881612578,12.8761541609645));
#27741=CARTESIAN_POINT('Ctrl Pts',(-2.90968926508048,3.64148157083744,13.0351190271493));
#27742=CARTESIAN_POINT('Ctrl Pts',(-4.63688395131922,-0.475380765357195,
13.1940838933341));
#27743=CARTESIAN_POINT('Ctrl Pts',(-2.11026509827526,-4.1561353280511,13.3530487595188));
#27744=CARTESIAN_POINT('Ctrl Pts',(2.35228192134809,-4.0241085239556,13.5120136257036));
#27745=CARTESIAN_POINT('Ctrl Pts',(4.65687787075036,-0.200419926626097,
13.6709784918883));
#27746=CARTESIAN_POINT('Ctrl Pts',(2.68931813427488,3.80713115386554,13.829943358073));
#27747=CARTESIAN_POINT('Ctrl Pts',(-1.74538505696882,4.32207249510964,13.9889082242578));
#27748=CARTESIAN_POINT('Ctrl Pts',(-4.57889601123979,0.872003995590307,
14.1478730904425));
#27749=CARTESIAN_POINT('Ctrl Pts',(-3.21179076461628,-3.37802897181164,
14.3068379566273));
#27750=CARTESIAN_POINT('Ctrl Pts',(1.10176713928815,-4.5291046378791,14.465802822812));
#27751=CARTESIAN_POINT('Ctrl Pts',(4.40457902853176,-1.52524202390685,14.6247676889968));
#27752=CARTESIAN_POINT('Ctrl Pts',(3.66669071843603,2.87785663739672,14.7837325551815));
#27753=CARTESIAN_POINT('Ctrl Pts',(-0.434969207726955,4.6408492152194,14.9426974213663));
#27754=CARTESIAN_POINT('Ctrl Pts',(-4.13759436734728,2.14639057521441,15.101662287551));
#27755=CARTESIAN_POINT('Ctrl Pts',(-4.04444738242773,-2.3171372468731,15.2606271537358));
#27756=CARTESIAN_POINT('Ctrl Pts',(-0.240980015348797,-4.65495523955664,
15.4195920199205));
#27757=CARTESIAN_POINT('Ctrl Pts',(3.78355910223096,-2.72238134176653,15.5785568861053));
#27758=CARTESIAN_POINT('Ctrl Pts',(4.33711315641111,1.7076677424367,15.73752175229));
#27759=CARTESIAN_POINT('Ctrl Pts',(0.911859274090375,4.57112593507645,15.8964866184748));
#27760=CARTESIAN_POINT('Ctrl Pts',(-3.34992176025076,3.24109608778754,16.0554514846595));
#27761=CARTESIAN_POINT('Ctrl Pts',(-4.53853066242366,-1.06227071705545,
16.2144163508443));
#27762=CARTESIAN_POINT('Ctrl Pts',(-1.56355397932982,-4.39112498157307,
16.373381217029));
#27763=CARTESIAN_POINT('Ctrl Pts',(2.8458056118763,-3.69162160432059,16.5323460832138));
#27764=CARTESIAN_POINT('Ctrl Pts',(4.64446228943243,0.394524640692141,16.6913109493985));
#27765=CARTESIAN_POINT('Ctrl Pts',(2.18235316458919,4.11873940849393,16.8502758155833));
#27766=CARTESIAN_POINT('Ctrl Pts',(-2.2818167270293,4.06447931158747,17.009240681768));
#27767=CARTESIAN_POINT('Ctrl Pts',(-4.65267934818278,0.281521816324489,
17.1682055479527));
#27768=CARTESIAN_POINT('Ctrl Pts',(-2.75523795029565,-3.75969991985049,
17.3271704141375));
#27769=CARTESIAN_POINT('Ctrl Pts',(1.66982083460383,-4.35182467826958,17.4861352803222));
#27770=CARTESIAN_POINT('Ctrl Pts',(4.56300896046017,-0.95164535244674,17.645100146507));
#27771=CARTESIAN_POINT('Ctrl Pts',(3.27015544722148,3.32156032627453,17.8040650126917));
#27772=CARTESIAN_POINT('Ctrl Pts',(-1.02269368009593,4.54761226213988,17.9630298788765));
#27773=CARTESIAN_POINT('Ctrl Pts',(-4.37733769626469,1.6017472781102,18.1219947450612));
#27774=CARTESIAN_POINT('Ctrl Pts',(-3.71627233650965,-2.81353862084143,
18.280959611246));
#27775=CARTESIAN_POINT('Ctrl Pts',(0.354050133552978,-4.64772289976546,
18.4399244774307));
#27776=CARTESIAN_POINT('Ctrl Pts',(4.09957188237618,-2.21815013723249,18.5988893436155));
#27777=CARTESIAN_POINT('Ctrl Pts',(4.08420279123045,2.24632304225772,18.7578542098002));
#27778=CARTESIAN_POINT('Ctrl Pts',(0.322042252874243,4.65005036934395,18.916819075985));
#27779=CARTESIAN_POINT('Ctrl Pts',(-3.73555541737554,2.78788546640533,19.0757839421697));
#27780=CARTESIAN_POINT('Ctrl Pts',(-4.36620594424068,-1.63184720563709,
19.2347488083544));
#27781=CARTESIAN_POINT('Ctrl Pts',(-0.991359211332678,-4.55454570337957,
19.3937136745392));
#27782=CARTESIAN_POINT('Ctrl Pts',(3.29294682220825,-3.29896663763241,19.5526785407239));
#27783=CARTESIAN_POINT('Ctrl Pts',(4.55634874782847,0.983039031877256,19.7116434069087));
#27784=CARTESIAN_POINT('Ctrl Pts',(1.63981902180431,4.3632182189042,19.8706082730935));
#27785=CARTESIAN_POINT('Ctrl Pts',(-2.7810581130229,3.74064104429479,20.0295731392782));
#27786=CARTESIAN_POINT('Ctrl Pts',(-4.65063079873739,-0.313548757905883,
20.188538005463));
#27787=CARTESIAN_POINT('Ctrl Pts',(-2.25377877661524,-4.08009324355364,
20.3475028716477));
#27788=CARTESIAN_POINT('Ctrl Pts',(2.21065888627362,-4.10361632464813,20.5064677378324));
#27789=CARTESIAN_POINT('Ctrl Pts',(4.64706850229723,-0.362538249772487,
20.6654326040172));
#27790=CARTESIAN_POINT('Ctrl Pts',(2.82032141299069,3.71112742678928,20.824397470202));
#27791=CARTESIAN_POINT('Ctrl Pts',(-1.59374973824449,4.38025586355546,20.9833623363867));
#27792=CARTESIAN_POINT('Ctrl Pts',(-4.54573680433624,1.03099783573258,21.1423272025715));
#27793=CARTESIAN_POINT('Ctrl Pts',(-3.32752747594111,-3.2640834172724,21.3012920687562));
#27794=CARTESIAN_POINT('Ctrl Pts',(0.943309788199209,-4.5647394607477,21.4602569349409));
#27795=CARTESIAN_POINT('Ctrl Pts',(4.34876760869419,-1.67776631304337,21.6192218011257));
#27796=CARTESIAN_POINT('Ctrl Pts',(3.76472590187142,2.74836653778883,21.7781866673104));
#27797=CARTESIAN_POINT('Ctrl Pts',(-0.273023632271506,4.65318579536423,
21.9371515334952));
#27798=CARTESIAN_POINT('Ctrl Pts',(-4.06030488446768,2.28923632220046,22.0961163996799));
#27799=CARTESIAN_POINT('Ctrl Pts',(-4.12271860238902,-2.17482685727795,
22.2550812658647));
#27800=CARTESIAN_POINT('Ctrl Pts',(-0.403006420923942,-4.64373418021473,
22.4140461320495));
#27801=CARTESIAN_POINT('Ctrl Pts',(3.68641720430509,-2.85254293338859,22.5730109982341));
#27802=CARTESIAN_POINT('Ctrl Pts',(4.39397451136436,1.55553056893478,22.7319758644189));
#27803=CARTESIAN_POINT('Ctrl Pts',(1.07055603753408,4.53658437320562,22.8909407306037));
#27804=CARTESIAN_POINT('Ctrl Pts',(-3.2349681382713,3.35583304175512,23.0499055967884));
#27805=CARTESIAN_POINT('Ctrl Pts',(-4.57279171636944,-0.903503706141469,
23.2088704629732));
#27806=CARTESIAN_POINT('Ctrl Pts',(-1.71557108377795,-4.33399700460152,
23.3678353291579));
#27807=CARTESIAN_POINT('Ctrl Pts',(2.71543736744218,-3.78850590125353,23.5268001953427));
#27808=CARTESIAN_POINT('Ctrl Pts',(4.65544310046753,0.232441199006727,23.6857650615274));
#27809=CARTESIAN_POINT('Ctrl Pts',(2.32441426297274,4.04027827433057,23.8447299277122));
#27810=CARTESIAN_POINT('Ctrl Pts',(-2.13862755866238,4.14137453531068,24.0036947938969));
#27811=CARTESIAN_POINT('Ctrl Pts',(-4.64043373817043,0.443698991460186,
24.1626596600816));
#27812=CARTESIAN_POINT('Ctrl Pts',(-2.88380971623262,-3.66191469620319,
24.3216245262664));
#27813=CARTESIAN_POINT('Ctrl Pts',(1.51577912758857,-4.40642449065004,24.4805893924511));
#27814=CARTESIAN_POINT('Ctrl Pts',(4.52982583855719,-1.1118560844723,24.6395542586359));
#27815=CARTESIAN_POINT('Ctrl Pts',(3.37832647762378,3.20941356591303,24.7985191248206));
#27816=CARTESIAN_POINT('Ctrl Pts',(0.559320177738415,4.11691623599613,24.9044957022771));
#27817=CARTESIAN_POINT('Ctrl Pts',(-0.730386029345736,3.8737449900757,24.9574839910054));
#27818=CARTESIAN_POINT('Ctrl Pts',(-3.94350653563855,-0.00347714007584369,
23.1778238829104));
#27819=CARTESIAN_POINT('Ctrl Pts',(-3.94586355936157,-0.259474013504655,
23.1881727429313));
#27820=CARTESIAN_POINT('Ctrl Pts',(-3.92307523690983,-0.515053183369563,
23.1985216029522));
#27821=CARTESIAN_POINT('Ctrl Pts',(-3.87361768125451,-0.765363131235343,
23.2088704629732));
#27822=CARTESIAN_POINT('Ctrl Pts',(-3.62038483883896,-2.0470014722948,23.2618587517014));
#27823=CARTESIAN_POINT('Ctrl Pts',(-2.66797796130846,-3.19049923844816,
23.3148470404297));
#27824=CARTESIAN_POINT('Ctrl Pts',(-1.45327311400651,-3.67133293763351,
23.3678353291579));
#27825=CARTESIAN_POINT('Ctrl Pts',(-0.238568266704596,-4.15216663681884,
23.4208236178862));
#27826=CARTESIAN_POINT('Ctrl Pts',(1.23843455036875,-3.9703362690362,23.4738119066144));
#27827=CARTESIAN_POINT('Ctrl Pts',(2.30027024774299,-3.20926323510153,23.5268001953427));
#27828=CARTESIAN_POINT('Ctrl Pts',(3.36210594511727,-2.44819020116684,23.5797884840709));
#27829=CARTESIAN_POINT('Ctrl Pts',(4.00877452279241,-1.10787450108007,23.6327767727992));
#27830=CARTESIAN_POINT('Ctrl Pts',(3.94360400538084,0.196922861517294,23.6857650615274));
#27831=CARTESIAN_POINT('Ctrl Pts',(3.87843348796927,1.50172022411466,23.7387533502557));
#27832=CARTESIAN_POINT('Ctrl Pts',(3.10142387547099,2.77099924922264,23.7917416389839));
#27833=CARTESIAN_POINT('Ctrl Pts',(1.96907876561599,3.42248813860663,23.8447299277122));
#27834=CARTESIAN_POINT('Ctrl Pts',(0.836733655761017,4.07397702799061,23.8977182164404));
#27835=CARTESIAN_POINT('Ctrl Pts',(-0.650946951450773,4.10767578165063,
23.9507065051686));
#27836=CARTESIAN_POINT('Ctrl Pts',(-1.81175495164127,3.50824590117222,24.0036947938969));
#27837=CARTESIAN_POINT('Ctrl Pts',(-2.20830746798924,3.30347006620307,24.0217965292646));
#27838=CARTESIAN_POINT('Ctrl Pts',(-2.56671309215799,3.02480645592577,24.0398982646323));
#27839=CARTESIAN_POINT('Ctrl Pts',(-2.87170785494343,2.69478584831398,24.058));
#27840=CARTESIAN_POINT('Ctrl Pts',(-1.96186193197213,-2.74910310536279,
1.04083408558608E-17));
#27841=CARTESIAN_POINT('Ctrl Pts',(-2.03089214936932,-2.70842374984998,
4.0844089957036E-17));
#27842=CARTESIAN_POINT('Ctrl Pts',(-2.0982520786512,-2.66519645821488,9.07751022854637E-17));
#27843=CARTESIAN_POINT('Ctrl Pts',(-2.16378064478676,-2.619448737651,1.42247325030098E-16));
#27844=CARTESIAN_POINT('Ctrl Pts',(-2.25130095090051,-2.55834783549675,
1.98311708005797E-16));
#27845=CARTESIAN_POINT('Ctrl Pts',(-2.33555581159229,-2.49275291176235,
1.14301651927622E-16));
#27846=CARTESIAN_POINT('Ctrl Pts',(-2.41645347142118,-2.4230636931251,1.90819582357449E-16));
#27847=CARTESIAN_POINT('Ctrl Pts',(-2.46698855966785,-2.37953028534638,
2.38618744594068E-16));
#27848=CARTESIAN_POINT('Ctrl Pts',(-2.51621317497323,-2.33439817262585,
-8.87118969308996E-17));
#27849=CARTESIAN_POINT('Ctrl Pts',(-2.56410004332752,-2.28775595645186,
-9.0205620750794E-17));
#27850=CARTESIAN_POINT('Ctrl Pts',(-2.58450501257648,-2.26788134323446,
-9.08421081566083E-17));
#27851=CARTESIAN_POINT('Ctrl Pts',(-2.60466703883067,-2.24773246660606,
1.20223089018126E-16));
#27852=CARTESIAN_POINT('Ctrl Pts',(-2.62458377340069,-2.22731585490721,
1.31838984174237E-16));
#27853=CARTESIAN_POINT('Ctrl Pts',(-2.6428539078105,-2.20858717031188,1.42494544454281E-16));
#27854=CARTESIAN_POINT('Ctrl Pts',(-2.66092072754138,-2.18962968712113,
4.62480998826576E-16));
#27855=CARTESIAN_POINT('Ctrl Pts',(-2.67876242915531,-2.17047018454057,
4.44089209850063E-16));
#27856=CARTESIAN_POINT('Ctrl Pts',(-2.75353668750271,-2.09017304546908,
3.67009545019966E-16));
#27857=CARTESIAN_POINT('Ctrl Pts',(-2.82442308955658,-2.00626812836577,
4.38199731939201E-16));
#27858=CARTESIAN_POINT('Ctrl Pts',(-2.89132427090349,-1.91917015947591,
2.28983498828939E-16));
#27859=CARTESIAN_POINT('Ctrl Pts',(-2.9553640840902,-1.83579737674842,2.87154585004375E-17));
#27860=CARTESIAN_POINT('Ctrl Pts',(-3.01575243661163,-1.74949800545801,
1.64657856526806E-16));
#27861=CARTESIAN_POINT('Ctrl Pts',(-3.07237914628982,-1.6606009570442,2.22044604925031E-16));
#27862=CARTESIAN_POINT('Ctrl Pts',(-3.09715333177403,-1.62170849836315,
2.47151307349255E-16));
#27863=CARTESIAN_POINT('Ctrl Pts',(-3.12120717339458,-1.58231843772374,
3.74830717982145E-16));
#27864=CARTESIAN_POINT('Ctrl Pts',(-3.14452974084395,-1.54245667505035,
4.16333634234434E-16));
#27865=CARTESIAN_POINT('Ctrl Pts',(-3.1552141693008,-1.52419538574881,4.35346761344512E-16));
#27866=CARTESIAN_POINT('Ctrl Pts',(-3.1657451101877,-1.50583508811633,6.65859873947159E-18));
#27867=CARTESIAN_POINT('Ctrl Pts',(-3.17612143314624,-1.48737821330264,
4.16333634234434E-17));
#27868=CARTESIAN_POINT('Ctrl Pts',(-3.1851701035806,-1.47128289918176,7.21331002193362E-17));
#27869=CARTESIAN_POINT('Ctrl Pts',(-3.19410146294443,-1.45511349134961,
1.2766348924177E-16));
#27870=CARTESIAN_POINT('Ctrl Pts',(-3.20290718418031,-1.4388859283946,1.2490009027033E-16));
#27871=CARTESIAN_POINT('Ctrl Pts',(-3.25753999780039,-1.33820622270319,
1.07755298047126E-16));
#27872=CARTESIAN_POINT('Ctrl Pts',(-3.30741231186542,-1.23516335787123,
5.68363615759287E-16));
#27873=CARTESIAN_POINT('Ctrl Pts',(-3.35241796906181,-1.13019103593447,
4.71844785465692E-16));
#27874=CARTESIAN_POINT('Ctrl Pts',(-3.39804200535616,-1.0237763911033,3.73999783509847E-16));
#27875=CARTESIAN_POINT('Ctrl Pts',(-3.43866526602443,-0.915378183946712,
-6.22512805566231E-17));
#27876=CARTESIAN_POINT('Ctrl Pts',(-3.47413966247048,-0.805410191460158,
-1.66533453693773E-16));
#27877=CARTESIAN_POINT('Ctrl Pts',(-3.50939387582959,-0.696124750178875,
-2.70168366465852E-16));
#27878=CARTESIAN_POINT('Ctrl Pts',(-3.53956336356882,-0.585288114116654,
-7.73645964354313E-17));
#27879=CARTESIAN_POINT('Ctrl Pts',(-3.56445901023683,-0.473280938901883,
-1.38777878078145E-16));
#27880=CARTESIAN_POINT('Ctrl Pts',(-3.58104437402115,-0.39866228078212,
-1.79691120092537E-16));
#27881=CARTESIAN_POINT('Ctrl Pts',(-3.59528821670414,-0.323523611696084,
-9.85603223433227E-18));
#27882=CARTESIAN_POINT('Ctrl Pts',(-3.60712230450606,-0.24797391740747,
-2.77555756156289E-17));
#27883=CARTESIAN_POINT('Ctrl Pts',(-3.61048639425725,-0.226497318913744,
-3.28438994009322E-17));
#27884=CARTESIAN_POINT('Ctrl Pts',(-3.613655686349,-0.204987494839638,2.70286722177284E-16));
#27885=CARTESIAN_POINT('Ctrl Pts',(-3.61662845468875,-0.183446929103701,
2.77555756156289E-16));
#27886=CARTESIAN_POINT('Ctrl Pts',(-3.61934694140478,-0.163748878291719,
2.84203018926811E-16));
#27887=CARTESIAN_POINT('Ctrl Pts',(-3.62190130092961,-0.144022588989176,
-9.4234710418247E-17));
#27888=CARTESIAN_POINT('Ctrl Pts',(-3.62428757941211,-0.124293547804644,
-8.32667268468867E-17));
#27889=CARTESIAN_POINT('Ctrl Pts',(-3.63845233765523,-0.007183537050793,
-1.81616534692129E-17));
#27890=CARTESIAN_POINT('Ctrl Pts',(-3.64672404198312,0.110194833970378,
2.72159498670366E-16));
#27891=CARTESIAN_POINT('Ctrl Pts',(-3.64895596115005,0.227419084314086,
2.4980018054066E-16));
#27892=CARTESIAN_POINT('Ctrl Pts',(-3.6502760977502,0.296754939123098,2.36575080521473E-16));
#27893=CARTESIAN_POINT('Ctrl Pts',(-3.64948239134564,0.366037414325706,
-3.91023963353986E-16));
#27894=CARTESIAN_POINT('Ctrl Pts',(-3.64653656430167,0.435182446792325,
-3.33066907387547E-16));
#27895=CARTESIAN_POINT('Ctrl Pts',(-3.64171075252927,0.548454851010284,
-2.38122486414389E-16));
#27896=CARTESIAN_POINT('Ctrl Pts',(-3.63111244226456,0.661358405661847,
1.01745842338307E-16));
#27897=CARTESIAN_POINT('Ctrl Pts',(-3.61501201454962,0.773605457518614,
8.32667268468867E-17));
#27898=CARTESIAN_POINT('Ctrl Pts',(-3.5986111375463,0.887947146080084,6.44427734916789E-17));
#27899=CARTESIAN_POINT('Ctrl Pts',(-3.57650072189919,1.00160829055033,1.76269981291295E-16));
#27900=CARTESIAN_POINT('Ctrl Pts',(-3.5489124899874,1.11428362811214,1.66533453693773E-16));
#27901=CARTESIAN_POINT('Ctrl Pts',(-3.53981806230419,1.1514269184982,1.63323819005896E-16));
#27902=CARTESIAN_POINT('Ctrl Pts',(-3.53012795001213,1.18846302772386,5.91487372108521E-17));
#27903=CARTESIAN_POINT('Ctrl Pts',(-3.51984924725713,1.22538078979166,5.55111512312578E-17));
#27904=CARTESIAN_POINT('Ctrl Pts',(-3.51512490385872,1.24234909694735,5.38392276706252E-17));
#27905=CARTESIAN_POINT('Ctrl Pts',(-3.51027554782375,1.25929445386572,-8.56270895207211E-17));
#27906=CARTESIAN_POINT('Ctrl Pts',(-3.5053071420154,1.27619828084334,-8.32667268468867E-17));
#27907=CARTESIAN_POINT('Ctrl Pts',(-3.4726474677456,1.38731510670219,-6.77509499438615E-17));
#27908=CARTESIAN_POINT('Ctrl Pts',(-3.43480620738079,1.4967920748245,-3.16991689118145E-16));
#27909=CARTESIAN_POINT('Ctrl Pts',(-3.3920889732967,1.60433756714027,-2.77555756156289E-16));
#27910=CARTESIAN_POINT('Ctrl Pts',(-3.34803513046651,1.71524812390167,-2.36885885322814E-16));
#27911=CARTESIAN_POINT('Ctrl Pts',(-3.29879531544834,1.82410515487266,-4.90905898233538E-17));
#27912=CARTESIAN_POINT('Ctrl Pts',(-3.2446494755425,1.93058787890887,-2.77555756156289E-17));
#27913=CARTESIAN_POINT('Ctrl Pts',(-3.19007975249465,2.03790420773747,-6.25353928999361E-18));
#27914=CARTESIAN_POINT('Ctrl Pts',(-3.13052656738101,2.14280969706861,3.27691398306138E-16));
#27915=CARTESIAN_POINT('Ctrl Pts',(-3.06622468325314,2.24496360523417,3.33066907387547E-16));
#27916=CARTESIAN_POINT('Ctrl Pts',(-3.02442954901331,2.31136191319685,3.36560897131582E-16));
#27917=CARTESIAN_POINT('Ctrl Pts',(-2.98062715064349,2.37659746123392,-1.92345692100733E-16));
#27918=CARTESIAN_POINT('Ctrl Pts',(-2.93487136195522,2.44057147262401,-2.22044604925031E-16));
#27919=CARTESIAN_POINT('Ctrl Pts',(-2.91011088425382,2.47519063509293,-2.38115998071626E-16));
#27920=CARTESIAN_POINT('Ctrl Pts',(-2.88477824351069,2.50944029002795,-9.06967170124101E-17));
#27921=CARTESIAN_POINT('Ctrl Pts',(-2.85888104291211,2.54330410738954,-1.11022302462516E-16));
#27922=CARTESIAN_POINT('Ctrl Pts',(-2.84939469288667,2.55570869233558,-1.1846772565866E-16));
#27923=CARTESIAN_POINT('Ctrl Pts',(-2.83983467756884,2.56805870725536,-6.92597506618051E-18));
#27924=CARTESIAN_POINT('Ctrl Pts',(-2.83020669950388,2.58034686246535,0.));
#27925=CARTESIAN_POINT('Ctrl Pts',(-2.75399123609851,2.67762039564213,5.48262984856848E-17));
#27926=CARTESIAN_POINT('Ctrl Pts',(-2.67342730379929,2.77114184208896,-1.37750122974287E-16));
#27927=CARTESIAN_POINT('Ctrl Pts',(-2.58880471591903,2.86057864451344,-1.11022302462516E-16));
#27928=CARTESIAN_POINT('Ctrl Pts',(-2.5041872730583,2.95001000921607,-8.42961069915503E-17));
#27929=CARTESIAN_POINT('Ctrl Pts',(-2.41551123635495,3.03535802102991,-2.67279349305171E-16));
#27930=CARTESIAN_POINT('Ctrl Pts',(-2.3230183042847,3.11627005080055,-3.33066907387547E-16));
#27931=CARTESIAN_POINT('Ctrl Pts',(-2.23098883090374,3.19677665085427,-3.98524820655353E-16));
#27932=CARTESIAN_POINT('Ctrl Pts',(-2.13518016460462,3.27289238327565,-7.81735663884996E-17));
#27933=CARTESIAN_POINT('Ctrl Pts',(-2.0357894675403,3.34423830723631,-2.22044604925031E-16));
#27934=CARTESIAN_POINT('Ctrl Pts',(-1.93639877047599,3.41558423119697,-3.65915643461563E-16));
#27935=CARTESIAN_POINT('Ctrl Pts',(-1.83342562767619,3.48216116641753,-4.77297284244418E-18));
#27936=CARTESIAN_POINT('Ctrl Pts',(-1.72703261341869,3.54354657824449,0.));
#27937=CARTESIAN_POINT('Origin',(0.,0.,0.));
#27938=CARTESIAN_POINT('Origin',(-1.73205080756888,-3.,-8.));
#27939=CARTESIAN_POINT('',(-1.73205080756888,-3.,-8.));
#27940=CARTESIAN_POINT('',(1.73205080756888,-3.,-8.));
#27941=CARTESIAN_POINT('',(-0.86602540378444,-3.,-8.));
#27942=CARTESIAN_POINT('',(-1.73205080756888,-3.,-4.));
#27943=CARTESIAN_POINT('',(-1.73205080756888,-3.,-8.));
#27944=CARTESIAN_POINT('',(1.73205080756888,-3.,-4.));
#27945=CARTESIAN_POINT('',(-1.73205080756888,-3.,-4.));
#27946=CARTESIAN_POINT('',(1.73205080756888,-3.,-8.));
#27947=CARTESIAN_POINT('Origin',(-3.46410161513775,4.24230095489963E-16,
-8.));
#27948=CARTESIAN_POINT('',(-3.46410161513775,4.24230095489963E-16,-8.));
#27949=CARTESIAN_POINT('',(-3.03108891324554,-0.749999999999999,-8.));
#27950=CARTESIAN_POINT('',(-3.46410161513775,5.55111512312578E-16,-4.));
#27951=CARTESIAN_POINT('',(-3.46410161513775,4.24230095489963E-16,-8.));
#27952=CARTESIAN_POINT('',(-3.46410161513775,4.24230095489963E-16,-4.));
#27953=CARTESIAN_POINT('Origin',(-1.73205080756888,3.,-8.));
#27954=CARTESIAN_POINT('',(-1.73205080756888,3.,-8.));
#27955=CARTESIAN_POINT('',(-2.1650635094611,2.25,-8.));
#27956=CARTESIAN_POINT('',(-1.73205080756888,3.,-4.));
#27957=CARTESIAN_POINT('',(-1.73205080756888,3.,-8.));
#27958=CARTESIAN_POINT('',(-1.73205080756888,3.,-4.));
#27959=CARTESIAN_POINT('Origin',(1.73205080756888,3.,-8.));
#27960=CARTESIAN_POINT('',(1.73205080756888,3.,-8.));
#27961=CARTESIAN_POINT('',(0.866025403784439,3.,-8.));
#27962=CARTESIAN_POINT('',(1.73205080756888,3.,-4.));
#27963=CARTESIAN_POINT('',(1.73205080756888,3.,-8.));
#27964=CARTESIAN_POINT('',(1.73205080756888,3.,-4.));
#27965=CARTESIAN_POINT('Origin',(3.46410161513775,0.,-8.));
#27966=CARTESIAN_POINT('',(3.46410161513775,0.,-8.));
#27967=CARTESIAN_POINT('',(3.03108891324554,0.75,-8.));
#27968=CARTESIAN_POINT('',(3.46410161513775,0.,-4.));
#27969=CARTESIAN_POINT('',(3.46410161513775,0.,-8.));
#27970=CARTESIAN_POINT('',(3.46410161513775,0.,-4.));
#27971=CARTESIAN_POINT('Origin',(1.73205080756888,-3.,-8.));
#27972=CARTESIAN_POINT('',(2.1650635094611,-2.25,-8.));
#27973=CARTESIAN_POINT('',(1.73205080756888,-3.,-4.));
#27974=CARTESIAN_POINT('Origin',(0.,5.55111512312578E-16,-4.));
#27975=CARTESIAN_POINT('Origin',(0.,0.,0.));
#27976=CARTESIAN_POINT('',(-6.5,-7.9602041944578E-16,0.));
#27977=CARTESIAN_POINT('Origin',(0.,0.,0.));
#27978=CARTESIAN_POINT('Origin',(0.,0.,-8.));
#27979=CARTESIAN_POINT('',(-6.5,-7.9602041944578E-16,-8.));
#27980=CARTESIAN_POINT('',(-6.5,-7.9602041944578E-16,-8.));
#27981=CARTESIAN_POINT('Origin',(0.,0.,-8.));
#27982=CARTESIAN_POINT('Origin',(0.,0.,-8.));
#27983=CARTESIAN_POINT('Origin',(0.,0.,25.));
#27984=CARTESIAN_POINT('',(0.,0.,0.));
#27985=CARTESIAN_POINT('Origin',(0.,0.,0.));
#27986=CARTESIAN_POINT('',(-4.5,-5.51091059616309E-16,2.));
#27987=CARTESIAN_POINT('Origin',(0.,0.,2.));
#27988=CARTESIAN_POINT('',(-4.5,-5.51091059616309E-16,0.));
#27989=CARTESIAN_POINT('',(-4.5,-5.51091059616309E-16,0.));
#27990=CARTESIAN_POINT('Origin',(0.,0.,0.));
#27991=CARTESIAN_POINT('Origin',(0.,0.,0.));
#27992=CARTESIAN_POINT('',(-9.,-1.10218211923262E-15,2.));
#27993=CARTESIAN_POINT('Origin',(0.,0.,2.));
#27994=CARTESIAN_POINT('',(-9.,-1.10218211923262E-15,0.));
#27995=CARTESIAN_POINT('',(-9.,-1.10218211923262E-15,0.));
#27996=CARTESIAN_POINT('Origin',(0.,0.,0.));
#27997=CARTESIAN_POINT('Origin',(0.,0.,2.));
#27998=CARTESIAN_POINT('Origin',(0.,0.,0.));
#27999=CARTESIAN_POINT('',(-300.,-225.,494.));
#28000=CARTESIAN_POINT('',(-275.,-200.,494.));
#28001=CARTESIAN_POINT('',(-250.,-200.,466.));
#28002=CARTESIAN_POINT('',(-285.,-235.,448.));
#28003=CARTESIAN_POINT('',(-285.,-235.,448.));
#28004=CARTESIAN_POINT('',(-300.,225.,494.));
#28005=CARTESIAN_POINT('',(275.,-200.,494.));
#28006=CARTESIAN_POINT('',(250.,-200.,466.));
#28007=CARTESIAN_POINT('',(-250.,200.,466.));
#28008=CARTESIAN_POINT('',(250.,200.,466.));
#28009=CARTESIAN_POINT('',(-285.,-165.,448.));
#28010=CARTESIAN_POINT('',(-285.,-165.,448.));
#28011=CARTESIAN_POINT('',(-215.,-235.,448.));
#28012=CARTESIAN_POINT('',(-215.,-235.,448.));
#28013=CARTESIAN_POINT('',(-215.,-165.,448.));
#28014=CARTESIAN_POINT('',(-215.,-165.,448.));
#28015=CARTESIAN_POINT('',(215.,-235.,448.));
#28016=CARTESIAN_POINT('',(215.,-235.,448.));
#28017=CARTESIAN_POINT('',(215.,-165.,448.));
#28018=CARTESIAN_POINT('',(215.,-165.,448.));
#28019=CARTESIAN_POINT('',(285.,-235.,448.));
#28020=CARTESIAN_POINT('',(285.,-235.,448.));
#28021=CARTESIAN_POINT('',(285.,-165.,448.));
#28022=CARTESIAN_POINT('',(285.,-165.,448.));
#28023=CARTESIAN_POINT('',(-285.,165.,448.));
#28024=CARTESIAN_POINT('',(-285.,165.,448.));
#28025=CARTESIAN_POINT('',(-285.,235.,448.));
#28026=CARTESIAN_POINT('',(-285.,235.,448.));
#28027=CARTESIAN_POINT('',(-215.,165.,448.));
#28028=CARTESIAN_POINT('',(-215.,165.,448.));
#28029=CARTESIAN_POINT('',(-215.,235.,448.));
#28030=CARTESIAN_POINT('',(-215.,235.,448.));
#28031=CARTESIAN_POINT('',(215.,165.,448.));
#28032=CARTESIAN_POINT('',(215.,165.,448.));
#28033=CARTESIAN_POINT('',(215.,235.,448.));
#28034=CARTESIAN_POINT('',(215.,235.,448.));
#28035=CARTESIAN_POINT('',(285.,165.,448.));
#28036=CARTESIAN_POINT('',(285.,165.,448.));
#28037=CARTESIAN_POINT('',(285.,235.,448.));
#28038=CARTESIAN_POINT('',(285.,235.,448.));
#28039=CARTESIAN_POINT('',(0.,0.,0.));
#28040=CARTESIAN_POINT('',(0.,0.,0.));
#28041=CARTESIAN_POINT('Origin',(0.,0.,387.));
#28042=CARTESIAN_POINT('',(-4.51811257745934,-3.71096681342671E-5,375.387416697508));
#28043=CARTESIAN_POINT('',(-4.51738402494857,7.56118822245166E-5,375.112583302492));
#28044=CARTESIAN_POINT('',(-4.51775,5.53264807684796E-16,387.));
#28045=CARTESIAN_POINT('',(-3.43378788736318,2.93584158412846,375.));
#28046=CARTESIAN_POINT('Ctrl Pts',(-4.51738402494857,7.56118822245166E-5,
375.112583302492));
#28047=CARTESIAN_POINT('Ctrl Pts',(-4.51750331650906,0.316697913039608,
375.101431493481));
#28048=CARTESIAN_POINT('Ctrl Pts',(-4.4846735281982,0.633280120229468,375.09027968447));
#28049=CARTESIAN_POINT('Ctrl Pts',(-4.41862189351514,0.942742403897512,
375.07912787546));
#28050=CARTESIAN_POINT('Ctrl Pts',(-4.26239834514751,1.67467426709133,375.052751916973));
#28051=CARTESIAN_POINT('Ctrl Pts',(-3.92033033613571,2.36677696691102,375.026375958487));
#28052=CARTESIAN_POINT('Ctrl Pts',(-3.43378788736318,2.93584158412846,375.));
#28053=CARTESIAN_POINT('',(-4.51775,5.53264807684796E-16,375.));
#28054=CARTESIAN_POINT('Origin',(0.,0.,375.));
#28055=CARTESIAN_POINT('',(-4.51775,-5.53264807684796E-16,374.));
#28056=CARTESIAN_POINT('',(-4.51775,5.53264807684796E-16,387.));
#28057=CARTESIAN_POINT('Origin',(0.,0.,374.));
#28058=CARTESIAN_POINT('',(3.43408816985915,2.93604417002329,375.));
#28059=CARTESIAN_POINT('Origin',(0.,0.,375.));
#28060=CARTESIAN_POINT('Ctrl Pts',(3.43408816985915,2.93604417002329,375.));
#28061=CARTESIAN_POINT('Ctrl Pts',(2.97450239048794,3.47304931219374,375.024906410057));
#28062=CARTESIAN_POINT('Ctrl Pts',(2.38685944123298,3.90077491345638,375.049812820113));
#28063=CARTESIAN_POINT('Ctrl Pts',(1.73419289985632,4.17206490566361,375.07471923017));
#28064=CARTESIAN_POINT('Ctrl Pts',(1.04301719200363,4.45936177245515,375.101095188656));
#28065=CARTESIAN_POINT('Ctrl Pts',(0.278918372660684,4.57121814160633,375.127471147143));
#28066=CARTESIAN_POINT('Ctrl Pts',(-0.465602633695269,4.49408396451439,
375.153847105629));
#28067=CARTESIAN_POINT('Ctrl Pts',(-1.21012364005122,4.41694978742245,375.180223064116));
#28068=CARTESIAN_POINT('Ctrl Pts',(-1.93506683342019,4.15082506408738,375.206599022603));
#28069=CARTESIAN_POINT('Ctrl Pts',(-2.55266299064051,3.7279323762134,375.232974981089));
#28070=CARTESIAN_POINT('Ctrl Pts',(-3.17025914786083,3.30503968833942,375.259350939576));
#28071=CARTESIAN_POINT('Ctrl Pts',(-3.68050826893252,2.72537903592653,375.285726898063));
#28072=CARTESIAN_POINT('Ctrl Pts',(-4.02163754569994,2.05912619262106,375.312102856549));
#28073=CARTESIAN_POINT('Ctrl Pts',(-4.346324085653,1.4249873333691,375.337207470202));
#28074=CARTESIAN_POINT('Ctrl Pts',(-4.51780131678173,0.712402743689628,
375.362312083855));
#28075=CARTESIAN_POINT('Ctrl Pts',(-4.51811257745934,-3.71096681342671E-5,
375.387416697508));
#28076=CARTESIAN_POINT('Origin',(0.,0.,387.));
#28077=CARTESIAN_POINT('',(-4.51742232703027,-5.89235854892012E-5,376.387416697508));
#28078=CARTESIAN_POINT('',(-4.51809885152616,4.59828434581654E-5,376.112583302492));
#28079=CARTESIAN_POINT('',(-4.51775,5.53264807684796E-16,387.));
#28080=CARTESIAN_POINT('Ctrl Pts',(-4.51809885152616,4.59828434581654E-5,
376.112583302492));
#28081=CARTESIAN_POINT('Ctrl Pts',(-4.51812276106344,0.0453867389231147,
376.110985620474));
#28082=CARTESIAN_POINT('Ctrl Pts',(-4.51745435602182,0.090726788718723,
376.109387938455));
#28083=CARTESIAN_POINT('Ctrl Pts',(-4.51608913278767,0.136045847103087,
376.107790256437));
#28084=CARTESIAN_POINT('Ctrl Pts',(-4.49355081105947,0.884213247670103,
376.08141429795));
#28085=CARTESIAN_POINT('Ctrl Pts',(-4.28109923000243,1.62665957583979,376.055038339464));
#28086=CARTESIAN_POINT('Ctrl Pts',(-3.90445518421615,2.27349934356334,376.028662380977));
#28087=CARTESIAN_POINT('Ctrl Pts',(-3.52781113842983,2.92033911128693,376.002286422491));
#28088=CARTESIAN_POINT('Ctrl Pts',(-2.98697462791424,3.47157231856439,375.975910464004));
#28089=CARTESIAN_POINT('Ctrl Pts',(-2.3474228959368,3.86046307951571,375.949534505517));
#28090=CARTESIAN_POINT('Ctrl Pts',(-1.70787116395944,4.24935384046699,375.923158547031));
#28091=CARTESIAN_POINT('Ctrl Pts',(-0.969604210520236,4.47590215509218,
375.896782588544));
#28092=CARTESIAN_POINT('Ctrl Pts',(-0.222001520476049,4.51268047531198,
375.870406630058));
#28093=CARTESIAN_POINT('Ctrl Pts',(0.525601169568224,4.54945879553177,375.844030671571));
#28094=CARTESIAN_POINT('Ctrl Pts',(1.28253959621751,4.39646712134613,375.817654713084));
#28095=CARTESIAN_POINT('Ctrl Pts',(1.95717379585807,4.07222787085974,375.791278754598));
#28096=CARTESIAN_POINT('Ctrl Pts',(2.63180799549863,3.74798862037335,375.764902796111));
#28097=CARTESIAN_POINT('Ctrl Pts',(3.2241379681305,3.25250179358621,375.738526837624));
#28098=CARTESIAN_POINT('Ctrl Pts',(3.66245231025333,2.64575380780901,375.712150879138));
#28099=CARTESIAN_POINT('Ctrl Pts',(4.10076665237614,2.03900582203184,375.685774920651));
#28100=CARTESIAN_POINT('Ctrl Pts',(4.38506536398996,1.3209966772646,375.659398962165));
#28101=CARTESIAN_POINT('Ctrl Pts',(4.48092940302618,0.578654357786939,375.633023003678));
#28102=CARTESIAN_POINT('Ctrl Pts',(4.57679344206242,-0.163687961690764,
375.606647045192));
#28103=CARTESIAN_POINT('Ctrl Pts',(4.48422280852107,-0.930363455878798,
375.580271086705));
#28104=CARTESIAN_POINT('Ctrl Pts',(4.21442463026058,-1.62855553605874,375.553895128218));
#28105=CARTESIAN_POINT('Ctrl Pts',(3.9446264520001,-2.32674761623864,375.527519169732));
#28106=CARTESIAN_POINT('Ctrl Pts',(3.49760072902049,-2.95645628241037,375.501143211245));
#28107=CARTESIAN_POINT('Ctrl Pts',(2.92746753425598,-3.44144014717816,375.474767252759));
#28108=CARTESIAN_POINT('Ctrl Pts',(2.35733433949146,-3.92642401194595,375.448391294272));
#28109=CARTESIAN_POINT('Ctrl Pts',(1.66409367294202,-4.26668307530983,375.422015335785));
#28110=CARTESIAN_POINT('Ctrl Pts',(0.931673460847324,-4.42103326145621,
375.395639377299));
#28111=CARTESIAN_POINT('Ctrl Pts',(0.199253248752631,-4.57538344760259,
375.369263418812));
#28112=CARTESIAN_POINT('Ctrl Pts',(-0.572346508887337,-4.54382475653147,
375.342887460326));
#28113=CARTESIAN_POINT('Ctrl Pts',(-1.28970997066769,-4.33015694226547,
375.316511501839));
#28114=CARTESIAN_POINT('Ctrl Pts',(-2.00707343244804,-4.11648912799948,
375.290135543353));
#28115=CARTESIAN_POINT('Ctrl Pts',(-2.67020059836879,-3.72071219053859,
375.263759584866));
#28116=CARTESIAN_POINT('Ctrl Pts',(-3.19881015683584,-3.19078643170059,
375.237383626379));
#28117=CARTESIAN_POINT('Ctrl Pts',(-3.72741971530293,-2.66086067286256,
375.211007667893));
#28118=CARTESIAN_POINT('Ctrl Pts',(-4.12151166631632,-1.99678609264739,
375.184631709406));
#28119=CARTESIAN_POINT('Ctrl Pts',(-4.33336809796127,-1.27886828925581,
375.158255750919));
#28120=CARTESIAN_POINT('Ctrl Pts',(-4.45565119847602,-0.864487596482785,
375.143031601444));
#28121=CARTESIAN_POINT('Ctrl Pts',(-4.51722117132128,-0.432168630785926,
375.127807451968));
#28122=CARTESIAN_POINT('Ctrl Pts',(-4.51738402494857,7.56118822245166E-5,
375.112583302492));
#28123=CARTESIAN_POINT('Ctrl Pts',(-4.51811257745934,-3.71096681342671E-5,
375.387416697508));
#28124=CARTESIAN_POINT('Ctrl Pts',(-4.51812834028524,-0.0361164032740072,
375.388688042342));
#28125=CARTESIAN_POINT('Ctrl Pts',(-4.51770513086054,-0.072195325689107,
375.389959387175));
#28126=CARTESIAN_POINT('Ctrl Pts',(-4.51684061704284,-0.108263669884894,
375.391230732009));
#28127=CARTESIAN_POINT('Ctrl Pts',(-4.49890497915514,-0.856555654887204,
375.417606690495));
#28128=CARTESIAN_POINT('Ctrl Pts',(-4.29102427091659,-1.60029459069377,
375.443982648982));
#28129=CARTESIAN_POINT('Ctrl Pts',(-3.91836620190419,-2.24943891961304,
375.470358607469));
#28130=CARTESIAN_POINT('Ctrl Pts',(-3.54570813289175,-2.89858324853235,
375.496734565955));
#28131=CARTESIAN_POINT('Ctrl Pts',(-3.00827270310544,-3.45313297056435,
375.523110524442));
#28132=CARTESIAN_POINT('Ctrl Pts',(-2.37112526060116,-3.84595044058964,
375.549486482929));
#28133=CARTESIAN_POINT('Ctrl Pts',(-1.73397781809692,-4.2387679106149,375.575862441415));
#28134=CARTESIAN_POINT('Ctrl Pts',(-0.997118362874728,-4.46985312863346,
375.602238399902));
#28135=CARTESIAN_POINT('Ctrl Pts',(-0.249756040595646,-4.5112294783827,
375.628614358388));
#28136=CARTESIAN_POINT('Ctrl Pts',(0.497606281683436,-4.55260582813195,
375.654990316875));
#28137=CARTESIAN_POINT('Ctrl Pts',(1.25547147101941,-4.40427330961188,375.681366275361));
#28138=CARTESIAN_POINT('Ctrl Pts',(1.93208738599618,-4.08418999671804,375.707742233848));
#28139=CARTESIAN_POINT('Ctrl Pts',(2.60870330097296,-3.76410668382419,375.734118192335));
#28140=CARTESIAN_POINT('Ctrl Pts',(3.20406994159053,-3.27227257655657,375.760494150821));
#28141=CARTESIAN_POINT('Ctrl Pts',(3.64610826956487,-2.66823238495421,375.786870109308));
#28142=CARTESIAN_POINT('Ctrl Pts',(4.0881465975392,-2.06419219335185,375.813246067794));
#28143=CARTESIAN_POINT('Ctrl Pts',(4.37685661287028,-1.34794591741475,375.839622026281));
#28144=CARTESIAN_POINT('Ctrl Pts',(4.47728517843054,-0.606207059497561,
375.865997984767));
#28145=CARTESIAN_POINT('Ctrl Pts',(4.57771374399081,0.135531798419669,375.892373943254));
#28146=CARTESIAN_POINT('Ctrl Pts',(4.48986085978024,0.902763238316989,375.918749901741));
#28147=CARTESIAN_POINT('Ctrl Pts',(4.22436257375966,1.6026011428634,375.945125860228));
#28148=CARTESIAN_POINT('Ctrl Pts',(3.95886428773907,2.30243904740981,375.971501818714));
#28149=CARTESIAN_POINT('Ctrl Pts',(3.51572059990846,2.93488341660531,375.9978777772));
#28150=CARTESIAN_POINT('Ctrl Pts',(2.9485814178138,3.42336635395337,376.024253735687));
#28151=CARTESIAN_POINT('Ctrl Pts',(2.38144223571922,3.91184929130138,376.050629694174));
#28152=CARTESIAN_POINT('Ctrl Pts',(1.69030755936062,4.25637079680199,376.07700565266));
#28153=CARTESIAN_POINT('Ctrl Pts',(0.958850723376994,4.41522081720076,376.103381611147));
#28154=CARTESIAN_POINT('Ctrl Pts',(0.227393887393287,4.57407083759954,376.129757569634));
#28155=CARTESIAN_POINT('Ctrl Pts',(-0.544385108215453,4.54724937289643,
376.15613352812));
#28156=CARTESIAN_POINT('Ctrl Pts',(-1.26304959302181,4.33800360748393,376.182509486607));
#28157=CARTESIAN_POINT('Ctrl Pts',(-1.98171407782812,4.12875784207144,376.208885445093));
#28158=CARTESIAN_POINT('Ctrl Pts',(-2.64726405183205,3.73708777594958,376.23526140358));
#28159=CARTESIAN_POINT('Ctrl Pts',(-3.17912363311765,3.21041157777291,376.261637362067));
#28160=CARTESIAN_POINT('Ctrl Pts',(-3.71098321440328,2.68373537959622,376.288013320553));
#28161=CARTESIAN_POINT('Ctrl Pts',(-4.10915240297055,2.0220530493647,376.31438927904));
#28162=CARTESIAN_POINT('Ctrl Pts',(-4.32542620311525,1.30547222672582,376.340765237526));
#28163=CARTESIAN_POINT('Ctrl Pts',(-4.45293485255022,0.882997322948535,
376.356315724187));
#28164=CARTESIAN_POINT('Ctrl Pts',(-4.51721787315074,0.44144006785591,376.371866210847));
#28165=CARTESIAN_POINT('Ctrl Pts',(-4.51742232703027,-5.89235854892012E-5,
376.387416697508));
#28166=CARTESIAN_POINT('Origin',(0.,0.,387.));
#28167=CARTESIAN_POINT('',(-4.51776278108284,0.000115059314115817,377.387416697508));
#28168=CARTESIAN_POINT('',(-4.51759690135649,-0.00010734614409786,377.112583302492));
#28169=CARTESIAN_POINT('',(-4.51775,5.53264807684796E-16,387.));
#28170=CARTESIAN_POINT('Ctrl Pts',(-4.51759690135649,-0.00010734614409786,
377.112583302492));
#28171=CARTESIAN_POINT('Ctrl Pts',(-4.51713109747156,0.522789201244633,
377.094163788979));
#28172=CARTESIAN_POINT('Ctrl Pts',(-4.42639959069602,1.04584321668838,377.075744275467));
#28173=CARTESIAN_POINT('Ctrl Pts',(-4.24853722021895,1.53736821094173,377.057324761954));
#28174=CARTESIAN_POINT('Ctrl Pts',(-3.99384588448772,2.24121105862155,377.030948803468));
#28175=CARTESIAN_POINT('Ctrl Pts',(-3.56049254147675,2.88040358637871,377.004572844981));
#28176=CARTESIAN_POINT('Ctrl Pts',(-3.00094181327236,3.37756091891157,376.978196886494));
#28177=CARTESIAN_POINT('Ctrl Pts',(-2.44139108506791,3.87471825144449,376.951820928008));
#28178=CARTESIAN_POINT('Ctrl Pts',(-1.75564297167002,4.22984038875309,376.925444969521));
#28179=CARTESIAN_POINT('Ctrl Pts',(-1.02671867551292,4.39993389597404,376.899069011035));
#28180=CARTESIAN_POINT('Ctrl Pts',(-0.297794379355856,4.57002740319499,
376.872693052548));
#28181=CARTESIAN_POINT('Ctrl Pts',(0.474306099560417,4.55509228032832,376.846317094061));
#28182=CARTESIAN_POINT('Ctrl Pts',(1.19610717026038,4.35693667212173,376.819941135575));
#28183=CARTESIAN_POINT('Ctrl Pts',(1.91790824096034,4.15878106391514,376.793565177088));
#28184=CARTESIAN_POINT('Ctrl Pts',(2.58940990344398,3.77740497036863,376.767189218602));
#28185=CARTESIAN_POINT('Ctrl Pts',(3.12931572485767,3.25898030397792,376.740813260115));
#28186=CARTESIAN_POINT('Ctrl Pts',(3.66922154627136,2.74055563758721,376.714437301628));
#28187=CARTESIAN_POINT('Ctrl Pts',(4.07753152661508,2.0850823983523,376.688061343142));
#28188=CARTESIAN_POINT('Ctrl Pts',(4.30481295893208,1.37191651212926,376.661685384655));
#28189=CARTESIAN_POINT('Ctrl Pts',(4.53209439124908,0.658750625906209,376.635309426169));
#28190=CARTESIAN_POINT('Ctrl Pts',(4.57834727553935,-0.112107907304984,
376.608933467682));
#28191=CARTESIAN_POINT('Ctrl Pts',(4.4379719316997,-0.847333854561028,376.582557509196));
#28192=CARTESIAN_POINT('Ctrl Pts',(4.29759658786004,-1.58255980181707,376.556181550709));
#28193=CARTESIAN_POINT('Ctrl Pts',(3.97059301589046,-2.28215316311797,376.529805592222));
#28194=CARTESIAN_POINT('Ctrl Pts',(3.49655043114217,-2.86141653901512,376.503429633736));
#28195=CARTESIAN_POINT('Ctrl Pts',(3.02250784639385,-3.4406799149123,376.477053675249));
#28196=CARTESIAN_POINT('Ctrl Pts',(2.40142624886681,-3.89961330540572,376.450677716762));
#28197=CARTESIAN_POINT('Ctrl Pts',(1.7084978848751,-4.18265519808121,376.424301758276));
#28198=CARTESIAN_POINT('Ctrl Pts',(1.01556952088344,-4.46569709075668,376.397925799789));
#28199=CARTESIAN_POINT('Ctrl Pts',(0.250794390427128,-4.57284748561423,
376.371549841303));
#28200=CARTESIAN_POINT('Ctrl Pts',(-0.493238770703864,-4.4911340483472,
376.345173882816));
#28201=CARTESIAN_POINT('Ctrl Pts',(-1.2372719318349,-4.40942061108017,376.31879792433));
#28202=CARTESIAN_POINT('Ctrl Pts',(-1.96056312364061,-4.13884334168854,
376.292421965843));
#28203=CARTESIAN_POINT('Ctrl Pts',(-2.5755459301882,-3.71216011150867,376.266046007356));
#28204=CARTESIAN_POINT('Ctrl Pts',(-3.19052873673575,-3.28547688132881,
376.23967004887));
#28205=CARTESIAN_POINT('Ctrl Pts',(-3.69720315802519,-2.70268769036073,
376.213294090383));
#28206=CARTESIAN_POINT('Ctrl Pts',(-4.03422783747023,-2.03434885839451,
376.186918131897));
#28207=CARTESIAN_POINT('Ctrl Pts',(-4.350837779367,-1.40649359537751,376.162139855428));
#28208=CARTESIAN_POINT('Ctrl Pts',(-4.51772804111577,-0.703138866533066,
376.13736157896));
#28209=CARTESIAN_POINT('Ctrl Pts',(-4.51809885152616,4.59828434581654E-5,
376.112583302492));
#28210=CARTESIAN_POINT('Ctrl Pts',(-4.51742232703027,-5.89235854892012E-5,
376.387416697508));
#28211=CARTESIAN_POINT('Ctrl Pts',(-4.51756465760558,-0.307408461731671,
376.398242169334));
#28212=CARTESIAN_POINT('Ctrl Pts',(-4.48665292107515,-0.614729763863418,
376.40906764116));
#28213=CARTESIAN_POINT('Ctrl Pts',(-4.42439936040209,-0.915565329693696,
376.419893112986));
#28214=CARTESIAN_POINT('Ctrl Pts',(-4.27272030582208,-1.64854274842831,
376.446269071473));
#28215=CARTESIAN_POINT('Ctrl Pts',(-3.9349837849399,-2.34301827085134,376.472645029959));
#28216=CARTESIAN_POINT('Ctrl Pts',(-3.45207841488762,-2.91491409664169,
376.499020988446));
#28217=CARTESIAN_POINT('Ctrl Pts',(-2.96917304483534,-3.48680992243204,
376.525396946932));
#28218=CARTESIAN_POINT('Ctrl Pts',(-2.34109882561295,-3.93612605158971,
376.551772905419));
#28219=CARTESIAN_POINT('Ctrl Pts',(-1.64389457655484,-4.20846530156397,
376.578148863906));
#28220=CARTESIAN_POINT('Ctrl Pts',(-0.946690327496738,-4.48080455153823,
376.604524822392));
#28221=CARTESIAN_POINT('Ctrl Pts',(-0.180356048602913,-4.57616692232909,
376.630900780879));
#28222=CARTESIAN_POINT('Ctrl Pts',(0.562330763470305,-4.48300721455655,
376.657276739365));
#28223=CARTESIAN_POINT('Ctrl Pts',(1.30501757554357,-4.38984750678402,376.683652697852));
#28224=CARTESIAN_POINT('Ctrl Pts',(2.02405692079622,-4.10816572044807,376.710028656339));
#28225=CARTESIAN_POINT('Ctrl Pts',(2.6323971400614,-3.67206411576684,376.736404614825));
#28226=CARTESIAN_POINT('Ctrl Pts',(3.24073735932655,-3.23596251108564,376.762780573312));
#28227=CARTESIAN_POINT('Ctrl Pts',(3.73837845260424,-2.64544108805917,376.789156531798));
#28228=CARTESIAN_POINT('Ctrl Pts',(4.0650726975356,-1.97199227611499,376.815532490285));
#28229=CARTESIAN_POINT('Ctrl Pts',(4.39176694246694,-1.29854346417084,376.841908448771));
#28230=CARTESIAN_POINT('Ctrl Pts',(4.54751433905197,-0.542167263308996,
376.868284407258));
#28231=CARTESIAN_POINT('Ctrl Pts',(4.51345907728089,0.205564420603285,376.894660365745));
#28232=CARTESIAN_POINT('Ctrl Pts',(4.4794038155098,0.953296104515694,376.921036324231));
#28233=CARTESIAN_POINT('Ctrl Pts',(4.25554589538254,1.69238327147853,376.947412282718));
#28234=CARTESIAN_POINT('Ctrl Pts',(3.86898703740037,2.33334714042606,376.973788241204));
#28235=CARTESIAN_POINT('Ctrl Pts',(3.48242817941824,2.97431100937351,377.000164199691));
#28236=CARTESIAN_POINT('Ctrl Pts',(2.93316838358124,3.51715158030568,377.026540158178));
#28237=CARTESIAN_POINT('Ctrl Pts',(2.28770467380867,3.89614898312949,377.052916116664));
#28238=CARTESIAN_POINT('Ctrl Pts',(1.6422409640361,4.27514638595329,377.079292075151));
#28239=CARTESIAN_POINT('Ctrl Pts',(0.900573340327957,4.49030062066872,377.105668033637));
#28240=CARTESIAN_POINT('Ctrl Pts',(0.152492990912077,4.51556369250058,377.132043992124));
#28241=CARTESIAN_POINT('Ctrl Pts',(-0.595587358503804,4.54082676433243,
377.158419950611));
#28242=CARTESIAN_POINT('Ctrl Pts',(-1.35008043362742,4.3761986732807,377.184795909097));
#28243=CARTESIAN_POINT('Ctrl Pts',(-2.01964231224972,4.04161038496754,377.211171867584));
#28244=CARTESIAN_POINT('Ctrl Pts',(-2.68920419087202,3.70702209665437,377.23754782607));
#28245=CARTESIAN_POINT('Ctrl Pts',(-3.27383487299299,3.20247361107977,377.263923784557));
#28246=CARTESIAN_POINT('Ctrl Pts',(-3.70275510124179,2.58904890520336,377.290299743043));
#28247=CARTESIAN_POINT('Ctrl Pts',(-4.13167532949061,1.97562419932691,377.31667570153));
#28248=CARTESIAN_POINT('Ctrl Pts',(-4.40488510386723,1.25332327314864,377.343051660017));
#28249=CARTESIAN_POINT('Ctrl Pts',(-4.48930784196123,0.509592654393879,
377.369427618503));
#28250=CARTESIAN_POINT('Ctrl Pts',(-4.50850066492699,0.340511546362542,
377.375423978172));
#28251=CARTESIAN_POINT('Ctrl Pts',(-4.51793615737842,0.170322859138234,
377.38142033784));
#28252=CARTESIAN_POINT('Ctrl Pts',(-4.51776278108284,0.000115059314115817,
377.387416697508));
#28253=CARTESIAN_POINT('Origin',(0.,0.,387.));
#28254=CARTESIAN_POINT('',(-4.51797310231548,-9.04168125550817E-5,378.387416697508));
#28255=CARTESIAN_POINT('',(-4.51753028950122,9.61292306860575E-5,378.112583302492));
#28256=CARTESIAN_POINT('',(-4.51775,5.53264807684796E-16,387.));
#28257=CARTESIAN_POINT('Ctrl Pts',(-4.51753028950122,9.61292306860575E-5,
378.112583302492));
#28258=CARTESIAN_POINT('Ctrl Pts',(-4.51772668562278,0.251779003793691,
378.103717915972));
#28259=CARTESIAN_POINT('Ctrl Pts',(-4.49704602585537,0.503429942291254,
378.094852529451));
#28260=CARTESIAN_POINT('Ctrl Pts',(-4.4551993669653,0.751510564258943,378.085987142931));
#28261=CARTESIAN_POINT('Ctrl Pts',(-4.33069878989798,1.48959053081815,378.059611184445));
#28262=CARTESIAN_POINT('Ctrl Pts',(-4.01884552637064,2.19606752935734,378.033235225958));
#28263=CARTESIAN_POINT('Ctrl Pts',(-3.55739459519457,2.78541078149727,378.006859267472));
#28264=CARTESIAN_POINT('Ctrl Pts',(-3.09594366401851,3.3747540336372,377.980483308985));
#28265=CARTESIAN_POINT('Ctrl Pts',(-2.48489506519372,3.84696353937788,377.954107350499));
#28266=CARTESIAN_POINT('Ctrl Pts',(-1.79822638382644,4.14487049256201,377.927731392012));
#28267=CARTESIAN_POINT('Ctrl Pts',(-1.11155770245912,4.44277744574616,377.901355433525));
#28268=CARTESIAN_POINT('Ctrl Pts',(-0.349268938549303,4.56638184637374,
377.874979475039));
#28269=CARTESIAN_POINT('Ctrl Pts',(0.396352188045507,4.50071932813326,377.848603516552));
#28270=CARTESIAN_POINT('Ctrl Pts',(1.14197331464023,4.43505680989279,377.822227558065));
#28271=CARTESIAN_POINT('Ctrl Pts',(1.87092680391995,4.18012737278432,377.795851599579));
#28272=CARTESIAN_POINT('Ctrl Pts',(2.49496072486742,3.76679446067473,377.769475641092));
#28273=CARTESIAN_POINT('Ctrl Pts',(3.11899464581496,3.35346154856509,377.743099682606));
#28274=CARTESIAN_POINT('Ctrl Pts',(3.63810899843023,2.7817251614543,377.716723724119));
#28275=CARTESIAN_POINT('Ctrl Pts',(3.98945636554489,2.120803488071,377.690347765632));
#28276=CARTESIAN_POINT('Ctrl Pts',(4.34080373265956,1.45988181468769,377.663971807146));
#28277=CARTESIAN_POINT('Ctrl Pts',(4.52438411427362,0.709774855031875,377.637595848659));
#28278=CARTESIAN_POINT('Ctrl Pts',(4.517972055111,-0.0387044808375217,377.611219890173));
#28279=CARTESIAN_POINT('Ctrl Pts',(4.51155999594838,-0.787183816706875,
377.584843931686));
#28280=CARTESIAN_POINT('Ctrl Pts',(4.3151554960091,-1.53403552878981,377.558467973199));
#28281=CARTESIAN_POINT('Ctrl Pts',(3.9525365831578,-2.18884080883012,377.532092014713));
#28282=CARTESIAN_POINT('Ctrl Pts',(3.5899176703065,-2.84364608887043,377.505716056226));
#28283=CARTESIAN_POINT('Ctrl Pts',(3.06108434454318,-3.40640493686811,377.47934009774));
#28284=CARTESIAN_POINT('Ctrl Pts',(2.43006066621085,-3.80898604436084,377.452964139253));
#28285=CARTESIAN_POINT('Ctrl Pts',(1.79903698787851,-4.21156715185356,377.426588180766));
#28286=CARTESIAN_POINT('Ctrl Pts',(1.06582295697716,-4.45397051884133,377.40021222228));
#28287=CARTESIAN_POINT('Ctrl Pts',(0.319186313873781,-4.50684919035867,
377.373836263793));
#28288=CARTESIAN_POINT('Ctrl Pts',(-0.427450329229602,-4.55972786187601,
377.347460305307));
#28289=CARTESIAN_POINT('Ctrl Pts',(-1.18750958453502,-4.42308183792293,
377.32108434682));
#28290=CARTESIAN_POINT('Ctrl Pts',(-1.86897365124353,-4.11345438999364,
377.294708388334));
#28291=CARTESIAN_POINT('Ctrl Pts',(-2.55043771795204,-3.80382694206434,
377.268332429847));
#28292=CARTESIAN_POINT('Ctrl Pts',(-3.15330659606364,-3.32121807015883,
377.24195647136));
#28293=CARTESIAN_POINT('Ctrl Pts',(-3.60459299156575,-2.72405559648777,
377.215580512874));
#28294=CARTESIAN_POINT('Ctrl Pts',(-4.05587938706785,-2.1268931228167,377.189204554387));
#28295=CARTESIAN_POINT('Ctrl Pts',(-4.35558329996046,-1.41517704738009,
377.162828595901));
#28296=CARTESIAN_POINT('Ctrl Pts',(-4.46742059218106,-0.675072425860511,
377.136452637414));
#28297=CARTESIAN_POINT('Ctrl Pts',(-4.50115689268563,-0.451816019874252,
377.12849619244));
#28298=CARTESIAN_POINT('Ctrl Pts',(-4.51779810878667,-0.225976373769842,
377.120539747466));
#28299=CARTESIAN_POINT('Ctrl Pts',(-4.51759690135649,-0.00010734614409786,
377.112583302492));
#28300=CARTESIAN_POINT('Ctrl Pts',(-4.51776278108284,0.000115059314115817,
377.387416697508));
#28301=CARTESIAN_POINT('Ctrl Pts',(-4.51717353368206,-0.578363695817441,
377.407796296326));
#28302=CARTESIAN_POINT('Ctrl Pts',(-4.40559318176197,-1.15706321872293,
377.428175895145));
#28303=CARTESIAN_POINT('Ctrl Pts',(-4.18884997964351,-1.69325291121775,
377.448555493963));
#28304=CARTESIAN_POINT('Ctrl Pts',(-3.90833367742039,-2.38720754674346,
377.47493145245));
#28305=CARTESIAN_POINT('Ctrl Pts',(-3.45166537116277,-3.0099565064637,377.501307410936));
#28306=CARTESIAN_POINT('Ctrl Pts',(-2.87413234662247,-3.48610568219112,
377.527683369423));
#28307=CARTESIAN_POINT('Ctrl Pts',(-2.29659932208215,-3.96225485791856,
377.55405932791));
#28308=CARTESIAN_POINT('Ctrl Pts',(-1.59820157925914,-4.29180424965317,
377.580435286396));
#28309=CARTESIAN_POINT('Ctrl Pts',(-0.863491768396101,-4.43485642825323,
377.606811244883));
#28310=CARTESIAN_POINT('Ctrl Pts',(-0.128781957533104,-4.57790860685328,
377.633187203369));
#28311=CARTESIAN_POINT('Ctrl Pts',(0.642239921369918,-4.5344635723188,377.659563161856));
#28312=CARTESIAN_POINT('Ctrl Pts',(1.35622885978989,-4.30978106789426,377.685939120342));
#28313=CARTESIAN_POINT('Ctrl Pts',(2.07021779820986,-4.08509856346973,377.712315078829));
#28314=CARTESIAN_POINT('Ctrl Pts',(2.72717379614679,-3.67917858915515,377.738691037316));
#28315=CARTESIAN_POINT('Ctrl Pts',(3.24756141510707,-3.14116450196653,377.765066995802));
#28316=CARTESIAN_POINT('Ctrl Pts',(3.76794903406735,-2.6031504147779,377.791442954289));
#28317=CARTESIAN_POINT('Ctrl Pts',(4.15176827405098,-1.93304221471522,377.817818912776));
#28318=CARTESIAN_POINT('Ctrl Pts',(4.35255143912362,-1.21196763285564,377.844194871262));
#28319=CARTESIAN_POINT('Ctrl Pts',(4.55333460419626,-0.49089305099606,377.870570829749));
#28320=CARTESIAN_POINT('Ctrl Pts',(4.57108169435792,0.28114791266043,377.896946788235));
#28321=CARTESIAN_POINT('Ctrl Pts',(4.40364412948689,1.01068687244984,377.923322746722));
#28322=CARTESIAN_POINT('Ctrl Pts',(4.23620656461585,1.7402258322393,377.949698705208));
#28323=CARTESIAN_POINT('Ctrl Pts',(3.88358434471212,2.42726278816168,377.976074663695));
#28324=CARTESIAN_POINT('Ctrl Pts',(3.38846824810894,2.98862050198153,378.002450622182));
#28325=CARTESIAN_POINT('Ctrl Pts',(2.89335215150579,3.54997821580136,378.028826580668));
#28326=CARTESIAN_POINT('Ctrl Pts',(2.25574217820322,3.98565668751868,378.055202539155));
#28327=CARTESIAN_POINT('Ctrl Pts',(1.55283160898984,4.2429097995867,378.081578497641));
#28328=CARTESIAN_POINT('Ctrl Pts',(0.849921039776497,4.5001629116547,378.107954456128));
#28329=CARTESIAN_POINT('Ctrl Pts',(0.0817098746523573,4.57899066407343,
378.134330414615));
#28330=CARTESIAN_POINT('Ctrl Pts',(-0.658797161460833,4.46984964773514,
378.160706373101));
#28331=CARTESIAN_POINT('Ctrl Pts',(-1.39930419757415,4.36070863139684,378.187082331588));
#28332=CARTESIAN_POINT('Ctrl Pts',(-2.11210710467651,4.06359884630146,378.213458290074));
#28333=CARTESIAN_POINT('Ctrl Pts',(-2.71090924805577,3.61449036824177,378.239834248561));
#28334=CARTESIAN_POINT('Ctrl Pts',(-3.309711391435,3.16538189018211,378.266210207048));
#28335=CARTESIAN_POINT('Ctrl Pts',(-3.79451277109115,2.56427471915816,378.292586165534));
#28336=CARTESIAN_POINT('Ctrl Pts',(-4.10662012532275,1.8839428652698,378.318962124021));
#28337=CARTESIAN_POINT('Ctrl Pts',(-4.37662833282249,1.29537876422316,378.341780315183));
#28338=CARTESIAN_POINT('Ctrl Pts',(-4.5173887163544,0.647521251956349,378.364598506346));
#28339=CARTESIAN_POINT('Ctrl Pts',(-4.51797310231548,-9.04168125550817E-5,
378.387416697508));
#28340=CARTESIAN_POINT('Origin',(0.,0.,387.));
#28341=CARTESIAN_POINT('',(-4.51737365644452,-1.98811769755447E-6,379.387416697508));
#28342=CARTESIAN_POINT('',(-4.51813007169143,-2.03714566067892E-5,379.112583302492));
#28343=CARTESIAN_POINT('',(-4.51775,5.53264807684796E-16,387.));
#28344=CARTESIAN_POINT('Ctrl Pts',(-4.51813007169143,-2.03714566067892E-5,
379.112583302492));
#28345=CARTESIAN_POINT('Ctrl Pts',(-4.517945231463,0.728944748987095,379.086896084477));
#28346=CARTESIAN_POINT('Ctrl Pts',(-4.33810981632971,1.45799779441603,379.061208866463));
#28347=CARTESIAN_POINT('Ctrl Pts',(-3.99878265125311,2.10316590777759,379.035521648449));
#28348=CARTESIAN_POINT('Ctrl Pts',(-3.65035725094643,2.76563263988363,379.009145689962));
#28349=CARTESIAN_POINT('Ctrl Pts',(-3.13377267064052,3.33965579170571,378.982769731476));
#28350=CARTESIAN_POINT('Ctrl Pts',(-2.51157005653494,3.75574032365363,378.956393772989));
#28351=CARTESIAN_POINT('Ctrl Pts',(-1.88936744242933,4.17182485560157,378.930017814502));
#28352=CARTESIAN_POINT('Ctrl Pts',(-1.16154679452404,4.42997076767533,378.903641856016));
#28353=CARTESIAN_POINT('Ctrl Pts',(-0.416222894566461,4.49892520827358,
378.877265897529));
#28354=CARTESIAN_POINT('Ctrl Pts',(0.329101005391076,4.56787964887184,378.850889939042));
#28355=CARTESIAN_POINT('Ctrl Pts',(1.0919281574009,4.44764261799461,378.824513980556));
#28356=CARTESIAN_POINT('Ctrl Pts',(1.779905660781,4.15277080589822,378.798138022069));
#28357=CARTESIAN_POINT('Ctrl Pts',(2.46788316416111,3.85789899380182,378.771762063583));
#28358=CARTESIAN_POINT('Ctrl Pts',(3.08101101891148,3.38839240048625,378.745386105096));
#28359=CARTESIAN_POINT('Ctrl Pts',(3.54505991145048,2.80109259965241,378.71901014661));
#28360=CARTESIAN_POINT('Ctrl Pts',(4.00910880398948,2.21379279881858,378.692634188123));
#28361=CARTESIAN_POINT('Ctrl Pts',(4.3240787343171,1.50869979046648,378.666258229636));
#28362=CARTESIAN_POINT('Ctrl Pts',(4.45183735932425,0.771176797969019,378.63988227115));
#28363=CARTESIAN_POINT('Ctrl Pts',(4.57959598433139,0.0336538054715552,
378.613506312663));
#28364=CARTESIAN_POINT('Ctrl Pts',(4.52014330401807,-0.736299171171277,
378.587130354177));
#28365=CARTESIAN_POINT('Ctrl Pts',(4.28067705310806,-1.44546653181419,378.56075439569));
#28366=CARTESIAN_POINT('Ctrl Pts',(4.04121080219804,-2.1546338924571,378.534378437203));
#28367=CARTESIAN_POINT('Ctrl Pts',(3.62173098069132,-2.80301563710009,378.508002478717));
#28368=CARTESIAN_POINT('Ctrl Pts',(3.07302259039553,-3.31211438306704,378.48162652023));
#28369=CARTESIAN_POINT('Ctrl Pts',(2.5243142000997,-3.82121312903403,378.455250561744));
#28370=CARTESIAN_POINT('Ctrl Pts',(1.84637724101477,-4.19102887632496,378.428874603257));
#28371=CARTESIAN_POINT('Ctrl Pts',(1.12128724556784,-4.37678928445587,378.40249864477));
#28372=CARTESIAN_POINT('Ctrl Pts',(0.396197250120947,-4.56254969258676,
378.376122686284));
#28373=CARTESIAN_POINT('Ctrl Pts',(-0.37604578168795,-4.56425476155764,
378.349746727797));
#28374=CARTESIAN_POINT('Ctrl Pts',(-1.10194900048777,-4.38169806444086,
378.323370769311));
#28375=CARTESIAN_POINT('Ctrl Pts',(-1.82785221928764,-4.19914136732407,
378.296994810824));
#28376=CARTESIAN_POINT('Ctrl Pts',(-2.50741562507842,-3.83232290411959,
378.270618852338));
#28377=CARTESIAN_POINT('Ctrl Pts',(-3.05836677703682,-3.32565214427459,
378.244242893851));
#28378=CARTESIAN_POINT('Ctrl Pts',(-3.60931792899519,-2.81898138442963,
378.217866935364));
#28379=CARTESIAN_POINT('Ctrl Pts',(-4.0316568271212,-2.17245832794416,378.191490976878));
#28380=CARTESIAN_POINT('Ctrl Pts',(-4.27425233088056,-1.46435533241182,
378.165115018391));
#28381=CARTESIAN_POINT('Ctrl Pts',(-4.435307559621,-0.99425721373283,378.147604446425));
#28382=CARTESIAN_POINT('Ctrl Pts',(-4.51714237540265,-0.497018246743604,
378.130093874458));
#28383=CARTESIAN_POINT('Ctrl Pts',(-4.51753028950122,9.61292306860575E-5,
378.112583302492));
#28384=CARTESIAN_POINT('Ctrl Pts',(-4.51797310231548,-9.04168125550817E-5,
378.387416697508));
#28385=CARTESIAN_POINT('Ctrl Pts',(-4.51806421862098,-0.101064749856769,
378.390974464832));
#28386=CARTESIAN_POINT('Ctrl Pts',(-4.51474759603089,-0.202033106339626,
378.394532232156));
#28387=CARTESIAN_POINT('Ctrl Pts',(-4.50798181202017,-0.302769806622464,
378.398089999481));
#28388=CARTESIAN_POINT('Ctrl Pts',(-4.45782281567894,-1.04959408787382,
378.424465957967));
#28389=CARTESIAN_POINT('Ctrl Pts',(-4.2180914941894,-1.78368611362381,378.450841916454));
#28390=CARTESIAN_POINT('Ctrl Pts',(-3.81781130701489,-2.41617184764166,
378.47721787494));
#28391=CARTESIAN_POINT('Ctrl Pts',(-3.41753111984037,-3.04865758165951,
378.503593833427));
#28392=CARTESIAN_POINT('Ctrl Pts',(-2.85670206698089,-3.57953702394521,
378.529969791913));
#28393=CARTESIAN_POINT('Ctrl Pts',(-2.20322182313489,-3.94453839775569,
378.5563457504));
#28394=CARTESIAN_POINT('Ctrl Pts',(-1.54974157928885,-4.30953977156619,
378.582721708887));
#28395=CARTESIAN_POINT('Ctrl Pts',(-0.803610144456304,-4.50866307690144,
378.609097667373));
#28396=CARTESIAN_POINT('Ctrl Pts',(-0.0551591253652737,-4.51780112933225,
378.63547362586));
#28397=CARTESIAN_POINT('Ctrl Pts',(0.693291893725671,-4.52693918176306,
378.661849584346));
#28398=CARTESIAN_POINT('Ctrl Pts',(1.44406249707508,-4.34609198128947,378.688225542833));
#28399=CARTESIAN_POINT('Ctrl Pts',(2.10625942952888,-3.99715408620027,378.71460150132));
#28400=CARTESIAN_POINT('Ctrl Pts',(2.76845636198275,-3.64821619111103,378.740977459806));
#28401=CARTESIAN_POINT('Ctrl Pts',(3.34207962354098,-3.13118760140616,378.767353418293));
#28402=CARTESIAN_POINT('Ctrl Pts',(3.75768258797375,-2.50866321799992,378.793729376779));
#28403=CARTESIAN_POINT('Ctrl Pts',(4.1732855524065,-1.88613883459371,378.820105335266));
#28404=CARTESIAN_POINT('Ctrl Pts',(4.43086821971381,-1.15811865748618,378.846481293753));
#28405=CARTESIAN_POINT('Ctrl Pts',(4.49924592843132,-0.412741624749648,
378.872857252239));
#28406=CARTESIAN_POINT('Ctrl Pts',(4.56762363714884,0.332635407986881,378.899233210726));
#28407=CARTESIAN_POINT('Ctrl Pts',(4.44679638727653,1.09536929635249,378.925609169213));
#28408=CARTESIAN_POINT('Ctrl Pts',(4.15139232488624,1.78311843077862,378.951985127699));
#28409=CARTESIAN_POINT('Ctrl Pts',(3.85598826249595,2.47086756520474,378.978361086186));
#28410=CARTESIAN_POINT('Ctrl Pts',(3.38600738758769,3.08363194569147,379.004737044672));
#28411=CARTESIAN_POINT('Ctrl Pts',(2.79834869352904,3.54722626325572,379.031113003159));
#28412=CARTESIAN_POINT('Ctrl Pts',(2.2106899994704,4.01082058081996,379.057488961645));
#28413=CARTESIAN_POINT('Ctrl Pts',(1.5053534862614,4.32524483546169,379.083864920132));
#28414=CARTESIAN_POINT('Ctrl Pts',(0.767731857583539,4.4524327471797,379.110240878618));
#28415=CARTESIAN_POINT('Ctrl Pts',(0.030110228905678,4.5796206588977,379.136616837105));
#28416=CARTESIAN_POINT('Ctrl Pts',(-0.739796515241018,4.51957222769198,
379.162992795591));
#28417=CARTESIAN_POINT('Ctrl Pts',(-1.44877837192307,4.27955731382987,379.189368754078));
#28418=CARTESIAN_POINT('Ctrl Pts',(-2.15776022860516,4.03954239996775,379.215744712565));
#28419=CARTESIAN_POINT('Ctrl Pts',(-2.80581719782259,3.61956100344924,379.242120671052));
#28420=CARTESIAN_POINT('Ctrl Pts',(-3.31449121636045,3.0704588500705,379.268496629538));
#28421=CARTESIAN_POINT('Ctrl Pts',(-3.82316523489829,2.52135669669179,379.294872588025));
#28422=CARTESIAN_POINT('Ctrl Pts',(-4.19245630275656,1.84313378645288,379.321248546511));
#28423=CARTESIAN_POINT('Ctrl Pts',(-4.37765560061389,1.11790027091894,379.347624504998));
#28424=CARTESIAN_POINT('Ctrl Pts',(-4.4707894813135,0.753191481541508,379.360888569168));
#28425=CARTESIAN_POINT('Ctrl Pts',(-4.51736785070585,0.376594041376692,
379.374152633338));
#28426=CARTESIAN_POINT('Ctrl Pts',(-4.51737365644452,-1.98811769755447E-6,
379.387416697508));
#28427=CARTESIAN_POINT('Origin',(0.,0.,387.));
#28428=CARTESIAN_POINT('',(-4.51796103056296,9.30366574888874E-5,380.387416697508));
#28429=CARTESIAN_POINT('',(-4.51744861143269,-7.15418913582019E-5,380.112583302492));
#28430=CARTESIAN_POINT('',(-4.51775,5.53264807684796E-16,387.));
#28431=CARTESIAN_POINT('Ctrl Pts',(-4.51744861143269,-7.15418913582019E-5,
380.112583302492));
#28432=CARTESIAN_POINT('Ctrl Pts',(-4.51718913038702,0.45796072853139,380.09645021147));
#28433=CARTESIAN_POINT('Ctrl Pts',(-4.44792028854276,0.916069730534027,
380.080317120448));
#28434=CARTESIAN_POINT('Ctrl Pts',(-4.31082918580142,1.35289366117352,380.064184029426));
#28435=CARTESIAN_POINT('Ctrl Pts',(-4.08669921406521,2.0670562382494,380.037808070939));
#28436=CARTESIAN_POINT('Ctrl Pts',(-3.68128769636301,2.72432612859277,380.011432112453));
#28437=CARTESIAN_POINT('Ctrl Pts',(-3.14367643259018,3.24512989181911,379.985056153966));
#28438=CARTESIAN_POINT('Ctrl Pts',(-2.60606516881736,3.76593365504543,379.958680195479));
#28439=CARTESIAN_POINT('Ctrl Pts',(-1.93625415897387,4.15027129115475,379.932304236993));
#28440=CARTESIAN_POINT('Ctrl Pts',(-1.21533515432327,4.35161234374879,379.905928278506));
#28441=CARTESIAN_POINT('Ctrl Pts',(-0.494416149672638,4.55295339634284,
379.87955232002));
#28442=CARTESIAN_POINT('Ctrl Pts',(0.27761084978516,4.57129786542164,379.853176361533));
#28443=CARTESIAN_POINT('Ctrl Pts',(1.0072791489844,4.40442484822049,379.826800403046));
#28444=CARTESIAN_POINT('Ctrl Pts',(1.73694744818368,4.23755183101932,379.80042444456));
#28445=CARTESIAN_POINT('Ctrl Pts',(2.4242570471244,3.88546132753817,379.774048486073));
#28446=CARTESIAN_POINT('Ctrl Pts',(2.98599769960395,3.39077974300318,379.747672527587));
#28447=CARTESIAN_POINT('Ctrl Pts',(3.5477383520835,2.89609815846819,379.7212965691));
#28448=CARTESIAN_POINT('Ctrl Pts',(3.98391005810188,2.25882549287937,379.694920610614));
#28449=CARTESIAN_POINT('Ctrl Pts',(4.24170698590533,1.55611419032241,379.668544652127));
#28450=CARTESIAN_POINT('Ctrl Pts',(4.49950391370875,0.853402887765529,379.64216869364));
#28451=CARTESIAN_POINT('Ctrl Pts',(4.57892606329728,0.0852529482405344,
379.615792735154));
#28452=CARTESIAN_POINT('Ctrl Pts',(4.47035806391024,-0.655338315706838,
379.589416776667));
#28453=CARTESIAN_POINT('Ctrl Pts',(4.36179006452319,-1.39592957965429,379.56304081818));
#28454=CARTESIAN_POINT('Ctrl Pts',(4.06523191616051,-2.10896216802411,379.536664859694));
#28455=CARTESIAN_POINT('Ctrl Pts',(3.61658690982335,-2.70811163937072,379.510288901207));
#28456=CARTESIAN_POINT('Ctrl Pts',(3.16794190348622,-3.30726111071731,379.483912942721));
#28457=CARTESIAN_POINT('Ctrl Pts',(2.56721003917463,-3.79252746504069,379.457536984234));
#28458=CARTESIAN_POINT('Ctrl Pts',(1.88711988987541,-4.10516114773068,379.431161025748));
#28459=CARTESIAN_POINT('Ctrl Pts',(1.20702974057619,-4.41779483042066,379.404785067261));
#28460=CARTESIAN_POINT('Ctrl Pts',(0.447581306289357,-4.55779584147724,
379.378409108774));
#28461=CARTESIAN_POINT('Ctrl Pts',(-0.299281562218895,-4.50821473247633,
379.352033150288));
#28462=CARTESIAN_POINT('Ctrl Pts',(-1.04614443072715,-4.45863362347542,
379.325657191801));
#28463=CARTESIAN_POINT('Ctrl Pts',(-1.7804217334568,-4.21947039441701,379.299281233315));
#28464=CARTESIAN_POINT('Ctrl Pts',(-2.41321700332044,-3.81967972773712,
379.272905274828));
#28465=CARTESIAN_POINT('Ctrl Pts',(-3.04601227318407,-3.41988906105724,
379.246529316342));
#28466=CARTESIAN_POINT('Ctrl Pts',(-3.57732551018167,-2.85947095675588,
379.220153357855));
#28467=CARTESIAN_POINT('Ctrl Pts',(-3.94283241951303,-2.20627333738088,
379.193777399368));
#28468=CARTESIAN_POINT('Ctrl Pts',(-4.30833932884442,-1.55307571800585,
379.167401440882));
#28469=CARTESIAN_POINT('Ctrl Pts',(-4.50803991050956,-0.807098583557167,
379.141025482395));
#28470=CARTESIAN_POINT('Ctrl Pts',(-4.51775709118839,-0.0586548601377958,
379.114649523908));
#28471=CARTESIAN_POINT('Ctrl Pts',(-4.51801083042644,-0.0391111728918336,
379.113960783436));
#28472=CARTESIAN_POINT('Ctrl Pts',(-4.51813502773401,-0.0195658037794806,
379.113272042964));
#28473=CARTESIAN_POINT('Ctrl Pts',(-4.51813007169143,-2.03714566067892E-5,
379.112583302492));
#28474=CARTESIAN_POINT('Ctrl Pts',(-4.51737365644452,-1.98811769755447E-6,
379.387416697508));
#28475=CARTESIAN_POINT('Ctrl Pts',(-4.51737939557777,-0.372277579931259,
379.400528591825));
#28476=CARTESIAN_POINT('Ctrl Pts',(-4.47187503399554,-0.744551793256104,
379.413640486141));
#28477=CARTESIAN_POINT('Ctrl Pts',(-4.38084409953505,-1.10533911035289,
379.426752380458));
#28478=CARTESIAN_POINT('Ctrl Pts',(-4.19772577274251,-1.83110085526187,
379.453128338944));
#28479=CARTESIAN_POINT('Ctrl Pts',(-3.83038159130104,-2.51038022425081,
379.479504297431));
#28480=CARTESIAN_POINT('Ctrl Pts',(-3.32328467158491,-3.06093916387039,
379.505880255917));
#28481=CARTESIAN_POINT('Ctrl Pts',(-2.81618775186881,-3.61149810348995,
379.532256214404));
#28482=CARTESIAN_POINT('Ctrl Pts',(-2.16933809387807,-4.03333661374015,
379.558632172891));
#28483=CARTESIAN_POINT('Ctrl Pts',(-1.46104759574481,-4.27538413435274,
379.585008131377));
#28484=CARTESIAN_POINT('Ctrl Pts',(-0.752757097611556,-4.51743165496533,
379.611384089864));
#28485=CARTESIAN_POINT('Ctrl Pts',(0.0169742406642152,-4.57968818594031,
379.63776004835));
#28486=CARTESIAN_POINT('Ctrl Pts',(0.75495765194394,-4.45461653984696,379.664136006837));
#28487=CARTESIAN_POINT('Ctrl Pts',(1.49294106322366,-4.32954489375361,379.690511965324));
#28488=CARTESIAN_POINT('Ctrl Pts',(2.19917654750734,-4.01714507059193,379.71688792381));
#28489=CARTESIAN_POINT('Ctrl Pts',(2.78816256572898,-3.55523825929773,379.743263882297));
#28490=CARTESIAN_POINT('Ctrl Pts',(3.37714858395063,-3.09333144800353,379.769639840783));
#28491=CARTESIAN_POINT('Ctrl Pts',(3.84888513611024,-2.48191764857682,379.79601579927));
#28492=CARTESIAN_POINT('Ctrl Pts',(4.14626067493935,-1.79501865972427,379.822391757756));
#28493=CARTESIAN_POINT('Ctrl Pts',(4.44363621376846,-1.10811967087172,379.848767716243));
#28494=CARTESIAN_POINT('Ctrl Pts',(4.56665073926708,-0.34573549259334,379.87514367473));
#28495=CARTESIAN_POINT('Ctrl Pts',(4.50041129930853,0.399834603758797,379.901519633216));
#28496=CARTESIAN_POINT('Ctrl Pts',(4.43417185934997,1.14540470011094,379.927895591703));
#28497=CARTESIAN_POINT('Ctrl Pts',(4.17867845393423,1.87416071453683,379.954271550189));
#28498=CARTESIAN_POINT('Ctrl Pts',(3.76486280466181,2.49787462363122,379.980647508676));
#28499=CARTESIAN_POINT('Ctrl Pts',(3.35104715538937,3.12158853272565,380.007023467163));
#28500=CARTESIAN_POINT('Ctrl Pts',(2.77890926226022,3.64026033648856,380.033399425649));
#28501=CARTESIAN_POINT('Ctrl Pts',(2.11771592297733,3.99109619564288,380.059775384136));
#28502=CARTESIAN_POINT('Ctrl Pts',(1.45652258369447,4.34193205479719,380.086151342622));
#28503=CARTESIAN_POINT('Ctrl Pts',(0.706273798257865,4.52493196934294,380.112527301109));
#28504=CARTESIAN_POINT('Ctrl Pts',(-0.0422003529064303,4.5179407591868,
380.138903259596));
#28505=CARTESIAN_POINT('Ctrl Pts',(-0.790674504070726,4.51094954903066,
380.165279218082));
#28506=CARTESIAN_POINT('Ctrl Pts',(-1.53737402096271,4.31396721417262,380.191655176569));
#28507=CARTESIAN_POINT('Ctrl Pts',(-2.19189852108271,3.95084173899465,380.218031135055));
#28508=CARTESIAN_POINT('Ctrl Pts',(-2.84642302120274,3.58771626381665,380.244407093542));
#28509=CARTESIAN_POINT('Ctrl Pts',(-3.40877250455077,3.05844764831869,380.270783052029));
#28510=CARTESIAN_POINT('Ctrl Pts',(-3.81086522305661,2.42711265189824,380.297159010515));
#28511=CARTESIAN_POINT('Ctrl Pts',(-4.21295794156245,1.7957776554778,380.323534969002));
#28512=CARTESIAN_POINT('Ctrl Pts',(-4.4547938952261,1.06237627813486,380.349910927489));
#28513=CARTESIAN_POINT('Ctrl Pts',(-4.50709482389231,0.315698941635839,
380.376286885975));
#28514=CARTESIAN_POINT('Ctrl Pts',(-4.51445126403015,0.210674283980221,
380.379996823153));
#28515=CARTESIAN_POINT('Ctrl Pts',(-4.51805792159162,0.105386973232761,
380.38370676033));
#28516=CARTESIAN_POINT('Ctrl Pts',(-4.51796103056296,9.30366574888874E-5,
380.387416697508));
#28517=CARTESIAN_POINT('Origin',(0.,0.,387.));
#28518=CARTESIAN_POINT('',(-4.51777632728029,-0.000114640610663838,381.387416697508));
#28519=CARTESIAN_POINT('',(-4.51771140424386,0.000115276608145368,381.112583302492));
#28520=CARTESIAN_POINT('',(-4.51775,5.53264807684796E-16,387.));
#28521=CARTESIAN_POINT('Ctrl Pts',(-4.51771140424386,0.000115276608145367,
381.112583302492));
#28522=CARTESIAN_POINT('Ctrl Pts',(-4.51789787410811,0.186866521003934,
381.106004338462));
#28523=CARTESIAN_POINT('Ctrl Pts',(-4.50653449305084,0.373595224723727,
381.099425374433));
#28524=CARTESIAN_POINT('Ctrl Pts',(-4.48344098370869,0.558861765736475,
381.092846410403));
#28525=CARTESIAN_POINT('Ctrl Pts',(-4.3908559747359,1.30162043908853,381.066470451916));
#28526=CARTESIAN_POINT('Ctrl Pts',(-4.10973064608376,2.02087752596908,381.04009449343));
#28527=CARTESIAN_POINT('Ctrl Pts',(-3.6740998895201,2.62955500597139,381.013718534943));
#28528=CARTESIAN_POINT('Ctrl Pts',(-3.23846913295646,3.23823248597366,380.987342576457));
#28529=CARTESIAN_POINT('Ctrl Pts',(-2.6483329484813,3.73633035909772,380.96096661797));
#28530=CARTESIAN_POINT('Ctrl Pts',(-1.9751371259962,4.06354560219426,380.934590659483));
#28531=CARTESIAN_POINT('Ctrl Pts',(-1.30194130351109,4.3907608452908,380.908214700997));
#28532=CARTESIAN_POINT('Ctrl Pts',(-0.545685843016022,4.54709345835984,
380.88183874251));
#28533=CARTESIAN_POINT('Ctrl Pts',(0.202071967249689,4.51361678121356,380.855462784024));
#28534=CARTESIAN_POINT('Ctrl Pts',(0.949829777515443,4.48014010406728,380.829086825537));
#28535=CARTESIAN_POINT('Ctrl Pts',(1.68908993755185,4.25685413670566,380.802710867051));
#28536=CARTESIAN_POINT('Ctrl Pts',(2.33035272260718,3.87079135524483,380.776334908564));
#28537=CARTESIAN_POINT('Ctrl Pts',(2.97161550766248,3.48472857378402,380.749958950077));
#28538=CARTESIAN_POINT('Ctrl Pts',(3.51488091773671,2.93588897822401,380.723582991591));
#28539=CARTESIAN_POINT('Ctrl Pts',(3.89437764890032,2.29071872025929,380.697207033104));
#28540=CARTESIAN_POINT('Ctrl Pts',(4.27387438006393,1.64554846229457,380.670831074617));
#28541=CARTESIAN_POINT('Ctrl Pts',(4.48960243231693,0.904047541925131,380.644455116131));
#28542=CARTESIAN_POINT('Ctrl Pts',(4.51544434073745,0.155986965169938,380.618079157644));
#28543=CARTESIAN_POINT('Ctrl Pts',(4.54128624915798,-0.592073611585275,
380.591703199158));
#28544=CARTESIAN_POINT('Ctrl Pts',(4.37724201374605,-1.34669384472619,380.565327240671));
#28545=CARTESIAN_POINT('Ctrl Pts',(4.04317191469819,-2.01651441745319,380.538951282185));
#28546=CARTESIAN_POINT('Ctrl Pts',(3.70910181565035,-2.68633499018016,380.512575323698));
#28547=CARTESIAN_POINT('Ctrl Pts',(3.20500585296659,-3.27135590249316,380.486199365211));
#28548=CARTESIAN_POINT('Ctrl Pts',(2.59191321819219,-3.70075065317313,380.459823406725));
#28549=CARTESIAN_POINT('Ctrl Pts',(1.9788205834178,-4.13014540385311,380.433447448238));
#28550=CARTESIAN_POINT('Ctrl Pts',(1.25673127655275,-4.40391399290007,380.407071489751));
#28551=CARTESIAN_POINT('Ctrl Pts',(0.513066205288616,-4.48891218410335,
380.380695531265));
#28552=CARTESIAN_POINT('Ctrl Pts',(-0.230598865975566,-4.57391037530665,
380.354319572778));
#28553=CARTESIAN_POINT('Ctrl Pts',(-0.995839701638859,-4.47013816866624,
380.327943614292));
#28554=CARTESIAN_POINT('Ctrl Pts',(-1.69001118451102,-4.19015891391108,
380.301567655805));
#28555=CARTESIAN_POINT('Ctrl Pts',(-2.38418266738314,-3.91017965915592,
380.275191697319));
#28556=CARTESIAN_POINT('Ctrl Pts',(-3.00728479746414,-3.45399335628602,
380.248815738832));
#28557=CARTESIAN_POINT('Ctrl Pts',(-3.48388070942679,-2.87682893653492,
380.222439780345));
#28558=CARTESIAN_POINT('Ctrl Pts',(-3.96047662138947,-2.2996645167838,380.196063821859));
#28559=CARTESIAN_POINT('Ctrl Pts',(-4.29056631523378,-1.60152198015145,
380.169687863372));
#28560=CARTESIAN_POINT('Ctrl Pts',(-4.43418694927082,-0.866923079931074,
380.143311904886));
#28561=CARTESIAN_POINT('Ctrl Pts',(-4.48996073737275,-0.581648170267025,
380.133069037421));
#28562=CARTESIAN_POINT('Ctrl Pts',(-4.5176133554335,-0.290875321156064,
380.122826169956));
#28563=CARTESIAN_POINT('Ctrl Pts',(-4.51744861143269,-7.15418913582019E-5,
380.112583302492));
#28564=CARTESIAN_POINT('Ctrl Pts',(-4.51796103056296,9.30366574888874E-5,
380.387416697508));
#28565=CARTESIAN_POINT('Ctrl Pts',(-4.5173690706415,-0.643204813367623,
380.410082718817));
#28566=CARTESIAN_POINT('Ctrl Pts',(-4.37853653898567,-1.28674998247137,
380.432748740126));
#28567=CARTESIAN_POINT('Ctrl Pts',(-4.11200700232459,-1.87215597270644,
380.455414761435));
#28568=CARTESIAN_POINT('Ctrl Pts',(-3.80185234842186,-2.55338025489479,
380.481790719921));
#28569=CARTESIAN_POINT('Ctrl Pts',(-3.3187771369476,-3.15587552361643,380.508166678408));
#28570=CARTESIAN_POINT('Ctrl Pts',(-2.72126564826557,-3.60669971648272,
380.534542636895));
#28571=CARTESIAN_POINT('Ctrl Pts',(-2.12375415958355,-4.05752390934902,
380.560918595381));
#28572=CARTESIAN_POINT('Ctrl Pts',(-1.41180639369374,-4.35667702635998,
380.587294553868));
#28573=CARTESIAN_POINT('Ctrl Pts',(-0.671615456256834,-4.46794161244568,
380.613670512354));
#28574=CARTESIAN_POINT('Ctrl Pts',(0.0685754811800957,-4.57920619853139,
380.640046470841));
#28575=CARTESIAN_POINT('Ctrl Pts',(0.837009590164088,-4.50258225369185,
380.666422429328));
#28576=CARTESIAN_POINT('Ctrl Pts',(1.54065515471516,-4.24734637951232,380.692798387814));
#28577=CARTESIAN_POINT('Ctrl Pts',(2.24430071926626,-3.99211050533279,380.719174346301));
#28578=CARTESIAN_POINT('Ctrl Pts',(2.88315773938438,-3.55826270181326,380.745550304787));
#28579=CARTESIAN_POINT('Ctrl Pts',(3.37988195854491,-2.99832745369971,380.771926263274));
#28580=CARTESIAN_POINT('Ctrl Pts',(3.87660617770542,-2.4383922055862,380.79830222176));
#28581=CARTESIAN_POINT('Ctrl Pts',(4.23119759590837,-1.75236951287867,380.824678180247));
#28582=CARTESIAN_POINT('Ctrl Pts',(4.40072703064927,-1.02331382039902,380.851054138734));
#28583=CARTESIAN_POINT('Ctrl Pts',(4.57025646539019,-0.294258127919331,
380.87743009722));
#28584=CARTESIAN_POINT('Ctrl Pts',(4.55472391666906,0.477830564332509,380.903806055707));
#28585=CARTESIAN_POINT('Ctrl Pts',(4.35600985757286,1.19947809235303,380.930182014193));
#28586=CARTESIAN_POINT('Ctrl Pts',(4.15729579847668,1.92112562037352,380.95655797268));
#28587=CARTESIAN_POINT('Ctrl Pts',(3.77540022900545,2.59233198416271,380.982933931167));
#28588=CARTESIAN_POINT('Ctrl Pts',(3.25655795281734,3.131836501679,381.009309889653));
#28589=CARTESIAN_POINT('Ctrl Pts',(2.73771567662922,3.6713410191953,381.03568584814));
#28590=CARTESIAN_POINT('Ctrl Pts',(2.08192669372421,4.07914369043871,381.062061806626));
#28591=CARTESIAN_POINT('Ctrl Pts',(1.36858515603701,4.30587322665008,381.088437765113));
#28592=CARTESIAN_POINT('Ctrl Pts',(0.655243618349795,4.53260276286145,381.1148137236));
#28593=CARTESIAN_POINT('Ctrl Pts',(-0.11565047411956,4.57825916404077,381.141189682086));
#28594=CARTESIAN_POINT('Ctrl Pts',(-0.850767583518968,4.43731496427064,
381.167565640573));
#28595=CARTESIAN_POINT('Ctrl Pts',(-1.58588469291835,4.2963707645005,381.193941599059));
#28596=CARTESIAN_POINT('Ctrl Pts',(-2.28522481924775,3.96882596378091,381.220317557546));
#28597=CARTESIAN_POINT('Ctrl Pts',(-2.8641212210839,3.49433530220608,381.246693516033));
#28598=CARTESIAN_POINT('Ctrl Pts',(-3.44301762292008,3.01984464063123,381.273069474519));
#28599=CARTESIAN_POINT('Ctrl Pts',(-3.90147030026302,2.39840811820112,381.299445433006));
#28600=CARTESIAN_POINT('Ctrl Pts',(-4.18397593959467,1.70526095076376,381.325821391492));
#28601=CARTESIAN_POINT('Ctrl Pts',(-4.40388606866954,1.16569620642928,381.346353160164));
#28602=CARTESIAN_POINT('Ctrl Pts',(-4.51718122901344,0.58267845338523,381.366884928836));
#28603=CARTESIAN_POINT('Ctrl Pts',(-4.51777632728029,-0.000114640610663838,
381.387416697508));
#28604=CARTESIAN_POINT('Origin',(0.,0.,387.));
#28605=CARTESIAN_POINT('',(-4.51741634198117,5.54534861180178E-5,382.387416697508));
#28606=CARTESIAN_POINT('',(-4.51801683772092,-7.91791388051273E-5,382.112583302492));
#28607=CARTESIAN_POINT('',(-4.51775,5.53264807684796E-16,387.));
#28608=CARTESIAN_POINT('Ctrl Pts',(-4.51801683772092,-7.91791388051273E-5,
382.112583302492));
#28609=CARTESIAN_POINT('Ctrl Pts',(-4.51747244268795,0.664048991360067,
382.089182506968));
#28610=CARTESIAN_POINT('Ctrl Pts',(-4.36919765227329,1.32841221793627,382.065781711444));
#28611=CARTESIAN_POINT('Ctrl Pts',(-4.08568376167234,1.92892657382487,382.04238091592));
#28612=CARTESIAN_POINT('Ctrl Pts',(-3.76612408682134,2.60578996102738,382.016004957434));
#28613=CARTESIAN_POINT('Ctrl Pts',(-3.27475081492882,3.20153698377045,381.989628998947));
#28614=CARTESIAN_POINT('Ctrl Pts',(-2.67105284443962,3.64404256695937,381.963253040461));
#28615=CARTESIAN_POINT('Ctrl Pts',(-2.06735487395043,4.08654815014828,381.936877081974));
#28616=CARTESIAN_POINT('Ctrl Pts',(-1.35133220486457,4.37581229378304,381.910501123487));
#28617=CARTESIAN_POINT('Ctrl Pts',(-0.609671277576736,4.47681476732048,
381.884125165001));
#28618=CARTESIAN_POINT('Ctrl Pts',(0.131989649711098,4.57781724085793,381.857749206514));
#28619=CARTESIAN_POINT('Ctrl Pts',(0.899288835200903,4.49055804429805,381.831373248027));
#28620=CARTESIAN_POINT('Ctrl Pts',(1.59933196425767,4.22560135314543,381.804997289541));
#28621=CARTESIAN_POINT('Ctrl Pts',(2.29937509331447,3.9606446619928,381.778621331054));
#28622=CARTESIAN_POINT('Ctrl Pts',(2.93216216593823,3.5179904762474,381.752245372568));
#28623=CARTESIAN_POINT('Ctrl Pts',(3.42108379359719,2.95122943953659,381.725869414081));
#28624=CARTESIAN_POINT('Ctrl Pts',(3.91000542125612,2.38446840282581,381.699493455595));
#28625=CARTESIAN_POINT('Ctrl Pts',(4.25506160395026,1.69360051514964,381.673117497108));
#28626=CARTESIAN_POINT('Ctrl Pts',(4.41447755785592,0.962266812681007,381.646741538621));
#28627=CARTESIAN_POINT('Ctrl Pts',(4.57389351176158,0.23093311021233,381.620365580135));
#28628=CARTESIAN_POINT('Ctrl Pts',(4.54766923687872,-0.540866407048814,
381.593989621648));
#28629=CARTESIAN_POINT('Ctrl Pts',(4.33897961738306,-1.25969258453608,381.567613663161));
#28630=CARTESIAN_POINT('Ctrl Pts',(4.1302899978874,-1.9785187620233,381.541237704675));
#28631=CARTESIAN_POINT('Ctrl Pts',(3.73913503377896,-2.64437159973664,381.514861746188));
#28632=CARTESIAN_POINT('Ctrl Pts',(3.21287053227619,-3.17663854891175,381.488485787702));
#28633=CARTESIAN_POINT('Ctrl Pts',(2.68660603077342,-3.70890549808685,381.462109829215));
#28634=CARTESIAN_POINT('Ctrl Pts',(2.02523199187631,-4.1075865587237,381.435733870728));
#28635=CARTESIAN_POINT('Ctrl Pts',(1.3088187313399,-4.32441476457735,381.409357912242));
#28636=CARTESIAN_POINT('Ctrl Pts',(0.592405470803483,-4.54124297043101,
381.382981953755));
#28637=CARTESIAN_POINT('Ctrl Pts',(-0.179047011372244,-4.57621832150146,
381.356605995269));
#28638=CARTESIAN_POINT('Ctrl Pts',(-0.912141574983824,-4.42510647044643,
381.330230036782));
#28639=CARTESIAN_POINT('Ctrl Pts',(-1.64523613859541,-4.2739946193914,381.303854078296));
#28640=CARTESIAN_POINT('Ctrl Pts',(-2.33997278364284,-3.93679556621089,
381.277478119809));
#28641=CARTESIAN_POINT('Ctrl Pts',(-2.91224209659624,-3.45433285865933,
381.251102161322));
#28642=CARTESIAN_POINT('Ctrl Pts',(-3.48451140954963,-2.97187015110778,
381.224726202836));
#28643=CARTESIAN_POINT('Ctrl Pts',(-3.93431339040899,-2.34414378918517,
381.198350244349));
#28644=CARTESIAN_POINT('Ctrl Pts',(-4.20719203619195,-1.64715047831211,
381.171974285863));
#28645=CARTESIAN_POINT('Ctrl Pts',(-4.4120064713043,-1.1240084389856,381.152177291406));
#28646=CARTESIAN_POINT('Ctrl Pts',(-4.51715029114881,-0.561844529442614,
381.132380296949));
#28647=CARTESIAN_POINT('Ctrl Pts',(-4.51771140424386,0.000115276608145367,
381.112583302492));
#28648=CARTESIAN_POINT('Ctrl Pts',(-4.51777632728029,-0.000114640610663838,
381.387416697508));
#28649=CARTESIAN_POINT('Ctrl Pts',(-4.51794571683875,-0.166001638386794,
381.393260887323));
#28650=CARTESIAN_POINT('Ctrl Pts',(-4.50898407036945,-0.331870434133353,
381.399105077137));
#28651=CARTESIAN_POINT('Ctrl Pts',(-4.49075105445655,-0.496713740704063,
381.404949266952));
#28652=CARTESIAN_POINT('Ctrl Pts',(-4.40846192866641,-1.24068345228999,
381.431325225439));
#28653=CARTESIAN_POINT('Ctrl Pts',(-4.13732507576575,-1.96376506301729,
381.457701183925));
#28654=CARTESIAN_POINT('Ctrl Pts',(-3.71016611657994,-2.57841753032532,
381.484077142412));
#28655=CARTESIAN_POINT('Ctrl Pts',(-3.28300715739413,-3.19306999763336,
381.510453100898));
#28656=CARTESIAN_POINT('Ctrl Pts',(-2.69982609192317,-3.69929332152213,
381.536829059385));
#28657=CARTESIAN_POINT('Ctrl Pts',(-2.03122667735788,-4.03580075802764,
381.563205017872));
#28658=CARTESIAN_POINT('Ctrl Pts',(-1.36262726279259,-4.37230819453315,
381.589580976358));
#28659=CARTESIAN_POINT('Ctrl Pts',(-0.608609499132967,-4.5390997436554,
381.615956934845));
#28660=CARTESIAN_POINT('Ctrl Pts',(0.139540235761641,-4.51598251722816,
381.642332893331));
#28661=CARTESIAN_POINT('Ctrl Pts',(0.887689970656269,-4.49286529080092,
381.668708851818));
#28662=CARTESIAN_POINT('Ctrl Pts',(1.62997167678589,-4.2798392888242,381.695084810305));
#28663=CARTESIAN_POINT('Ctrl Pts',(2.27651982104296,-3.90269484814088,381.721460768791));
#28664=CARTESIAN_POINT('Ctrl Pts',(2.92306796530002,-3.52555040745756,381.747836727278));
#28665=CARTESIAN_POINT('Ctrl Pts',(3.47388254768454,-2.98428752806765,381.774212685764));
#28666=CARTESIAN_POINT('Ctrl Pts',(3.86227831153366,-2.3444350742905,381.800588644251));
#28667=CARTESIAN_POINT('Ctrl Pts',(4.25067407538277,-1.70458262051336,381.826964602737));
#28668=CARTESIAN_POINT('Ctrl Pts',(4.47665102069649,-0.966140592348972,
381.853340561224));
#28669=CARTESIAN_POINT('Ctrl Pts',(4.51285088376856,-0.21850966609316,381.879716519711));
#28670=CARTESIAN_POINT('Ctrl Pts',(4.54905074684063,0.529121260162651,381.906092478197));
#28671=CARTESIAN_POINT('Ctrl Pts',(4.39547352767104,1.28594108450989,381.932468436684));
#28672=CARTESIAN_POINT('Ctrl Pts',(4.07071230023681,1.96032419308837,381.95884439517));
#28673=CARTESIAN_POINT('Ctrl Pts',(3.74595107280257,2.63470730166687,381.985220353657));
#28674=CARTESIAN_POINT('Ctrl Pts',(3.25000583710367,3.2266536944766,382.011596312144));
#28675=CARTESIAN_POINT('Ctrl Pts',(2.64291900376427,3.66449842582154,382.03797227063));
#28676=CARTESIAN_POINT('Ctrl Pts',(2.03583217042486,4.10234315716648,382.064348229117));
#28677=CARTESIAN_POINT('Ctrl Pts',(1.31760373944494,4.38608622704663,382.090724187603));
#28678=CARTESIAN_POINT('Ctrl Pts',(0.575187195343948,4.48137582262626,382.11710014609));
#28679=CARTESIAN_POINT('Ctrl Pts',(-0.167229348757025,4.57666541820589,
382.143476104577));
#28680=CARTESIAN_POINT('Ctrl Pts',(-0.933834005979071,4.48350153948501,
382.169852063063));
#28681=CARTESIAN_POINT('Ctrl Pts',(-1.63181654587318,4.21316322184666,382.19622802155));
#28682=CARTESIAN_POINT('Ctrl Pts',(-2.32979908576728,3.94282490420832,382.222603980037));
#28683=CARTESIAN_POINT('Ctrl Pts',(-2.95915950833345,3.4953121476525,382.248979938523));
#28684=CARTESIAN_POINT('Ctrl Pts',(-3.44370327796121,2.9248038065255,382.27535589701));
#28685=CARTESIAN_POINT('Ctrl Pts',(-3.92824704758899,2.35429546539847,382.301731855496));
#28686=CARTESIAN_POINT('Ctrl Pts',(-4.26797416427836,1.66079153970024,382.328107813983));
#28687=CARTESIAN_POINT('Ctrl Pts',(-4.42175501618481,0.928252201802573,
382.354483772469));
#28688=CARTESIAN_POINT('Ctrl Pts',(-4.48575841876287,0.623370224843185,
382.365461414149));
#28689=CARTESIAN_POINT('Ctrl Pts',(-4.5175519448549,0.311726478256462,382.376439055828));
#28690=CARTESIAN_POINT('Ctrl Pts',(-4.51741634198117,5.54534861180178E-5,
382.387416697508));
#28691=CARTESIAN_POINT('Origin',(0.,0.,387.));
#28692=CARTESIAN_POINT('',(-4.51810647145572,4.12515443024009E-5,383.387416697508));
#28693=CARTESIAN_POINT('',(-4.51737744603353,-1.71510238390164E-5,383.112583302492));
#28694=CARTESIAN_POINT('',(-4.51775,5.53264807684796E-16,387.));
#28695=CARTESIAN_POINT('Ctrl Pts',(-4.51737744603353,-1.71510238390164E-5,
383.112583302492));
#28696=CARTESIAN_POINT('Ctrl Pts',(-4.51732510787532,0.393119355640695,
383.09873663396));
#28697=CARTESIAN_POINT('Ctrl Pts',(-4.46651507043149,0.786269138328428,
383.084889965429));
#28698=CARTESIAN_POINT('Ctrl Pts',(-4.36511527641182,1.16590657912072,383.071043296898));
#28699=CARTESIAN_POINT('Ctrl Pts',(-4.17196291261205,1.8890625754899,383.044667338411));
#28700=CARTESIAN_POINT('Ctrl Pts',(-3.79524613196318,2.56318917681575,383.018291379924));
#28701=CARTESIAN_POINT('Ctrl Pts',(-3.28057275969385,3.10667215778483,382.991915421438));
#28702=CARTESIAN_POINT('Ctrl Pts',(-2.76589938742451,3.65015513875392,382.965539462951));
#28703=CARTESIAN_POINT('Ctrl Pts',(-2.11326942353471,4.06299449936623,382.939163504465));
#28704=CARTESIAN_POINT('Ctrl Pts',(-1.40169456822207,4.29520917593283,382.912787545978));
#28705=CARTESIAN_POINT('Ctrl Pts',(-0.690119712909428,4.52742385249943,
382.886411587491));
#28706=CARTESIAN_POINT('Ctrl Pts',(0.0804000338260355,4.57901384502031,
382.860035629005));
#28707=CARTESIAN_POINT('Ctrl Pts',(0.816580454902776,4.44373332776299,382.833659670518));
#28708=CARTESIAN_POINT('Ctrl Pts',(1.55276087597956,4.30845281050567,382.807283712031));
#28709=CARTESIAN_POINT('Ctrl Pts',(2.2546019713976,3.98630178347012,382.780907753545));
#28710=CARTESIAN_POINT('Ctrl Pts',(2.83713421587333,3.51628198083169,382.754531795058));
#28711=CARTESIAN_POINT('Ctrl Pts',(3.41966646034902,3.04626217819329,382.728155836572));
#28712=CARTESIAN_POINT('Ctrl Pts',(3.88288985388241,2.42837359995203,382.701779878085));
#28713=CARTESIAN_POINT('Ctrl Pts',(4.17072350849794,1.7374219243648,382.675403919598));
#28714=CARTESIAN_POINT('Ctrl Pts',(4.45855716311345,1.04647024877758,382.649027961112));
#28715=CARTESIAN_POINT('Ctrl Pts',(4.57100107881112,0.282455475844346,382.622652002625));
#28716=CARTESIAN_POINT('Ctrl Pts',(4.4944420514052,-0.462125712508384,382.596276044139));
#28717=CARTESIAN_POINT('Ctrl Pts',(4.41788302399928,-1.20670690086118,382.569900085652));
#28718=CARTESIAN_POINT('Ctrl Pts',(4.15232105348975,-1.93185450463351,382.543524127166));
#28719=CARTESIAN_POINT('Ctrl Pts',(3.72990682856509,-2.54977735848138,382.517148168679));
#28720=CARTESIAN_POINT('Ctrl Pts',(3.30749260364046,-3.16770021232922,382.490772210192));
#28721=CARTESIAN_POINT('Ctrl Pts',(2.72822612430073,-3.6783983162526,382.464396251706));
#28722=CARTESIAN_POINT('Ctrl Pts',(2.06223722204694,-4.02004317981846,382.438020293219));
#28723=CARTESIAN_POINT('Ctrl Pts',(1.39624831979316,-4.36168804338432,382.411644334732));
#28724=CARTESIAN_POINT('Ctrl Pts',(0.643536994625335,-4.53427966659265,
382.385268376246));
#28725=CARTESIAN_POINT('Ctrl Pts',(-0.104768541682353,-4.51692296594424,
382.358892417759));
#28726=CARTESIAN_POINT('Ctrl Pts',(-0.853074077990042,-4.49956626529584,
382.332516459273));
#28727=CARTESIAN_POINT('Ctrl Pts',(-1.59697382543758,-4.29226124079071,
382.306140500786));
#28728=CARTESIAN_POINT('Ctrl Pts',(-2.2464063601331,-3.92010560989808,382.2797645423));
#28729=CARTESIAN_POINT('Ctrl Pts',(-2.89583889482865,-3.54794997900543,
382.253388583813));
#28730=CARTESIAN_POINT('Ctrl Pts',(-3.45080421677215,-3.01094374172526,
382.227012625326));
#28731=CARTESIAN_POINT('Ctrl Pts',(-3.84411455331502,-2.37410042512789,
382.20063666684));
#28732=CARTESIAN_POINT('Ctrl Pts',(-4.23742488985787,-1.73725710853056,
382.174260708353));
#28733=CARTESIAN_POINT('Ctrl Pts',(-4.46908024100009,-1.00057671261605,
382.147884749867));
#28734=CARTESIAN_POINT('Ctrl Pts',(-4.51103487766645,-0.253246638827817,
382.12150879138));
#28735=CARTESIAN_POINT('Ctrl Pts',(-4.51576728885779,-0.168949085903131,
382.118533628417));
#28736=CARTESIAN_POINT('Ctrl Pts',(-4.51808605177553,-0.0845160322941951,
382.115558465455));
#28737=CARTESIAN_POINT('Ctrl Pts',(-4.51801683772092,-7.91791388051273E-5,
382.112583302492));
#28738=CARTESIAN_POINT('Ctrl Pts',(-4.51741634198117,5.54534861180178E-5,
382.387416697508));
#28739=CARTESIAN_POINT('Ctrl Pts',(-4.51722613209177,-0.43712489171991,
382.402815014315));
#28740=CARTESIAN_POINT('Ctrl Pts',(-4.45421338524669,-0.874358908440133,
382.418213331122));
#28741=CARTESIAN_POINT('Ctrl Pts',(-4.32915293519383,-1.29306010572185,
382.433611647929));
#28742=CARTESIAN_POINT('Ctrl Pts',(-4.11493541517289,-2.01025832525158,
382.459987606416));
#28743=CARTESIAN_POINT('Ctrl Pts',(-3.71866578800746,-2.67308001421398,
382.486363564902));
#28744=CARTESIAN_POINT('Ctrl Pts',(-3.1883190758562,-3.2012795947618,382.512739523389));
#28745=CARTESIAN_POINT('Ctrl Pts',(-2.65797236370492,-3.72947917530964,
382.539115481875));
#28746=CARTESIAN_POINT('Ctrl Pts',(-1.99354856656775,-4.1230566474429,382.565491440362));
#28747=CARTESIAN_POINT('Ctrl Pts',(-1.27548722410474,-4.33436291909808,
382.591867398849));
#28748=CARTESIAN_POINT('Ctrl Pts',(-0.557425881641732,-4.54566919075325,
382.618243357335));
#28749=CARTESIAN_POINT('Ctrl Pts',(0.214273006147169,-4.57470426193039,
382.644619315822));
#28750=CARTESIAN_POINT('Ctrl Pts',(0.94618246756513,-4.4179529548626,382.670995274309));
#28751=CARTESIAN_POINT('Ctrl Pts',(1.67809192898305,-4.26120164779482,382.697371232795));
#28752=CARTESIAN_POINT('Ctrl Pts',(2.37021196402998,-3.91866396248217,382.723747191282));
#28753=CARTESIAN_POINT('Ctrl Pts',(2.93874994329017,-3.4318097767969,382.750123149768));
#28754=CARTESIAN_POINT('Ctrl Pts',(3.50728792255042,-2.94495559111159,382.776499108255));
#28755=CARTESIAN_POINT('Ctrl Pts',(3.95224384602383,-2.31378490505366,382.802875066742));
#28756=CARTESIAN_POINT('Ctrl Pts',(4.21974840648906,-1.61471141670574,382.829251025228));
#28757=CARTESIAN_POINT('Ctrl Pts',(4.48725296695428,-0.91563792835784,382.855626983715));
#28758=CARTESIAN_POINT('Ctrl Pts',(4.57730616441131,-0.148661637719957,
382.882002942201));
#28759=CARTESIAN_POINT('Ctrl Pts',(4.47900556312629,0.593362232359432,382.908378900688));
#28760=CARTESIAN_POINT('Ctrl Pts',(4.38070496184126,1.33538610243882,382.934754859174));
#28761=CARTESIAN_POINT('Ctrl Pts',(4.09405056181417,2.05245755195971,382.961130817661));
#28762=CARTESIAN_POINT('Ctrl Pts',(3.6537466407651,2.65776316823087,382.987506776148));
#28763=CARTESIAN_POINT('Ctrl Pts',(3.21344271971605,3.26306878450199,383.013882734634));
#28764=CARTESIAN_POINT('Ctrl Pts',(2.61948927764498,3.75660856752342,383.040258693121));
#28765=CARTESIAN_POINT('Ctrl Pts',(1.94379424690704,4.07863132668275,383.066634651607));
#28766=CARTESIAN_POINT('Ctrl Pts',(1.26809921616909,4.4006540858421,383.093010610094));
#28767=CARTESIAN_POINT('Ctrl Pts',(0.510662596764224,4.55115982113938,383.119386568581));
#28768=CARTESIAN_POINT('Ctrl Pts',(-0.236815324157952,4.51192731275126,
383.145762527067));
#28769=CARTESIAN_POINT('Ctrl Pts',(-0.984293245080149,4.47269480436314,
383.172138485554));
#28770=CARTESIAN_POINT('Ctrl Pts',(-1.72181246751965,4.24372405228961,383.19851444404));
#28771=CARTESIAN_POINT('Ctrl Pts',(-2.36008403614551,3.85273577028557,383.224890402527));
#28772=CARTESIAN_POINT('Ctrl Pts',(-2.99835560477138,3.46174748828153,383.251266361013));
#28773=CARTESIAN_POINT('Ctrl Pts',(-3.53737951958361,2.90874167634699,383.2776423195));
#28774=CARTESIAN_POINT('Ctrl Pts',(-3.91189798012409,2.26066887588782,383.304018277987));
#28775=CARTESIAN_POINT('Ctrl Pts',(-4.28641644066456,1.61259607542868,383.330394236473));
#28776=CARTESIAN_POINT('Ctrl Pts',(-4.49642944693329,0.869456286444925,
383.35677019496));
#28777=CARTESIAN_POINT('Ctrl Pts',(-4.51651143527701,0.121218927230134,
383.383146153446));
#28778=CARTESIAN_POINT('Ctrl Pts',(-4.5175952633915,0.0808364375906089,
383.384569668134));
#28779=CARTESIAN_POINT('Ctrl Pts',(-4.51812586459283,0.0404390998600549,
383.385993182821));
#28780=CARTESIAN_POINT('Ctrl Pts',(-4.51810647145572,4.12515443024009E-5,
383.387416697508));
#28781=CARTESIAN_POINT('Origin',(0.,0.,387.));
#28782=CARTESIAN_POINT('',(-4.51758348284472,-0.000105543616906456,384.387416697508));
#28783=CARTESIAN_POINT('',(-4.51791286673421,0.000101789655423226,384.112583302492));
#28784=CARTESIAN_POINT('',(-4.51775,5.53264807684796E-16,387.));
#28785=CARTESIAN_POINT('Ctrl Pts',(-4.51791286673421,0.000101789655423226,
384.112583302492));
#28786=CARTESIAN_POINT('Ctrl Pts',(-4.51803160945122,0.121934720290465,
384.108290760953));
#28787=CARTESIAN_POINT('Ctrl Pts',(-4.51320179205148,0.243758262585871,
384.103998219414));
#28788=CARTESIAN_POINT('Ctrl Pts',(-4.50335615873677,0.365175074681226,
384.099705677874));
#28789=CARTESIAN_POINT('Ctrl Pts',(-4.4428586625063,1.11123303735971,384.073329719388));
#28790=CARTESIAN_POINT('Ctrl Pts',(-4.19298336184317,1.84193444118764,384.046953760901));
#28791=CARTESIAN_POINT('Ctrl Pts',(-3.78398181342604,2.46881574105112,384.020577802415));
#28792=CARTESIAN_POINT('Ctrl Pts',(-3.37498026500888,3.09569704091462,383.994201843928));
#28793=CARTESIAN_POINT('Ctrl Pts',(-2.80685246883769,3.61875823681367,383.967825885442));
#28794=CARTESIAN_POINT('Ctrl Pts',(-2.14837973375322,3.97467408062589,383.941449926955));
#28795=CARTESIAN_POINT('Ctrl Pts',(-1.48990699866878,4.33058992443809,383.915073968468));
#28796=CARTESIAN_POINT('Ctrl Pts',(-0.741089324671071,4.5193604161635,383.888698009982));
#28797=CARTESIAN_POINT('Ctrl Pts',(0.00741646763062709,4.51813175146638,
383.862322051495));
#28798=CARTESIAN_POINT('Ctrl Pts',(0.755922259932325,4.51690308676927,383.835946093009));
#28799=CARTESIAN_POINT('Ctrl Pts',(1.50411617053801,4.32567526564963,383.809570134522));
#28800=CARTESIAN_POINT('Ctrl Pts',(2.16141689576047,3.96759959299347,383.783194176035));
#28801=CARTESIAN_POINT('Ctrl Pts',(2.81871762098293,3.60952392033731,383.756818217549));
#28802=CARTESIAN_POINT('Ctrl Pts',(3.38512516082216,3.08460039614464,383.730442259062));
#28803=CARTESIAN_POINT('Ctrl Pts',(3.79206647204748,2.45637973431923,383.704066300576));
#28804=CARTESIAN_POINT('Ctrl Pts',(4.19900778327279,1.82815907249382,383.677690342089));
#28805=CARTESIAN_POINT('Ctrl Pts',(4.44648286588418,1.09664127303568,383.651314383602));
#28806=CARTESIAN_POINT('Ctrl Pts',(4.50453074947641,0.35038871931369,383.624938425116));
#28807=CARTESIAN_POINT('Ctrl Pts',(4.56257863306864,-0.395863834408303,
383.598562466629));
#28808=CARTESIAN_POINT('Ctrl Pts',(4.4311993176417,-1.15685114239415,383.572186508143));
#28809=CARTESIAN_POINT('Ctrl Pts',(4.12629845211925,-1.84044304764888,383.545810549656));
#28810=CARTESIAN_POINT('Ctrl Pts',(3.8213975865968,-2.52403495290361,383.519434591169));
#28811=CARTESIAN_POINT('Ctrl Pts',(3.34297517097883,-3.13023145542722,383.493058632683));
#28812=CARTESIAN_POINT('Ctrl Pts',(2.74895218738718,-3.58564239698551,383.466682674196));
#28813=CARTESIAN_POINT('Ctrl Pts',(2.15492920379552,-4.04105333854382,383.44030671571));
#28814=CARTESIAN_POINT('Ctrl Pts',(1.44530565223012,-4.34567871913682,383.413930757223));
#28815=CARTESIAN_POINT('Ctrl Pts',(0.705993253592304,-4.46263857526945,
383.387554798737));
#28816=CARTESIAN_POINT('Ctrl Pts',(-0.0333191450455116,-4.57959843140208,
383.36117884025));
#28817=CARTESIAN_POINT('Ctrl Pts',(-0.802320390755788,-4.50889276307437,
383.334802881763));
#28818=CARTESIAN_POINT('Ctrl Pts',(-1.50791010623509,-4.25908166617111,
383.308426923277));
#28819=CARTESIAN_POINT('Ctrl Pts',(-2.21349982171436,-4.00927056926786,
383.28205096479));
#28820=CARTESIAN_POINT('Ctrl Pts',(-2.8556780069626,-3.58035404378911,383.255675006304));
#28821=CARTESIAN_POINT('Ctrl Pts',(-3.35669832323709,-3.02425956134359,
383.229299047817));
#28822=CARTESIAN_POINT('Ctrl Pts',(-3.85771863951158,-2.46816507889806,
383.20292308933));
#28823=CARTESIAN_POINT('Ctrl Pts',(-4.21758108681228,-1.78489263948572,
383.176547130844));
#28824=CARTESIAN_POINT('Ctrl Pts',(-4.39271833698727,-1.05716372407332,
383.150171172357));
#28825=CARTESIAN_POINT('Ctrl Pts',(-4.4759132430793,-0.711472908911519,
383.137641882402));
#28826=CARTESIAN_POINT('Ctrl Pts',(-4.51742480471468,-0.355750464977554,
383.125112592447));
#28827=CARTESIAN_POINT('Ctrl Pts',(-4.51737744603353,-1.71510238390164E-5,
383.112583302492));
#28828=CARTESIAN_POINT('Ctrl Pts',(-4.51810647145572,4.12515443024009E-5,
383.387416697508));
#28829=CARTESIAN_POINT('Ctrl Pts',(-4.51776653385746,-0.70808283654263,
383.412369141307));
#28830=CARTESIAN_POINT('Ctrl Pts',(-4.34843679840707,-1.41636380567975,
383.437321585107));
#28831=CARTESIAN_POINT('Ctrl Pts',(-4.0275273935072,-2.04758215167448,383.462274028906));
#28832=CARTESIAN_POINT('Ctrl Pts',(-3.68831039297495,-2.71481094191849,
383.488649987393));
#28833=CARTESIAN_POINT('Ctrl Pts',(-3.17972542149173,-3.29593359296068,
383.515025945879));
#28834=CARTESIAN_POINT('Ctrl Pts',(-2.56334513970026,-3.72059555287616,
383.541401904366));
#28835=CARTESIAN_POINT('Ctrl Pts',(-1.94696485790879,-4.14525751279165,
383.567777862853));
#28836=CARTESIAN_POINT('Ctrl Pts',(-1.22278926580908,-4.41345878158044,
383.594153821339));
#28837=CARTESIAN_POINT('Ctrl Pts',(-0.478491850582746,-4.49272913964694,
383.620529779826));
#28838=CARTESIAN_POINT('Ctrl Pts',(0.265805564643564,-4.57199949771343,
383.646905738312));
#28839=CARTESIAN_POINT('Ctrl Pts',(1.0302248029965,-4.46233894505765,383.673281696799));
#28840=CARTESIAN_POINT('Ctrl Pts',(1.72222021529061,-4.17702371352512,383.699657655286));
#28841=CARTESIAN_POINT('Ctrl Pts',(2.41421562758474,-3.89170848199258,383.726033613772));
#28842=CARTESIAN_POINT('Ctrl Pts',(3.03378721382,-3.43073857158334,383.752409572259));
#28843=CARTESIAN_POINT('Ctrl Pts',(3.50592553965972,-2.84992204870037,383.778785530746));
#28844=CARTESIAN_POINT('Ctrl Pts',(3.97806386549944,-2.2691055258174,383.805161489232));
#28845=CARTESIAN_POINT('Ctrl Pts',(4.30276893094358,-1.56844239046068,383.831537447719));
#28846=CARTESIAN_POINT('Ctrl Pts',(4.44072979303352,-0.832759556277373,
383.857913406205));
#28847=CARTESIAN_POINT('Ctrl Pts',(4.57869065512346,-0.0970767220940631,
383.884289364692));
#28848=CARTESIAN_POINT('Ctrl Pts',(4.52990731385923,0.673625810915847,383.910665323178));
#28849=CARTESIAN_POINT('Ctrl Pts',(4.30028580320783,1.38604169635549,383.937041281665));
#28850=CARTESIAN_POINT('Ctrl Pts',(4.07066429255644,2.0984575817951,383.963417240152));
#28851=CARTESIAN_POINT('Ctrl Pts',(3.66020461251785,2.75258681966445,383.989793198638));
#28852=CARTESIAN_POINT('Ctrl Pts',(3.11859972691059,3.26923619774099,384.016169157125));
#28853=CARTESIAN_POINT('Ctrl Pts',(2.57699484130331,3.78588557581757,384.042545115611));
#28854=CARTESIAN_POINT('Ctrl Pts',(1.90424475012738,4.16505509410136,384.068921074098));
#28855=CARTESIAN_POINT('Ctrl Pts',(1.18179702927259,4.36083998272228,384.095297032584));
#28856=CARTESIAN_POINT('Ctrl Pts',(0.459349308417798,4.55662487134321,384.121672991071));
#28857=CARTESIAN_POINT('Ctrl Pts',(-0.312796042115809,4.56902513030122,
384.148048949558));
#28858=CARTESIAN_POINT('Ctrl Pts',(-1.04115799889843,4.39653950222634,384.174424908044));
#28859=CARTESIAN_POINT('Ctrl Pts',(-1.76951995568104,4.22405387415146,384.200800866531));
#28860=CARTESIAN_POINT('Ctrl Pts',(-2.45409851871268,3.86668235904368,384.227176825017));
#28861=CARTESIAN_POINT('Ctrl Pts',(-3.0120140790621,3.36769071632751,384.253552783504));
#28862=CARTESIAN_POINT('Ctrl Pts',(-3.56992963941149,2.86869907361137,384.279928741991));
#28863=CARTESIAN_POINT('Ctrl Pts',(-4.00118219707867,2.22808730328684,384.306304700477));
#28864=CARTESIAN_POINT('Ctrl Pts',(-4.25356146494663,1.52341210354517,384.332680658964));
#28865=CARTESIAN_POINT('Ctrl Pts',(-4.42814268873775,1.0359589946372,384.350926005145));
#28866=CARTESIAN_POINT('Ctrl Pts',(-4.51713190568983,0.51785112729682,384.369171351326));
#28867=CARTESIAN_POINT('Ctrl Pts',(-4.51758348284472,-0.000105543616906456,
384.387416697508));
#28868=CARTESIAN_POINT('Origin',(0.,0.,387.));
#28869=CARTESIAN_POINT('',(-4.51754236316255,9.86160820556914E-5,385.387416697508));
#28870=CARTESIAN_POINT('',(-4.51782825948384,-0.000111641905798056,385.112583302492));
#28871=CARTESIAN_POINT('',(-4.51775,5.53264807684796E-16,387.));
#28872=CARTESIAN_POINT('Ctrl Pts',(-4.51782825948384,-0.000111641905798056,
385.112583302492));
#28873=CARTESIAN_POINT('Ctrl Pts',(-4.51721726779753,0.599198793910267,
385.091468929459));
#28874=CARTESIAN_POINT('Ctrl Pts',(-4.39722715972494,1.19874658011254,385.070354556425));
#28875=CARTESIAN_POINT('Ctrl Pts',(-4.16499712691276,1.75110492558535,385.049240183392));
#28876=CARTESIAN_POINT('Ctrl Pts',(-3.87489664914265,2.44110792813221,385.022864224905));
#28877=CARTESIAN_POINT('Ctrl Pts',(-3.40964724164981,3.05747242764947,384.996488266419));
#28878=CARTESIAN_POINT('Ctrl Pts',(-2.82557507506063,3.52557726093145,384.970112307932));
#28879=CARTESIAN_POINT('Ctrl Pts',(-2.24150290847142,3.99368209421345,384.943736349446));
#28880=CARTESIAN_POINT('Ctrl Pts',(-1.53860798278584,4.31352726126017,384.917360390959));
#28881=CARTESIAN_POINT('Ctrl Pts',(-0.801987406950171,4.44639019055842,
384.890984432472));
#28882=CARTESIAN_POINT('Ctrl Pts',(-0.065366831114539,4.57925311985666,
384.864608473986));
#28883=CARTESIAN_POINT('Ctrl Pts',(0.7049793948712,4.52513381140646,384.838232515499));
#28884=CARTESIAN_POINT('Ctrl Pts',(1.41578806149518,4.29058430665667,384.811856557012));
#28885=CARTESIAN_POINT('Ctrl Pts',(2.12659672811916,4.05603480190689,384.785480598526));
#28886=CARTESIAN_POINT('Ctrl Pts',(2.77786783538139,3.64105510085751,384.759104640039));
#28887=CARTESIAN_POINT('Ctrl Pts',(3.29075419525559,3.09588539096791,384.732728681553));
#28888=CARTESIAN_POINT('Ctrl Pts',(3.8036405551298,2.55071568107831,384.706352723066));
#28889=CARTESIAN_POINT('Ctrl Pts',(4.178142167616,1.87535596234848,384.67997676458));
#28890=CARTESIAN_POINT('Ctrl Pts',(4.36891939039539,1.15156974944116,384.653600806093));
#28891=CARTESIAN_POINT('Ctrl Pts',(4.55969661317478,0.427783536533828,384.627224847606));
#28892=CARTESIAN_POINT('Ctrl Pts',(4.56674944624736,-0.344429170550942,
384.60084888912));
#28893=CARTESIAN_POINT('Ctrl Pts',(4.38922402699095,-1.07157919375385,384.574472930633));
#28894=CARTESIAN_POINT('Ctrl Pts',(4.21169860773453,-1.79872921695679,384.548096972147));
#28895=CARTESIAN_POINT('Ctrl Pts',(3.84959493614911,-2.48081655627781,384.52172101366));
#28896=CARTESIAN_POINT('Ctrl Pts',(3.34675167782285,-3.03526320680608,384.495345055174));
#28897=CARTESIAN_POINT('Ctrl Pts',(2.84390841949662,-3.58970985733432,384.468969096687));
#28898=CARTESIAN_POINT('Ctrl Pts',(2.20032557442955,-4.01651581906983,384.4425931382));
#28899=CARTESIAN_POINT('Ctrl Pts',(1.49391953877316,-4.26400913921072,384.416217179714));
#28900=CARTESIAN_POINT('Ctrl Pts',(0.787513503116781,-4.51150245935161,
384.389841221227));
#28901=CARTESIAN_POINT('Ctrl Pts',(0.0182842768710745,-4.57968313789789,
384.363465262741));
#28902=CARTESIAN_POINT('Ctrl Pts',(-0.720640161828923,-4.46029677092904,
384.337089304254));
#28903=CARTESIAN_POINT('Ctrl Pts',(-1.45956460052894,-4.34091040396018,
384.310713345767));
#28904=CARTESIAN_POINT('Ctrl Pts',(-2.16818425168326,-4.03395699147619,
384.284337387281));
#28905=CARTESIAN_POINT('Ctrl Pts',(-2.76070893321464,-3.57659834391139,
384.257961428794));
#28906=CARTESIAN_POINT('Ctrl Pts',(-3.35323361474601,-3.11923969634659,
384.231585470308));
#28907=CARTESIAN_POINT('Ctrl Pts',(-3.82966332665445,-2.51147581370097,
384.205209511821));
#28908=CARTESIAN_POINT('Ctrl Pts',(-4.13231833670975,-1.82688661161363,
384.178833553334));
#28909=CARTESIAN_POINT('Ctrl Pts',(-4.38571791578798,-1.25371052039765,
384.156750136387));
#28910=CARTESIAN_POINT('Ctrl Pts',(-4.51730198273802,-0.626680125117799,
384.134666719439));
#28911=CARTESIAN_POINT('Ctrl Pts',(-4.51791286673421,0.000101789655423226,
384.112583302492));
#28912=CARTESIAN_POINT('Ctrl Pts',(-4.51758348284472,-0.000105543616906456,
384.387416697508));
#28913=CARTESIAN_POINT('Ctrl Pts',(-4.51778471765472,-0.230920834279876,
384.395547309813));
#28914=CARTESIAN_POINT('Ctrl Pts',(-4.50040387332536,-0.461706099887457,
384.403677922118));
#28915=CARTESIAN_POINT('Ctrl Pts',(-4.46518027924831,-0.689735200724739,
384.411808534423));
#28916=CARTESIAN_POINT('Ctrl Pts',(-4.35091384761331,-1.42946867609407,
384.43818449291));
#28917=CARTESIAN_POINT('Ctrl Pts',(-4.04887500627456,-2.14019699767394,
384.464560451397));
#28918=CARTESIAN_POINT('Ctrl Pts',(-3.59563057517656,-2.73587469379764,
384.490936409884));
#28919=CARTESIAN_POINT('Ctrl Pts',(-3.14238614407856,-3.33155238992132,
384.51731236837));
#28920=CARTESIAN_POINT('Ctrl Pts',(-2.53793612322135,-3.81217946058886,
384.543688326857));
#28921=CARTESIAN_POINT('Ctrl Pts',(-1.85545923021652,-4.11956801355568,
384.570064285343));
#28922=CARTESIAN_POINT('Ctrl Pts',(-1.17298233721168,-4.42695656652252,
384.59644024383));
#28923=CARTESIAN_POINT('Ctrl Pts',(-0.412478572059261,-4.56110660178858,
384.622816202316));
#28924=CARTESIAN_POINT('Ctrl Pts',(0.333980449139521,-4.50577702875979,
384.649192160803));
#28925=CARTESIAN_POINT('Ctrl Pts',(1.08043947033828,-4.450447455731,384.67556811929));
#28926=CARTESIAN_POINT('Ctrl Pts',(1.81285374758341,-4.20563827440736,384.701944077776));
#28927=CARTESIAN_POINT('Ctrl Pts',(2.44255236397545,-3.80098770355085,384.728320036263));
#28928=CARTESIAN_POINT('Ctrl Pts',(3.0722509803675,-3.39633713269433,384.754695994749));
#28929=CARTESIAN_POINT('Ctrl Pts',(3.59923393590646,-2.83184517230493,384.781071953236));
#28930=CARTESIAN_POINT('Ctrl Pts',(3.95970118830781,-2.17585295289468,384.807447911723));
#28931=CARTESIAN_POINT('Ctrl Pts',(4.32016844070917,-1.51986073348444,384.833823870209));
#28932=CARTESIAN_POINT('Ctrl Pts',(4.51411998997293,-0.772368255053362,
384.860199828696));
#28933=CARTESIAN_POINT('Ctrl Pts',(4.51807477866807,-0.023871901270034,
384.886575787182));
#28934=CARTESIAN_POINT('Ctrl Pts',(4.52202956736322,0.724624452513337,384.912951745669));
#28935=CARTESIAN_POINT('Ctrl Pts',(4.33598759548973,1.47412468164896,384.939327704155));
#28936=CARTESIAN_POINT('Ctrl Pts',(3.98247233472248,2.13388933088782,384.965703662642));
#28937=CARTESIAN_POINT('Ctrl Pts',(3.62895707395525,2.79365398012665,384.992079621129));
#28938=CARTESIAN_POINT('Ctrl Pts',(3.10796852429429,3.36368304946875,385.018455579615));
#28939=CARTESIAN_POINT('Ctrl Pts',(2.48258100559898,3.77496504936747,385.044831538102));
#28940=CARTESIAN_POINT('Ctrl Pts',(1.8571934869037,4.18624704926618,385.071207496588));
#28941=CARTESIAN_POINT('Ctrl Pts',(1.12740699917409,4.43878197972154,385.097583455075));
#28942=CARTESIAN_POINT('Ctrl Pts',(0.38157432172954,4.50199629168033,385.123959413562));
#28943=CARTESIAN_POINT('Ctrl Pts',(-0.364258355715052,4.56521060363914,
385.150335372048));
#28944=CARTESIAN_POINT('Ctrl Pts',(-1.12613722287458,4.43910429710136,385.176711330535));
#28945=CARTESIAN_POINT('Ctrl Pts',(-1.81182418470336,4.13894463565663,385.203087289021));
#28946=CARTESIAN_POINT('Ctrl Pts',(-2.49751114653216,3.8387849742119,385.229463247508));
#28947=CARTESIAN_POINT('Ctrl Pts',(-3.1070062030302,3.36457195786021,385.255839205995));
#28948=CARTESIAN_POINT('Ctrl Pts',(-3.56651985120111,2.7737169510055,385.282215164481));
#28949=CARTESIAN_POINT('Ctrl Pts',(-4.02603349937199,2.18286194415082,385.308591122968));
#28950=CARTESIAN_POINT('Ctrl Pts',(-4.33556573921576,1.47536494679312,385.334967081454));
#28951=CARTESIAN_POINT('Ctrl Pts',(-4.45764255040047,0.736880225115328,
385.361343039941));
#28952=CARTESIAN_POINT('Ctrl Pts',(-4.49786843733614,0.493539965571841,
385.37003425913));
#28953=CARTESIAN_POINT('Ctrl Pts',(-4.51774064501623,0.246835097138747,
385.378725478319));
#28954=CARTESIAN_POINT('Ctrl Pts',(-4.51754236316255,9.86160820556914E-5,
385.387416697508));
#28955=CARTESIAN_POINT('Origin',(0.,0.,387.));
#28956=CARTESIAN_POINT('',(-4.51812581071634,-2.54303748789628E-5,386.387416697508));
#28957=CARTESIAN_POINT('',(-4.51739693228094,4.16105383547416E-5,386.112583302492));
#28958=CARTESIAN_POINT('',(-4.51775,5.53264807684796E-16,387.));
#28959=CARTESIAN_POINT('Ctrl Pts',(-4.51739693228094,4.16105383547416E-5,
386.112583302492));
#28960=CARTESIAN_POINT('Ctrl Pts',(-4.51750350848484,0.328257645647765,
386.101023056451));
#28961=CARTESIAN_POINT('Ctrl Pts',(-4.48221658085224,0.656451107309221,
386.08946281041));
#28962=CARTESIAN_POINT('Ctrl Pts',(-4.41129467440341,0.976754228647579,
386.077902564369));
#28963=CARTESIAN_POINT('Ctrl Pts',(-4.24947863228365,1.70756063203963,386.051526605882));
#28964=CARTESIAN_POINT('Ctrl Pts',(-3.90215620987833,2.39729198722953,386.025150647396));
#28965=CARTESIAN_POINT('Ctrl Pts',(-3.41137655698045,2.96244485418463,385.998774688909));
#28966=CARTESIAN_POINT('Ctrl Pts',(-2.92059690408257,3.52759772113973,385.972398730423));
#28967=CARTESIAN_POINT('Ctrl Pts',(-2.28636002069214,3.96817209986003,385.946022771936));
#28968=CARTESIAN_POINT('Ctrl Pts',(-1.58545081902196,4.23082914191337,385.91964681345));
#28969=CARTESIAN_POINT('Ctrl Pts',(-0.884541617351764,4.49348618396671,
385.893270854963));
#28970=CARTESIAN_POINT('Ctrl Pts',(-0.116960097401826,4.57822588935307,
385.866894896476));
#28971=CARTESIAN_POINT('Ctrl Pts',(0.624365244915622,4.47478910883432,385.84051893799));
#28972=CARTESIAN_POINT('Ctrl Pts',(1.36569058723307,4.37135232831557,385.814142979503));
#28973=CARTESIAN_POINT('Ctrl Pts',(2.08075975191802,4.07973906189171,385.787767021017));
#28974=CARTESIAN_POINT('Ctrl Pts',(2.68300173612543,3.63525394044883,385.76139106253));
#28975=CARTESIAN_POINT('Ctrl Pts',(3.28524372033282,3.19076881900596,385.735015104043));
#28976=CARTESIAN_POINT('Ctrl Pts',(3.77465852406267,2.5934118425441,385.708639145557));
#28977=CARTESIAN_POINT('Ctrl Pts',(4.09199435398004,1.91550299780405,385.68226318707));
#28978=CARTESIAN_POINT('Ctrl Pts',(4.4093301838974,1.23759415306402,385.655887228584));
#28979=CARTESIAN_POINT('Ctrl Pts',(4.55458704000229,0.479133440045757,385.629511270097));
#28980=CARTESIAN_POINT('Ctrl Pts',(4.51017916650468,-0.268054870554405,
385.60313531161));
#28981=CARTESIAN_POINT('Ctrl Pts',(4.46577129300707,-1.01524318115463,385.576759353124));
#28982=CARTESIAN_POINT('Ctrl Pts',(4.23169868990694,-1.7511590893368,385.550383394637));
#28983=CARTESIAN_POINT('Ctrl Pts',(3.83629973479027,-2.38670774759897,385.524007436151));
#28984=CARTESIAN_POINT('Ctrl Pts',(3.44090077967361,-3.0222564058611,385.497631477664));
#28985=CARTESIAN_POINT('Ctrl Pts',(2.88417547254044,-3.55743781420323,385.471255519177));
#28986=CARTESIAN_POINT('Ctrl Pts',(2.23352466148768,-3.92745937141648,385.444879560691));
#28987=CARTESIAN_POINT('Ctrl Pts',(1.58287385043492,-4.29748092862973,385.418503602204));
#28988=CARTESIAN_POINT('Ctrl Pts',(0.838297535462584,-4.5023426347141,385.392127643717));
#28989=CARTESIAN_POINT('Ctrl Pts',(0.0899390502021953,-4.5172425764895,
385.365751685231));
#28990=CARTESIAN_POINT('Ctrl Pts',(-0.658419435058194,-4.53214251826491,
385.339375726744));
#28991=CARTESIAN_POINT('Ctrl Pts',(-1.41056009060662,-4.35708069573135,
385.312999768258));
#28992=CARTESIAN_POINT('Ctrl Pts',(-2.07542379370768,-4.01325125105728,
385.286623809771));
#28993=CARTESIAN_POINT('Ctrl Pts',(-2.74028749680876,-3.6694218063832,385.260247851285));
#28994=CARTESIAN_POINT('Ctrl Pts',(-3.31787424746246,-3.15682473956861,
385.233871892798));
#28995=CARTESIAN_POINT('Ctrl Pts',(-3.73825757323288,-2.53751844205472,
385.207495934311));
#28996=CARTESIAN_POINT('Ctrl Pts',(-4.15864089900331,-1.91821214454083,
385.181119975825));
#28997=CARTESIAN_POINT('Ctrl Pts',(-4.42182079989046,-1.19219661632765,
385.154744017338));
#28998=CARTESIAN_POINT('Ctrl Pts',(-4.49593497631034,-0.44736809943281,
385.128368058852));
#28999=CARTESIAN_POINT('Ctrl Pts',(-4.51071957921785,-0.298786621658729,
385.123106473398));
#29000=CARTESIAN_POINT('Ctrl Pts',(-4.51798051524647,-0.149456501261902,
385.117844887945));
#29001=CARTESIAN_POINT('Ctrl Pts',(-4.51782825948384,-0.000111641905798056,
385.112583302492));
#29002=CARTESIAN_POINT('Ctrl Pts',(-4.51754236316255,9.86160820556914E-5,
385.387416697508));
#29003=CARTESIAN_POINT('Ctrl Pts',(-4.51713890274882,-0.501956417601758,
385.405101436806));
#29004=CARTESIAN_POINT('Ctrl Pts',(-4.43363680853372,-1.00414233826904,
385.422786176103));
#29005=CARTESIAN_POINT('Ctrl Pts',(-4.26942186585053,-1.47837968895145,
385.440470915401));
#29006=CARTESIAN_POINT('Ctrl Pts',(-4.02450298759024,-2.18568243534247,
385.466846873887));
#29007=CARTESIAN_POINT('Ctrl Pts',(-3.60004384854402,-2.83081548212662,
385.493222832374));
#29008=CARTESIAN_POINT('Ctrl Pts',(-3.04743227963612,-3.33567475547881,
385.519598790861));
#29009=CARTESIAN_POINT('Ctrl Pts',(-2.49482071072822,-3.84053402883101,
385.545974749347));
#29010=CARTESIAN_POINT('Ctrl Pts',(-1.81405671195863,-4.20511952875126,
385.572350707834));
#29011=CARTESIAN_POINT('Ctrl Pts',(-1.0875580758779,-4.38529212309734,385.59872666632));
#29012=CARTESIAN_POINT('Ctrl Pts',(-0.361059439797152,-4.56546471744342,
385.625102624807));
#29013=CARTESIAN_POINT('Ctrl Pts',(0.411173833594756,-4.56122440621533,
385.651478583294));
#29014=CARTESIAN_POINT('Ctrl Pts',(1.13565007634523,-4.37308454953753,385.67785454178));
#29015=CARTESIAN_POINT('Ctrl Pts',(1.86012631909569,-4.18494469285974,385.704230500267));
#29016=CARTESIAN_POINT('Ctrl Pts',(2.53684553120472,-3.81290529073225,385.730606458753));
#29017=CARTESIAN_POINT('Ctrl Pts',(3.08387960874885,-3.30200789400175,385.75698241724));
#29018=CARTESIAN_POINT('Ctrl Pts',(3.63091368629297,-2.79111049727125,385.783358375726));
#29019=CARTESIAN_POINT('Ctrl Pts',(4.04826262927219,-2.14135510593772,385.809734334213));
#29020=CARTESIAN_POINT('Ctrl Pts',(4.28539941412795,-1.43140540543153,385.8361102927));
#29021=CARTESIAN_POINT('Ctrl Pts',(4.52253619898372,-0.721455704925321,
385.862486251186));
#29022=CARTESIAN_POINT('Ctrl Pts',(4.57946082571602,0.048688304753508,385.888862209673));
#29023=CARTESIAN_POINT('Ctrl Pts',(4.44928162248921,0.785787895736858,385.915238168159));
#29024=CARTESIAN_POINT('Ctrl Pts',(4.31910241926241,1.52288748672023,385.941614126646));
#29025=CARTESIAN_POINT('Ctrl Pts',(4.00181938607647,2.22694265900807,385.967990085133));
#29026=CARTESIAN_POINT('Ctrl Pts',(3.53584490557238,2.81271583652609,385.994366043619));
#29027=CARTESIAN_POINT('Ctrl Pts',(3.06987042506831,3.39848901404408,386.020742002106));
#29028=CARTESIAN_POINT('Ctrl Pts',(2.45520449724608,3.86598019679227,386.047117960592));
#29029=CARTESIAN_POINT('Ctrl Pts',(1.76626264498691,4.1585918100038,386.073493919079));
#29030=CARTESIAN_POINT('Ctrl Pts',(1.07732079272774,4.45120342321533,386.099869877566));
#29031=CARTESIAN_POINT('Ctrl Pts',(0.3141030160316,4.56893546689021,386.126245836052));
#29032=CARTESIAN_POINT('Ctrl Pts',(-0.43099049281119,4.49753452109188,386.152621794539));
#29033=CARTESIAN_POINT('Ctrl Pts',(-1.17608400165398,4.42613357529356,386.178997753025));
#29034=CARTESIAN_POINT('Ctrl Pts',(-1.90305324264344,4.16559964002203,386.205373711512));
#29035=CARTESIAN_POINT('Ctrl Pts',(-2.52388651098497,3.74747467676233,386.231749669998));
#29036=CARTESIAN_POINT('Ctrl Pts',(-3.14471977932654,3.3293497135026,386.258125628485));
#29037=CARTESIAN_POINT('Ctrl Pts',(-3.65941707502018,2.75363372225468,386.284501586972));
#29038=CARTESIAN_POINT('Ctrl Pts',(-4.00566573902476,2.09002668894682,386.310877545458));
#29039=CARTESIAN_POINT('Ctrl Pts',(-4.34058663747219,1.44813002069409,386.336390596142));
#29040=CARTESIAN_POINT('Ctrl Pts',(-4.51790043884109,0.723999072118772,
386.361903646825));
#29041=CARTESIAN_POINT('Ctrl Pts',(-4.51812581071634,-2.54303748789628E-5,
386.387416697508));
#29042=CARTESIAN_POINT('Origin',(0.,0.,387.));
#29043=CARTESIAN_POINT('',(-4.51744020728156,-6.7888199640348E-5,387.387416697508));
#29044=CARTESIAN_POINT('',(-4.51807831563064,5.66723631286815E-5,387.112583302492));
#29045=CARTESIAN_POINT('',(-4.51775,5.53264807684796E-16,387.));
#29046=CARTESIAN_POINT('Ctrl Pts',(-4.51807831563064,5.66723631286815E-5,
387.112583302492));
#29047=CARTESIAN_POINT('Ctrl Pts',(-4.51811411951228,0.0569892498064094,
387.110577183443));
#29048=CARTESIAN_POINT('Ctrl Pts',(-4.51706018525489,0.113920500037806,
387.108571064395));
#29049=CARTESIAN_POINT('Ctrl Pts',(-4.51490790649659,0.170810197164546,
387.106564945346));
#29050=CARTESIAN_POINT('Ctrl Pts',(-4.4866102761939,0.918781904413813,387.08018898686));
#29051=CARTESIAN_POINT('Ctrl Pts',(-4.26844906050963,1.65957059993282,387.053813028373));
#29052=CARTESIAN_POINT('Ctrl Pts',(-3.88683629922459,2.30349150435396,387.027437069886));
#29053=CARTESIAN_POINT('Ctrl Pts',(-3.50522353793953,2.94741240877514,387.0010611114));
#29054=CARTESIAN_POINT('Ctrl Pts',(-2.96015923105368,3.49446552209844,386.974685152913));
#29055=CARTESIAN_POINT('Ctrl Pts',(-2.31763246884327,3.87842097598549,386.948309194426));
#29056=CARTESIAN_POINT('Ctrl Pts',(-1.67510570663291,4.26237642987252,386.92193323594));
#29057=CARTESIAN_POINT('Ctrl Pts',(-0.935116489098005,4.48323422432332,
386.895557277453));
#29058=CARTESIAN_POINT('Ctrl Pts',(-0.187252805513337,4.51425585389532,
386.869181318967));
#29059=CARTESIAN_POINT('Ctrl Pts',(0.560610878071331,4.54527748346732,386.84280536048));
#29060=CARTESIAN_POINT('Ctrl Pts',(1.31634902770576,4.38646294816051,386.816429401993));
#29061=CARTESIAN_POINT('Ctrl Pts',(1.98846698422516,4.05703938608529,386.790053443507));
#29062=CARTESIAN_POINT('Ctrl Pts',(2.66058494074455,3.72761582401007,386.76367748502));
#29063=CARTESIAN_POINT('Ctrl Pts',(3.2490827041489,3.22758323516643,386.737301526534));
#29064=CARTESIAN_POINT('Ctrl Pts',(3.68271284262869,2.6174788721857,386.710925568047));
#29065=CARTESIAN_POINT('Ctrl Pts',(4.1163429811085,2.00737450920494,386.684549609561));
#29066=CARTESIAN_POINT('Ctrl Pts',(4.39510549466373,1.28719837208709,386.658173651074));
#29067=CARTESIAN_POINT('Ctrl Pts',(4.48525154955086,0.544139747539571,386.631797692587));
#29068=CARTESIAN_POINT('Ctrl Pts',(4.57539760443799,-0.198918877007948,
386.605421734101));
#29069=CARTESIAN_POINT('Ctrl Pts',(4.47692720065701,-0.96485998898513,386.579045775614));
#29070=CARTESIAN_POINT('Ctrl Pts',(4.20176181661432,-1.66095369111926,386.552669817128));
#29071=CARTESIAN_POINT('Ctrl Pts',(3.92659643257165,-2.35704739325338,386.526293858641));
#29072=CARTESIAN_POINT('Ctrl Pts',(3.47473606826728,-2.98329368554445,386.499917900154));
#29073=CARTESIAN_POINT('Ctrl Pts',(2.90088592819845,-3.46387504959129,386.473541941668));
#29074=CARTESIAN_POINT('Ctrl Pts',(2.32703578812962,-3.94445641363812,386.447165983181));
#29075=CARTESIAN_POINT('Ctrl Pts',(1.63119587229633,-4.27937284944072,386.420790024695));
#29076=CARTESIAN_POINT('Ctrl Pts',(0.897609163487301,-4.4280771580026,386.394414066208));
#29077=CARTESIAN_POINT('Ctrl Pts',(0.164022454678273,-4.57678146656449,
386.368038107722));
#29078=CARTESIAN_POINT('Ctrl Pts',(-0.607311047106494,-4.53927364788568,
386.341662149235));
#29079=CARTESIAN_POINT('Ctrl Pts',(-1.32300860621665,-4.3200946465879,386.315286190748));
#29080=CARTESIAN_POINT('Ctrl Pts',(-2.03870616532682,-4.10091564529013,
386.288910232262));
#29081=CARTESIAN_POINT('Ctrl Pts',(-2.69876778176237,-3.7000654613734,386.262534273775));
#29082=CARTESIAN_POINT('Ctrl Pts',(-3.22328203031241,-3.16607366949443,
386.236158315289));
#29083=CARTESIAN_POINT('Ctrl Pts',(-3.74779627886247,-2.63208187761544,
386.209782356802));
#29084=CARTESIAN_POINT('Ctrl Pts',(-4.136763159527,-1.9649484777742,386.183406398315));
#29085=CARTESIAN_POINT('Ctrl Pts',(-4.34309176894218,-1.24544105205646,
386.157030439829));
#29086=CARTESIAN_POINT('Ctrl Pts',(-4.45898918165419,-0.84128454994014,
386.142214727383));
#29087=CARTESIAN_POINT('Ctrl Pts',(-4.51726034328579,-0.420602931019958,
386.127399014937));
#29088=CARTESIAN_POINT('Ctrl Pts',(-4.51739693228094,4.16105383547416E-5,
386.112583302492));
#29089=CARTESIAN_POINT('Ctrl Pts',(-4.51812581071634,-2.54303748789628E-5,
386.387416697508));
#29090=CARTESIAN_POINT('Ctrl Pts',(-4.51813343329163,-0.024513540432781,
386.388279605311));
#29091=CARTESIAN_POINT('Ctrl Pts',(-4.51793847697299,-0.049001528722538,
386.389142513115));
#29092=CARTESIAN_POINT('Ctrl Pts',(-4.51754018801501,-0.0734862094280138,
386.390005420918));
#29093=CARTESIAN_POINT('Ctrl Pts',(-4.50536594068517,-0.821893999127264,
386.416381379405));
#29094=CARTESIAN_POINT('Ctrl Pts',(-4.30321741370996,-1.56721150315799,
386.442757337891));
#29095=CARTESIAN_POINT('Ctrl Pts',(-3.9355680448604,-2.21920565463873,386.469133296378));
#29096=CARTESIAN_POINT('Ctrl Pts',(-3.56791867601083,-2.87119980611948,
386.495509254864));
#29097=CARTESIAN_POINT('Ctrl Pts',(-3.03476846528691,-3.42987060505022,
386.521885213351));
#29098=CARTESIAN_POINT('Ctrl Pts',(-2.40066410367865,-3.8275816692287,386.548261171838));
#29099=CARTESIAN_POINT('Ctrl Pts',(-1.76655974207041,-4.22529273340718,
386.574637130324));
#29100=CARTESIAN_POINT('Ctrl Pts',(-1.0315012295778,-4.46204406283341,386.601013088811));
#29101=CARTESIAN_POINT('Ctrl Pts',(-0.28447961170951,-4.50917297559413,
386.627389047297));
#29102=CARTESIAN_POINT('Ctrl Pts',(0.4625420061588,-4.55630188835485,386.653765005784));
#29103=CARTESIAN_POINT('Ctrl Pts',(1.22152672940277,-4.4138083844501,386.68014096427));
#29104=CARTESIAN_POINT('Ctrl Pts',(1.90058684718235,-4.09894366997453,386.706516922757));
#29105=CARTESIAN_POINT('Ctrl Pts',(2.57964696496189,-3.78407895549898,386.732892881244));
#29106=CARTESIAN_POINT('Ctrl Pts',(3.17878247727702,-3.29684303045261,386.75926883973));
#29107=CARTESIAN_POINT('Ctrl Pts',(3.62545807607245,-2.69622389870498,386.785644798217));
#29108=CARTESIAN_POINT('Ctrl Pts',(4.07213367486792,-2.0956047669573,386.812020756704));
#29109=CARTESIAN_POINT('Ctrl Pts',(4.3663493601437,-1.38160242850832,386.83839671519));
#29110=CARTESIAN_POINT('Ctrl Pts',(4.47248543497401,-0.64065872916252,386.864772673677));
#29111=CARTESIAN_POINT('Ctrl Pts',(4.57862150980431,0.10028497018324,386.891148632163));
#29112=CARTESIAN_POINT('Ctrl Pts',(4.49667797418915,0.868170030425805,386.91752459065));
#29113=CARTESIAN_POINT('Ctrl Pts',(4.23657545455911,1.57003120705739,386.943900549137));
#29114=CARTESIAN_POINT('Ctrl Pts',(3.97647293492907,2.27189238368897,386.970276507623));
#29115=CARTESIAN_POINT('Ctrl Pts',(3.53821143128416,2.90772967670955,386.99665246611));
#29116=CARTESIAN_POINT('Ctrl Pts',(2.97484978010159,3.40056441773073,387.023028424596));
#29117=CARTESIAN_POINT('Ctrl Pts',(2.41148812891902,3.8933991587519,387.049404383083));
#29118=CARTESIAN_POINT('Ctrl Pts',(1.72302633019879,4.24323134777366,387.07578034157));
#29119=CARTESIAN_POINT('Ctrl Pts',(0.992814123069943,4.40770798605575,387.102156300056));
#29120=CARTESIAN_POINT('Ctrl Pts',(0.262601915941074,4.57218462433785,387.128532258543));
#29121=CARTESIAN_POINT('Ctrl Pts',(-0.509360699596469,4.55130571188027,
387.154908217029));
#29122=CARTESIAN_POINT('Ctrl Pts',(-1.2296148232201,4.34759898792704,387.181284175516));
#29123=CARTESIAN_POINT('Ctrl Pts',(-1.94986894684372,4.14389226397381,387.207660134002));
#29124=CARTESIAN_POINT('Ctrl Pts',(-2.61841457855343,3.75735772852497,387.234036092489));
#29125=CARTESIAN_POINT('Ctrl Pts',(-3.15431316213248,3.23479180914392,387.260412050976));
#29126=CARTESIAN_POINT('Ctrl Pts',(-3.69021174571151,2.71222588976291,387.286788009462));
#29127=CARTESIAN_POINT('Ctrl Pts',(-4.09346328115986,2.05362858644968,387.313163967949));
#29128=CARTESIAN_POINT('Ctrl Pts',(-4.3152474703208,1.33873404498307,387.339539926435));
#29129=CARTESIAN_POINT('Ctrl Pts',(-4.4494392553304,0.906183036834296,387.355498850126));
#29130=CARTESIAN_POINT('Ctrl Pts',(-4.51719722678179,0.453022038514597,
387.371457773817));
#29131=CARTESIAN_POINT('Ctrl Pts',(-4.51744020728156,-6.7888199640348E-5,
387.387416697508));
#29132=CARTESIAN_POINT('Origin',(0.,0.,387.));
#29133=CARTESIAN_POINT('',(-4.51772665650122,0.000115440622527052,388.387416697508));
#29134=CARTESIAN_POINT('',(-4.51762944300479,-0.000110891096316518,388.112583302492));
#29135=CARTESIAN_POINT('',(-4.51775,5.53264807684796E-16,387.));
#29136=CARTESIAN_POINT('Ctrl Pts',(-4.51762944300479,-0.000110891096316518,
388.112583302492));
#29137=CARTESIAN_POINT('Ctrl Pts',(-4.51713192095981,0.534369387836516,
388.093755351949));
#29138=CARTESIAN_POINT('Ctrl Pts',(-4.42224443214638,1.0690216395804,388.074927401406));
#29139=CARTESIAN_POINT('Ctrl Pts',(-4.23657544981682,1.57003120529822,388.056099450863));
#29140=CARTESIAN_POINT('Ctrl Pts',(-3.97647293047822,2.27189238114416,388.029723492377));
#29141=CARTESIAN_POINT('Ctrl Pts',(-3.53821142732417,2.90772967345308,388.00334753389));
#29142=CARTESIAN_POINT('Ctrl Pts',(-2.97484977677246,3.40056441392273,387.976971575404));
#29143=CARTESIAN_POINT('Ctrl Pts',(-2.41148812622074,3.89339915439239,387.950595616917));
#29144=CARTESIAN_POINT('Ctrl Pts',(-1.72302632827134,4.24323134302276,387.924219658431));
#29145=CARTESIAN_POINT('Ctrl Pts',(-0.992814121960003,4.40770798112098,
387.897843699944));
#29146=CARTESIAN_POINT('Ctrl Pts',(-0.262601915648666,4.5721846192192,387.871467741457));
#29147=CARTESIAN_POINT('Ctrl Pts',(0.509360699024613,4.55130570678527,387.845091782971));
#29148=CARTESIAN_POINT('Ctrl Pts',(1.22961482184198,4.34759898306034,387.818715824484));
#29149=CARTESIAN_POINT('Ctrl Pts',(1.94986894465933,4.14389225933542,387.792339865998));
#29150=CARTESIAN_POINT('Ctrl Pts',(2.61841457562078,3.75735772431952,387.765963907511));
#29151=CARTESIAN_POINT('Ctrl Pts',(3.15431315860007,3.2347918055237,387.739587949024));
#29152=CARTESIAN_POINT('Ctrl Pts',(3.69021174157935,2.71222588672787,387.713211990538));
#29153=CARTESIAN_POINT('Ctrl Pts',(4.09346327657648,2.05362858415213,387.686836032051));
#29154=CARTESIAN_POINT('Ctrl Pts',(4.3152474654894,1.3387340434859,387.660460073565));
#29155=CARTESIAN_POINT('Ctrl Pts',(4.53703165440232,0.62383950281966,387.634084115078));
#29156=CARTESIAN_POINT('Ctrl Pts',(4.57734849723102,-0.147352275937061,
387.607708156591));
#29157=CARTESIAN_POINT('Ctrl Pts',(4.4313169703101,-0.881475715061101,387.581332198105));
#29158=CARTESIAN_POINT('Ctrl Pts',(4.28528544338918,-1.61559915418514,387.554956239618));
#29159=CARTESIAN_POINT('Ctrl Pts',(3.95290554671864,-2.3126542536765,387.528580281132));
#29160=CARTESIAN_POINT('Ctrl Pts',(3.47441738908987,-2.88825091257507,387.502204322645));
#29161=CARTESIAN_POINT('Ctrl Pts',(2.99592923146112,-3.46384757147362,387.475828364158));
#29162=CARTESIAN_POINT('Ctrl Pts',(2.37133281287417,-3.91798578977939,387.449452405672));
#29163=CARTESIAN_POINT('Ctrl Pts',(1.67624590710662,-4.19568459092305,387.423076447185));
#29164=CARTESIAN_POINT('Ctrl Pts',(0.981159001339069,-4.47338339206671,
387.396700488698));
#29165=CARTESIAN_POINT('Ctrl Pts',(0.215581608390928,-4.57464277604826,
387.370324530212));
#29166=CARTESIAN_POINT('Ctrl Pts',(-0.527800408696545,-4.48720361207072,
387.343948571725));
#29167=CARTESIAN_POINT('Ctrl Pts',(-1.27118242578404,-4.39976444809319,
387.317572613239));
#29168=CARTESIAN_POINT('Ctrl Pts',(-1.99236906701087,-4.12362673615656,
387.291196654752));
#29169=CARTESIAN_POINT('Ctrl Pts',(-2.60404870735825,-3.69222153415889,
387.264820696266));
#29170=CARTESIAN_POINT('Ctrl Pts',(-3.21572834770564,-3.26081633216121,
387.238444737779));
#29171=CARTESIAN_POINT('Ctrl Pts',(-3.71790098717359,-2.67414364010249,
387.212068779293));
#29172=CARTESIAN_POINT('Ctrl Pts',(-4.049770284447,-2.00322993458336,387.185692820806));
#29173=CARTESIAN_POINT('Ctrl Pts',(-4.35639806038402,-1.38334500078815,
387.161322981368));
#29174=CARTESIAN_POINT('Ctrl Pts',(-4.51764337890668,-0.691546237269266,
387.13695314193));
#29175=CARTESIAN_POINT('Ctrl Pts',(-4.51807831563064,5.66723631286815E-5,
387.112583302492));
#29176=CARTESIAN_POINT('Ctrl Pts',(-4.51744020728156,-6.7888199640348E-5,
387.387416697508));
#29177=CARTESIAN_POINT('Ctrl Pts',(-4.51759881047873,-0.295818004161051,
387.397833732304));
#29178=CARTESIAN_POINT('Ctrl Pts',(-4.48899129636465,-0.591537838638136,
387.408250767099));
#29179=CARTESIAN_POINT('Ctrl Pts',(-4.43131697527066,-0.881475716049439,
387.418667801895));
#29180=CARTESIAN_POINT('Ctrl Pts',(-4.28528544818601,-1.61559915599528,
387.445043760382));
#29181=CARTESIAN_POINT('Ctrl Pts',(-3.95290555114312,-2.31265425626688,
387.471419718868));
#29182=CARTESIAN_POINT('Ctrl Pts',(-3.47441739297849,-2.88825091580966,
387.497795677355));
#29183=CARTESIAN_POINT('Ctrl Pts',(-2.99592923481386,-3.46384757535244,
387.524171635842));
#29184=CARTESIAN_POINT('Ctrl Pts',(-2.37133281552749,-3.91798579416642,
387.550547594328));
#29185=CARTESIAN_POINT('Ctrl Pts',(-1.67624590898167,-4.19568459562072,
387.576923552815));
#29186=CARTESIAN_POINT('Ctrl Pts',(-0.981159002435877,-4.47338339707502,
387.603299511301));
#29187=CARTESIAN_POINT('Ctrl Pts',(-0.215581608630632,-4.57464278116965,
387.629675469788));
#29188=CARTESIAN_POINT('Ctrl Pts',(0.527800409289026,-4.48720361709396,
387.656051428274));
#29189=CARTESIAN_POINT('Ctrl Pts',(1.27118242720868,-4.39976445301828,387.682427386761));
#29190=CARTESIAN_POINT('Ctrl Pts',(1.99236906924277,-4.12362674077227,387.708803345248));
#29191=CARTESIAN_POINT('Ctrl Pts',(2.60404871027476,-3.69222153829144,387.735179303734));
#29192=CARTESIAN_POINT('Ctrl Pts',(3.21572835130679,-3.26081633581058,387.761555262221));
#29193=CARTESIAN_POINT('Ctrl Pts',(3.71790099133673,-2.67414364309488,387.787931220707));
#29194=CARTESIAN_POINT('Ctrl Pts',(4.04977028898144,-2.00322993682453,387.814307179194));
#29195=CARTESIAN_POINT('Ctrl Pts',(4.38163958662613,-1.33231623055421,387.840683137681));
#29196=CARTESIAN_POINT('Ctrl Pts',(4.54320554188561,-0.577161510729227,
387.867059096167));
#29197=CARTESIAN_POINT('Ctrl Pts',(4.51490791155097,0.170810197357385,387.893435054654));
#29198=CARTESIAN_POINT('Ctrl Pts',(4.48661028121633,0.918781905443997,387.919811013141));
#29199=CARTESIAN_POINT('Ctrl Pts',(4.26844906528759,1.65957060179219,387.946186971627));
#29200=CARTESIAN_POINT('Ctrl Pts',(3.88683630357511,2.30349150693406,387.972562930114));
#29201=CARTESIAN_POINT('Ctrl Pts',(3.50522354186264,2.94741241207594,387.9989388886));
#29202=CARTESIAN_POINT('Ctrl Pts',(2.96015923436644,3.49446552601145,388.025314847087));
#29203=CARTESIAN_POINT('Ctrl Pts',(2.31763247143664,3.87842098032811,388.051690805573));
#29204=CARTESIAN_POINT('Ctrl Pts',(1.67510570850681,4.2623764346448,388.07806676406));
#29205=CARTESIAN_POINT('Ctrl Pts',(0.935116490143367,4.48323422934263,388.104442722547));
#29206=CARTESIAN_POINT('Ctrl Pts',(0.187252805721414,4.5142558589491,388.130818681033));
#29207=CARTESIAN_POINT('Ctrl Pts',(-0.560610878700497,4.54527748855557,
388.15719463952));
#29208=CARTESIAN_POINT('Ctrl Pts',(-1.31634902918093,4.38646295307071,388.183570598006));
#29209=CARTESIAN_POINT('Ctrl Pts',(-1.98846698645264,4.05703939062647,388.209946556493));
#29210=CARTESIAN_POINT('Ctrl Pts',(-2.66058494372436,3.72761582818222,388.23632251498));
#29211=CARTESIAN_POINT('Ctrl Pts',(-3.24908270778736,3.22758323877859,388.262698473466));
#29212=CARTESIAN_POINT('Ctrl Pts',(-3.68271284675239,2.6174788751147,388.289074431953));
#29213=CARTESIAN_POINT('Ctrl Pts',(-4.11634298571743,2.00737451145079,388.315450390439));
#29214=CARTESIAN_POINT('Ctrl Pts',(-4.3951054995845,1.28719837352659,388.341826348926));
#29215=CARTESIAN_POINT('Ctrl Pts',(-4.48525155457229,0.544139748147192,
388.368202307413));
#29216=CARTESIAN_POINT('Ctrl Pts',(-4.50714145691119,0.363704999850856,
388.374607104111));
#29217=CARTESIAN_POINT('Ctrl Pts',(-4.51790959247399,0.181920986011914,
388.381011900809));
#29218=CARTESIAN_POINT('Ctrl Pts',(-4.51772665650122,0.000115440622527052,
388.387416697508));
#29219=CARTESIAN_POINT('Origin',(0.,0.,387.));
#29220=CARTESIAN_POINT('',(-4.51800421755028,-8.27334347235434E-5,389.387416697508));
#29221=CARTESIAN_POINT('',(-4.51750342669873,8.9713446903977E-5,389.112583302492));
#29222=CARTESIAN_POINT('',(-4.51775,5.53264807684796E-16,387.));
#29223=CARTESIAN_POINT('Ctrl Pts',(-4.51750342669873,8.9713446903977E-5,
389.112583302492));
#29224=CARTESIAN_POINT('Ctrl Pts',(-4.51769355714261,0.263372352578081,
389.103309478941));
#29225=CARTESIAN_POINT('Ctrl Pts',(-4.49505280568826,0.526622657629559,
389.094035655391));
#29226=CARTESIAN_POINT('Ctrl Pts',(-4.4492816175085,0.7857878948557,389.084761831841));
#29227=CARTESIAN_POINT('Ctrl Pts',(-4.31910241442768,1.52288748501391,389.058385873354));
#29228=CARTESIAN_POINT('Ctrl Pts',(-4.00181938159719,2.22694265651365,389.032009914867));
#29229=CARTESIAN_POINT('Ctrl Pts',(-3.53584490161497,2.81271583337604,389.005633956381));
#29230=CARTESIAN_POINT('Ctrl Pts',(-3.06987042163275,3.39848901023841,388.979257997894));
#29231=CARTESIAN_POINT('Ctrl Pts',(-2.45520449449881,3.86598019246346,388.952882039408));
#29232=CARTESIAN_POINT('Ctrl Pts',(-1.76626264301101,4.15859180534764,388.926506080921));
#29233=CARTESIAN_POINT('Ctrl Pts',(-1.07732079152318,4.45120341823184,388.900130122435));
#29234=CARTESIAN_POINT('Ctrl Pts',(-0.314103015681492,4.56893546177518,
388.873754163948));
#29235=CARTESIAN_POINT('Ctrl Pts',(0.430990492327212,4.49753451605703,388.847378205461));
#29236=CARTESIAN_POINT('Ctrl Pts',(1.1760840003359,4.42613357033888,388.821002246975));
#29237=CARTESIAN_POINT('Ctrl Pts',(1.90305324051159,4.16559963535927,388.794626288488));
#29238=CARTESIAN_POINT('Ctrl Pts',(2.52388650815824,3.74747467256786,388.768250330001));
#29239=CARTESIAN_POINT('Ctrl Pts',(3.14471977580489,3.32934970977646,388.741874371515));
#29240=CARTESIAN_POINT('Ctrl Pts',(3.65941707092249,2.75363371917326,388.715498413028));
#29241=CARTESIAN_POINT('Ctrl Pts',(4.00566573453967,2.09002668660847,388.689122454542));
#29242=CARTESIAN_POINT('Ctrl Pts',(4.35191439815685,1.42641965404367,388.662746496055));
#29243=CARTESIAN_POINT('Ctrl Pts',(4.52971443027359,0.67492157951728,388.636370537568));
#29244=CARTESIAN_POINT('Ctrl Pts',(4.51754018295765,-0.0734862093441271,
388.609994579082));
#29245=CARTESIAN_POINT('Ctrl Pts',(4.50536593564171,-0.821893998205556,
388.583618620595));
#29246=CARTESIAN_POINT('Ctrl Pts',(4.30321740889306,-1.567211501402,388.557242662109));
#29247=CARTESIAN_POINT('Ctrl Pts',(3.93556804045529,-2.21920565215297,388.530866703622));
#29248=CARTESIAN_POINT('Ctrl Pts',(3.56791867201753,-2.87119980290394,388.504490745136));
#29249=CARTESIAN_POINT('Ctrl Pts',(3.03476846189066,-3.42987060120944,388.478114786649));
#29250=CARTESIAN_POINT('Ctrl Pts',(2.40066410099242,-3.8275816649429,388.451738828162));
#29251=CARTESIAN_POINT('Ctrl Pts',(1.7665597400942,-4.22529272867635,388.425362869676));
#29252=CARTESIAN_POINT('Ctrl Pts',(1.03150122842463,-4.46204405783778,388.398986911189));
#29253=CARTESIAN_POINT('Ctrl Pts',(0.284479611392651,-4.509172970546,388.372610952703));
#29254=CARTESIAN_POINT('Ctrl Pts',(-0.462542005639328,-4.55630188325423,
388.346234994216));
#29255=CARTESIAN_POINT('Ctrl Pts',(-1.22152672803371,-4.41380837950926,
388.319859035729));
#29256=CARTESIAN_POINT('Ctrl Pts',(-1.90058684505317,-4.09894366538644,
388.293483077243));
#29257=CARTESIAN_POINT('Ctrl Pts',(-2.57964696207265,-3.78407895126361,
388.267107118756));
#29258=CARTESIAN_POINT('Ctrl Pts',(-3.17878247371721,-3.29684302676292,
388.24073116027));
#29259=CARTESIAN_POINT('Ctrl Pts',(-3.62545807201282,-2.6962238956878,388.214355201783));
#29260=CARTESIAN_POINT('Ctrl Pts',(-4.07213367030842,-2.09560476461269,
388.187979243296));
#29261=CARTESIAN_POINT('Ctrl Pts',(-4.36634935525508,-1.38160242696316,
388.16160328481));
#29262=CARTESIAN_POINT('Ctrl Pts',(-4.47248542996683,-0.640658728446904,
388.135227326323));
#29263=CARTESIAN_POINT('Ctrl Pts',(-4.50285839007941,-0.428622872948985,
388.127679318379));
#29264=CARTESIAN_POINT('Ctrl Pts',(-4.51782889648961,-0.2143807013974,388.120131310436));
#29265=CARTESIAN_POINT('Ctrl Pts',(-4.51762944300479,-0.000110891096316518,
388.112583302492));
#29266=CARTESIAN_POINT('Ctrl Pts',(-4.51772665650122,0.000115440622527052,
388.387416697508));
#29267=CARTESIAN_POINT('Ctrl Pts',(-4.51715623341347,-0.566782797039444,
388.407387859296));
#29268=CARTESIAN_POINT('Ctrl Pts',(-4.41010960182223,-1.13389038388221,
388.427359021084));
#29269=CARTESIAN_POINT('Ctrl Pts',(-4.20176182131765,-1.66095369298009,
388.447330182872));
#29270=CARTESIAN_POINT('Ctrl Pts',(-3.9265964369667,-2.35704739589339,388.473706141359));
#29271=CARTESIAN_POINT('Ctrl Pts',(-3.47473607215626,-2.9832936888854,388.500082099846));
#29272=CARTESIAN_POINT('Ctrl Pts',(-2.90088593144485,-3.46387505347005,
388.526458058332));
#29273=CARTESIAN_POINT('Ctrl Pts',(-2.32703579073342,-3.94445641805472,
388.552834016819));
#29274=CARTESIAN_POINT('Ctrl Pts',(-1.631195874121,-4.27937285423203,388.579209975305));
#29275=CARTESIAN_POINT('Ctrl Pts',(-0.897609164490652,-4.42807716296015,
388.605585933792));
#29276=CARTESIAN_POINT('Ctrl Pts',(-0.164022454860301,-4.57678147168827,
388.631961892278));
#29277=CARTESIAN_POINT('Ctrl Pts',(0.607311047787985,-4.53927365296719,
388.658337850765));
#29278=CARTESIAN_POINT('Ctrl Pts',(1.32300860769931,-4.32009465142378,388.684713809252));
#29279=CARTESIAN_POINT('Ctrl Pts',(2.03870616761062,-4.10091564988038,388.711089767738));
#29280=CARTESIAN_POINT('Ctrl Pts',(2.69876778478497,-3.70006546551466,388.737465726225));
#29281=CARTESIAN_POINT('Ctrl Pts',(3.22328203392201,-3.16607367303769,388.763841684711));
#29282=CARTESIAN_POINT('Ctrl Pts',(3.74779628305905,-2.63208188056073,388.790217643198));
#29283=CARTESIAN_POINT('Ctrl Pts',(4.13676316415879,-1.96494847997252,388.816593601685));
#29284=CARTESIAN_POINT('Ctrl Pts',(4.3430917738047,-1.24544105344924,388.842969560171));
#29285=CARTESIAN_POINT('Ctrl Pts',(4.54942038345061,-0.525933626925946,
388.869345518658));
#29286=CARTESIAN_POINT('Ctrl Pts',(4.57311072164268,0.245947825532416,388.895721477144));
#29287=CARTESIAN_POINT('Ctrl Pts',(4.41129467934152,0.976754229742574,388.922097435631));
#29288=CARTESIAN_POINT('Ctrl Pts',(4.24947863704035,1.70756063395273,388.948473394118));
#29289=CARTESIAN_POINT('Ctrl Pts',(3.90215621424595,2.39729198991468,388.974849352604));
#29290=CARTESIAN_POINT('Ctrl Pts',(3.41137656079843,2.96244485750231,389.001225311091));
#29291=CARTESIAN_POINT('Ctrl Pts',(2.92059690735092,3.52759772508993,389.027601269577));
#29292=CARTESIAN_POINT('Ctrl Pts',(2.2863600232503,3.96817210430322,389.053977228064));
#29293=CARTESIAN_POINT('Ctrl Pts',(1.58545082079536,4.23082914665035,389.08035318655));
#29294=CARTESIAN_POINT('Ctrl Pts',(0.88454161834042,4.49348618899748,389.106729145037));
#29295=CARTESIAN_POINT('Ctrl Pts',(0.116960097531164,4.57822589447844,389.133105103524));
#29296=CARTESIAN_POINT('Ctrl Pts',(-0.624365245616139,4.47478911384364,
389.15948106201));
#29297=CARTESIAN_POINT('Ctrl Pts',(-1.36569058876346,4.37135233320883,389.185857020497));
#29298=CARTESIAN_POINT('Ctrl Pts',(-2.08075975424883,4.07973906645826,389.212232978983));
#29299=CARTESIAN_POINT('Ctrl Pts',(-2.6830017391303,3.63525394451758,389.23860893747));
#29300=CARTESIAN_POINT('Ctrl Pts',(-3.28524372401176,3.19076882257689,389.264984895957));
#29301=CARTESIAN_POINT('Ctrl Pts',(-3.77465852828932,2.59341184544609,389.291360854443));
#29302=CARTESIAN_POINT('Ctrl Pts',(-4.09199435856171,1.91550299994699,389.31773681293));
#29303=CARTESIAN_POINT('Ctrl Pts',(-4.37143979921575,1.3185375205331,389.340963441123));
#29304=CARTESIAN_POINT('Ctrl Pts',(-4.51744597443699,0.659107802205375,
389.364190069315));
#29305=CARTESIAN_POINT('Ctrl Pts',(-4.51800421755028,-8.27334347235434E-5,
389.387416697508));
#29306=CARTESIAN_POINT('Origin',(0.,0.,387.));
#29307=CARTESIAN_POINT('',(-4.51737568732049,-1.26367906908009E-5,390.387416697508));
#29308=CARTESIAN_POINT('',(-4.51813713037119,-8.34916185418341E-6,390.112583302492));
#29309=CARTESIAN_POINT('',(-4.51775,5.53264807684796E-16,387.));
#29310=CARTESIAN_POINT('Ctrl Pts',(-4.5181365124173,-8.33583456870006E-6,
390.112583302492));
#29311=CARTESIAN_POINT('Ctrl Pts',(-4.51805642563476,0.740544543431,390.086487647447));
#29312=CARTESIAN_POINT('Ctrl Pts',(-4.33223070178982,1.48113615227849,390.060391992403));
#29313=CARTESIAN_POINT('Ctrl Pts',(-3.98247233026486,2.13388932849751,390.034296337358));
#29314=CARTESIAN_POINT('Ctrl Pts',(-3.62895706989363,2.79365397699786,390.007920378871));
#29315=CARTESIAN_POINT('Ctrl Pts',(-3.10796852081612,3.36368304570199,389.981544420385));
#29316=CARTESIAN_POINT('Ctrl Pts',(-2.48258100282108,3.7749650451405,389.955168461898));
#29317=CARTESIAN_POINT('Ctrl Pts',(-1.85719348482602,4.18624704457905,389.928792503412));
#29318=CARTESIAN_POINT('Ctrl Pts',(-1.12740699791342,4.43878197475195,389.902416544925));
#29319=CARTESIAN_POINT('Ctrl Pts',(-0.381574321303787,4.50199628664022,
389.876040586438));
#29320=CARTESIAN_POINT('Ctrl Pts',(0.364258355305801,4.56521059852849,389.849664627952));
#29321=CARTESIAN_POINT('Ctrl Pts',(1.12613722161242,4.43910429213214,389.823288669465));
#29322=CARTESIAN_POINT('Ctrl Pts',(1.81182418267365,4.13894463102368,389.796912710979));
#29323=CARTESIAN_POINT('Ctrl Pts',(2.49751114373488,3.83878496991522,389.770536752492));
#29324=CARTESIAN_POINT('Ctrl Pts',(3.10700619955072,3.36457195409465,389.744160794005));
#29325=CARTESIAN_POINT('Ctrl Pts',(3.56651984720739,2.7737169479016,389.717784835519));
#29326=CARTESIAN_POINT('Ctrl Pts',(4.02603349486408,2.18286194170853,389.691408877032));
#29327=CARTESIAN_POINT('Ctrl Pts',(4.33556573436158,1.47536494514296,389.665032918546));
#29328=CARTESIAN_POINT('Ctrl Pts',(4.45764254540988,0.736880224291923,389.638656960059));
#29329=CARTESIAN_POINT('Ctrl Pts',(4.57971935645818,-0.0016044965591186,
389.612281001572));
#29330=CARTESIAN_POINT('Ctrl Pts',(4.51434073905728,-0.77107694169564,389.585905043086));
#29331=CARTESIAN_POINT('Ctrl Pts',(4.26942186107142,-1.47837968729494,389.559529084599));
#29332=CARTESIAN_POINT('Ctrl Pts',(4.02450298308556,-2.18568243289422,389.533153126113));
#29333=CARTESIAN_POINT('Ctrl Pts',(3.60004384451474,-2.83081547895628,389.506777167626));
#29334=CARTESIAN_POINT('Ctrl Pts',(3.04743227622566,-3.33567475174347,389.480401209139));
#29335=CARTESIAN_POINT('Ctrl Pts',(2.49482070793658,-3.84053402453067,389.454025250653));
#29336=CARTESIAN_POINT('Ctrl Pts',(1.81405670992924,-4.205119524043,389.427649292166));
#29337=CARTESIAN_POINT('Ctrl Pts',(1.08755807466189,-4.38529211818763,389.40127333368));
#29338=CARTESIAN_POINT('Ctrl Pts',(0.361059439394515,-4.56546471233226,
389.374897375193));
#29339=CARTESIAN_POINT('Ctrl Pts',(-0.411173833132874,-4.56122440110918,
389.348521416706));
#29340=CARTESIAN_POINT('Ctrl Pts',(-1.13565007507237,-4.37308454464225,
389.32214545822));
#29341=CARTESIAN_POINT('Ctrl Pts',(-1.86012631701186,-4.18494468817533,
389.295769499733));
#29342=CARTESIAN_POINT('Ctrl Pts',(-2.53684552836345,-3.81290528646455,
389.269393541247));
#29343=CARTESIAN_POINT('Ctrl Pts',(-3.08387960529535,-3.30200789030617,
389.24301758276));
#29344=CARTESIAN_POINT('Ctrl Pts',(-3.63091368222724,-2.79111049414779,
389.216641624274));
#29345=CARTESIAN_POINT('Ctrl Pts',(-4.04826262473945,-2.14135510354181,
389.190265665787));
#29346=CARTESIAN_POINT('Ctrl Pts',(-4.28539940932997,-1.43140540383048,
389.1638897073));
#29347=CARTESIAN_POINT('Ctrl Pts',(-4.43915857188131,-0.971075002245244,
389.146787572364));
#29348=CARTESIAN_POINT('Ctrl Pts',(-4.51715280146967,-0.485437663288439,
389.129685437428));
#29349=CARTESIAN_POINT('Ctrl Pts',(-4.51750342669873,8.9713446903977E-5,
389.112583302492));
#29350=CARTESIAN_POINT('Ctrl Pts',(-4.51800421755028,-8.27334347235434E-5,
389.387416697508));
#29351=CARTESIAN_POINT('Ctrl Pts',(-4.51807991049777,-0.089463280026118,
389.390566027802));
#29352=CARTESIAN_POINT('Ctrl Pts',(-4.5154815404334,-0.178839429239229,
389.393715358096));
#29353=CARTESIAN_POINT('Ctrl Pts',(-4.51017917155373,-0.268054870856108,
389.39686468839));
#29354=CARTESIAN_POINT('Ctrl Pts',(-4.46577129800614,-1.01524318229275,
389.423240646876));
#29355=CARTESIAN_POINT('Ctrl Pts',(-4.23169869464373,-1.75115909129866,
389.449616605363));
#29356=CARTESIAN_POINT('Ctrl Pts',(-3.83629973908422,-2.38670775027215,
389.475992563849));
#29357=CARTESIAN_POINT('Ctrl Pts',(-3.4409007835247,-3.02225640924567,389.502368522336));
#29358=CARTESIAN_POINT('Ctrl Pts',(-2.88417547576807,-3.55743781818676,
389.528744480823));
#29359=CARTESIAN_POINT('Ctrl Pts',(-2.23352466398677,-3.92745937581404,
389.555120439309));
#29360=CARTESIAN_POINT('Ctrl Pts',(-1.58287385220546,-4.29748093344132,
389.581496397796));
#29361=CARTESIAN_POINT('Ctrl Pts',(-0.838297536399466,-4.50234263975477,
389.607872356282));
#29362=CARTESIAN_POINT('Ctrl Pts',(-0.0899390503012636,-4.51724258154659,
389.634248314769));
#29363=CARTESIAN_POINT('Ctrl Pts',(0.658419435796918,-4.53214252333841,
389.660624273256));
#29364=CARTESIAN_POINT('Ctrl Pts',(1.4105600921873,-4.3570807006086,389.687000231742));
#29365=CARTESIAN_POINT('Ctrl Pts',(2.07542379603256,-4.01325125554937,389.713376190229));
#29366=CARTESIAN_POINT('Ctrl Pts',(2.74028749987779,-3.66942181049016,389.739752148715));
#29367=CARTESIAN_POINT('Ctrl Pts',(3.31787425117789,-3.15682474310154,389.766128107202));
#29368=CARTESIAN_POINT('Ctrl Pts',(3.7382575774187,-2.53751844489424,389.792504065688));
#29369=CARTESIAN_POINT('Ctrl Pts',(4.15864090365956,-1.91821214668688,389.818880024175));
#29370=CARTESIAN_POINT('Ctrl Pts',(4.4218208048411,-1.19219661766082,389.845255982662));
#29371=CARTESIAN_POINT('Ctrl Pts',(4.4959349813437,-0.447368099932093,389.871631941148));
#29372=CARTESIAN_POINT('Ctrl Pts',(4.5700491578463,0.297460417796599,389.898007899635));
#29373=CARTESIAN_POINT('Ctrl Pts',(4.45509760966997,1.06110192422797,389.924383858122));
#29374=CARTESIAN_POINT('Ctrl Pts',(4.16499713157485,1.7511049275472,389.950759816608));
#29375=CARTESIAN_POINT('Ctrl Pts',(3.87489665347973,2.44110793086643,389.977135775095));
#29376=CARTESIAN_POINT('Ctrl Pts',(3.40964724546582,3.05747243107353,390.003511733581));
#29377=CARTESIAN_POINT('Ctrl Pts',(2.8255750782226,3.52557726487935,390.029887692068));
#29378=CARTESIAN_POINT('Ctrl Pts',(2.24150291097938,3.99368209868516,390.056263650554));
#29379=CARTESIAN_POINT('Ctrl Pts',(1.53860798450686,4.31352726608968,390.082639609041));
#29380=CARTESIAN_POINT('Ctrl Pts',(0.80198740784653,4.44639019553642,390.109015567528));
#29381=CARTESIAN_POINT('Ctrl Pts',(0.0653668311861832,4.57925312498317,
390.135391526014));
#29382=CARTESIAN_POINT('Ctrl Pts',(-0.704979395661959,4.52513381647212,
390.161767484501));
#29383=CARTESIAN_POINT('Ctrl Pts',(-1.41578806308163,4.2905843114595,390.188143442987));
#29384=CARTESIAN_POINT('Ctrl Pts',(-2.1265967305013,4.05603480644688,390.214519401474));
#29385=CARTESIAN_POINT('Ctrl Pts',(-2.7778678384925,3.64105510493269,390.240895359961));
#29386=CARTESIAN_POINT('Ctrl Pts',(-3.2907541989407,3.09588539443257,390.267271318447));
#29387=CARTESIAN_POINT('Ctrl Pts',(-3.8036405593889,2.55071568393247,390.293647276934));
#29388=CARTESIAN_POINT('Ctrl Pts',(-4.17814217229411,1.87535596444644,390.320023235421));
#29389=CARTESIAN_POINT('Ctrl Pts',(-4.36891939528681,1.15156975072878,390.346399193907));
#29390=CARTESIAN_POINT('Ctrl Pts',(-4.46781255254173,0.776380811874881,
390.360071695107));
#29391=CARTESIAN_POINT('Ctrl Pts',(-4.51733762799004,0.388179321285348,
390.373744196308));
#29392=CARTESIAN_POINT('Ctrl Pts',(-4.51737568732049,-1.26367906908009E-5,
390.387416697508));
#29393=CARTESIAN_POINT('Origin',(0.,0.,387.));
#29394=CARTESIAN_POINT('',(-4.51792755410097,9.93894350090341E-5,391.387416697508));
#29395=CARTESIAN_POINT('',(-4.51747010126728,-7.96701847477171E-5,391.112583302492));
#29396=CARTESIAN_POINT('',(-4.51775,5.53264807684796E-16,387.));
#29397=CARTESIAN_POINT('Ctrl Pts',(-4.51747010126728,-7.96701847477171E-5,
391.112583302492));
#29398=CARTESIAN_POINT('Ctrl Pts',(-4.51717195077355,0.469542077919004,
391.09604177444));
#29399=CARTESIAN_POINT('Ctrl Pts',(-4.44429158523714,0.939254240738123,
391.079500246387));
#29400=CARTESIAN_POINT('Ctrl Pts',(-4.30028579839415,1.38604169480228,391.062958718335));
#29401=CARTESIAN_POINT('Ctrl Pts',(-4.07066428800006,2.09845757944446,391.036582759848));
#29402=CARTESIAN_POINT('Ctrl Pts',(-3.66020460842122,2.75258681658163,391.010206801362));
#29403=CARTESIAN_POINT('Ctrl Pts',(-3.11859972342044,3.26923619408001,390.983830842875));
#29404=CARTESIAN_POINT('Ctrl Pts',(-2.57699483841966,3.78588557157838,390.957454884389));
#29405=CARTESIAN_POINT('Ctrl Pts',(-1.90424474799695,4.16505508943795,390.931078925902));
#29406=CARTESIAN_POINT('Ctrl Pts',(-1.181797027951,4.36083997783993,390.904702967415));
#29407=CARTESIAN_POINT('Ctrl Pts',(-0.459349307905077,4.55662486624191,
390.878327008929));
#29408=CARTESIAN_POINT('Ctrl Pts',(0.312796041764081,4.5690251251863,390.851951050442));
#29409=CARTESIAN_POINT('Ctrl Pts',(1.04115799773134,4.39653949730477,390.825575091955));
#29410=CARTESIAN_POINT('Ctrl Pts',(1.76951995369859,4.22405386942324,390.799199133469));
#29411=CARTESIAN_POINT('Ctrl Pts',(2.45409851596394,3.86668235471579,390.772823174982));
#29412=CARTESIAN_POINT('Ctrl Pts',(3.01201407568894,3.36769071255846,390.746447216496));
#29413=CARTESIAN_POINT('Ctrl Pts',(3.56992963541394,2.86869907040112,390.720071258009));
#29414=CARTESIAN_POINT('Ctrl Pts',(4.00118219259857,2.22808730079389,390.693695299523));
#29415=CARTESIAN_POINT('Ctrl Pts',(4.25356146018424,1.52341210184117,390.667319341036));
#29416=CARTESIAN_POINT('Ctrl Pts',(4.5059407277699,0.818736902888453,390.640943382549));
#29417=CARTESIAN_POINT('Ctrl Pts',(4.5794467057566,0.0499982745902433,390.614567424063));
#29418=CARTESIAN_POINT('Ctrl Pts',(4.46518027424979,-0.68973519995098,390.588191465576));
#29419=CARTESIAN_POINT('Ctrl Pts',(4.35091384274297,-1.42946867449225,390.56181550709));
#29420=CARTESIAN_POINT('Ctrl Pts',(4.04887500174263,-2.14019699527652,390.535439548603));
#29421=CARTESIAN_POINT('Ctrl Pts',(3.59563057115222,-2.73587469073354,390.509063590117));
#29422=CARTESIAN_POINT('Ctrl Pts',(3.14238614056185,-3.33155238619052,390.48268763163));
#29423=CARTESIAN_POINT('Ctrl Pts',(2.53793612038144,-3.81217945632025,390.456311673143));
#29424=CARTESIAN_POINT('Ctrl Pts',(1.85545922814075,-4.11956800894318,390.429935714657));
#29425=CARTESIAN_POINT('Ctrl Pts',(1.17298233590006,-4.42695656156612,390.40355975617));
#29426=CARTESIAN_POINT('Ctrl Pts',(0.412478571599103,-4.56110659668227,
390.377183797684));
#29427=CARTESIAN_POINT('Ctrl Pts',(-0.333980448764015,-4.50577702371569,
390.350807839197));
#29428=CARTESIAN_POINT('Ctrl Pts',(-1.08043946912713,-4.45044745074911,
390.32443188071));
#29429=CARTESIAN_POINT('Ctrl Pts',(-1.81285374555241,-4.2056382696998,390.298055922224));
#29430=CARTESIAN_POINT('Ctrl Pts',(-2.44255236123965,-3.80098769929651,
390.271679963737));
#29431=CARTESIAN_POINT('Ctrl Pts',(-3.07225097692695,-3.39633712889319,
390.245304005251));
#29432=CARTESIAN_POINT('Ctrl Pts',(-3.59923393187618,-2.83184516913586,
390.218928046764));
#29433=CARTESIAN_POINT('Ctrl Pts',(-3.95970118387424,-2.17585295046006,
390.192552088277));
#29434=CARTESIAN_POINT('Ctrl Pts',(-4.32016843587225,-1.51986073178434,
390.166176129791));
#29435=CARTESIAN_POINT('Ctrl Pts',(-4.51411998491911,-0.772368254190162,
390.139800171304));
#29436=CARTESIAN_POINT('Ctrl Pts',(-4.51807477361008,-0.0238719012447998,
390.113424212818));
#29437=CARTESIAN_POINT('Ctrl Pts',(-4.51811680206878,-0.0159174565147239,
390.113143909376));
#29438=CARTESIAN_POINT('Ctrl Pts',(-4.51813737266016,-0.00796289840890401,
390.112863605934));
#29439=CARTESIAN_POINT('Ctrl Pts',(-4.5181365124173,-8.33583456870006E-6,
390.112583302492));
#29440=CARTESIAN_POINT('Ctrl Pts',(-4.51737568732049,-1.26367906908009E-5,
390.387416697508));
#29441=CARTESIAN_POINT('Ctrl Pts',(-4.51741104918088,-0.360691336761726,
390.400120154794));
#29442=CARTESIAN_POINT('Ctrl Pts',(-4.47472562929359,-0.721361807575693,
390.412823612081));
#29443=CARTESIAN_POINT('Ctrl Pts',(-4.38922403190431,-1.07157919495506,
390.425527069367));
#29444=CARTESIAN_POINT('Ctrl Pts',(-4.2116986124489,-1.79872921897196,390.451903027853));
#29445=CARTESIAN_POINT('Ctrl Pts',(-3.84959494045787,-2.48081655905642,
390.47827898634));
#29446=CARTESIAN_POINT('Ctrl Pts',(-3.3467516815685,-3.03526321020521,390.504654944827));
#29447=CARTESIAN_POINT('Ctrl Pts',(-2.84390842267912,-3.589709861354,390.531030903313));
#29448=CARTESIAN_POINT('Ctrl Pts',(-2.2003255768914,-4.01651582356711,390.5574068618));
#29449=CARTESIAN_POINT('Ctrl Pts',(-1.49391954044408,-4.26400914398482,
390.583782820286));
#29450=CARTESIAN_POINT('Ctrl Pts',(-0.787513503996787,-4.51150246440253,
390.610158778773));
#29451=CARTESIAN_POINT('Ctrl Pts',(-0.018284276889904,-4.57968314302485,
390.636534737259));
#29452=CARTESIAN_POINT('Ctrl Pts',(0.720640162637278,-4.46029677592208,
390.662910695746));
#29453=CARTESIAN_POINT('Ctrl Pts',(1.45956460216448,-4.34091040881931,390.689286654233));
#29454=CARTESIAN_POINT('Ctrl Pts',(2.16818425411199,-4.03395699599143,390.715662612719));
#29455=CARTESIAN_POINT('Ctrl Pts',(2.76070893630653,-3.57659834791441,390.742038571206));
#29456=CARTESIAN_POINT('Ctrl Pts',(3.35323361850104,-3.11923969983741,390.768414529692));
#29457=CARTESIAN_POINT('Ctrl Pts',(3.8296633309426,-2.51147581651127,390.794790488179));
#29458=CARTESIAN_POINT('Ctrl Pts',(4.13231834133649,-1.82688661365747,390.821166446666));
#29459=CARTESIAN_POINT('Ctrl Pts',(4.43497335173039,-1.14229741080364,390.847542405152));
#29460=CARTESIAN_POINT('Ctrl Pts',(4.5638536600766,-0.380882888422163,390.873918363639));
#29461=CARTESIAN_POINT('Ctrl Pts',(4.50335616377816,0.365175075091525,390.900294322126));
#29462=CARTESIAN_POINT('Ctrl Pts',(4.44285866747971,1.11123303860522,390.926670280612));
#29463=CARTESIAN_POINT('Ctrl Pts',(4.1929833665366,1.84193444325112,390.953046239099));
#29464=CARTESIAN_POINT('Ctrl Pts',(3.78398181766136,2.46881574381626,390.979422197585));
#29465=CARTESIAN_POINT('Ctrl Pts',(3.37498026878612,3.0956970443814,391.005798156072));
#29466=CARTESIAN_POINT('Ctrl Pts',(2.80685247197875,3.61875824086581,391.032174114558));
#29467=CARTESIAN_POINT('Ctrl Pts',(2.14837973615702,3.97467408507625,391.058550073045));
#29468=CARTESIAN_POINT('Ctrl Pts',(1.48990700033531,4.33058992928668,391.084926031532));
#29469=CARTESIAN_POINT('Ctrl Pts',(0.74108932549923,4.51936042122317,391.111301990018));
#29470=CARTESIAN_POINT('Ctrl Pts',(-0.00741646764041988,4.51813175652443,
391.137677948505));
#29471=CARTESIAN_POINT('Ctrl Pts',(-0.75592226078007,4.51690309182569,391.164053906991));
#29472=CARTESIAN_POINT('Ctrl Pts',(-1.5041161722233,4.32567527049173,391.190429865478));
#29473=CARTESIAN_POINT('Ctrl Pts',(-2.16141689818149,3.96759959743449,391.216805823964));
#29474=CARTESIAN_POINT('Ctrl Pts',(-2.81871762413969,3.60952392437724,391.243181782451));
#29475=CARTESIAN_POINT('Ctrl Pts',(-3.38512516461286,3.0846003995967,391.269557740938));
#29476=CARTESIAN_POINT('Ctrl Pts',(-3.79206647629354,2.45637973706784,391.295933699424));
#29477=CARTESIAN_POINT('Ctrl Pts',(-4.19900778797422,1.82815907453898,391.322309657911));
#29478=CARTESIAN_POINT('Ctrl Pts',(-4.44648287086241,1.0966412742618,391.348685616397));
#29479=CARTESIAN_POINT('Ctrl Pts',(-4.50453075451936,0.350388719704337,
391.375061574884));
#29480=CARTESIAN_POINT('Ctrl Pts',(-4.51359442160846,0.233867939052437,
391.379179949092));
#29481=CARTESIAN_POINT('Ctrl Pts',(-4.51803983860459,0.116987923926286,
391.3832983233));
#29482=CARTESIAN_POINT('Ctrl Pts',(-4.51792755410097,9.93894350090341E-5,
391.387416697508));
#29483=CARTESIAN_POINT('Origin',(0.,0.,387.));
#29484=CARTESIAN_POINT('',(-4.51781275651133,-0.000112770352403077,392.387416697508));
#29485=CARTESIAN_POINT('',(-4.51767617872592,0.000114137193723671,392.112583302492));
#29486=CARTESIAN_POINT('',(-4.51775,5.53264807684796E-16,387.));
#29487=CARTESIAN_POINT('Ctrl Pts',(-4.51767617872592,0.000114137193723671,
392.112583302492));
#29488=CARTESIAN_POINT('Ctrl Pts',(-4.5178695555558,0.198463769522385,392.105595901432));
#29489=CARTESIAN_POINT('Ctrl Pts',(-4.5050469141142,0.396788584023774,392.098608500372));
#29490=CARTESIAN_POINT('Ctrl Pts',(-4.47900555811224,0.593362231693622,
392.091621099312));
#29491=CARTESIAN_POINT('Ctrl Pts',(-4.38070495693752,1.33538610094233,392.065245140825));
#29492=CARTESIAN_POINT('Ctrl Pts',(-4.0940505572316,2.05245754966054,392.038869182339));
#29493=CARTESIAN_POINT('Ctrl Pts',(-3.65374663667568,2.65776316525419,392.012493223852));
#29494=CARTESIAN_POINT('Ctrl Pts',(-3.21344271611974,3.26306878084786,391.986117265366));
#29495=CARTESIAN_POINT('Ctrl Pts',(-2.61948927471379,3.75660856331697,391.959741306879));
#29496=CARTESIAN_POINT('Ctrl Pts',(-1.94379424473237,4.07863132211605,391.933365348393));
#29497=CARTESIAN_POINT('Ctrl Pts',(-1.26809921475095,4.40065408091513,391.906989389906));
#29498=CARTESIAN_POINT('Ctrl Pts',(-0.510662596194056,4.55115981604418,
391.88061343142));
#29499=CARTESIAN_POINT('Ctrl Pts',(0.236815323891349,4.51192730770023,391.854237472933));
#29500=CARTESIAN_POINT('Ctrl Pts',(0.984293243976733,4.47269479935628,391.827861514446));
#29501=CARTESIAN_POINT('Ctrl Pts',(1.72181246559064,4.24372404753933,391.80148555596));
#29502=CARTESIAN_POINT('Ctrl Pts',(2.36008403350207,3.85273576597324,391.775109597473));
#29503=CARTESIAN_POINT('Ctrl Pts',(2.99835560141351,3.46174748440714,391.748733638986));
#29504=CARTESIAN_POINT('Ctrl Pts',(3.53737951562248,2.90874167309189,391.7223576805));
#29505=CARTESIAN_POINT('Ctrl Pts',(3.9118979757439,2.2606688733584,391.695981722013));
#29506=CARTESIAN_POINT('Ctrl Pts',(4.28641643586534,1.6125960736249,391.669605763527));
#29507=CARTESIAN_POINT('Ctrl Pts',(4.49642944189922,0.869456285473188,391.64322980504));
#29508=CARTESIAN_POINT('Ctrl Pts',(4.51651143022073,0.121218927096046,391.616853846553));
#29509=CARTESIAN_POINT('Ctrl Pts',(4.53659341854224,-0.627018431281127,
391.590477888067));
#29510=CARTESIAN_POINT('Ctrl Pts',(4.36674438915135,-1.3803533598837,391.56410192958));
#29511=CARTESIAN_POINT('Ctrl Pts',(4.02752738899906,-2.04758214938088,391.537725971094));
#29512=CARTESIAN_POINT('Ctrl Pts',(3.68831038884679,-2.71481093887802,391.511350012607));
#29513=CARTESIAN_POINT('Ctrl Pts',(3.17972541793314,-3.29593358926979,391.48497405412));
#29514=CARTESIAN_POINT('Ctrl Pts',(2.56334513683187,-3.72059554871007,391.458598095634));
#29515=CARTESIAN_POINT('Ctrl Pts',(1.94696485573061,-4.14525750815035,391.432222137147));
#29516=CARTESIAN_POINT('Ctrl Pts',(1.22278926444172,-4.41345877663913,391.405846178661));
#29517=CARTESIAN_POINT('Ctrl Pts',(0.478491850048684,-4.49272913461715,
391.379470220174));
#29518=CARTESIAN_POINT('Ctrl Pts',(-0.265805564344378,-4.57199949259517,
391.353094261688));
#29519=CARTESIAN_POINT('Ctrl Pts',(-1.03022480184161,-4.46233894006242,
391.326718303201));
#29520=CARTESIAN_POINT('Ctrl Pts',(-1.72222021336115,-4.17702370884953,
391.300342344714));
#29521=CARTESIAN_POINT('Ctrl Pts',(-2.41421562488067,-3.89170847763665,
391.273966386228));
#29522=CARTESIAN_POINT('Ctrl Pts',(-3.03378721042251,-3.43073856774365,
391.247590427741));
#29523=CARTESIAN_POINT('Ctrl Pts',(-3.50592553573386,-2.84992204551108,
391.221214469255));
#29524=CARTESIAN_POINT('Ctrl Pts',(-3.97806386104521,-2.26910552327851,
391.194838510768));
#29525=CARTESIAN_POINT('Ctrl Pts',(-4.30276892612607,-1.56844238870636,
391.168462552281));
#29526=CARTESIAN_POINT('Ctrl Pts',(-4.44072978806182,-0.83275955534669,
391.142086593795));
#29527=CARTESIAN_POINT('Ctrl Pts',(-4.4921693025746,-0.558455906816085,
391.13225216336));
#29528=CARTESIAN_POINT('Ctrl Pts',(-4.51764736060392,-0.279283767746957,
391.122417732926));
#29529=CARTESIAN_POINT('Ctrl Pts',(-4.51747010126728,-7.96701847477171E-5,
391.112583302492));
#29530=CARTESIAN_POINT('Ctrl Pts',(-4.51792755410097,9.93894350090341E-5,
391.387416697508));
#29531=CARTESIAN_POINT('Ctrl Pts',(-4.51732071711229,-0.631619894993005,
391.409674281787));
#29532=CARTESIAN_POINT('Ctrl Pts',(-4.38359173091614,-1.26358801454013,
391.431931866065));
#29533=CARTESIAN_POINT('Ctrl Pts',(-4.12629845673798,-1.84044304971073,
391.454189450344));
#29534=CARTESIAN_POINT('Ctrl Pts',(-3.82139759087395,-2.52403495573063,
391.48056540883));
#29535=CARTESIAN_POINT('Ctrl Pts',(-3.34297517472017,-3.13023145893271,
391.506941367317));
#29536=CARTESIAN_POINT('Ctrl Pts',(-2.74895219046335,-3.58564240100063,
391.533317325804));
#29537=CARTESIAN_POINT('Ctrl Pts',(-2.15492920620652,-4.04105334306855,
391.55969328429));
#29538=CARTESIAN_POINT('Ctrl Pts',(-1.44530565384664,-4.34567872400231,
391.586069242777));
#29539=CARTESIAN_POINT('Ctrl Pts',(-0.705993254381129,-4.46263858026562,
391.612445201263));
#29540=CARTESIAN_POINT('Ctrl Pts',(0.0333191450843864,-4.57959843652893,
391.63882115975));
#29541=CARTESIAN_POINT('Ctrl Pts',(0.802320391655539,-4.5088927681218,391.665197118237));
#29542=CARTESIAN_POINT('Ctrl Pts',(1.50791010792466,-4.25908167093864,391.691573076723));
#29543=CARTESIAN_POINT('Ctrl Pts',(2.21349982419377,-4.00927057375548,391.71794903521));
#29544=CARTESIAN_POINT('Ctrl Pts',(2.85567801016084,-3.58035404779628,391.744324993696));
#29545=CARTESIAN_POINT('Ctrl Pts',(3.35669832699602,-3.02425956472802,391.770700952183));
#29546=CARTESIAN_POINT('Ctrl Pts',(3.85771864383119,-2.46816508165977,391.79707691067));
#29547=CARTESIAN_POINT('Ctrl Pts',(4.21758109153447,-1.78489264148247,391.823452869156));
#29548=CARTESIAN_POINT('Ctrl Pts',(4.39271834190528,-1.05716372525534,391.849828827643));
#29549=CARTESIAN_POINT('Ctrl Pts',(4.56785559227609,-0.329434809028198,
391.876204786129));
#29550=CARTESIAN_POINT('Ctrl Pts',(4.55826764531442,0.442750583248765,391.902580744616));
#29551=CARTESIAN_POINT('Ctrl Pts',(4.36511528129817,1.16590658042746,391.928956703102));
#29552=CARTESIAN_POINT('Ctrl Pts',(4.17196291728192,1.88906257760614,391.955332661589));
#29553=CARTESIAN_POINT('Ctrl Pts',(3.79524613621108,2.56318917968655,391.981708620076));
#29554=CARTESIAN_POINT('Ctrl Pts',(3.28057276336538,3.10667216126389,392.008084578562));
#29555=CARTESIAN_POINT('Ctrl Pts',(2.76589939051967,3.65015514284124,392.034460537049));
#29556=CARTESIAN_POINT('Ctrl Pts',(2.11326942589908,4.0629945039155,392.060836495535));
#29557=CARTESIAN_POINT('Ctrl Pts',(1.40169456978973,4.29520918074182,392.087212454022));
#29558=CARTESIAN_POINT('Ctrl Pts',(0.690119713680387,4.52742385756813,392.113588412509));
#29559=CARTESIAN_POINT('Ctrl Pts',(-0.0804000339177079,4.57901385014649,
392.139964370995));
#29560=CARTESIAN_POINT('Ctrl Pts',(-0.816580455818562,4.44373333273746,
392.166340329482));
#29561=CARTESIAN_POINT('Ctrl Pts',(-1.55276087771942,4.30845281532842,392.192716287968));
#29562=CARTESIAN_POINT('Ctrl Pts',(-2.25460197392303,3.98630178793199,392.219092246455));
#29563=CARTESIAN_POINT('Ctrl Pts',(-2.83713421905071,3.51628198476719,392.245468204942));
#29564=CARTESIAN_POINT('Ctrl Pts',(-3.4196664641784,3.0462621816024,392.271844163428));
#29565=CARTESIAN_POINT('Ctrl Pts',(-3.88288985823016,2.42837360266924,392.298220121915));
#29566=CARTESIAN_POINT('Ctrl Pts',(-4.17072351316767,1.73742192630838,392.324596080401));
#29567=CARTESIAN_POINT('Ctrl Pts',(-4.3992382776818,1.18886668648237,392.345536286104));
#29568=CARTESIAN_POINT('Ctrl Pts',(-4.51720537865769,0.59425998006379,392.366476491806));
#29569=CARTESIAN_POINT('Ctrl Pts',(-4.51781275651133,-0.000112770352403077,
392.387416697508));
#29570=CARTESIAN_POINT('Origin',(0.,0.,387.));
#29571=CARTESIAN_POINT('',(-4.51740214664894,4.58334405226135E-5,393.387416697508));
#29572=CARTESIAN_POINT('',(-4.51804470017939,-7.02313581118758E-5,393.112583302492));
#29573=CARTESIAN_POINT('',(-4.51775,5.53264807684796E-16,387.));
#29574=CARTESIAN_POINT('Ctrl Pts',(-4.51804470017939,-7.02313581118758E-5,
393.112583302492));
#29575=CARTESIAN_POINT('Ctrl Pts',(-4.51753951069973,0.675637543377085,
393.088774069938));
#29576=CARTESIAN_POINT('Ctrl Pts',(-4.36387000533556,1.351567384844,393.064964837384));
#29577=CARTESIAN_POINT('Ctrl Pts',(-4.07071229568028,1.96032419089247,393.04115560483));
#29578=CARTESIAN_POINT('Ctrl Pts',(-3.74595106860983,2.63470729871608,393.014779646343));
#29579=CARTESIAN_POINT('Ctrl Pts',(-3.25000583346633,3.2266536908633,392.988403687856));
#29580=CARTESIAN_POINT('Ctrl Pts',(-2.64291900080672,3.66449842171826,392.96202772937));
#29581=CARTESIAN_POINT('Ctrl Pts',(-2.03583216814709,4.10234315257323,392.935651770883));
#29582=CARTESIAN_POINT('Ctrl Pts',(-1.31760373797134,4.38608622213596,392.909275812397));
#29583=CARTESIAN_POINT('Ctrl Pts',(-0.575187194701503,4.48137581760917,
392.88289985391));
#29584=CARTESIAN_POINT('Ctrl Pts',(0.167229348568301,4.57666541308236,392.856523895423));
#29585=CARTESIAN_POINT('Ctrl Pts',(0.933834004932164,4.48350153446603,392.830147936937));
#29586=CARTESIAN_POINT('Ctrl Pts',(1.63181654404497,4.21316321713056,392.80377197845));
#29587=CARTESIAN_POINT('Ctrl Pts',(2.32979908315777,3.94282489979509,392.777396019963));
#29588=CARTESIAN_POINT('Ctrl Pts',(2.95915950501951,3.49531214374047,392.751020061477));
#29589=CARTESIAN_POINT('Ctrl Pts',(3.44370327410501,2.92480380325231,392.72464410299));
#29590=CARTESIAN_POINT('Ctrl Pts',(3.92824704319053,2.35429546276414,392.698268144504));
#29591=CARTESIAN_POINT('Ctrl Pts',(4.26797415949979,1.66079153784243,392.671892186017));
#29592=CARTESIAN_POINT('Ctrl Pts',(4.42175501123433,0.928252200764915,392.64551622753));
#29593=CARTESIAN_POINT('Ctrl Pts',(4.57553586296886,0.195712863687411,392.619140269044));
#29594=CARTESIAN_POINT('Ctrl Pts',(4.54337045012868,-0.575861885545891,
392.592764310557));
#29595=CARTESIAN_POINT('Ctrl Pts',(4.32915293034778,-1.29306010427281,392.566388352071));
#29596=CARTESIAN_POINT('Ctrl Pts',(4.11493541056688,-2.01025832299973,392.540012393584));
#29597=CARTESIAN_POINT('Ctrl Pts',(3.71866578384527,-2.67308001122027,392.513636435098));
#29598=CARTESIAN_POINT('Ctrl Pts',(3.18831907228789,-3.20127959117695,392.487260476611));
#29599=CARTESIAN_POINT('Ctrl Pts',(2.65797236073051,-3.72947917113363,392.460884518124));
#29600=CARTESIAN_POINT('Ctrl Pts',(1.99354856433737,-4.12305664282645,392.434508559638));
#29601=CARTESIAN_POINT('Ctrl Pts',(1.27548722267832,-4.33436291424531,392.408132601151));
#29602=CARTESIAN_POINT('Ctrl Pts',(0.557425881019256,-4.54566918566418,
392.381756642665));
#29603=CARTESIAN_POINT('Ctrl Pts',(-0.214273005905716,-4.57470425680908,
392.355380684178));
#29604=CARTESIAN_POINT('Ctrl Pts',(-0.946182466504358,-4.41795294991702,
392.329004725691));
#29605=CARTESIAN_POINT('Ctrl Pts',(-1.678091927103,-4.26120164302497,392.302628767205));
#29606=CARTESIAN_POINT('Ctrl Pts',(-2.37021196137532,-3.91866395809597,
392.276252808718));
#29607=CARTESIAN_POINT('Ctrl Pts',(-2.93874993999921,-3.43180977295588,
392.249876850232));
#29608=CARTESIAN_POINT('Ctrl Pts',(-3.50728791862308,-2.9449555878158,392.223500891745));
#29609=CARTESIAN_POINT('Ctrl Pts',(-3.95224384159854,-2.31378490246464,
392.197124933258));
#29610=CARTESIAN_POINT('Ctrl Pts',(-4.21974840176451,-1.61471141489946,
392.170748974772));
#29611=CARTESIAN_POINT('Ctrl Pts',(-4.41638684920909,-1.1008333518145,392.151360417345));
#29612=CARTESIAN_POINT('Ctrl Pts',(-4.51713959899635,-0.550264065511563,
392.131971859919));
#29613=CARTESIAN_POINT('Ctrl Pts',(-4.51767617872592,0.000114137193723671,
392.112583302492));
#29614=CARTESIAN_POINT('Ctrl Pts',(-4.51781275651133,-0.000112770352403077,
392.387416697508));
#29615=CARTESIAN_POINT('Ctrl Pts',(-4.51797042238654,-0.154402722371687,
392.392852450292));
#29616=CARTESIAN_POINT('Ctrl Pts',(-4.51021990758361,-0.308676909473601,
392.398288203077));
#29617=CARTESIAN_POINT('Ctrl Pts',(-4.49444205643657,-0.462125713027313,
392.403723955861));
#29618=CARTESIAN_POINT('Ctrl Pts',(-4.41788302894468,-1.20670690221361,
392.430099914348));
#29619=CARTESIAN_POINT('Ctrl Pts',(-4.15232105813761,-1.93185450679764,
392.456475872834));
#29620=CARTESIAN_POINT('Ctrl Pts',(-3.72990683273987,-2.54977736133712,
392.482851831321));
#29621=CARTESIAN_POINT('Ctrl Pts',(-3.30749260734213,-3.16770021587658,
392.509227789807));
#29622=CARTESIAN_POINT('Ctrl Pts',(-2.72822612735372,-3.67839832037151,
392.535603748294));
#29623=CARTESIAN_POINT('Ctrl Pts',(-2.06223722435424,-4.02004318431961,
392.561979706781));
#29624=CARTESIAN_POINT('Ctrl Pts',(-1.39624832135474,-4.36168804826772,
392.588355665267));
#29625=CARTESIAN_POINT('Ctrl Pts',(-0.643536995344169,-4.53427967166901,
392.614731623754));
#29626=CARTESIAN_POINT('Ctrl Pts',(0.10476854180126,-4.5169229710009,392.64110758224));
#29627=CARTESIAN_POINT('Ctrl Pts',(0.853074078946657,-4.4995662703328,392.667483540727));
#29628=CARTESIAN_POINT('Ctrl Pts',(1.59697382722691,-4.29226124559533,392.693859499214));
#29629=CARTESIAN_POINT('Ctrl Pts',(2.24640636264933,-3.92010561428585,392.7202354577));
#29630=CARTESIAN_POINT('Ctrl Pts',(2.89583889807178,-3.54794998297635,392.746611416187));
#29631=CARTESIAN_POINT('Ctrl Pts',(3.45080422063637,-3.01094374509482,392.772987374673));
#29632=CARTESIAN_POINT('Ctrl Pts',(3.84411455761933,-2.37410042778438,392.79936333316));
#29633=CARTESIAN_POINT('Ctrl Pts',(4.23742489460227,-1.73725711047397,392.825739291647));
#29634=CARTESIAN_POINT('Ctrl Pts',(4.46908024600357,-1.00057671373466,392.852115250133));
#29635=CARTESIAN_POINT('Ctrl Pts',(4.51103488271665,-0.253246639109774,
392.87849120862));
#29636=CARTESIAN_POINT('Ctrl Pts',(4.55298951942973,0.494083435515108,392.904867167106));
#29637=CARTESIAN_POINT('Ctrl Pts',(4.40524344145459,1.25206318802556,392.931243125593));
#29638=CARTESIAN_POINT('Ctrl Pts',(4.0856837662456,1.92892657598571,392.95761908408));
#29639=CARTESIAN_POINT('Ctrl Pts',(3.76612409103661,2.60578996394588,392.983995042566));
#29640=CARTESIAN_POINT('Ctrl Pts',(3.27475081859377,3.20153698735573,393.010371001053));
#29641=CARTESIAN_POINT('Ctrl Pts',(2.67105284742856,3.64404257103983,393.03674695954));
#29642=CARTESIAN_POINT('Ctrl Pts',(2.06735487626337,4.08654815472391,393.063122918026));
#29643=CARTESIAN_POINT('Ctrl Pts',(1.35133220637582,4.37581229868225,393.089498876512));
#29644=CARTESIAN_POINT('Ctrl Pts',(0.60967127825766,4.4768147723325,393.115874834999));
#29645=CARTESIAN_POINT('Ctrl Pts',(-0.131989649860521,4.57781724598275,
393.142250793486));
#29646=CARTESIAN_POINT('Ctrl Pts',(-0.89928883620931,4.49055804932491,393.168626751973));
#29647=CARTESIAN_POINT('Ctrl Pts',(-1.5993319660497,4.2256013578754,393.195002710459));
#29648=CARTESIAN_POINT('Ctrl Pts',(-2.29937509589006,3.9606446664259,393.221378668946));
#29649=CARTESIAN_POINT('Ctrl Pts',(-2.93216216922203,3.51799048018475,393.247754627432));
#29650=CARTESIAN_POINT('Ctrl Pts',(-3.42108379742811,2.95122944283932,393.274130585919));
#29651=CARTESIAN_POINT('Ctrl Pts',(-3.91000542563421,2.38446840549387,393.300506544405));
#29652=CARTESIAN_POINT('Ctrl Pts',(-4.25506160871441,1.69360051704413,393.326882502892));
#29653=CARTESIAN_POINT('Ctrl Pts',(-4.41447756279827,0.962266813756684,
393.353258461379));
#29654=CARTESIAN_POINT('Ctrl Pts',(-4.4832948761755,0.646561770734553,393.364644540088));
#29655=CARTESIAN_POINT('Ctrl Pts',(-4.51751793652066,0.323315880315216,
393.376030618798));
#29656=CARTESIAN_POINT('Ctrl Pts',(-4.51740214664894,4.58334405226135E-5,
393.387416697508));
#29657=CARTESIAN_POINT('Origin',(0.,0.,387.));
#29658=CARTESIAN_POINT('',(-4.51808751818987,5.21912322906659E-5,394.387416697508));
#29659=CARTESIAN_POINT('',(-4.5173836733729,-2.76243915998559E-5,394.112583302492));
#29660=CARTESIAN_POINT('',(-4.51775,5.53264807684796E-16,387.));
#29661=CARTESIAN_POINT('Ctrl Pts',(-4.5173836733729,-2.76243915998559E-5,
394.112583302492));
#29662=CARTESIAN_POINT('Ctrl Pts',(-4.51729674156455,0.40470368583773,394.09832819693));
#29663=CARTESIAN_POINT('Ctrl Pts',(-4.46340651421681,0.809457698610517,
394.084073091368));
#29664=CARTESIAN_POINT('Ctrl Pts',(-4.35600985269673,1.19947809100869,394.069817985807));
#29665=CARTESIAN_POINT('Ctrl Pts',(-4.15729579382325,1.92112561822137,394.04344202732));
#29666=CARTESIAN_POINT('Ctrl Pts',(-3.77540022477979,2.59233198125928,394.017066068833));
#29667=CARTESIAN_POINT('Ctrl Pts',(-3.2565579491727,3.13183649817179,393.990690110347));
#29668=CARTESIAN_POINT('Ctrl Pts',(-2.7377156735656,3.6713410150843,393.96431415186));
#29669=CARTESIAN_POINT('Ctrl Pts',(-2.08192669139488,4.0791436858714,393.937938193374));
#29670=CARTESIAN_POINT('Ctrl Pts',(-1.36858515450633,4.30587322182919,393.911562234887));
#29671=CARTESIAN_POINT('Ctrl Pts',(-0.655243617617784,4.53260275778698,
393.885186276401));
#29672=CARTESIAN_POINT('Ctrl Pts',(0.115650473988585,4.57825915891545,393.858810317914));
#29673=CARTESIAN_POINT('Ctrl Pts',(0.850767582565068,4.43731495930334,393.832434359427));
#29674=CARTESIAN_POINT('Ctrl Pts',(1.58588469114154,4.29637075969123,393.806058400941));
#29675=CARTESIAN_POINT('Ctrl Pts',(2.28522481668813,3.96882595933856,393.779682442454));
#29676=CARTESIAN_POINT('Ctrl Pts',(2.86412121787636,3.49433529829511,393.753306483967));
#29677=CARTESIAN_POINT('Ctrl Pts',(3.44301761906461,3.01984463725166,393.726930525481));
#29678=CARTESIAN_POINT('Ctrl Pts',(3.9014702958945,2.39840811551743,393.700554566994));
#29679=CARTESIAN_POINT('Ctrl Pts',(4.18397593491012,1.70526094885616,393.674178608508));
#29680=CARTESIAN_POINT('Ctrl Pts',(4.46648157392573,1.0121137821949,393.647802650021));
#29681=CARTESIAN_POINT('Ctrl Pts',(4.57304017512708,0.247255970606617,393.621426691535));
#29682=CARTESIAN_POINT('Ctrl Pts',(4.49075104942932,-0.496713740146479,
393.595050733048));
#29683=CARTESIAN_POINT('Ctrl Pts',(4.40846192373155,-1.24068345089957,393.568674774561));
#29684=CARTESIAN_POINT('Ctrl Pts',(4.13732507113467,-1.96376506081748,393.542298816075));
#29685=CARTESIAN_POINT('Ctrl Pts',(3.71016611242726,-2.57841752743756,393.515922857588));
#29686=CARTESIAN_POINT('Ctrl Pts',(3.28300715371985,-3.19306999405764,393.489546899101));
#29687=CARTESIAN_POINT('Ctrl Pts',(2.69982608890194,-3.69929331737988,393.463170940615));
#29688=CARTESIAN_POINT('Ctrl Pts',(2.03122667508525,-4.03580075350889,393.436794982129));
#29689=CARTESIAN_POINT('Ctrl Pts',(1.36262726126856,-4.37230818963791,393.410419023642));
#29690=CARTESIAN_POINT('Ctrl Pts',(0.60860949845307,-4.53909973857368,393.384043065155));
#29691=CARTESIAN_POINT('Ctrl Pts',(-0.139540235604001,-4.51598251217256,
393.357667106668));
#29692=CARTESIAN_POINT('Ctrl Pts',(-0.887689969661061,-4.49286528577144,
393.331291148182));
#29693=CARTESIAN_POINT('Ctrl Pts',(-1.62997167495974,-4.27983928403344,
393.304915189695));
#29694=CARTESIAN_POINT('Ctrl Pts',(-2.2765198184931,-3.90269484377256,393.278539231209));
#29695=CARTESIAN_POINT('Ctrl Pts',(-2.92306796202647,-3.52555040351167,
393.252163272722));
#29696=CARTESIAN_POINT('Ctrl Pts',(-3.47388254379453,-2.9842875247279,393.225787314236));
#29697=CARTESIAN_POINT('Ctrl Pts',(-3.86227830720905,-2.3444350716672,393.199411355749));
#29698=CARTESIAN_POINT('Ctrl Pts',(-4.25067407062357,-1.7045826186065,393.173035397262));
#29699=CARTESIAN_POINT('Ctrl Pts',(-4.47665101568456,-0.966140591268864,
393.146659438776));
#29700=CARTESIAN_POINT('Ctrl Pts',(-4.51285087871635,-0.218509665850027,
393.120283480289));
#29701=CARTESIAN_POINT('Ctrl Pts',(-4.51637359912257,-0.145755392857762,
393.117716754357));
#29702=CARTESIAN_POINT('Ctrl Pts',(-4.51809916152901,-0.0729141025000744,
393.115150028424));
#29703=CARTESIAN_POINT('Ctrl Pts',(-4.51804470017939,-7.02313581118758E-5,
393.112583302492));
#29704=CARTESIAN_POINT('Ctrl Pts',(-4.51740214664894,4.58334405226135E-5,
393.387416697508));
#29705=CARTESIAN_POINT('Ctrl Pts',(-4.51724970819312,-0.425542225591553,
393.402406577285));
#29706=CARTESIAN_POINT('Ctrl Pts',(-4.4575812765459,-0.851172152520294,
393.417396457061));
#29707=CARTESIAN_POINT('Ctrl Pts',(-4.33897962224013,-1.25969258594773,
393.432386336838));
#29708=CARTESIAN_POINT('Ctrl Pts',(-4.13029000251061,-1.97851876423963,
393.458762295325));
#29709=CARTESIAN_POINT('Ctrl Pts',(-3.73913503796403,-2.64437160269829,
393.485138253812));
#29710=CARTESIAN_POINT('Ctrl Pts',(-3.21287053587191,-3.1766385524691,393.511514212298));
#29711=CARTESIAN_POINT('Ctrl Pts',(-2.68660603377979,-3.7089055022399,393.537890170785));
#29712=CARTESIAN_POINT('Ctrl Pts',(-2.02523199414213,-4.10758656332286,
393.564266129271));
#29713=CARTESIAN_POINT('Ctrl Pts',(-1.3088187328036,-4.324414769419,393.590642087758));
#29714=CARTESIAN_POINT('Ctrl Pts',(-0.592405471465078,-4.54124297551514,
393.617018046244));
#29715=CARTESIAN_POINT('Ctrl Pts',(0.179047011574318,-4.57621832662447,
393.643394004731));
#29716=CARTESIAN_POINT('Ctrl Pts',(0.912141576006553,-4.42510647540001,
393.669769963218));
#29717=CARTESIAN_POINT('Ctrl Pts',(1.6452361404388,-4.27399462417554,393.696145921704));
#29718=CARTESIAN_POINT('Ctrl Pts',(2.33997278626389,-3.93679557061728,393.722521880191));
#29719=CARTESIAN_POINT('Ctrl Pts',(2.91224209985778,-3.45433286252538,393.748897838677));
#29720=CARTESIAN_POINT('Ctrl Pts',(3.48451141345166,-2.97187015443348,393.775273797164));
#29721=CARTESIAN_POINT('Ctrl Pts',(3.93431339481433,-2.34414379180799,393.801649755651));
#29722=CARTESIAN_POINT('Ctrl Pts',(4.20719204090252,-1.64715048015453,393.828025714137));
#29723=CARTESIAN_POINT('Ctrl Pts',(4.48007068699071,-0.950157168501087,
393.854401672624));
#29724=CARTESIAN_POINT('Ctrl Pts',(4.5760259978044,-0.183896907819673,393.88077763111));
#29725=CARTESIAN_POINT('Ctrl Pts',(4.48344098872769,0.558861766363823,393.907153589597));
#29726=CARTESIAN_POINT('Ctrl Pts',(4.39085597965098,1.30162044054734,393.933529548083));
#29727=CARTESIAN_POINT('Ctrl Pts',(4.10973065068387,2.02087752823294,393.95990550657));
#29728=CARTESIAN_POINT('Ctrl Pts',(3.67409989363231,2.62955500891649,393.986281465057));
#29729=CARTESIAN_POINT('Ctrl Pts',(3.23846913658077,3.23823248960003,394.012657423543));
#29730=CARTESIAN_POINT('Ctrl Pts',(2.64833295144478,3.73633036328149,394.03903338203));
#29731=CARTESIAN_POINT('Ctrl Pts',(1.97513712820591,4.06354560674411,394.065409340517));
#29732=CARTESIAN_POINT('Ctrl Pts',(1.30194130496704,4.39076085020672,394.091785299003));
#29733=CARTESIAN_POINT('Ctrl Pts',(0.54568584362529,4.54709346345051,394.11816125749));
#29734=CARTESIAN_POINT('Ctrl Pts',(-0.202071967477526,4.51361678626648,
394.144537215976));
#29735=CARTESIAN_POINT('Ctrl Pts',(-0.949829778580352,4.48014010908246,
394.170913174463));
#29736=CARTESIAN_POINT('Ctrl Pts',(-1.68908993944425,4.25685414147062,394.19728913295));
#29737=CARTESIAN_POINT('Ctrl Pts',(-2.33035272521732,3.8707913595774,394.223665091436));
#29738=CARTESIAN_POINT('Ctrl Pts',(-2.97161551099039,3.48472857768417,394.250041049923));
#29739=CARTESIAN_POINT('Ctrl Pts',(-3.51488092167263,2.93588898150954,394.276417008409));
#29740=CARTESIAN_POINT('Ctrl Pts',(-3.89437765326087,2.29071872282242,394.302792966896));
#29741=CARTESIAN_POINT('Ctrl Pts',(-4.27387438484911,1.64554846413529,394.329168925382));
#29742=CARTESIAN_POINT('Ctrl Pts',(-4.48960243734335,0.904047542935649,
394.355544883869));
#29743=CARTESIAN_POINT('Ctrl Pts',(-4.51544434579255,0.15598696534298,394.381920842355));
#29744=CARTESIAN_POINT('Ctrl Pts',(-4.51723920487186,0.104030147904069,
394.383752794073));
#29745=CARTESIAN_POINT('Ctrl Pts',(-4.51811804423603,0.0520416863733224,
394.38558474579));
#29746=CARTESIAN_POINT('Ctrl Pts',(-4.51808751818987,5.21912322906659E-5,
394.387416697508));
#29747=CARTESIAN_POINT('Origin',(0.,0.,387.));
#29748=CARTESIAN_POINT('',(-4.51761539860092,-0.000109498206778275,395.387416697508));
#29749=CARTESIAN_POINT('',(-4.51787769339044,0.000106674156513836,395.112583302492));
#29750=CARTESIAN_POINT('',(-4.51775,5.53264807684796E-16,387.));
#29751=CARTESIAN_POINT('Ctrl Pts',(-4.51787769339044,0.000106674156513836,
395.112583302492));
#29752=CARTESIAN_POINT('Ctrl Pts',(-4.51801115526906,0.13353505519604,395.107882323922));
#29753=CARTESIAN_POINT('Ctrl Pts',(-4.51221712826522,0.266951885784635,
395.103181345353));
#29754=CARTESIAN_POINT('Ctrl Pts',(-4.50041129427044,0.39983460330973,395.098480366784));
#29755=CARTESIAN_POINT('Ctrl Pts',(-4.43417185438628,1.14540469882723,395.072104408297));
#29756=CARTESIAN_POINT('Ctrl Pts',(-4.17867844925679,1.87416071243738,395.04572844981));
#29757=CARTESIAN_POINT('Ctrl Pts',(-3.76486280044783,2.49787462083366,395.019352491324));
#29758=CARTESIAN_POINT('Ctrl Pts',(-3.35104715163886,3.12158852922995,394.992976532837));
#29759=CARTESIAN_POINT('Ctrl Pts',(-2.77890925915041,3.64026033241238,394.966600574351));
#29760=CARTESIAN_POINT('Ctrl Pts',(-2.11771592060786,3.99109619117415,394.940224615864));
#29761=CARTESIAN_POINT('Ctrl Pts',(-1.45652258206532,4.34193204993591,394.913848657377));
#29762=CARTESIAN_POINT('Ctrl Pts',(-0.706273797468684,4.52493196427704,
394.887472698891));
#29763=CARTESIAN_POINT('Ctrl Pts',(0.0422003528576968,4.51794075412897,
394.861096740404));
#29764=CARTESIAN_POINT('Ctrl Pts',(0.790674503184078,4.51094954398091,394.834720781918));
#29765=CARTESIAN_POINT('Ctrl Pts',(1.5373740192402,4.31396720934364,394.808344823431));
#29766=CARTESIAN_POINT('Ctrl Pts',(2.19189851862757,3.9508417345724,394.781968864945));
#29767=CARTESIAN_POINT('Ctrl Pts',(2.84642301801496,3.58771625980115,394.755592906458));
#29768=CARTESIAN_POINT('Ctrl Pts',(3.4087725007336,3.05844764489591,394.729216947971));
#29769=CARTESIAN_POINT('Ctrl Pts',(3.81086521878951,2.4271126491824,394.702840989485));
#29770=CARTESIAN_POINT('Ctrl Pts',(4.2129579368454,1.79577765346891,394.676465030998));
#29771=CARTESIAN_POINT('Ctrl Pts',(4.45479389023857,1.06237627694715,394.650089072511));
#29772=CARTESIAN_POINT('Ctrl Pts',(4.50709481884649,0.315698941284091,394.623713114025));
#29773=CARTESIAN_POINT('Ctrl Pts',(4.55939574745442,-0.430978394378985,
394.597337155538));
#29774=CARTESIAN_POINT('Ctrl Pts',(4.4221616512771,-1.19093168918336,394.570961197052));
#29775=CARTESIAN_POINT('Ctrl Pts',(4.11200699772181,-1.8721559706092,394.544585238565));
#29776=CARTESIAN_POINT('Ctrl Pts',(3.80185234416652,-2.55338025203503,394.518209280079));
#29777=CARTESIAN_POINT('Ctrl Pts',(3.31877713323327,-3.15587552008233,394.491833321592));
#29778=CARTESIAN_POINT('Ctrl Pts',(2.72126564522031,-3.60669971244412,394.465457363105));
#29779=CARTESIAN_POINT('Ctrl Pts',(2.12375415720733,-4.05752390480593,394.439081404619));
#29780=CARTESIAN_POINT('Ctrl Pts',(1.41180639211463,-4.35667702148223,394.412705446132));
#29781=CARTESIAN_POINT('Ctrl Pts',(0.67161545550637,-4.46794160744361,394.386329487646));
#29782=CARTESIAN_POINT('Ctrl Pts',(-0.0685754811018632,-4.57920619340499,
394.359953529159));
#29783=CARTESIAN_POINT('Ctrl Pts',(-0.837009589225651,-4.50258224865146,
394.333577570673));
#29784=CARTESIAN_POINT('Ctrl Pts',(-1.54065515298906,-4.2473463747579,394.307201612186));
#29785=CARTESIAN_POINT('Ctrl Pts',(-2.24430071675247,-3.99211050086433,
394.280825653699));
#29786=CARTESIAN_POINT('Ctrl Pts',(-2.88315773615551,-3.55826269783073,
394.254449695213));
#29787=CARTESIAN_POINT('Ctrl Pts',(-3.37988195476012,-2.99832745034422,
394.228073736726));
#29788=CARTESIAN_POINT('Ctrl Pts',(-3.87660617336475,-2.43839220285771,
394.20169777824));
#29789=CARTESIAN_POINT('Ctrl Pts',(-4.23119759117096,-1.75236951091828,
394.175321819753));
#29790=CARTESIAN_POINT('Ctrl Pts',(-4.40072702572232,-1.02331381925484,
394.148945861266));
#29791=CARTESIAN_POINT('Ctrl Pts',(-4.47863287106505,-0.688282323920289,
394.136825008341));
#29792=CARTESIAN_POINT('Ctrl Pts',(-4.51745758988365,-0.34416318088334,
394.124704155417));
#29793=CARTESIAN_POINT('Ctrl Pts',(-4.5173836733729,-2.76243915998559E-5,
394.112583302492));
#29794=CARTESIAN_POINT('Ctrl Pts',(-4.51808751818987,5.21912322906659E-5,
394.387416697508));
#29795=CARTESIAN_POINT('Ctrl Pts',(-4.51767853826069,-0.696489376170657,
394.411960704277));
#29796=CARTESIAN_POINT('Ctrl Pts',(-4.35403905930357,-1.39321647594668,
394.436504711046));
#29797=CARTESIAN_POINT('Ctrl Pts',(-4.0431719192238,-2.01651441971212,394.461048717815));
#29798=CARTESIAN_POINT('Ctrl Pts',(-3.70910181980172,-2.68633499318885,
394.487424676302));
#29799=CARTESIAN_POINT('Ctrl Pts',(-3.20500585655341,-3.27135590615661,
394.513800634789));
#29800=CARTESIAN_POINT('Ctrl Pts',(-2.59191322109249,-3.70075065731708,
394.540176593275));
#29801=CARTESIAN_POINT('Ctrl Pts',(-1.97882058563158,-4.13014540847754,
394.566552551762));
#29802=CARTESIAN_POINT('Ctrl Pts',(-1.25673127795806,-4.40391399783071,
394.592928510249));
#29803=CARTESIAN_POINT('Ctrl Pts',(-0.513066205861354,-4.48891218912888,
394.619304468735));
#29804=CARTESIAN_POINT('Ctrl Pts',(0.230598866235364,-4.57391038042705,
394.645680427222));
#29805=CARTESIAN_POINT('Ctrl Pts',(0.995839702755266,-4.47013817367021,
394.672056385708));
#29806=CARTESIAN_POINT('Ctrl Pts',(1.69001118640443,-4.19015891860138,394.698432344195));
#29807=CARTESIAN_POINT('Ctrl Pts',(2.3841826700536,-3.91017966353254,394.724808302681));
#29808=CARTESIAN_POINT('Ctrl Pts',(3.00728480083202,-3.45399336015171,394.751184261168));
#29809=CARTESIAN_POINT('Ctrl Pts',(3.48388071332803,-2.87682893975429,394.777560219655));
#29810=CARTESIAN_POINT('Ctrl Pts',(3.96047662582402,-2.29966451935688,394.803936178141));
#29811=CARTESIAN_POINT('Ctrl Pts',(4.29056632003761,-1.6015219819429,394.830312136628));
#29812=CARTESIAN_POINT('Ctrl Pts',(4.43418695423518,-0.866923080900132,
394.856688095114));
#29813=CARTESIAN_POINT('Ctrl Pts',(4.57780758843275,-0.132324179857343,
394.883064053601));
#29814=CARTESIAN_POINT('Ctrl Pts',(4.5349591626143,0.638731084814249,394.909440012088));
#29815=CARTESIAN_POINT('Ctrl Pts',(4.31082919062693,1.35289366268957,394.935815970574));
#29816=CARTESIAN_POINT('Ctrl Pts',(4.08669921863955,2.06705624056489,394.962191929061));
#29817=CARTESIAN_POINT('Ctrl Pts',(3.68128770048325,2.72432613164396,394.988567887547));
#29818=CARTESIAN_POINT('Ctrl Pts',(3.14367643610836,3.24512989545316,395.014943846034));
#29819=CARTESIAN_POINT('Ctrl Pts',(2.60606517173349,3.76593365926234,395.04131980452));
#29820=CARTESIAN_POINT('Ctrl Pts',(1.93625416114004,4.15027129580166,395.067695763007));
#29821=CARTESIAN_POINT('Ctrl Pts',(1.21533515568228,4.35161234862086,395.094071721494));
#29822=CARTESIAN_POINT('Ctrl Pts',(0.494416150224501,4.55295340144005,395.12044767998));
#29823=CARTESIAN_POINT('Ctrl Pts',(-0.277610850097608,4.57129787053912,
395.146823638467));
#29824=CARTESIAN_POINT('Ctrl Pts',(-1.00727915011366,4.40442485315088,395.173199596953));
#29825=CARTESIAN_POINT('Ctrl Pts',(-1.73694745012971,4.23755183576263,395.19957555544));
#29826=CARTESIAN_POINT('Ctrl Pts',(-2.42425704983972,3.88546133188709,395.225951513927));
#29827=CARTESIAN_POINT('Ctrl Pts',(-2.98599770294795,3.39077974679813,395.252327472413));
#29828=CARTESIAN_POINT('Ctrl Pts',(-3.54773835605617,2.89609816170917,395.2787034309));
#29829=CARTESIAN_POINT('Ctrl Pts',(-3.9839100625626,2.25882549540681,395.305079389386));
#29830=CARTESIAN_POINT('Ctrl Pts',(-4.24170699065442,1.55611419206311,395.331455347873));
#29831=CARTESIAN_POINT('Ctrl Pts',(-4.42402787244154,1.05913796579184,395.350109131085));
#29832=CARTESIAN_POINT('Ctrl Pts',(-4.5171311009058,0.529431318295306,395.368762914296));
#29833=CARTESIAN_POINT('Ctrl Pts',(-4.51761539860092,-0.000109498206778275,
395.387416697508));
#29834=CARTESIAN_POINT('Origin',(0.,0.,387.));
#29835=CARTESIAN_POINT('',(-4.51751463264715,9.2546932777271E-5,396.387416697508));
#29836=CARTESIAN_POINT('',(-4.51786437784292,-0.000108222965875699,396.112583302492));
#29837=CARTESIAN_POINT('',(-4.51775,5.53264807684796E-16,387.));
#29838=CARTESIAN_POINT('Ctrl Pts',(-4.51786437784292,-0.000108222965875699,
396.112583302492));
#29839=CARTESIAN_POINT('Ctrl Pts',(-4.5172490555957,0.610781207776803,396.091060492428));
#29840=CARTESIAN_POINT('Ctrl Pts',(-4.39244234778488,1.22191440722307,396.069537682365));
#29841=CARTESIAN_POINT('Ctrl Pts',(-4.15139232023937,1.78311842878099,396.048014872301));
#29842=CARTESIAN_POINT('Ctrl Pts',(-3.85598825818002,2.47086756243728,396.021638913814));
#29843=CARTESIAN_POINT('Ctrl Pts',(-3.38600738379809,3.0836319422382,395.995262955328));
#29844=CARTESIAN_POINT('Ctrl Pts',(-2.79834869039748,3.54722625928365,395.968886996841));
#29845=CARTESIAN_POINT('Ctrl Pts',(-2.21068999699688,4.0108205763291,395.942511038355));
#29846=CARTESIAN_POINT('Ctrl Pts',(-1.50535348457759,4.32524483061908,395.916135079868));
#29847=CARTESIAN_POINT('Ctrl Pts',(-0.767731856725531,4.45243274219494,
395.889759121381));
#29848=CARTESIAN_POINT('Ctrl Pts',(-0.0301102288734742,4.5796206537708,
395.863383162895));
#29849=CARTESIAN_POINT('Ctrl Pts',(0.739796514411352,4.51957222263255,395.837007204408));
#29850=CARTESIAN_POINT('Ctrl Pts',(1.44877837029978,4.27955730903937,395.810631245922));
#29851=CARTESIAN_POINT('Ctrl Pts',(2.15776022618821,4.03954239544619,395.784255287435));
#29852=CARTESIAN_POINT('Ctrl Pts',(2.80581719468025,3.61956099939807,395.757879328948));
#29853=CARTESIAN_POINT('Ctrl Pts',(3.31449121264882,3.07045884663426,395.731503370462));
#29854=CARTESIAN_POINT('Ctrl Pts',(3.82316523061738,2.52135669387044,395.705127411975));
#29855=CARTESIAN_POINT('Ctrl Pts',(4.19245629806247,1.84313378439093,395.678751453489));
#29856=CARTESIAN_POINT('Ctrl Pts',(4.37765559571272,1.11790026966896,395.652375495002));
#29857=CARTESIAN_POINT('Ctrl Pts',(4.56285489336297,0.392666754946975,395.625999536516));
#29858=CARTESIAN_POINT('Ctrl Pts',(4.56396242121836,-0.379577365017472,
395.599623578029));
#29859=CARTESIAN_POINT('Ctrl Pts',(4.38084409463107,-1.10533910911399,395.573247619542));
#29860=CARTESIAN_POINT('Ctrl Pts',(4.19772576804378,-1.8311008532105,395.546871661056));
#29861=CARTESIAN_POINT('Ctrl Pts',(3.8303815870138,-2.51038022143909,395.520495702569));
#29862=CARTESIAN_POINT('Ctrl Pts',(3.32328466786559,-3.06093916044248,395.494119744083));
#29863=CARTESIAN_POINT('Ctrl Pts',(2.81618774871737,-3.61149809944587,395.467743785596));
#29864=CARTESIAN_POINT('Ctrl Pts',(2.16933809145092,-4.03333660922406,395.441367827109));
#29865=CARTESIAN_POINT('Ctrl Pts',(1.46104759411067,-4.27538412956593,395.414991868623));
#29866=CARTESIAN_POINT('Ctrl Pts',(0.75275709677042,-4.5174316499078,395.388615910136));
#29867=CARTESIAN_POINT('Ctrl Pts',(-0.0169742406436262,-4.57968818081335,
395.36223995165));
#29868=CARTESIAN_POINT('Ctrl Pts',(-0.754957651097232,-4.45461653486027,
395.335863993163));
#29869=CARTESIAN_POINT('Ctrl Pts',(-1.49294106155083,-4.3295448889072,395.309488034676));
#29870=CARTESIAN_POINT('Ctrl Pts',(-2.19917654504398,-4.01714506609549,
395.28311207619));
#29871=CARTESIAN_POINT('Ctrl Pts',(-2.78816256260641,-3.5552382553186,395.256736117703));
#29872=CARTESIAN_POINT('Ctrl Pts',(-3.37714858016886,-3.0933314445417,395.230360159217));
#29873=CARTESIAN_POINT('Ctrl Pts',(-3.84888513180058,-2.4819176457996,395.20398420073));
#29874=CARTESIAN_POINT('Ctrl Pts',(-4.14626067029702,-1.79501865771611,
395.177608242243));
#29875=CARTESIAN_POINT('Ctrl Pts',(-4.39063506253172,-1.23054545461321,
395.155933262326));
#29876=CARTESIAN_POINT('Ctrl Pts',(-4.51726233565243,-0.615096615266284,
395.134258282409));
#29877=CARTESIAN_POINT('Ctrl Pts',(-4.51787769339044,0.000106674156513836,
395.112583302492));
#29878=CARTESIAN_POINT('Ctrl Pts',(-4.51761539860092,-0.000109498206778275,
395.387416697508));
#29879=CARTESIAN_POINT('Ctrl Pts',(-4.51781588509979,-0.219325458522322,
395.395138872783));
#29880=CARTESIAN_POINT('Ctrl Pts',(-4.5021438757463,-0.438512999682626,
395.402861048058));
#29881=CARTESIAN_POINT('Ctrl Pts',(-4.47035806891458,-0.655338316442091,
395.410583223333));
#29882=CARTESIAN_POINT('Ctrl Pts',(-4.36179006940572,-1.39592958121857,
395.436959181819));
#29883=CARTESIAN_POINT('Ctrl Pts',(-4.06523192071081,-2.10896217038649,
395.463335140306));
#29884=CARTESIAN_POINT('Ctrl Pts',(-3.61658691387121,-2.70811164240368,
395.489711098793));
#29885=CARTESIAN_POINT('Ctrl Pts',(-3.16794190703161,-3.30726111442086,
395.516087057279));
#29886=CARTESIAN_POINT('Ctrl Pts',(-2.56721004204732,-3.79252746928731,
395.542463015766));
#29887=CARTESIAN_POINT('Ctrl Pts',(-1.88711989198663,-4.10516115232706,
395.568838974252));
#29888=CARTESIAN_POINT('Ctrl Pts',(-1.20702974192593,-4.4177948353668,395.595214932739));
#29889=CARTESIAN_POINT('Ctrl Pts',(-0.447581306788832,-4.55779584657986,
395.621590891225));
#29890=CARTESIAN_POINT('Ctrl Pts',(0.299281562555524,-4.50821473752317,
395.647966849712));
#29891=CARTESIAN_POINT('Ctrl Pts',(1.04614443189988,-4.45863362846649,395.674342808199));
#29892=CARTESIAN_POINT('Ctrl Pts',(1.78042173545149,-4.21947039914007,395.700718766685));
#29893=CARTESIAN_POINT('Ctrl Pts',(2.4132170060234,-3.81967973201239,395.727094725172));
#29894=CARTESIAN_POINT('Ctrl Pts',(3.04601227659532,-3.41988906488471,395.753470683659));
#29895=CARTESIAN_POINT('Ctrl Pts',(3.57732551418753,-2.85947095995576,395.779846642145));
#29896=CARTESIAN_POINT('Ctrl Pts',(3.94283242392784,-2.20627333984937,395.806222600631));
#29897=CARTESIAN_POINT('Ctrl Pts',(4.30833933366816,-1.55307571974297,395.832598559118));
#29898=CARTESIAN_POINT('Ctrl Pts',(4.50803991555659,-0.807098584459129,
395.858974517605));
#29899=CARTESIAN_POINT('Ctrl Pts',(4.51775709624605,-0.0586548602019053,
395.885350476092));
#29900=CARTESIAN_POINT('Ctrl Pts',(4.5274742769355,0.689788864055318,395.911726434578));
#29901=CARTESIAN_POINT('Ctrl Pts',(4.34720805642599,1.44069917728592,395.938102393065));
#29902=CARTESIAN_POINT('Ctrl Pts',(3.99878265572902,2.10316591013349,395.964478351551));
#29903=CARTESIAN_POINT('Ctrl Pts',(3.65035725503204,2.76563264298105,395.990854310038));
#29904=CARTESIAN_POINT('Ctrl Pts',(3.13377267414759,3.33965579544558,396.017230268524));
#29905=CARTESIAN_POINT('Ctrl Pts',(2.5115700593453,3.75574032785908,396.043606227011));
#29906=CARTESIAN_POINT('Ctrl Pts',(1.88936744454301,4.17182486027259,396.069982185498));
#29907=CARTESIAN_POINT('Ctrl Pts',(1.16154679582287,4.42997077263507,396.096358143984));
#29908=CARTESIAN_POINT('Ctrl Pts',(0.416222895030907,4.49892521331027,396.122734102471));
#29909=CARTESIAN_POINT('Ctrl Pts',(-0.329101005761055,4.56787965398547,
396.149110060957));
#29910=CARTESIAN_POINT('Ctrl Pts',(-1.09192815862484,4.44764262297338,396.175486019444));
#29911=CARTESIAN_POINT('Ctrl Pts',(-1.77990566277504,4.15277081054664,396.201861977931));
#29912=CARTESIAN_POINT('Ctrl Pts',(-2.46788316692524,3.85789899811989,396.228237936417));
#29913=CARTESIAN_POINT('Ctrl Pts',(-3.08101102236186,3.38839240427848,396.254613894904));
#29914=CARTESIAN_POINT('Ctrl Pts',(-3.54505991542016,2.80109260278699,396.28098985339));
#29915=CARTESIAN_POINT('Ctrl Pts',(-4.00910880847846,2.2137928012955,396.307365811877));
#29916=CARTESIAN_POINT('Ctrl Pts',(-4.32407873915844,1.50869979215393,396.333741770364));
#29917=CARTESIAN_POINT('Ctrl Pts',(-4.45183736430835,0.771176798830757,
396.36011772885));
#29918=CARTESIAN_POINT('Ctrl Pts',(-4.4959138504198,0.516732749092945,396.369217385069));
#29919=CARTESIAN_POINT('Ctrl Pts',(-4.51770775311255,0.258428762447222,
396.378317041289));
#29920=CARTESIAN_POINT('Ctrl Pts',(-4.51751463264715,9.2546932777271E-5,
396.387416697508));
#29921=CARTESIAN_POINT('Origin',(0.,0.,387.));
#29922=CARTESIAN_POINT('',(-4.51813440218219,-1.34914224690988E-5,397.387416697508));
#29923=CARTESIAN_POINT('',(-4.51738673749921,3.14726202902737E-5,397.112583302492));
#29924=CARTESIAN_POINT('',(-4.51775,5.53264807684796E-16,387.));
#29925=CARTESIAN_POINT('Ctrl Pts',(-4.51738673749921,3.14726202902737E-5,
397.112583302492));
#29926=CARTESIAN_POINT('Ctrl Pts',(-4.51746996308395,0.339845959287686,
397.100614619421));
#29927=CARTESIAN_POINT('Ctrl Pts',(-4.47962267703118,0.67964219695818,397.088645936349));
#29928=CARTESIAN_POINT('Ctrl Pts',(-4.40364412455734,1.01068687131693,397.076677253278));
#29929=CARTESIAN_POINT('Ctrl Pts',(-4.236206559874,1.7402258302897,397.050301294792));
#29930=CARTESIAN_POINT('Ctrl Pts',(-3.88358434036526,2.42726278544303,397.023925336305));
#29931=CARTESIAN_POINT('Ctrl Pts',(-3.38846824431658,2.9886204986346,396.997549377818));
#29932=CARTESIAN_POINT('Ctrl Pts',(-2.89335214826789,3.54997821182617,396.971173419332));
#29933=CARTESIAN_POINT('Ctrl Pts',(-2.25574217567927,3.98565668305597,396.944797460845));
#29934=CARTESIAN_POINT('Ctrl Pts',(-1.55283160725287,4.24290979483623,396.918421502359));
#29935=CARTESIAN_POINT('Ctrl Pts',(-0.849921038826476,4.5001629066165,396.892045543872));
#29936=CARTESIAN_POINT('Ctrl Pts',(-0.0817098745623172,4.57899065894722,
396.865669585385));
#29937=CARTESIAN_POINT('Ctrl Pts',(0.658797160721962,4.46984964273134,396.839293626899));
#29938=CARTESIAN_POINT('Ctrl Pts',(1.39930419600623,4.36070862651545,396.812917668412));
#29939=CARTESIAN_POINT('Ctrl Pts',(2.11210710231061,4.06359884175296,396.786541709925));
#29940=CARTESIAN_POINT('Ctrl Pts',(2.71090924501961,3.61449036419631,396.760165751439));
#29941=CARTESIAN_POINT('Ctrl Pts',(3.30971138772862,3.16538188663966,396.733789792952));
#29942=CARTESIAN_POINT('Ctrl Pts',(3.79451276684224,2.56427471628884,396.707413834466));
#29943=CARTESIAN_POINT('Ctrl Pts',(4.10662012072468,1.88394286316225,396.681037875979));
#29944=CARTESIAN_POINT('Ctrl Pts',(4.41872747460713,1.20361101003566,396.654661917493));
#29945=CARTESIAN_POINT('Ctrl Pts',(4.5581408032584,0.444054474133294,396.628285959006));
#29946=CARTESIAN_POINT('Ctrl Pts',(4.50798180697358,-0.302769806282027,
396.601910000519));
#29947=CARTESIAN_POINT('Ctrl Pts',(4.45782281068875,-1.04959408669733,396.575534042033));
#29948=CARTESIAN_POINT('Ctrl Pts',(4.21809148946783,-1.78368611162558,396.549158083546));
#29949=CARTESIAN_POINT('Ctrl Pts',(3.81781130274164,-2.41617184493549,396.52278212506));
#29950=CARTESIAN_POINT('Ctrl Pts',(3.41753111601545,-3.0486575782454,396.496406166573));
#29951=CARTESIAN_POINT('Ctrl Pts',(2.85670206378398,-3.57953701993697,396.470030208087));
#29952=CARTESIAN_POINT('Ctrl Pts',(2.20322182066968,-3.94453839333905,396.4436542496));
#29953=CARTESIAN_POINT('Ctrl Pts',(1.54974157755536,-4.30953976674113,396.417278291113));
#29954=CARTESIAN_POINT('Ctrl Pts',(0.803610143558188,-4.50866307185371,
396.390902332627));
#29955=CARTESIAN_POINT('Ctrl Pts',(0.0551591253050773,-4.51780112427455,
396.36452637414));
#29956=CARTESIAN_POINT('Ctrl Pts',(-0.693291892948023,-4.52693917669538,
396.338150415653));
#29957=CARTESIAN_POINT('Ctrl Pts',(-1.44406249545706,-4.34609197642448,
396.311774457167));
#29958=CARTESIAN_POINT('Ctrl Pts',(-2.10625942716968,-3.9971540817261,396.28539849868));
#29959=CARTESIAN_POINT('Ctrl Pts',(-2.7684563588823,-3.64821618702772,396.259022540194));
#29960=CARTESIAN_POINT('Ctrl Pts',(-3.3420796197985,-3.13118759790186,396.232646581707));
#29961=CARTESIAN_POINT('Ctrl Pts',(-3.7576825837662,-2.5086632151927,396.206270623221));
#29962=CARTESIAN_POINT('Ctrl Pts',(-4.17328554773389,-1.88613883248355,
396.179894664734));
#29963=CARTESIAN_POINT('Ctrl Pts',(-4.43086821475307,-1.15811865619109,
396.153518706247));
#29964=CARTESIAN_POINT('Ctrl Pts',(-4.49924592339428,-0.412741624289035,
396.127142747761));
#29965=CARTESIAN_POINT('Ctrl Pts',(-4.51182734935556,-0.275593039955457,
396.122289599338));
#29966=CARTESIAN_POINT('Ctrl Pts',(-4.51800312599824,-0.137856828684076,
396.117436450915));
#29967=CARTESIAN_POINT('Ctrl Pts',(-4.51786437784292,-0.000108222965875699,
396.112583302492));
#29968=CARTESIAN_POINT('Ctrl Pts',(-4.51751463264715,9.2546932777271E-5,
396.387416697508));
#29969=CARTESIAN_POINT('Ctrl Pts',(-4.51714798060515,-0.490375932126388,
396.404692999775));
#29970=CARTESIAN_POINT('Ctrl Pts',(-4.43752790145426,-0.98096058190497,
396.421969302042));
#29971=CARTESIAN_POINT('Ctrl Pts',(-4.28067705789975,-1.44546653343395,
396.43924560431));
#29972=CARTESIAN_POINT('Ctrl Pts',(-4.04121080672139,-2.1546338948707,396.465621562796));
#29973=CARTESIAN_POINT('Ctrl Pts',(-3.62173098474482,-2.80301564023941,
396.491997521283));
#29974=CARTESIAN_POINT('Ctrl Pts',(-3.07302259383454,-3.3121143867761,396.51837347977));
#29975=CARTESIAN_POINT('Ctrl Pts',(-2.52431420292427,-3.8212131333128,396.544749438256));
#29976=CARTESIAN_POINT('Ctrl Pts',(-1.84637724308029,-4.19102888101748,
396.571125396743));
#29977=CARTESIAN_POINT('Ctrl Pts',(-1.12128724682158,-4.37678928935608,
396.597501355229));
#29978=CARTESIAN_POINT('Ctrl Pts',(-0.396197250562878,-4.56254969769468,
396.623877313716));
#29979=CARTESIAN_POINT('Ctrl Pts',(0.376045782110559,-4.5642547666672,396.650253272203));
#29980=CARTESIAN_POINT('Ctrl Pts',(1.10194900172297,-4.38169806934578,396.676629230689));
#29981=CARTESIAN_POINT('Ctrl Pts',(1.82785222133539,-4.19914137202436,396.703005189176));
#29982=CARTESIAN_POINT('Ctrl Pts',(2.50741562788679,-3.83232290840901,396.729381147662));
#29983=CARTESIAN_POINT('Ctrl Pts',(3.05836678046179,-3.32565214799663,396.755757106149));
#29984=CARTESIAN_POINT('Ctrl Pts',(3.60931793303678,-2.81898138758426,396.782133064635));
#29985=CARTESIAN_POINT('Ctrl Pts',(4.03165683163537,-2.17245833037488,396.808509023122));
#29986=CARTESIAN_POINT('Ctrl Pts',(4.27425233566608,-1.46435533404973,396.834884981609));
#29987=CARTESIAN_POINT('Ctrl Pts',(4.51684783969678,-0.756252337724576,
396.861260940095));
#29988=CARTESIAN_POINT('Ctrl Pts',(4.57969994915959,0.0134305977163408,
396.887636898582));
#29989=CARTESIAN_POINT('Ctrl Pts',(4.45519937195264,0.751510565101793,396.914012857069));
#29990=CARTESIAN_POINT('Ctrl Pts',(4.33069879474569,1.48959053248724,396.940388815555));
#29991=CARTESIAN_POINT('Ctrl Pts',(4.01884553086897,2.19606753181724,396.966764774042));
#29992=CARTESIAN_POINT('Ctrl Pts',(3.5573945991761,2.78541078461679,396.993140732528));
#29993=CARTESIAN_POINT('Ctrl Pts',(3.09594366748323,3.37475403741634,397.019516691015));
#29994=CARTESIAN_POINT('Ctrl Pts',(2.4848950679742,3.84696354368545,397.045892649502));
#29995=CARTESIAN_POINT('Ctrl Pts',(1.79822638583807,4.14487049720285,397.072268607988));
#29996=CARTESIAN_POINT('Ctrl Pts',(1.11155770370195,4.44277745072024,397.098644566475));
#29997=CARTESIAN_POINT('Ctrl Pts',(0.349268938938723,4.56638185148592,397.125020524961));
#29998=CARTESIAN_POINT('Ctrl Pts',(-0.396352188490757,4.50071933317169,
397.151396483448));
#29999=CARTESIAN_POINT('Ctrl Pts',(-1.14197331592023,4.43505681485745,397.177772441934));
#30000=CARTESIAN_POINT('Ctrl Pts',(-1.87092680601596,4.18012737746331,397.204148400421));
#30001=CARTESIAN_POINT('Ctrl Pts',(-2.49496072766192,3.76679446489074,397.230524358908));
#30002=CARTESIAN_POINT('Ctrl Pts',(-3.1189946493079,3.35346155231816,397.256900317394));
#30003=CARTESIAN_POINT('Ctrl Pts',(-3.63810900250409,2.78172516456714,397.283276275881));
#30004=CARTESIAN_POINT('Ctrl Pts',(-3.98945637001185,2.12080349044383,397.309652234368));
#30005=CARTESIAN_POINT('Ctrl Pts',(-4.33474984909618,1.47126982272609,397.335573722081));
#30006=CARTESIAN_POINT('Ctrl Pts',(-4.51800794997827,0.735597803364803,
397.361495209794));
#30007=CARTESIAN_POINT('Ctrl Pts',(-4.51813440218219,-1.34914224690988E-5,
397.387416697508));
#30008=CARTESIAN_POINT('Origin',(0.,0.,387.));
#30009=CARTESIAN_POINT('',(-4.51746064445937,-7.62825515632226E-5,398.387416697508));
#30010=CARTESIAN_POINT('',(-4.51805439081064,6.66898104614677E-5,398.112583302492));
#30011=CARTESIAN_POINT('',(-4.51775,5.53264807684796E-16,387.));
#30012=CARTESIAN_POINT('Ctrl Pts',(-4.51805439081064,6.66898104614677E-5,
398.112583302492));
#30013=CARTESIAN_POINT('Ctrl Pts',(-4.51810357212516,0.0685915430668216,
398.110168746413));
#30014=CARTESIAN_POINT('Ctrl Pts',(-4.51657662108523,0.137114203419027,
398.107754190334));
#30015=CARTESIAN_POINT('Ctrl Pts',(-4.51345907222813,0.205564420371811,
398.105339634255));
#30016=CARTESIAN_POINT('Ctrl Pts',(-4.47940381049539,0.953296103447074,
398.078963675769));
#30017=CARTESIAN_POINT('Ctrl Pts',(-4.255545890619,1.6923832695825,398.052587717282));
#30018=CARTESIAN_POINT('Ctrl Pts',(-3.86898703306984,2.33334713781254,398.026211758796));
#30019=CARTESIAN_POINT('Ctrl Pts',(-3.48242817552068,2.97431100604258,397.999835800309));
#30020=CARTESIAN_POINT('Ctrl Pts',(-2.93316838029875,3.51715157636723,397.973459841822));
#30021=CARTESIAN_POINT('Ctrl Pts',(-2.28770467124889,3.89614897876697,397.947083883336));
#30022=CARTESIAN_POINT('Ctrl Pts',(-1.64224096219904,4.27514638116671,397.920707924849));
#30023=CARTESIAN_POINT('Ctrl Pts',(-0.900573339321256,4.49030061564153,
397.894331966363));
#30024=CARTESIAN_POINT('Ctrl Pts',(-0.15249299074285,4.51556368744535,397.867956007876));
#30025=CARTESIAN_POINT('Ctrl Pts',(0.595587357835559,4.54082675924917,397.841580049389));
#30026=CARTESIAN_POINT('Ctrl Pts',(1.35008043211458,4.37619866838198,397.815204090903));
#30027=CARTESIAN_POINT('Ctrl Pts',(2.01964230998743,4.0416103804436,397.788828132416));
#30028=CARTESIAN_POINT('Ctrl Pts',(2.68920418786027,3.70702209250522,397.76245217393));
#30029=CARTESIAN_POINT('Ctrl Pts',(3.27383486932692,3.20247360749564,397.736076215443));
#30030=CARTESIAN_POINT('Ctrl Pts',(3.70275509709574,2.58904890230608,397.709700256956));
#30031=CARTESIAN_POINT('Ctrl Pts',(4.13167532486456,1.97562419711653,397.68332429847));
#30032=CARTESIAN_POINT('Ctrl Pts',(4.40488509893554,1.25332327174699,397.656948339983));
#30033=CARTESIAN_POINT('Ctrl Pts',(4.48930783693528,0.509592653824902,397.630572381497));
#30034=CARTESIAN_POINT('Ctrl Pts',(4.57373057493501,-0.234137964097188,
397.60419642301));
#30035=CARTESIAN_POINT('Ctrl Pts',(4.4693662768635,-0.999298274571833,397.577820464523));
#30036=CARTESIAN_POINT('Ctrl Pts',(4.18884997495465,-1.69325290932077,397.551444506037));
#30037=CARTESIAN_POINT('Ctrl Pts',(3.9083336730458,-2.3872075440697,397.52506854755));
#30038=CARTESIAN_POINT('Ctrl Pts',(3.4516653672996,-3.00995650309293,397.498692589064));
#30039=CARTESIAN_POINT('Ctrl Pts',(2.87413234340601,-3.48610567828749,397.472316630577));
#30040=CARTESIAN_POINT('Ctrl Pts',(2.29659931951241,-3.96225485348206,397.44594067209));
#30041=CARTESIAN_POINT('Ctrl Pts',(1.5982015774714,-4.29180424484795,397.419564713604));
#30042=CARTESIAN_POINT('Ctrl Pts',(0.863491767430947,-4.43485642328811,
397.393188755117));
#30043=CARTESIAN_POINT('Ctrl Pts',(0.128781957390508,-4.57790860172826,
397.366812796631));
#30044=CARTESIAN_POINT('Ctrl Pts',(-0.642239920649369,-4.53446356724268,
397.340436838144));
#30045=CARTESIAN_POINT('Ctrl Pts',(-1.35622885827011,-4.30978106306993,
397.314060879658));
#30046=CARTESIAN_POINT('Ctrl Pts',(-2.07021779589086,-4.08509855889717,
397.287684921171));
#30047=CARTESIAN_POINT('Ctrl Pts',(-2.72717379309247,-3.67917858503723,
397.261308962684));
#30048=CARTESIAN_POINT('Ctrl Pts',(-3.24756141147036,-3.14116449845108,
397.234933004198));
#30049=CARTESIAN_POINT('Ctrl Pts',(-3.76794902984825,-2.60315041186493,
397.208557045711));
#30050=CARTESIAN_POINT('Ctrl Pts',(-4.15176826940243,-1.93304221255256,
397.182181087224));
#30051=CARTESIAN_POINT('Ctrl Pts',(-4.35255143425054,-1.21196763150028,
397.155805128738));
#30052=CARTESIAN_POINT('Ctrl Pts',(-4.46222473223498,-0.818096823374597,
397.141397853322));
#30053=CARTESIAN_POINT('Ctrl Pts',(-4.51728655488816,-0.409019453899831,
397.126990577907));
#30054=CARTESIAN_POINT('Ctrl Pts',(-4.51738673749921,3.14726202902737E-5,
397.112583302492));
#30055=CARTESIAN_POINT('Ctrl Pts',(-4.51813440218219,-1.34914224690988E-5,
397.387416697508));
#30056=CARTESIAN_POINT('Ctrl Pts',(-4.51813661921663,-0.0129106614282636,
397.387871168281));
#30057=CARTESIAN_POINT('Ctrl Pts',(-4.51808254311073,-0.0258078127678308,
397.388325639054));
#30058=CARTESIAN_POINT('Ctrl Pts',(-4.51797206016886,-0.0387044808823415,
397.388780109827));
#30059=CARTESIAN_POINT('Ctrl Pts',(-4.51156000099881,-0.787183817589628,
397.415156068314));
#30060=CARTESIAN_POINT('Ctrl Pts',(-4.31515550083941,-1.5340355305086,397.4415320268));
#30061=CARTESIAN_POINT('Ctrl Pts',(-3.95253658758193,-2.18884081128186,
397.467907985287));
#30062=CARTESIAN_POINT('Ctrl Pts',(-3.58991767432445,-2.84364609205511,
397.494283943774));
#30063=CARTESIAN_POINT('Ctrl Pts',(-3.06108434796891,-3.40640494068263,
397.52065990226));
#30064=CARTESIAN_POINT('Ctrl Pts',(-2.43006066892999,-3.80898604862584,
397.547035860747));
#30065=CARTESIAN_POINT('Ctrl Pts',(-1.79903698989108,-4.21156715656904,
397.573411819233));
#30066=CARTESIAN_POINT('Ctrl Pts',(-1.0658229581688,-4.45397052382792,397.59978777772));
#30067=CARTESIAN_POINT('Ctrl Pts',(-0.319186314229528,-4.5068491954042,
397.626163736207));
#30068=CARTESIAN_POINT('Ctrl Pts',(0.427450329709741,-4.55972786698048,
397.652539694693));
#30069=CARTESIAN_POINT('Ctrl Pts',(1.18750958586602,-4.42308184287416,397.67891565318));
#30070=CARTESIAN_POINT('Ctrl Pts',(1.86897365333732,-4.11345439459799,397.705291611666));
#30071=CARTESIAN_POINT('Ctrl Pts',(2.55043772080863,-3.80382694632181,397.731667570153));
#30072=CARTESIAN_POINT('Ctrl Pts',(3.15330659959498,-3.32121807387579,397.75804352864));
#30073=CARTESIAN_POINT('Ctrl Pts',(3.60459299560209,-2.72405559953603,397.784419487126));
#30074=CARTESIAN_POINT('Ctrl Pts',(4.0558793916092,-2.12689312519627,397.810795445613));
#30075=CARTESIAN_POINT('Ctrl Pts',(4.35558330483707,-1.41517704896277,397.837171404099));
#30076=CARTESIAN_POINT('Ctrl Pts',(4.46742059718259,-0.675072426614591,
397.863547362586));
#30077=CARTESIAN_POINT('Ctrl Pts',(4.57925788952811,0.065032195733587,397.889923321072));
#30078=CARTESIAN_POINT('Ctrl Pts',(4.50322856099129,0.833525364196443,397.916299279559));
#30079=CARTESIAN_POINT('Ctrl Pts',(4.24853722497469,1.53736821266419,397.942675238046));
#30080=CARTESIAN_POINT('Ctrl Pts',(3.9938458889581,2.24121106113193,397.969051196532));
#30081=CARTESIAN_POINT('Ctrl Pts',(3.56049254546173,2.88040358960456,397.995427155019));
#30082=CARTESIAN_POINT('Ctrl Pts',(3.00094181663071,3.37756092269383,398.021803113505));
#30083=CARTESIAN_POINT('Ctrl Pts',(2.44139108779969,3.87471825578309,398.048179071992));
#30084=CARTESIAN_POINT('Ctrl Pts',(1.75564297363402,4.22984039348899,398.074555030479));
#30085=CARTESIAN_POINT('Ctrl Pts',(1.02671867666087,4.39993390090012,398.100930988965));
#30086=CARTESIAN_POINT('Ctrl Pts',(0.297794379687701,4.57002740831124,398.127306947452));
#30087=CARTESIAN_POINT('Ctrl Pts',(-0.474306100092957,4.55509228542758,
398.153682905938));
#30088=CARTESIAN_POINT('Ctrl Pts',(-1.19610717160092,4.35693667699891,398.180058864425));
#30089=CARTESIAN_POINT('Ctrl Pts',(-1.91790824310887,4.15878106857024,398.206434822912));
#30090=CARTESIAN_POINT('Ctrl Pts',(-2.58940990634414,3.77740497459655,398.232810781398));
#30091=CARTESIAN_POINT('Ctrl Pts',(-3.12931572836207,3.25898030762527,398.259186739885));
#30092=CARTESIAN_POINT('Ctrl Pts',(-3.66922155038001,2.74055564065398,398.285562698372));
#30093=CARTESIAN_POINT('Ctrl Pts',(-4.07753153118063,2.08508240068509,398.311938656858));
#30094=CARTESIAN_POINT('Ctrl Pts',(-4.30481296375181,1.37191651366358,398.338314615345));
#30095=CARTESIAN_POINT('Ctrl Pts',(-4.44585038591782,0.929367920299095,
398.354681976066));
#30096=CARTESIAN_POINT('Ctrl Pts',(-4.51717896496231,0.464603561951737,
398.371049336787));
#30097=CARTESIAN_POINT('Ctrl Pts',(-4.51746064445937,-7.62825515632226E-5,
398.387416697508));
#30098=CARTESIAN_POINT('Origin',(0.,0.,387.));
#30099=CARTESIAN_POINT('',(-4.51769110620511,0.00011483889287206,399.387416697508));
#30100=CARTESIAN_POINT('',(-4.51766328535307,-0.00011344722995056,399.112583302492));
#30101=CARTESIAN_POINT('',(-4.51775,5.53264807684796E-16,387.));
#30102=CARTESIAN_POINT('',(3.43378788736219,2.93584158412962,400.));
#30103=CARTESIAN_POINT('Ctrl Pts',(-4.51769110620511,0.00011483889287206,
399.387416697508));
#30104=CARTESIAN_POINT('Ctrl Pts',(-4.51714363756808,-0.555201766580607,
399.406979422266));
#30105=CARTESIAN_POINT('Ctrl Pts',(-4.41453063358526,-1.11071503909854,
399.426542147024));
#30106=CARTESIAN_POINT('Ctrl Pts',(-4.21442463507641,-1.62855553809715,
399.446104871782));
#30107=CARTESIAN_POINT('Ctrl Pts',(-3.94462645640127,-2.32674761887018,
399.472480830268));
#30108=CARTESIAN_POINT('Ctrl Pts',(-3.49760073249453,-2.95645628495937,
399.498856788754));
#30109=CARTESIAN_POINT('Ctrl Pts',(-2.92746753734289,-3.44144015063649,
399.525232747241));
#30110=CARTESIAN_POINT('Ctrl Pts',(-2.35733434219124,-3.92642401631361,
399.551608705728));
#30111=CARTESIAN_POINT('Ctrl Pts',(-1.66409367579469,-4.26668308157866,
399.577984664215));
#30112=CARTESIAN_POINT('Ctrl Pts',(-0.931673462414912,-4.42103326728196,
399.604360622701));
#30113=CARTESIAN_POINT('Ctrl Pts',(-0.199253249035141,-4.57538345298525,
399.630736581188));
#30114=CARTESIAN_POINT('Ctrl Pts',(0.572346511327848,-4.5438247591268,399.657112539674));
#30115=CARTESIAN_POINT('Ctrl Pts',(1.28970997251907,-4.33015694611576,399.683488498161));
#30116=CARTESIAN_POINT('Ctrl Pts',(2.00707343371029,-4.11648913310473,399.709864456647));
#30117=CARTESIAN_POINT('Ctrl Pts',(2.67020059572975,-3.72071220094113,399.736240415134));
#30118=CARTESIAN_POINT('Ctrl Pts',(3.19881015567137,-3.19078644074148,399.762616373621));
#30119=CARTESIAN_POINT('Ctrl Pts',(3.72741971561299,-2.66086068054184,399.788992332107));
#30120=CARTESIAN_POINT('Ctrl Pts',(4.12151167347679,-1.99678609230616,399.815368290594));
#30121=CARTESIAN_POINT('Ctrl Pts',(4.33336809368492,-1.27886829832022,399.84174424908));
#30122=CARTESIAN_POINT('Ctrl Pts',(4.54522451389304,-0.560950504334284,
399.868120207567));
#30123=CARTESIAN_POINT('Ctrl Pts',(4.57484539644551,0.210810495401909,399.894496166054));
#30124=CARTESIAN_POINT('Ctrl Pts',(4.41862185200597,0.942742363213577,399.92087212454));
#30125=CARTESIAN_POINT('Ctrl Pts',(4.26239830756643,1.67467423102524,399.947248083027));
#30126=CARTESIAN_POINT('Ctrl Pts',(3.92033033613488,2.36677696691239,399.973624041513));
#30127=CARTESIAN_POINT('Ctrl Pts',(3.43378788736214,2.93584158412968,400.));
#30128=CARTESIAN_POINT('',(-3.43408816619742,2.93604416807593,400.));
#30129=CARTESIAN_POINT('Origin',(0.,0.,400.));
#30130=CARTESIAN_POINT('Ctrl Pts',(-3.43408816619742,2.93604416807593,400.));
#30131=CARTESIAN_POINT('Ctrl Pts',(-2.97450238708434,3.47304931101404,399.975093589943));
#30132=CARTESIAN_POINT('Ctrl Pts',(-2.38685943846713,3.90077490879642,399.950187179887));
#30133=CARTESIAN_POINT('Ctrl Pts',(-1.73419289785415,4.17206489997238,399.92528076983));
#30134=CARTESIAN_POINT('Ctrl Pts',(-1.04301719081029,4.45936176567177,399.898904811344));
#30135=CARTESIAN_POINT('Ctrl Pts',(-0.278918372417421,4.57121813647734,
399.872528852857));
#30136=CARTESIAN_POINT('Ctrl Pts',(0.465602633104777,4.49408395991645,399.84615289437));
#30137=CARTESIAN_POINT('Ctrl Pts',(1.21012363862699,4.41694978335555,399.819776935884));
#30138=CARTESIAN_POINT('Ctrl Pts',(1.93506683127852,4.15082505942817,399.793400977397));
#30139=CARTESIAN_POINT('Ctrl Pts',(2.55266298782158,3.72793237180886,399.767025018911));
#30140=CARTESIAN_POINT('Ctrl Pts',(3.17025914436463,3.30503968418955,399.740649060424));
#30141=CARTESIAN_POINT('Ctrl Pts',(3.68050826479921,2.72537903287831,399.714273101937));
#30142=CARTESIAN_POINT('Ctrl Pts',(4.02163754117277,2.05912619043133,399.687897143451));
#30143=CARTESIAN_POINT('Ctrl Pts',(4.36276681754633,1.39287334798434,399.661521184964));
#30144=CARTESIAN_POINT('Ctrl Pts',(4.53477624985888,0.640028314401621,399.635145226478));
#30145=CARTESIAN_POINT('Ctrl Pts',(4.51684061200005,-0.108263669819661,
399.608769267991));
#30146=CARTESIAN_POINT('Ctrl Pts',(4.49890497414122,-0.856555654040941,
399.582393309504));
#30147=CARTESIAN_POINT('Ctrl Pts',(4.29102426611101,-1.60029458890078,399.556017351018));
#30148=CARTESIAN_POINT('Ctrl Pts',(3.91836619751067,-2.24943891706491,399.529641392531));
#30149=CARTESIAN_POINT('Ctrl Pts',(3.54570812891033,-2.89858324522903,399.503265434045));
#30150=CARTESIAN_POINT('Ctrl Pts',(3.00827269973986,-3.45313296669745,399.476889475558));
#30151=CARTESIAN_POINT('Ctrl Pts',(2.37112525795217,-3.84595043629749,399.450513517072));
#30152=CARTESIAN_POINT('Ctrl Pts',(1.73397781616448,-4.23876790589754,399.424137558585));
#30153=CARTESIAN_POINT('Ctrl Pts',(0.99711836175957,-4.4698531236292,399.397761600098));
#30154=CARTESIAN_POINT('Ctrl Pts',(0.249756040315393,-4.51122947332523,
399.371385641612));
#30155=CARTESIAN_POINT('Ctrl Pts',(-0.497606281128785,-4.55260582302126,
399.345009683125));
#30156=CARTESIAN_POINT('Ctrl Pts',(-1.25547146961223,-4.40427330468165,
399.318633724638));
#30157=CARTESIAN_POINT('Ctrl Pts',(-1.93208738383067,-4.08418999214993,
399.292257766152));
#30158=CARTESIAN_POINT('Ctrl Pts',(-2.60870329804912,-3.7641066796182,399.265881807665));
#30159=CARTESIAN_POINT('Ctrl Pts',(-3.20406993800257,-3.27227257289437,
399.239505849179));
#30160=CARTESIAN_POINT('Ctrl Pts',(-3.64610826548277,-2.6682323819666,399.213129890692));
#30161=CARTESIAN_POINT('Ctrl Pts',(-4.08814659296297,-2.06419219103883,
399.186753932205));
#30162=CARTESIAN_POINT('Ctrl Pts',(-4.37685660796992,-1.34794591590712,
399.160377973719));
#30163=CARTESIAN_POINT('Ctrl Pts',(-4.47728517341772,-0.606207058821207,
399.134002015232));
#30164=CARTESIAN_POINT('Ctrl Pts',(-4.50446965905899,-0.405429628414596,
399.126862444319));
#30165=CARTESIAN_POINT('Ctrl Pts',(-4.51785871427772,-0.20278434994614,
399.119722873405));
#30166=CARTESIAN_POINT('Ctrl Pts',(-4.51766328535307,-0.00011344722995056,
399.112583302492));
#30167=CARTESIAN_POINT('Origin',(0.,0.,402.208336844637));
#30168=CARTESIAN_POINT('',(-5.07399177313997,5.16404304284901E-5,375.791663155363));
#30169=CARTESIAN_POINT('',(-5.07400718786956,-4.16755268873004E-5,375.708336844637));
#30170=CARTESIAN_POINT('',(-5.0736,-1.59740085886799E-13,402.208336844637));
#30171=CARTESIAN_POINT('',(1.3130361863572,-4.90075024188303,375.));
#30172=CARTESIAN_POINT('Ctrl Pts',(-5.07400718786956,-4.16755268873182E-5,
375.708336844637));
#30173=CARTESIAN_POINT('Ctrl Pts',(-5.07365763063996,0.800054575924722,
375.683232230984));
#30174=CARTESIAN_POINT('Ctrl Pts',(-4.67875473787853,2.4410987772414,375.631751658845));
#30175=CARTESIAN_POINT('Ctrl Pts',(-2.98728944096456,4.36266186682328,375.553895128218));
#30176=CARTESIAN_POINT('Ctrl Pts',(-0.544875549618088,5.2592655277028,375.474767252759));
#30177=CARTESIAN_POINT('Ctrl Pts',(2.02945798133318,4.88240903418803,375.395639377299));
#30178=CARTESIAN_POINT('Ctrl Pts',(4.1124194375256,3.3233956145555,375.316511501839));
#30179=CARTESIAN_POINT('Ctrl Pts',(5.19956989745793,0.959601216722932,375.237383626379));
#30180=CARTESIAN_POINT('Ctrl Pts',(5.02785240284651,-1.63637626402564,375.15825575092));
#30181=CARTESIAN_POINT('Ctrl Pts',(3.63845954881624,-3.83644847785649,375.07912787546));
#30182=CARTESIAN_POINT('Ctrl Pts',(2.1252131908655,-4.68314727417153,375.026375958487));
#30183=CARTESIAN_POINT('Ctrl Pts',(1.3130361863572,-4.90075024188303,375.));
#30184=CARTESIAN_POINT('',(-1.31318542874413,-4.90112866933894,375.));
#30185=CARTESIAN_POINT('Origin',(0.,0.,375.));
#30186=CARTESIAN_POINT('Ctrl Pts',(-5.07399177313997,5.16404304287937E-5,
375.791663155363));
#30187=CARTESIAN_POINT('Ctrl Pts',(-5.07401862443284,0.0509709830336597,
375.790065473344));
#30188=CARTESIAN_POINT('Ctrl Pts',(-5.06087568855098,0.942498320863251,
375.762091832839));
#30189=CARTESIAN_POINT('Ctrl Pts',(-4.56924148341307,2.66059337382158,375.707742233848));
#30190=CARTESIAN_POINT('Ctrl Pts',(-2.74710339271414,4.51775908713646,375.628614358388));
#30191=CARTESIAN_POINT('Ctrl Pts',(-0.25980027835232,5.28102544478076,375.549486482929));
#30192=CARTESIAN_POINT('Ctrl Pts',(2.29040909674433,4.76557955369675,375.470358607468));
#30193=CARTESIAN_POINT('Ctrl Pts',(4.28603436317887,3.09622956904483,375.391230732009));
#30194=CARTESIAN_POINT('Ctrl Pts',(5.24386820297344,0.677177255244125,375.312102856549));
#30195=CARTESIAN_POINT('Ctrl Pts',(4.93198748823577,-1.90583737857549,375.232974981089));
#30196=CARTESIAN_POINT('Ctrl Pts',(3.42590832840442,-4.02739560248487,375.153847105629));
#30197=CARTESIAN_POINT('Ctrl Pts',(1.13368018117025,-5.15247588128094,375.0761887786));
#30198=CARTESIAN_POINT('Ctrl Pts',(-0.546344062323364,-5.10618409554666,
375.024906410057));
#30199=CARTESIAN_POINT('Ctrl Pts',(-1.31318542874413,-4.90112866933894,
375.));
#30200=CARTESIAN_POINT('Origin',(0.,0.,402.208336844637));
#30201=CARTESIAN_POINT('',(-5.07342806457247,-0.000120553681964564,376.791663155363));
#30202=CARTESIAN_POINT('',(-5.0732320111606,-6.61733612274322E-5,376.708336844637));
#30203=CARTESIAN_POINT('',(-5.0736,-1.59740085886799E-13,402.208336844637));
#30204=CARTESIAN_POINT('Ctrl Pts',(-5.0732320111606,-6.61733612272383E-5,
376.708336844637));
#30205=CARTESIAN_POINT('Ctrl Pts',(-5.07300240190748,0.495753489740335,
376.692786357976));
#30206=CARTESIAN_POINT('Ctrl Pts',(-4.87836138639172,1.83273410665417,376.650859912829));
#30207=CARTESIAN_POINT('Ctrl Pts',(-3.72041242686768,3.75702756739127,376.582557509196));
#30208=CARTESIAN_POINT('Ctrl Pts',(-1.47810086816716,5.0766073897426,376.503429633736));
#30209=CARTESIAN_POINT('Ctrl Pts',(1.12210802704861,5.16697187426544,376.424301758276));
#30210=CARTESIAN_POINT('Ctrl Pts',(3.45061728097363,4.00624077340234,376.345173882816));
#30211=CARTESIAN_POINT('Ctrl Pts',(4.94361743453053,1.87546566308182,376.266046007357));
#30212=CARTESIAN_POINT('Ctrl Pts',(5.23960352937691,-0.709422013391795,
376.186918131896));
#30213=CARTESIAN_POINT('Ctrl Pts',(4.2669075188957,-3.12253502690154,376.107790256437));
#30214=CARTESIAN_POINT('Ctrl Pts',(2.26105138176727,-4.77957859502704,376.028662380977));
#30215=CARTESIAN_POINT('Ctrl Pts',(-0.292280359441297,-5.27932727476591,
375.949534505517));
#30216=CARTESIAN_POINT('Ctrl Pts',(-2.77484145645776,-4.50077558721857,
375.870406630058));
#30217=CARTESIAN_POINT('Ctrl Pts',(-4.58552092957851,-2.63243616845826,
375.791278754598));
#30218=CARTESIAN_POINT('Ctrl Pts',(-5.06368921675185,-0.921683996926001,
375.737255492791));
#30219=CARTESIAN_POINT('Ctrl Pts',(-5.07402489010486,-0.0405600539318397,
375.709608189471));
#30220=CARTESIAN_POINT('Ctrl Pts',(-5.07400718786956,-4.16755268873182E-5,
375.708336844637));
#30221=CARTESIAN_POINT('Ctrl Pts',(-5.07342806457247,-0.000120553681964737,
376.791663155363));
#30222=CARTESIAN_POINT('Ctrl Pts',(-5.07290494961689,0.587111569129446,
376.77324364185));
#30223=CARTESIAN_POINT('Ctrl Pts',(-4.82510106239333,2.01566514286781,376.728448169851));
#30224=CARTESIAN_POINT('Ctrl Pts',(-3.51189274247934,3.95263634434836,376.657276739365));
#30225=CARTESIAN_POINT('Ctrl Pts',(-1.20153141562281,5.1490821475793,376.578148863906));
#30226=CARTESIAN_POINT('Ctrl Pts',(1.39976059245402,5.09876406487689,376.499020988446));
#30227=CARTESIAN_POINT('Ctrl Pts',(3.66212404867255,3.81386577598244,376.419893112986));
#30228=CARTESIAN_POINT('Ctrl Pts',(5.03776558457334,1.60550385251465,376.340765237526));
#30229=CARTESIAN_POINT('Ctrl Pts',(5.19359667332446,-0.99160390296118,376.261637362067));
#30230=CARTESIAN_POINT('Ctrl Pts',(4.09188543028651,-3.34861140308599,376.182509486607));
#30231=CARTESIAN_POINT('Ctrl Pts',(1.99939275591558,-4.89480881330613,376.103381611147));
#30232=CARTESIAN_POINT('Ctrl Pts',(-0.577219342064538,-5.2558103583336,
376.024253735687));
#30233=CARTESIAN_POINT('Ctrl Pts',(-3.01406745721832,-4.34420557675964,
375.945125860227));
#30234=CARTESIAN_POINT('Ctrl Pts',(-4.68664255775979,-2.42036918652462,
375.867595666786));
#30235=CARTESIAN_POINT('Ctrl Pts',(-5.0735753393625,-0.789650899948463,
375.816441431831));
#30236=CARTESIAN_POINT('Ctrl Pts',(-5.07399177313997,5.16404304287937E-5,
375.791663155363));
#30237=CARTESIAN_POINT('Origin',(0.,0.,402.208336844637));
#30238=CARTESIAN_POINT('',(-5.07335325700037,0.000107956674043064,377.791663155363));
#30239=CARTESIAN_POINT('',(-5.07361435362778,0.000129215856731547,377.708336844637));
#30240=CARTESIAN_POINT('',(-5.0736,-1.59740085886799E-13,402.208336844637));
#30241=CARTESIAN_POINT('Ctrl Pts',(-5.07361435362778,0.000129215856731774,
377.708336844637));
#30242=CARTESIAN_POINT('Ctrl Pts',(-5.07380906160703,0.191278857423315,
377.702340484969));
#30243=CARTESIAN_POINT('Ctrl Pts',(-5.01660264728387,1.22311525648581,377.669968166814));
#30244=CARTESIAN_POINT('Ctrl Pts',(-4.33319923422642,3.02986949626759,377.611219890172));
#30245=CARTESIAN_POINT('Ctrl Pts',(-2.36351373006459,4.72974921277116,377.532092014713));
#30246=CARTESIAN_POINT('Ctrl Pts',(0.178456984968689,5.28439948077629,377.452964139253));
#30247=CARTESIAN_POINT('Ctrl Pts',(2.67721733402229,4.55952104001336,377.373836263793));
#30248=CARTESIAN_POINT('Ctrl Pts',(4.52773440567874,2.73063104786141,377.294708388334));
#30249=CARTESIAN_POINT('Ctrl Pts',(5.28193652635228,0.240564543316707,377.215580512874));
#30250=CARTESIAN_POINT('Ctrl Pts',(4.75720630136386,-2.3077506308472,377.136452637414));
#30251=CARTESIAN_POINT('Ctrl Pts',(3.08059835436342,-4.29728269340077,377.057324761954));
#30252=CARTESIAN_POINT('Ctrl Pts',(0.658075181053442,-5.24629982216222,
376.978196886494));
#30253=CARTESIAN_POINT('Ctrl Pts',(-1.923789860657,-4.92501343550216,376.899069011035));
#30254=CARTESIAN_POINT('Ctrl Pts',(-4.03984145181191,-3.4112176436405,376.819941135575));
#30255=CARTESIAN_POINT('Ctrl Pts',(-4.95409465736432,-1.5312714924381,376.756363746775));
#30256=CARTESIAN_POINT('Ctrl Pts',(-5.07339185365009,-0.345231048960516,
376.719162316463));
#30257=CARTESIAN_POINT('Ctrl Pts',(-5.0732320111606,-6.61733612272383E-5,
376.708336844637));
#30258=CARTESIAN_POINT('Ctrl Pts',(-5.07335325700037,0.00010795667404348,
377.791663155363));
#30259=CARTESIAN_POINT('Ctrl Pts',(-5.07357381709386,0.28275711441475,377.782797768842));
#30260=CARTESIAN_POINT('Ctrl Pts',(-4.98125011308217,1.40619065190393,377.747556423836));
#30261=CARTESIAN_POINT('Ctrl Pts',(-4.16308913613231,3.25966463764834,377.685939120343));
#30262=CARTESIAN_POINT('Ctrl Pts',(-2.1043987453421,4.85059075019948,377.606811244883));
#30263=CARTESIAN_POINT('Ctrl Pts',(0.463836508427624,5.26702766261653,377.527683369423));
#30264=CARTESIAN_POINT('Ctrl Pts',(2.91976153075723,4.40814216068722,377.448555493963));
#30265=CARTESIAN_POINT('Ctrl Pts',(4.66871526619766,2.48189896419878,377.369427618503));
#30266=CARTESIAN_POINT('Ctrl Pts',(5.28721789969248,-0.0452944421492617,
377.290299743044));
#30267=CARTESIAN_POINT('Ctrl Pts',(4.62550939154664,-2.56152055897115,377.211171867584));
#30268=CARTESIAN_POINT('Ctrl Pts',(2.84381135938942,-4.45751743210561,377.132043992124));
#30269=CARTESIAN_POINT('Ctrl Pts',(0.373532100567371,-5.27420121678766,
377.052916116664));
#30270=CARTESIAN_POINT('Ctrl Pts',(-2.18719169184094,-4.81382563128935,
376.973788241204));
#30271=CARTESIAN_POINT('Ctrl Pts',(-4.21832369780876,-3.18786290260816,
376.894660365745));
#30272=CARTESIAN_POINT('Ctrl Pts',(-4.99301148124094,-1.34818805955531,
376.833952003797));
#30273=CARTESIAN_POINT('Ctrl Pts',(-5.07365402794313,-0.253779808523861,
376.799619600337));
#30274=CARTESIAN_POINT('Ctrl Pts',(-5.07342806457247,-0.000120553681964737,
376.791663155363));
#30275=CARTESIAN_POINT('Origin',(0.,0.,402.208336844637));
#30276=CARTESIAN_POINT('',(-5.07402683453791,-2.287789782323E-5,378.791663155363));
#30277=CARTESIAN_POINT('',(-5.07385055213498,-0.000101541417780425,378.708336844637));
#30278=CARTESIAN_POINT('',(-5.0736,-1.59740085886799E-13,402.208336844637));
#30279=CARTESIAN_POINT('Ctrl Pts',(-5.07385055213498,-0.000101541417780338,
378.708336844637));
#30280=CARTESIAN_POINT('Ctrl Pts',(-5.07319426513103,0.727190265934581,
378.685518653475));
#30281=CARTESIAN_POINT('Ctrl Pts',(-4.73238867060224,2.2957670138656,378.636324503826));
#30282=CARTESIAN_POINT('Ctrl Pts',(-3.17247821056078,4.22990623671853,378.56075439569));
#30283=CARTESIAN_POINT('Ctrl Pts',(-0.770966287939471,5.23090200164121,
378.48162652023));
#30284=CARTESIAN_POINT('Ctrl Pts',(1.81722219130848,4.96532257515351,378.40249864477));
#30285=CARTESIAN_POINT('Ctrl Pts',(3.96540079385267,3.49747356130477,378.323370769311));
#30286=CARTESIAN_POINT('Ctrl Pts',(5.15342409853101,1.18276998126983,378.244242893851));
#30287=CARTESIAN_POINT('Ctrl Pts',(5.09363218664291,-1.41832151330666,378.165115018391));
#30288=CARTESIAN_POINT('Ctrl Pts',(3.80050266687247,-3.67599024033094,378.085987142931));
#30289=CARTESIAN_POINT('Ctrl Pts',(1.58714516515185,-5.04357958127442,378.006859267472));
#30290=CARTESIAN_POINT('Ctrl Pts',(-1.01051292004705,-5.18995071328536,
377.927731392012));
#30291=CARTESIAN_POINT('Ctrl Pts',(-3.36349224912901,-4.07966232156074,
377.848603516552));
#30292=CARTESIAN_POINT('Ctrl Pts',(-4.78546484347183,-2.14054821676427,
377.77547200076));
#30293=CARTESIAN_POINT('Ctrl Pts',(-5.07295260704762,-0.649523777787379,
377.728716443455));
#30294=CARTESIAN_POINT('Ctrl Pts',(-5.07361435362778,0.000129215856731774,
377.708336844637));
#30295=CARTESIAN_POINT('Ctrl Pts',(-5.07402683453791,-2.28778978229567E-5,
378.791663155363));
#30296=CARTESIAN_POINT('Ctrl Pts',(-5.07381925213896,0.818631858438491,
378.765975937348));
#30297=CARTESIAN_POINT('Ctrl Pts',(-4.66448051806342,2.47809170659261,378.713912760847));
#30298=CARTESIAN_POINT('Ctrl Pts',(-2.9391988257698,4.39520590733944,378.63547362586));
#30299=CARTESIAN_POINT('Ctrl Pts',(-0.487090471470337,5.2649280695866,378.5563457504));
#30300=CARTESIAN_POINT('Ctrl Pts',(2.08295867142411,4.85983619872698,378.47721787494));
#30301=CARTESIAN_POINT('Ctrl Pts',(4.1486543056634,3.27801649742928,378.398089999481));
#30302=CARTESIAN_POINT('Ctrl Pts',(5.20982287752563,0.902480077413658,378.318962124021));
#30303=CARTESIAN_POINT('Ctrl Pts',(5.00952021436078,-1.69157675771122,378.239834248561));
#30304=CARTESIAN_POINT('Ctrl Pts',(3.59624624674644,-3.8760466506584,378.160706373101));
#30305=CARTESIAN_POINT('Ctrl Pts',(1.31220156369858,-5.12199685294173,378.081578497641));
#30306=CARTESIAN_POINT('Ctrl Pts',(-1.28957072085835,-5.12774141910675,
378.002450622182));
#30307=CARTESIAN_POINT('Ctrl Pts',(-3.57909508295452,-3.89188939879962,
377.923322746722));
#30308=CARTESIAN_POINT('Ctrl Pts',(-4.84258096039032,-1.9577252596909,377.853060257782));
#30309=CARTESIAN_POINT('Ctrl Pts',(-5.07291761514975,-0.558169836019873,
377.809173727329));
#30310=CARTESIAN_POINT('Ctrl Pts',(-5.07335325700037,0.00010795667404348,
377.791663155363));
#30311=CARTESIAN_POINT('Origin',(0.,0.,402.208336844637));
#30312=CARTESIAN_POINT('',(-5.07326152951467,-8.03441847486985E-5,379.791663155363));
#30313=CARTESIAN_POINT('',(-5.07317735229637,-2.23272941127382E-6,379.708336844637));
#30314=CARTESIAN_POINT('',(-5.0736,-1.59740085886799E-13,402.208336844637));
#30315=CARTESIAN_POINT('Ctrl Pts',(-5.07317735229636,-2.23272941118208E-6,
379.708336844637));
#30316=CARTESIAN_POINT('Ctrl Pts',(-5.07317083223754,0.422929008539474,
379.695072780467));
#30317=CARTESIAN_POINT('Ctrl Pts',(-4.91684325738401,1.68687545589345,379.65543275781));
#30318=CARTESIAN_POINT('Ctrl Pts',(-3.87882817196482,3.59324599495851,379.589416776668));
#30319=CARTESIAN_POINT('Ctrl Pts',(-1.69545248338881,5.00820982432685,379.510288901207));
#30320=CARTESIAN_POINT('Ctrl Pts',(0.898448589337301,5.21051963821565,379.431161025747));
#30321=CARTESIAN_POINT('Ctrl Pts',(3.27480540417913,4.15118950816177,379.352033150288));
#30322=CARTESIAN_POINT('Ctrl Pts',(4.85822301267979,2.08671845896413,379.272905274828));
#30323=CARTESIAN_POINT('Ctrl Pts',(5.26530339668872,-0.483016468385486,
379.193777399368));
#30324=CARTESIAN_POINT('Ctrl Pts',(4.39747886842774,-2.93579705866137,379.114649523908));
#30325=CARTESIAN_POINT('Ctrl Pts',(2.4648785829925,-4.67772362790043,379.035521648449));
#30326=CARTESIAN_POINT('Ctrl Pts',(-0.0645507124447473,-5.28701787148826,
378.956393772989));
#30327=CARTESIAN_POINT('Ctrl Pts',(-2.57835013545374,-4.61614940691036,
378.877265897529));
#30328=CARTESIAN_POINT('Ctrl Pts',(-4.46784531508162,-2.82755778162292,
378.798138022069));
#30329=CARTESIAN_POINT('Ctrl Pts',(-5.04261473172305,-1.0675305862618,378.741828337772));
#30330=CARTESIAN_POINT('Ctrl Pts',(-5.07395287910916,-0.113499444385656,
378.711894611961));
#30331=CARTESIAN_POINT('Ctrl Pts',(-5.07385055213498,-0.000101541417780338,
378.708336844637));
#30332=CARTESIAN_POINT('Ctrl Pts',(-5.07326152951467,-8.03441847485598E-5,
379.791663155363));
#30333=CARTESIAN_POINT('Ctrl Pts',(-5.07297012272296,0.514306801455685,
379.775530064341));
#30334=CARTESIAN_POINT('Ctrl Pts',(-4.86799754311315,1.86989152588461,379.733021014832));
#30335=CARTESIAN_POINT('Ctrl Pts',(-3.67892986111526,3.7976571438602,379.664136006837));
#30336=CARTESIAN_POINT('Ctrl Pts',(-1.42226240084736,5.09253319757995,379.585008131377));
#30337=CARTESIAN_POINT('Ctrl Pts',(1.17878204679748,5.15433774518764,379.505880255918));
#30338=CARTESIAN_POINT('Ctrl Pts',(3.49440419135096,3.9681058520139,379.426752380457));
#30339=CARTESIAN_POINT('Ctrl Pts',(4.96391496617568,1.82106367650753,379.347624504998));
#30340=CARTESIAN_POINT('Ctrl Pts',(5.2314969825461,-0.766918526917405,379.268496629538));
#30341=CARTESIAN_POINT('Ctrl Pts',(4.23235974285854,-3.16920427116154,379.189368754078));
#30342=CARTESIAN_POINT('Ctrl Pts',(2.20842757301423,-4.80412035237133,379.110240878619));
#30343=CARTESIAN_POINT('Ctrl Pts',(-0.350238295746339,-5.27579926091873,
379.031113003158));
#30344=CARTESIAN_POINT('Ctrl Pts',(-2.82409983509395,-4.47003185970082,
378.951985127699));
#30345=CARTESIAN_POINT('Ctrl Pts',(-4.61415296279982,-2.58192121126957,
378.872857252239));
#30346=CARTESIAN_POINT('Ctrl Pts',(-5.06855147600533,-0.884525550463806,
378.819416594794));
#30347=CARTESIAN_POINT('Ctrl Pts',(-5.07403240035665,-0.0219731198176094,
378.792351895835));
#30348=CARTESIAN_POINT('Ctrl Pts',(-5.07402683453791,-2.28778978229567E-5,
378.791663155363));
#30349=CARTESIAN_POINT('Origin',(0.,0.,402.208336844637));
#30350=CARTESIAN_POINT('',(-5.07355665554129,0.000129459885802874,380.791663155363));
#30351=CARTESIAN_POINT('',(-5.07383699511133,0.000104483598321417,380.708336844637));
#30352=CARTESIAN_POINT('',(-5.0736,-1.59740085886799E-13,402.208336844637));
#30353=CARTESIAN_POINT('Ctrl Pts',(-5.07383699511133,0.000104483598321794,
380.708336844637));
#30354=CARTESIAN_POINT('Ctrl Pts',(-5.07394580731281,0.118353460768718,
380.704626907459));
#30355=CARTESIAN_POINT('Ctrl Pts',(-5.04109883614377,1.0772383012794,380.674541011795));
#30356=CARTESIAN_POINT('Ctrl Pts',(-4.45971656638884,2.84036140577044,380.618079157644));
#30357=CARTESIAN_POINT('Ctrl Pts',(-2.56509888808806,4.6235259772432,380.538951282184));
#30358=CARTESIAN_POINT('Ctrl Pts',(-0.0493855337170155,5.28718127521391,
380.459823406725));
#30359=CARTESIAN_POINT('Ctrl Pts',(2.47828569939099,4.67063429954727,380.380695531265));
#30360=CARTESIAN_POINT('Ctrl Pts',(4.40588161411396,2.92317156019379,380.301567655805));
#30361=CARTESIAN_POINT('Ctrl Pts',(5.26666718771851,0.467911852513223,380.222439780345));
#30362=CARTESIAN_POINT('Ctrl Pts',(4.8522176299277,-2.10064486282949,380.143311904886));
#30363=CARTESIAN_POINT('Ctrl Pts',(3.26288495036134,-4.1605656548862,380.064184029426));
#30364=CARTESIAN_POINT('Ctrl Pts',(0.883499402425967,-5.21307525111868,
379.985056153966));
#30365=CARTESIAN_POINT('Ctrl Pts',(-1.70981070849824,-5.0033261046046,379.905928278506));
#30366=CARTESIAN_POINT('Ctrl Pts',(-3.88911883186622,-3.58210545343612,
379.826800403046));
#30367=CARTESIAN_POINT('Ctrl Pts',(-4.91928148884334,-1.67716650260946,
379.760936591757));
#30368=CARTESIAN_POINT('Ctrl Pts',(-5.07318379755486,-0.418081463015616,
379.721448738954));
#30369=CARTESIAN_POINT('Ctrl Pts',(-5.07317735229636,-2.23272941118208E-6,
379.708336844637));
#30370=CARTESIAN_POINT('Ctrl Pts',(-5.07355665554129,0.000129459885803325,
380.791663155363));
#30371=CARTESIAN_POINT('Ctrl Pts',(-5.07376606808144,0.209858000324401,
380.785084191333));
#30372=CARTESIAN_POINT('Ctrl Pts',(-5.00984200321542,1.26028988400143,380.752129268817));
#30373=CARTESIAN_POINT('Ctrl Pts',(-4.29966508516876,3.07727230850615,380.692798387814));
#30374=CARTESIAN_POINT('Ctrl Pts',(-2.31143093395199,4.75541919738815,380.613670512354));
#30375=CARTESIAN_POINT('Ctrl Pts',(0.236477452546483,5.28212108151216,380.534542636895));
#30376=CARTESIAN_POINT('Ctrl Pts',(2.7271267899117,4.52984593303835,380.455414761435));
#30377=CARTESIAN_POINT('Ctrl Pts',(4.55744811217567,2.68074456264382,380.376286885975));
#30378=CARTESIAN_POINT('Ctrl Pts',(5.28425980776137,0.182545855597361,380.297159010515));
#30379=CARTESIAN_POINT('Ctrl Pts',(4.73157661405697,-2.35985326887651,380.218031135055));
#30380=CARTESIAN_POINT('Ctrl Pts',(3.03322149728047,-4.33085350176541,380.138903259596));
#30381=CARTESIAN_POINT('Ctrl Pts',(0.600422665576261,-5.25321019263273,
380.059775384136));
#30382=CARTESIAN_POINT('Ctrl Pts',(-1.97775844481349,-4.90359013777528,
379.980647508676));
#30383=CARTESIAN_POINT('Ctrl Pts',(-4.07705851709219,-3.36664796994342,
379.901519633216));
#30384=CARTESIAN_POINT('Ctrl Pts',(-4.96242349460837,-1.49409344074893,
379.838524848778));
#30385=CARTESIAN_POINT('Ctrl Pts',(-5.07344654310827,-0.326663721856642,
379.801906022827));
#30386=CARTESIAN_POINT('Ctrl Pts',(-5.07326152951467,-8.03441847485598E-5,
379.791663155363));
#30387=CARTESIAN_POINT('Origin',(0.,0.,402.208336844637));
#30388=CARTESIAN_POINT('',(-5.07389966860957,-8.89210953775033E-5,381.791663155363));
#30389=CARTESIAN_POINT('',(-5.0736295665075,-0.000128745637012367,381.708336844637));
#30390=CARTESIAN_POINT('',(-5.0736,-1.59740085886799E-13,402.208336844637));
#30391=CARTESIAN_POINT('Ctrl Pts',(-5.0736295665075,-0.000128745637012449,
381.708336844637));
#30392=CARTESIAN_POINT('Ctrl Pts',(-5.07296124918876,0.654369409793758,
381.687805075965));
#30393=CARTESIAN_POINT('Ctrl Pts',(-4.78227571732073,2.15023935796871,381.640897348807));
#30394=CARTESIAN_POINT('Ctrl Pts',(-3.35177659407457,4.08929314568265,381.567613663161));
#30395=CARTESIAN_POINT('Ctrl Pts',(-0.995622270609436,5.1928278483096,381.488485787702));
#30396=CARTESIAN_POINT('Ctrl Pts',(1.60160528794473,5.03900637720777,381.409357912242));
#30397=CARTESIAN_POINT('Ctrl Pts',(3.81103098679937,3.66507402184023,381.330230036782));
#30398=CARTESIAN_POINT('Ctrl Pts',(5.09767944760569,1.40370545962173,381.251102161322));
#30399=CARTESIAN_POINT('Ctrl Pts',(5.15001032416474,-1.1975468378773,381.171974285863));
#30400=CARTESIAN_POINT('Ctrl Pts',(3.95535257236717,-3.50883325283227,381.092846410403));
#30401=CARTESIAN_POINT('Ctrl Pts',(1.8029725310162,-4.97051454281288,381.013718534943));
#30402=CARTESIAN_POINT('Ctrl Pts',(-0.785967070782117,-5.22866909753901,
380.934590659483));
#30403=CARTESIAN_POINT('Ctrl Pts',(-3.18459792796892,-4.22078912113472,
380.855462784024));
#30404=CARTESIAN_POINT('Ctrl Pts',(-4.73582433047741,-2.28608714092918,
380.780044845741));
#30405=CARTESIAN_POINT('Ctrl Pts',(-5.07317220227002,-0.722342746081139,
380.731002865946));
#30406=CARTESIAN_POINT('Ctrl Pts',(-5.07383699511133,0.000104483598321794,
380.708336844637));
#30407=CARTESIAN_POINT('Ctrl Pts',(-5.07389966860957,-8.89210953773471E-5,
381.791663155363));
#30408=CARTESIAN_POINT('Ctrl Pts',(-5.07328829289394,0.745751527323211,
381.768262359839));
#30409=CARTESIAN_POINT('Ctrl Pts',(-4.71908116243226,2.33281964194823,381.718485605828));
#30410=CARTESIAN_POINT('Ctrl Pts',(-3.12583571520092,4.26449009693918,381.642332893332));
#30411=CARTESIAN_POINT('Ctrl Pts',(-0.713476057932961,5.23905302703404,
381.563205017871));
#30412=CARTESIAN_POINT('Ctrl Pts',(1.87163986094335,4.94506713162178,381.484077142412));
#30413=CARTESIAN_POINT('Ctrl Pts',(4.00356957706116,3.45371616479241,381.404949266952));
#30414=CARTESIAN_POINT('Ctrl Pts',(5.16610206459392,1.12610575148009,381.325821391492));
#30415=CARTESIAN_POINT('Ctrl Pts',(5.07774957870228,-1.47417228345499,381.246693516033));
#30416=CARTESIAN_POINT('Ctrl Pts',(3.75990519207135,-3.71750422352859,381.167565640573));
#30417=CARTESIAN_POINT('Ctrl Pts',(1.53166282114666,-5.06070486272762,381.088437765113));
#30418=CARTESIAN_POINT('Ctrl Pts',(-1.0674460141586,-5.17854069330105,381.009309889653));
#30419=CARTESIAN_POINT('Ctrl Pts',(-3.40809069944175,-4.04247974511891,
380.930182014193));
#30420=CARTESIAN_POINT('Ctrl Pts',(-4.79752508832052,-2.10343849769112,
380.857633102763));
#30421=CARTESIAN_POINT('Ctrl Pts',(-5.07292650482488,-0.630972144226672,
380.81146014982));
#30422=CARTESIAN_POINT('Ctrl Pts',(-5.07355665554129,0.000129459885803325,
380.791663155363));
#30423=CARTESIAN_POINT('Origin',(0.,0.,402.208336844637));
#30424=CARTESIAN_POINT('',(-5.0731816081447,-1.92612327425123E-5,382.791663155363));
#30425=CARTESIAN_POINT('',(-5.07322528972955,6.22763117692481E-5,382.708336844637));
#30426=CARTESIAN_POINT('',(-5.0736,-1.59740085886799E-13,402.208336844637));
#30427=CARTESIAN_POINT('Ctrl Pts',(-5.07322528972955,6.22763117691383E-5,
382.708336844637));
#30428=CARTESIAN_POINT('Ctrl Pts',(-5.07337757676184,0.350080340895845,
382.697359202958));
#30429=CARTESIAN_POINT('Ctrl Pts',(-4.95188321010373,1.54098189440445,382.660005602791));
#30430=CARTESIAN_POINT('Ctrl Pts',(-4.03004033454984,3.42279121037416,382.596276044139));
#30431=CARTESIAN_POINT('Ctrl Pts',(-1.90965538190854,4.93051124025298,382.517148168679));
#30432=CARTESIAN_POINT('Ctrl Pts',(0.673120594328623,5.24439066369047,382.438020293219));
#30433=CARTESIAN_POINT('Ctrl Pts',(3.09291170766135,4.28842884242289,382.35889241776));
#30434=CARTESIAN_POINT('Ctrl Pts',(4.76380612269667,2.29409589888282,382.2797645423));
#30435=CARTESIAN_POINT('Ctrl Pts',(5.28122477966896,-0.255713891925586,
382.20063666684));
#30436=CARTESIAN_POINT('Ctrl Pts',(4.51988342850276,-2.74360685242242,382.12150879138));
#30437=CARTESIAN_POINT('Ctrl Pts',(2.66412810880644,-4.56718142707082,382.04238091592));
#30438=CARTESIAN_POINT('Ctrl Pts',(0.16329884807764,-5.28488961607806,381.96325304046));
#30439=CARTESIAN_POINT('Ctrl Pts',(-2.37707049000228,-4.72295041827389,
381.884125165001));
#30440=CARTESIAN_POINT('Ctrl Pts',(-4.3418720751543,-3.0174279860352,381.804997289541));
#30441=CARTESIAN_POINT('Ctrl Pts',(-5.01833358746616,-1.21340586700331,
381.746401182753));
#30442=CARTESIAN_POINT('Ctrl Pts',(-5.07381979723383,-0.186425967023143,
381.714181034452));
#30443=CARTESIAN_POINT('Ctrl Pts',(-5.0736295665075,-0.000128745637012449,
381.708336844637));
#30444=CARTESIAN_POINT('Ctrl Pts',(-5.0731816081447,-1.92612327423736E-5,
382.791663155363));
#30445=CARTESIAN_POINT('Ctrl Pts',(-5.07312283046122,0.441487546406695,
382.777816486831));
#30446=CARTESIAN_POINT('Ctrl Pts',(-4.90736705066614,1.72404611325897,382.737593859813));
#30447=CARTESIAN_POINT('Ctrl Pts',(-3.83913463932894,3.63562510806912,382.670995274309));
#30448=CARTESIAN_POINT('Ctrl Pts',(-1.64035202533435,5.0265266276326,382.591867398849));
#30449=CARTESIAN_POINT('Ctrl Pts',(0.955614320991023,5.2003390249901,382.512739523389));
#30450=CARTESIAN_POINT('Ctrl Pts',(3.32019468624774,4.11497654315675,382.433611647929));
#30451=CARTESIAN_POINT('Ctrl Pts',(4.8808455917412,2.03324150432223,382.354483772469));
#30452=CARTESIAN_POINT('Ctrl Pts',(5.25968159463003,-0.540808864968189,
382.27535589701));
#30453=CARTESIAN_POINT('Ctrl Pts',(4.36497391033337,-2.98391143759783,382.19622802155));
#30454=CARTESIAN_POINT('Ctrl Pts',(2.41336099931917,-4.70450989926509,382.11710014609));
#30455=CARTESIAN_POINT('Ctrl Pts',(-0.122606802820077,-5.28599018890692,
382.03797227063));
#30456=CARTESIAN_POINT('Ctrl Pts',(-2.6288874239146,-4.58755660648474,381.958844395171));
#30457=CARTESIAN_POINT('Ctrl Pts',(-4.49862704479611,-2.77832313044165,
381.879716519711));
#30458=CARTESIAN_POINT('Ctrl Pts',(-5.04828738596174,-1.03036438158544,
381.823989439775));
#30459=CARTESIAN_POINT('Ctrl Pts',(-5.07397739854758,-0.0949146237502798,
381.794638318325));
#30460=CARTESIAN_POINT('Ctrl Pts',(-5.07389966860957,-8.89210953773471E-5,
381.791663155363));
#30461=CARTESIAN_POINT('Origin',(0.,0.,402.208336844637));
#30462=CARTESIAN_POINT('',(-5.07378290535392,0.000114313540020838,383.791663155363));
#30463=CARTESIAN_POINT('',(-5.07400033060213,4.63270069165547E-5,383.708336844637));
#30464=CARTESIAN_POINT('',(-5.0736,-1.59740085886799E-13,402.208336844637));
#30465=CARTESIAN_POINT('Ctrl Pts',(-5.07400033060213,4.63270069167923E-5,
383.708336844637));
#30466=CARTESIAN_POINT('Ctrl Pts',(-5.0740221098109,0.0454146017487004,
383.70691332995));
#30467=CARTESIAN_POINT('Ctrl Pts',(-5.06238522132993,0.931389441082911,
383.679113856776));
#30468=CARTESIAN_POINT('Ctrl Pts',(-4.57795151673967,2.64557832586642,383.624938425116));
#30469=CARTESIAN_POINT('Ctrl Pts',(-2.76192026167378,4.50871614055144,383.545810549656));
#30470=CARTESIAN_POINT('Ctrl Pts',(-0.277136335846315,5.28014395819535,
383.466682674197));
#30471=CARTESIAN_POINT('Ctrl Pts',(2.27475150580887,4.77307347049397,383.387554798736));
#30472=CARTESIAN_POINT('Ctrl Pts',(4.27584642055071,3.11028329188466,383.308426923277));
#30473=CARTESIAN_POINT('Ctrl Pts',(5.24161683545466,0.6943901771998,383.229299047817));
#30474=CARTESIAN_POINT('Ctrl Pts',(4.93821764164047,-1.8896378731662,383.150171172357));
#30475=CARTESIAN_POINT('Ctrl Pts',(3.43911186553428,-4.01612180396144,383.071043296897));
#30476=CARTESIAN_POINT('Ctrl Pts',(1.1072828290795,-5.17016919494313,382.991915421438));
#30477=CARTESIAN_POINT('Ctrl Pts',(-1.49265617402097,-5.07234682509687,
382.912787545978));
#30478=CARTESIAN_POINT('Ctrl Pts',(-3.73117351815568,-3.74634074068643,
382.833659670518));
#30479=CARTESIAN_POINT('Ctrl Pts',(-4.88103073617416,-1.82302830121342,
382.765509436738));
#30480=CARTESIAN_POINT('Ctrl Pts',(-5.07301167700312,-0.490907387666408,
382.723735161444));
#30481=CARTESIAN_POINT('Ctrl Pts',(-5.07322528972955,6.22763117691383E-5,
382.708336844637));
#30482=CARTESIAN_POINT('Ctrl Pts',(-5.07378290535392,0.000114313540020942,
383.791663155363));
#30483=CARTESIAN_POINT('Ctrl Pts',(-5.07391625780791,0.136937191492554,
383.787370613824));
#30484=CARTESIAN_POINT('Ctrl Pts',(-5.03516348602304,1.11440684342152,383.756702113798));
#30485=CARTESIAN_POINT('Ctrl Pts',(-4.42825589269063,2.88916500985471,383.699657655286));
#30486=CARTESIAN_POINT('Ctrl Pts',(-2.51417043865664,4.65141609735177,383.620529779826));
#30487=CARTESIAN_POINT('Ctrl Pts',(0.00867922154690349,5.28740478651213,
383.541401904366));
#30488=CARTESIAN_POINT('Ctrl Pts',(2.52942735381344,4.6431370825228,383.462274028906));
#30489=CARTESIAN_POINT('Ctrl Pts',(4.43771707378134,2.87461160478899,383.383146153446));
#30490=CARTESIAN_POINT('Ctrl Pts',(5.27148802998996,0.410047137522666,383.304018277987));
#30491=CARTESIAN_POINT('Ctrl Pts',(4.82885656869832,-2.15380336712922,383.224890402527));
#30492=CARTESIAN_POINT('Ctrl Pts',(3.2169984748157,-4.19614650820864,383.145762527067));
#30493=CARTESIAN_POINT('Ctrl Pts',(0.82619815304806,-5.22246314656389,383.066634651607));
#30494=CARTESIAN_POINT('Ctrl Pts',(-1.76465219517988,-4.98424792073636,
382.987506776148));
#30495=CARTESIAN_POINT('Ctrl Pts',(-3.92822160960685,-3.5391806525149,382.908378900688));
#30496=CARTESIAN_POINT('Ctrl Pts',(-4.9284760402056,-1.63999308805888,382.84309769376));
#30497=CARTESIAN_POINT('Ctrl Pts',(-5.07323479369165,-0.399520902907398,
382.804192445318));
#30498=CARTESIAN_POINT('Ctrl Pts',(-5.0731816081447,-1.92612327423736E-5,
382.791663155363));
#30499=CARTESIAN_POINT('Origin',(0.,0.,402.208336844637));
#30500=CARTESIAN_POINT('',(-5.07368788828891,-0.000125377980982264,384.791663155363));
#30501=CARTESIAN_POINT('',(-5.07341299508847,-0.000118529377325131,384.708336844637));
#30502=CARTESIAN_POINT('',(-5.0736,-1.59740085886799E-13,402.208336844637));
#30503=CARTESIAN_POINT('Ctrl Pts',(-5.07341299508847,-0.000118529377325025,
384.708336844637));
#30504=CARTESIAN_POINT('Ctrl Pts',(-5.07290585727583,0.581565929821983,
384.690091498456));
#30505=CARTESIAN_POINT('Ctrl Pts',(-4.82849439364024,2.00456420438781,384.645470193788));
#30506=CARTESIAN_POINT('Ctrl Pts',(-3.52485021126398,3.94108560628483,384.574472930633));
#30507=CARTESIAN_POINT('Ctrl Pts',(-1.21842922909547,5.14510981239459,384.495345055173));
#30508=CARTESIAN_POINT('Ctrl Pts',(1.38301395642869,5.10333196688562,384.416217179714));
#30509=CARTESIAN_POINT('Ctrl Pts',(3.64958350715001,3.82586787438508,384.337089304254));
#30510=CARTESIAN_POINT('Ctrl Pts',(5.03246761935876,1.62203404033908,384.257961428794));
#30511=CARTESIAN_POINT('Ctrl Pts',(5.19682409785237,-0.974548133184912,
384.178833553334));
#30512=CARTESIAN_POINT('Ctrl Pts',(4.10285677781212,-3.33515982055948,384.099705677875));
#30513=CARTESIAN_POINT('Ctrl Pts',(2.0154514986864,-4.88821849187982,384.020577802414));
#30514=CARTESIAN_POINT('Ctrl Pts',(-0.559961559389509,-5.25767703647906,
383.941449926955));
#30515=CARTESIAN_POINT('Ctrl Pts',(-2.99978931706339,-4.3540772640303,383.862322051495));
#30516=CARTESIAN_POINT('Ctrl Pts',(-4.68244282170845,-2.43143282852321,
383.784617690723));
#30517=CARTESIAN_POINT('Ctrl Pts',(-5.0736185681322,-0.795203160750922,
383.733289288436));
#30518=CARTESIAN_POINT('Ctrl Pts',(-5.07400033060213,4.63270069167923E-5,
383.708336844637));
#30519=CARTESIAN_POINT('Ctrl Pts',(-5.07368788828891,-0.000125377980982003,
384.791663155363));
#30520=CARTESIAN_POINT('Ctrl Pts',(-5.07300172207351,0.67292236196844,384.770548782329));
#30521=CARTESIAN_POINT('Ctrl Pts',(-4.76991529656479,2.18733716132669,384.72305845081));
#30522=CARTESIAN_POINT('Ctrl Pts',(-3.30666744538294,4.12585447040522,384.649192160803));
#30523=CARTESIAN_POINT('Ctrl Pts',(-0.93853660926441,5.20344825460853,384.570064285343));
#30524=CARTESIAN_POINT('Ctrl Pts',(1.65684512644118,5.02111431181428,384.490936409884));
#30525=CARTESIAN_POINT('Ctrl Pts',(3.85104960199139,3.62300174831864,384.411808534424));
#30526=CARTESIAN_POINT('Ctrl Pts',(5.11278700298303,1.34764007340457,384.332680658964));
#30527=CARTESIAN_POINT('Ctrl Pts',(5.13654877856401,-1.25403004379905,384.253552783504));
#30528=CARTESIAN_POINT('Ctrl Pts',(3.91658141328989,-3.55205781743347,384.174424908044));
#30529=CARTESIAN_POINT('Ctrl Pts',(1.74827954439566,-4.99001436270134,384.095297032584));
#30530=CARTESIAN_POINT('Ctrl Pts',(-0.843338895500463,-5.21972261836337,
384.016169157125));
#30531=CARTESIAN_POINT('Ctrl Pts',(-3.23075696562154,-4.18556258278454,
383.937041281665));
#30532=CARTESIAN_POINT('Ctrl Pts',(-4.74882528908407,-2.24901858620394,
383.862205947744));
#30533=CARTESIAN_POINT('Ctrl Pts',(-5.07309686007849,-0.703784911249602,
383.81374657231));
#30534=CARTESIAN_POINT('Ctrl Pts',(-5.07378290535392,0.000114313540020942,
383.791663155363));
#30535=CARTESIAN_POINT('Origin',(0.,0.,402.208336844637));
#30536=CARTESIAN_POINT('',(-5.07320349191978,4.67301704154544E-5,385.791663155363));
#30537=CARTESIAN_POINT('',(-5.07336681616767,0.000110749500208817,385.708336844637));
#30538=CARTESIAN_POINT('',(-5.0736,-1.59740085886799E-13,402.208336844637));
#30539=CARTESIAN_POINT('Ctrl Pts',(-5.07336681616767,0.000110749500209159,
385.708336844637));
#30540=CARTESIAN_POINT('Ctrl Pts',(-5.07358949400792,0.277204924762013,
385.699645625448));
#30541=CARTESIAN_POINT('Ctrl Pts',(-4.98354435800546,1.39507636552693,385.664578447772));
#30542=CARTESIAN_POINT('Ctrl Pts',(-4.1737680903862,3.24597977436508,385.60313531161));
#30543=CARTESIAN_POINT('Ctrl Pts',(-2.12031175571847,4.84365593601313,385.524007436151));
#30544=CARTESIAN_POINT('Ctrl Pts',(0.446542510511727,5.26852204647746,385.44487956069));
#30545=CARTESIAN_POINT('Ctrl Pts',(2.90527399685678,4.41770390260608,385.365751685231));
#30546=CARTESIAN_POINT('Ctrl Pts',(4.66054210967394,2.4972128487314,385.286623809771));
#30547=CARTESIAN_POINT('Ctrl Pts',(5.2873381133244,-0.0279364153108744,
385.207495934311));
#30548=CARTESIAN_POINT('Ctrl Pts',(4.63389386761938,-2.54632134491165,385.128368058852));
#30549=CARTESIAN_POINT('Ctrl Pts',(2.85842993763932,-4.44815726560116,385.049240183392));
#30550=CARTESIAN_POINT('Ctrl Pts',(0.390845137441743,-5.27294650517633,
384.970112307932));
#30551=CARTESIAN_POINT('Ctrl Pts',(-2.1713762578616,-4.82098018194518,384.890984432472));
#30552=CARTESIAN_POINT('Ctrl Pts',(-4.20783530881936,-3.2016943610792,384.811856557012));
#30553=CARTESIAN_POINT('Ctrl Pts',(-4.99079834853979,-1.35930215545066,
384.750974027734));
#30554=CARTESIAN_POINT('Ctrl Pts',(-5.07363898920769,-0.259332620176451,
384.716467456942));
#30555=CARTESIAN_POINT('Ctrl Pts',(-5.07341299508847,-0.000118529377325025,
384.708336844637));
#30556=CARTESIAN_POINT('Ctrl Pts',(-5.07320349191978,4.6730170415385E-5,
385.791663155363));
#30557=CARTESIAN_POINT('Ctrl Pts',(-5.07332318093048,0.368645452041058,
385.780102909322));
#30558=CARTESIAN_POINT('Ctrl Pts',(-4.94327787593756,1.57815905047111,385.742166704794));
#30559=CARTESIAN_POINT('Ctrl Pts',(-3.99220955212729,3.46684115546438,385.67785454178));
#30560=CARTESIAN_POINT('Ctrl Pts',(-1.85539526299902,4.95118502212943,385.59872666632));
#30561=CARTESIAN_POINT('Ctrl Pts',(0.73067187193628,5.23668247279509,385.51959879086));
#30562=CARTESIAN_POINT('Ctrl Pts',(3.13981906729605,4.25420508790564,385.440470915401));
#30563=CARTESIAN_POINT('Ctrl Pts',(4.78871173391359,2.24164328892807,385.361343039941));
#30564=CARTESIAN_POINT('Ctrl Pts',(5.27809816640793,-0.313694837508304,
385.282215164481));
#30565=CARTESIAN_POINT('Ctrl Pts',(4.48948164772799,-2.79307702006795,385.203087289022));
#30566=CARTESIAN_POINT('Ctrl Pts',(2.61381244185943,-4.59616244535579,385.123959413562));
#30567=CARTESIAN_POINT('Ctrl Pts',(0.105252389857621,-5.28636421747,385.044831538102));
#30568=CARTESIAN_POINT('Ctrl Pts',(-2.42879276314368,-4.69656155277656,
384.965703662642));
#30569=CARTESIAN_POINT('Ctrl Pts',(-4.3747464822184,-2.96956527485689,384.886575787182));
#30570=CARTESIAN_POINT('Ctrl Pts',(-5.02482764874857,-1.17623295765146,
384.828562284756));
#30571=CARTESIAN_POINT('Ctrl Pts',(-5.0738588771301,-0.167845167351579,
384.796924740816));
#30572=CARTESIAN_POINT('Ctrl Pts',(-5.07368788828891,-0.000125377980982003,
384.791663155363));
#30573=CARTESIAN_POINT('Origin',(0.,0.,402.208336844637));
#30574=CARTESIAN_POINT('',(-5.07396871057133,6.36451556410011E-5,386.791663155363));
#30575=CARTESIAN_POINT('',(-5.07402204930561,-2.85592496231871E-5,386.708336844637));
#30576=CARTESIAN_POINT('',(-5.0736,-1.59740085886799E-13,402.208336844637));
#30577=CARTESIAN_POINT('Ctrl Pts',(-5.07402204930561,-2.85592496232024E-5,
386.708336844637));
#30578=CARTESIAN_POINT('Ctrl Pts',(-5.07376894837123,0.813077680770696,
386.682823793954));
#30579=CARTESIAN_POINT('Ctrl Pts',(-4.66877404608003,2.46703434122352,386.630934784784));
#30580=CARTESIAN_POINT('Ctrl Pts',(-2.95361232316089,4.38553292227813,386.552669817127));
#30581=CARTESIAN_POINT('Ctrl Pts',(-0.504372453036948,5.26330059910421,
386.473541941668));
#30582=CARTESIAN_POINT('Ctrl Pts',(2.06699274767947,4.86664830750627,386.394414066208));
#30583=CARTESIAN_POINT('Ctrl Pts',(4.1378703204085,3.29161874757629,386.315286190749));
#30584=CARTESIAN_POINT('Ctrl Pts',(5.20683199193,0.919578912180737,386.236158315288));
#30585=CARTESIAN_POINT('Ctrl Pts',(5.01504662121074,-1.67512153439562,386.157030439829));
#30586=CARTESIAN_POINT('Ctrl Pts',(3.60895181930755,-3.86421939514695,386.077902564369));
#30587=CARTESIAN_POINT('Ctrl Pts',(1.32900986066236,-5.11766133679979,385.998774688909));
#30588=CARTESIAN_POINT('Ctrl Pts',(-1.2727295467071,-5.13194741485647,385.91964681345));
#30589=CARTESIAN_POINT('Ctrl Pts',(-3.5662988394905,-3.90361849510962,385.84051893799));
#30590=CARTESIAN_POINT('Ctrl Pts',(-4.83927537814081,-1.96882864770619,
385.770082281719));
#30591=CARTESIAN_POINT('Ctrl Pts',(-5.07291371523136,-0.563715584161085,
385.726021583935));
#30592=CARTESIAN_POINT('Ctrl Pts',(-5.07336681616767,0.000110749500209159,
385.708336844637));
#30593=CARTESIAN_POINT('Ctrl Pts',(-5.07396871057133,6.36451556408537E-5,
386.791663155363));
#30594=CARTESIAN_POINT('Ctrl Pts',(-5.07400891965194,0.0640010310039327,
386.789657036314));
#30595=CARTESIAN_POINT('Ctrl Pts',(-5.05726353871135,0.968550309919132,
386.761274958779));
#30596=CARTESIAN_POINT('Ctrl Pts',(-4.54862274572651,2.695692085973,386.706516922757));
#30597=CARTESIAN_POINT('Ctrl Pts',(-2.71224074091265,4.53877459989496,386.627389047297));
#30598=CARTESIAN_POINT('Ctrl Pts',(-0.219135128106394,5.28286896496098,
386.548261171838));
#30599=CARTESIAN_POINT('Ctrl Pts',(2.32703038082081,4.74780520999492,386.469133296378));
#30600=CARTESIAN_POINT('Ctrl Pts',(4.30974451002784,3.06314004962277,386.390005420918));
#30601=CARTESIAN_POINT('Ctrl Pts',(5.24892628554031,0.636786898642001,386.310877545458));
#30602=CARTESIAN_POINT('Ctrl Pts',(4.91716859158436,-1.94375352019086,386.231749669999));
#30603=CARTESIAN_POINT('Ctrl Pts',(3.39480098979053,-4.05364662310803,386.152621794539));
#30604=CARTESIAN_POINT('Ctrl Pts',(1.05043926306477,-5.18201718059,386.073493919079));
#30605=CARTESIAN_POINT('Ctrl Pts',(-1.54826871412865,-5.0556491862241,385.994366043619));
#30606=CARTESIAN_POINT('Ctrl Pts',(-3.772089388456,-3.70514053050835,385.91523816816));
#30607=CARTESIAN_POINT('Ctrl Pts',(-4.89110742269369,-1.78586579845603,
385.84767053874));
#30608=CARTESIAN_POINT('Ctrl Pts',(-5.07305009743672,-0.472352615975399,
385.806478867808));
#30609=CARTESIAN_POINT('Ctrl Pts',(-5.07320349191978,4.6730170415385E-5,
385.791663155363));
#30610=CARTESIAN_POINT('Origin',(0.,0.,402.208336844637));
#30611=CARTESIAN_POINT('',(-5.07346461004462,-0.000124534794222197,387.791663155363));
#30612=CARTESIAN_POINT('',(-5.07325209134275,-7.62409538748165E-5,387.708336844637));
#30613=CARTESIAN_POINT('',(-5.0736,-1.59740085886799E-13,402.208336844637));
#30614=CARTESIAN_POINT('Ctrl Pts',(-5.07325209134275,-7.62409538748038E-5,
387.708336844637));
#30615=CARTESIAN_POINT('Ctrl Pts',(-5.0729792152731,0.508760470280088,387.692377920946));
#30616=CARTESIAN_POINT('Ctrl Pts',(-4.87111972002504,1.85878392032608,387.650043038769));
#30617=CARTESIAN_POINT('Ctrl Pts',(-3.69137763771595,3.78555886279474,387.581332198105));
#30618=CARTESIAN_POINT('Ctrl Pts',(-1.43897337649567,5.08783651365194,387.502204322645));
#30619=CARTESIAN_POINT('Ctrl Pts',(1.16185415459233,5.15817988164137,387.423076447186));
#30620=CARTESIAN_POINT('Ctrl Pts',(3.48135818778607,3.97955649994419,387.343948571725));
#30621=CARTESIAN_POINT('Ctrl Pts',(4.95790972221771,1.83735025355874,387.264820696266));
#30622=CARTESIAN_POINT('Ctrl Pts',(5.23398656730458,-0.749739542233496,
387.185692820806));
#30623=CARTESIAN_POINT('Ctrl Pts',(4.24274134513742,-3.15529248187465,387.106564945346));
#30624=CARTESIAN_POINT('Ctrl Pts',(2.22418746193322,-4.79684426494046,387.027437069886));
#30625=CARTESIAN_POINT('Ctrl Pts',(-0.332916112977428,-5.27692065788687,
386.948309194427));
#30626=CARTESIAN_POINT('Ctrl Pts',(-2.80940963451955,-4.47927921359921,
386.869181318967));
#30627=CARTESIAN_POINT('Ctrl Pts',(-4.6056517301173,-2.59705543044056,386.790053443507));
#30628=CARTESIAN_POINT('Ctrl Pts',(-5.06711936969965,-0.895633636916161,
386.73643861873));
#30629=CARTESIAN_POINT('Ctrl Pts',(-5.07403060973901,-0.0275296106999626,
386.70919975244));
#30630=CARTESIAN_POINT('Ctrl Pts',(-5.07402204930561,-2.85592496232024E-5,
386.708336844637));
#30631=CARTESIAN_POINT('Ctrl Pts',(-5.07346461004462,-0.000124534794222232,
387.791663155363));
#30632=CARTESIAN_POINT('Ctrl Pts',(-5.07290587442459,0.600116546096426,
387.77283520482));
#30633=CARTESIAN_POINT('Ctrl Pts',(-4.81706146775411,2.04169530250574,387.727631295791));
#30634=CARTESIAN_POINT('Ctrl Pts',(-3.48135818389009,3.97955649548785,387.656051428275));
#30635=CARTESIAN_POINT('Ctrl Pts',(-1.16185415329344,5.15817987586638,387.576923552815));
#30636=CARTESIAN_POINT('Ctrl Pts',(1.43897337488296,5.0878365079566,387.497795677355));
#30637=CARTESIAN_POINT('Ctrl Pts',(3.69137763358211,3.7855588585581,387.418667801895));
#30638=CARTESIAN_POINT('Ctrl Pts',(5.04997670698908,1.56667161976776,387.339539926436));
#30639=CARTESIAN_POINT('Ctrl Pts',(5.1858086147589,-1.03155887685117,387.260412050976));
#30640=CARTESIAN_POINT('Ctrl Pts',(4.06598393848355,-3.38001469187811,387.181284175516));
#30641=CARTESIAN_POINT('Ctrl Pts',(1.96164944276588,-4.91005663602919,387.102156300056));
#30642=CARTESIAN_POINT('Ctrl Pts',(-0.617665566383616,-5.25121071310437,
387.023028424596));
#30643=CARTESIAN_POINT('Ctrl Pts',(-3.04742321760052,-4.32087218488899,
386.943900549136));
#30644=CARTESIAN_POINT('Ctrl Pts',(-4.69640454618417,-2.39441853297418,
386.866778792725));
#30645=CARTESIAN_POINT('Ctrl Pts',(-5.07348026057684,-0.776631949401611,
386.816032994801));
#30646=CARTESIAN_POINT('Ctrl Pts',(-5.07396871057133,6.36451556408537E-5,
386.791663155363));
#30647=CARTESIAN_POINT('Origin',(0.,0.,402.208336844637));
#30648=CARTESIAN_POINT('',(-5.07332308908166,0.000100751512192854,388.791663155363));
#30649=CARTESIAN_POINT('',(-5.07357378438926,0.00012964408007953,388.708336844637));
#30650=CARTESIAN_POINT('',(-5.0736,-1.59740085886799E-13,402.208336844637));
#30651=CARTESIAN_POINT('Ctrl Pts',(-5.07357378438926,0.000129644080079632,
388.708336844637));
#30652=CARTESIAN_POINT('Ctrl Pts',(-5.07377922823885,0.204303981988881,
388.701932047939));
#30653=CARTESIAN_POINT('Ctrl Pts',(-5.01188528533374,1.24917654214382,388.669151292754));
#30654=CARTESIAN_POINT('Ctrl Pts',(-4.30974451485365,3.06314005305047,388.609994579082));
#30655=CARTESIAN_POINT('Ctrl Pts',(-2.32703038342756,4.74780521530929,388.530866703622));
#30656=CARTESIAN_POINT('Ctrl Pts',(0.2191351283499,5.28286897087523,388.451738828163));
#30657=CARTESIAN_POINT('Ctrl Pts',(2.71224074394742,4.53877460497707,388.372610952702));
#30658=CARTESIAN_POINT('Ctrl Pts',(4.54862275081774,2.69569208899244,388.293483077243));
#30659=CARTESIAN_POINT('Ctrl Pts',(5.28363204425109,0.199892943537846,388.214355201783));
#30660=CARTESIAN_POINT('Ctrl Pts',(4.73929845080001,-2.34430692575821,388.135227326323));
#30661=CARTESIAN_POINT('Ctrl Pts',(3.04742322101362,-4.32087218972514,388.056099450863));
#30662=CARTESIAN_POINT('Ctrl Pts',(0.617665567076949,-5.25121071898288,
387.976971575404));
#30663=CARTESIAN_POINT('Ctrl Pts',(-1.96164944496022,-4.9100566415267,387.897843699944));
#30664=CARTESIAN_POINT('Ctrl Pts',(-4.06598394303424,-3.38001469566346,
387.818715824484));
#30665=CARTESIAN_POINT('Ctrl Pts',(-4.95995652391698,-1.50520772763894,
387.755546872715));
#30666=CARTESIAN_POINT('Ctrl Pts',(-5.07343020858722,-0.332214537305361,
387.718753879433));
#30667=CARTESIAN_POINT('Ctrl Pts',(-5.07325209134275,-7.62409538748038E-5,
387.708336844637));
#30668=CARTESIAN_POINT('Ctrl Pts',(-5.07332308908166,0.000100751512193097,
388.791663155363));
#30669=CARTESIAN_POINT('Ctrl Pts',(-5.07353661258784,0.295776873009828,
388.782389331812));
#30670=CARTESIAN_POINT('Ctrl Pts',(-4.97579423080698,1.43225469143156,388.746739549775));
#30671=CARTESIAN_POINT('Ctrl Pts',(-4.13787031577727,3.29161874388992,388.684713809251));
#30672=CARTESIAN_POINT('Ctrl Pts',(-2.0669927453671,4.86664830205737,388.605585933792));
#30673=CARTESIAN_POINT('Ctrl Pts',(0.504372452470541,5.2633005932121,388.526458058332));
#30674=CARTESIAN_POINT('Ctrl Pts',(2.95361231985281,4.38553291736953,388.447330182872));
#30675=CARTESIAN_POINT('Ctrl Pts',(4.68768449948338,2.44588199605403,388.368202307412));
#30676=CARTESIAN_POINT('Ctrl Pts',(5.28671249546426,-0.0859982303311033,
388.289074431953));
#30677=CARTESIAN_POINT('Ctrl Pts',(4.60565172496217,-2.59705542753155,388.209946556493));
#30678=CARTESIAN_POINT('Ctrl Pts',(2.80940963137597,-4.47927920858367,388.130818681033));
#30679=CARTESIAN_POINT('Ctrl Pts',(0.332916112606594,-5.27692065197923,
388.051690805573));
#30680=CARTESIAN_POINT('Ctrl Pts',(-2.22418745944155,-4.79684425957118,
387.972562930114));
#30681=CARTESIAN_POINT('Ctrl Pts',(-4.24274134038657,-3.15529247834378,
387.893435054654));
#30682=CARTESIAN_POINT('Ctrl Pts',(-4.99812636818859,-1.3221248286521,387.833135129737));
#30683=CARTESIAN_POINT('Ctrl Pts',(-5.07368860366989,-0.240757440453781,
387.799211163307));
#30684=CARTESIAN_POINT('Ctrl Pts',(-5.07346461004462,-0.000124534794222232,
387.791663155363));
#30685=CARTESIAN_POINT('Origin',(0.,0.,402.208336844637));
#30686=CARTESIAN_POINT('',(-5.07403406771079,-9.36144982375056E-6,389.791663155363));
#30687=CARTESIAN_POINT('',(-5.07388549569213,-9.2912700738374E-5,389.708336844637));
#30688=CARTESIAN_POINT('',(-5.0736,-1.59740085886799E-13,402.208336844637));
#30689=CARTESIAN_POINT('Ctrl Pts',(-5.07388549569213,-9.2912700738277E-5,
389.708336844637));
#30690=CARTESIAN_POINT('Ctrl Pts',(-5.07325856807114,0.740202389523463,
389.685110216444));
#30691=CARTESIAN_POINT('Ctrl Pts',(-4.72308495981242,2.32174429013103,389.635507629765));
#30692=CARTESIAN_POINT('Ctrl Pts',(-3.13981907081257,4.25420509266713,389.559529084599));
#30693=CARTESIAN_POINT('Ctrl Pts',(-0.730671872756092,5.23668247865729,
389.48040120914));
#30694=CARTESIAN_POINT('Ctrl Pts',(1.85539526507438,4.95118502767294,389.401273333679));
#30695=CARTESIAN_POINT('Ctrl Pts',(3.99220955659535,3.46684115934693,389.32214545822));
#30696=CARTESIAN_POINT('Ctrl Pts',(5.16237725796638,1.14305984722794,389.24301758276));
#30697=CARTESIAN_POINT('Ctrl Pts',(5.08256188536855,-1.45749423645932,389.1638897073));
#30698=CARTESIAN_POINT('Ctrl Pts',(3.77208939268016,-3.70514053465492,389.08476183184));
#30699=CARTESIAN_POINT('Ctrl Pts',(1.54826871586373,-5.05564919188336,389.005633956381));
#30700=CARTESIAN_POINT('Ctrl Pts',(-1.05043926423896,-5.18201718639165,
388.926506080921));
#30701=CARTESIAN_POINT('Ctrl Pts',(-3.39480099358967,-4.05364662764723,
388.847378205461));
#30702=CARTESIAN_POINT('Ctrl Pts',(-4.79394457591898,-2.1145332421108,388.7746551267));
#30703=CARTESIAN_POINT('Ctrl Pts',(-5.07293317820744,-0.636518001009154,
388.728308006425));
#30704=CARTESIAN_POINT('Ctrl Pts',(-5.07357378438926,0.000129644080079632,
388.708336844637));
#30705=CARTESIAN_POINT('Ctrl Pts',(-5.07403406771079,-9.36144982382212E-6,
389.791663155363));
#30706=CARTESIAN_POINT('Ctrl Pts',(-5.07394412729799,0.831658855747162,
389.765567500318));
#30707=CARTESIAN_POINT('Ctrl Pts',(-4.65432422371577,2.50401601420859,389.713095886787));
#30708=CARTESIAN_POINT('Ctrl Pts',(-2.90527399360582,4.41770389765948,389.634248314769));
#30709=CARTESIAN_POINT('Ctrl Pts',(-0.446542510013585,5.2685220405792,389.55512043931));
#30710=CARTESIAN_POINT('Ctrl Pts',(2.12031175334316,4.84365593059135,389.475992563849));
#30711=CARTESIAN_POINT('Ctrl Pts',(4.17376808571255,3.24597977073262,389.39686468839));
#30712=CARTESIAN_POINT('Ctrl Pts',(5.21661647505316,0.862344048232485,389.31773681293));
#30713=CARTESIAN_POINT('Ctrl Pts',(4.99634867366186,-1.73009382303836,389.23860893747));
#30714=CARTESIAN_POINT('Ctrl Pts',(3.56629883549932,-3.90361849073832,389.15948106201));
#30715=CARTESIAN_POINT('Ctrl Pts',(1.27272954528402,-5.13194740911081,389.08035318655));
#30716=CARTESIAN_POINT('Ctrl Pts',(-1.3290098591728,-5.11766133107102,389.001225311091));
#30717=CARTESIAN_POINT('Ctrl Pts',(-3.60895181526604,-3.86421939082217,
388.922097435631));
#30718=CARTESIAN_POINT('Ctrl Pts',(-4.85025165556801,-1.93168481258741,
388.852243383721));
#30719=CARTESIAN_POINT('Ctrl Pts',(-5.07292932400786,-0.545164413360684,
388.808765290299));
#30720=CARTESIAN_POINT('Ctrl Pts',(-5.07332308908166,0.000100751512193097,
388.791663155363));
#30721=CARTESIAN_POINT('Origin',(0.,0.,402.208336844637));
#30722=CARTESIAN_POINT('',(-5.0732856633921,-8.9472558095216E-5,390.791663155363));
#30723=CARTESIAN_POINT('',(-5.07317963304504,-1.41915822972106E-5,390.708336844637));
#30724=CARTESIAN_POINT('',(-5.0736,-1.59740085886799E-13,402.208336844637));
#30725=CARTESIAN_POINT('Ctrl Pts',(-5.07317963304504,-1.41915822972002E-5,
390.708336844637));
#30726=CARTESIAN_POINT('Ctrl Pts',(-5.07313689101218,0.435939705489138,
390.694664343437));
#30727=CARTESIAN_POINT('Ctrl Pts',(-4.9102234101679,1.71293434968472,390.65461588375));
#30728=CARTESIAN_POINT('Ctrl Pts',(-3.85104960630393,3.62300175237324,390.588191465576));
#30729=CARTESIAN_POINT('Ctrl Pts',(-1.65684512829777,5.02111431743484,390.509063590116));
#30730=CARTESIAN_POINT('Ctrl Pts',(0.938536610313288,5.20344826043412,390.429935714657));
#30731=CARTESIAN_POINT('Ctrl Pts',(3.30666744908329,4.12585447502528,390.350807839197));
#30732=CARTESIAN_POINT('Ctrl Pts',(4.874144221702,2.04925422384882,390.271679963737));
#30733=CARTESIAN_POINT('Ctrl Pts',(5.26142871608132,-0.523538569265068,
390.192552088277));
#30734=CARTESIAN_POINT('Ctrl Pts',(4.37474648711696,-2.96956527817979,390.113424212818));
#30735=CARTESIAN_POINT('Ctrl Pts',(2.42879276586438,-4.69656155803349,390.034296337358));
#30736=CARTESIAN_POINT('Ctrl Pts',(-0.105252389973582,-5.28636422338813,
389.955168461898));
#30737=CARTESIAN_POINT('Ctrl Pts',(-2.61381244478399,-4.59616245050211,
389.876040586438));
#30738=CARTESIAN_POINT('Ctrl Pts',(-4.48948165275299,-2.79307702319636,
389.796912710979));
#30739=CARTESIAN_POINT('Ctrl Pts',(-5.04661334373894,-1.04147487532298,
389.741011463711));
#30740=CARTESIAN_POINT('Ctrl Pts',(-5.07397050166598,-0.10047056555588,
389.711486174931));
#30741=CARTESIAN_POINT('Ctrl Pts',(-5.07388549569213,-9.2912700738277E-5,
389.708336844637));
#30742=CARTESIAN_POINT('Ctrl Pts',(-5.0732856633921,-8.94725580950079E-5,
390.791663155363));
#30743=CARTESIAN_POINT('Ctrl Pts',(-5.07295082938292,0.527313084285289,
390.77512162731));
#30744=CARTESIAN_POINT('Ctrl Pts',(-4.86059546998445,1.89593815106623,390.732204140772));
#30745=CARTESIAN_POINT('Ctrl Pts',(-3.64958350306562,3.82586787010077,390.662910695746));
#30746=CARTESIAN_POINT('Ctrl Pts',(-1.38301395488213,5.10333196117197,390.583782820286));
#30747=CARTESIAN_POINT('Ctrl Pts',(1.21842922772966,5.14510980663504,390.504654944826));
#30748=CARTESIAN_POINT('Ctrl Pts',(3.52485020731651,3.94108560187402,390.425527069367));
#30749=CARTESIAN_POINT('Ctrl Pts',(4.97778782502355,1.78279361519087,390.346399193907));
#30750=CARTESIAN_POINT('Ctrl Pts',(5.2254376041702,-0.807171945896316,390.267271318447));
#30751=CARTESIAN_POINT('Ctrl Pts',(4.2078353041098,-3.20169435749343,390.188143442988));
#30752=CARTESIAN_POINT('Ctrl Pts',(2.17137625543244,-4.82098017654731,390.109015567527));
#30753=CARTESIAN_POINT('Ctrl Pts',(-0.390845137002325,-5.27294649927341,
390.029887692068));
#30754=CARTESIAN_POINT('Ctrl Pts',(-2.85842993443779,-4.44815726062243,
389.950759816608));
#30755=CARTESIAN_POINT('Ctrl Pts',(-4.63389386243089,-2.54632134206259,
389.871631941148));
#30756=CARTESIAN_POINT('Ctrl Pts',(-5.07183812704173,-0.858476903537314,
389.818599720733));
#30757=CARTESIAN_POINT('Ctrl Pts',(-5.07403503379527,-0.00894262882346251,
389.791943458805));
#30758=CARTESIAN_POINT('Ctrl Pts',(-5.07403406771079,-9.36144982382212E-6,
389.791663155363));
#30759=CARTESIAN_POINT('Origin',(0.,0.,402.208336844637));
#30760=CARTESIAN_POINT('',(-5.07351709598447,0.000128180283586465,391.791663155363));
#30761=CARTESIAN_POINT('',(-5.07379939980891,0.000111618004047815,391.708336844637));
#30762=CARTESIAN_POINT('',(-5.0736,-1.59740085886799E-13,402.208336844637));
#30763=CARTESIAN_POINT('Ctrl Pts',(-5.07379939980891,0.000111618004048301,
391.708336844637));
#30764=CARTESIAN_POINT('Ctrl Pts',(-5.07392549945089,0.131381756589591,
391.704218470429));
#30765=CARTESIAN_POINT('Ctrl Pts',(-5.03695972030326,1.10329526429473,391.673724137734));
#30766=CARTESIAN_POINT('Ctrl Pts',(-4.43771707875037,2.8746116080056,391.616853846554));
#30767=CARTESIAN_POINT('Ctrl Pts',(-2.52942735664669,4.64313708771996,391.537725971094));
#30768=CARTESIAN_POINT('Ctrl Pts',(-0.00867922155838994,5.28740479243137,
391.458598095634));
#30769=CARTESIAN_POINT('Ctrl Pts',(2.51417044146968,4.65141610255989,391.379470220174));
#30770=CARTESIAN_POINT('Ctrl Pts',(4.42825589764708,2.88916501309064,391.300342344714));
#30771=CARTESIAN_POINT('Ctrl Pts',(5.27011345519119,0.427351070346123,391.221214469255));
#30772=CARTESIAN_POINT('Ctrl Pts',(4.8359014254693,-2.1379387669101,391.142086593795));
#30773=CARTESIAN_POINT('Ctrl Pts',(3.23075696923981,-4.18556258746916,391.062958718335));
#30774=CARTESIAN_POINT('Ctrl Pts',(0.843338896446427,-5.21972262420654,
390.983830842875));
#30775=CARTESIAN_POINT('Ctrl Pts',(-1.7482795463511,-4.99001436828829,390.904702967415));
#30776=CARTESIAN_POINT('Ctrl Pts',(-3.91658141767327,-3.55205782141137,
390.825575091956));
#30777=CARTESIAN_POINT('Ctrl Pts',(-4.92575069087544,-1.65110613686035,
390.760119717696));
#30778=CARTESIAN_POINT('Ctrl Pts',(-5.07321934571947,-0.405069684288436,
390.721040301923));
#30779=CARTESIAN_POINT('Ctrl Pts',(-5.07317963304504,-1.41915822972002E-5,
390.708336844637));
#30780=CARTESIAN_POINT('Ctrl Pts',(-5.07351709598447,0.0001281802835865,
391.791663155363));
#30781=CARTESIAN_POINT('Ctrl Pts',(-5.07373426530186,0.222882138466162,
391.784675754303));
#30782=CARTESIAN_POINT('Ctrl Pts',(-5.00497588579108,1.28635201118677,391.751312394756));
#30783=CARTESIAN_POINT('Ctrl Pts',(-4.27584641576499,3.1102832884012,391.691573076723));
#30784=CARTESIAN_POINT('Ctrl Pts',(-2.27475150326393,4.77307346514974,391.612445201264));
#30785=CARTESIAN_POINT('Ctrl Pts',(0.277136335534271,5.28014395228432,391.533317325804));
#30786=CARTESIAN_POINT('Ctrl Pts',(2.76192025858026,4.50871613550486,391.454189450344));
#30787=CARTESIAN_POINT('Ctrl Pts',(4.57795151161372,2.64557832290629,391.375061574885));
#30788=CARTESIAN_POINT('Ctrl Pts',(5.28550858366077,0.141858088829558,391.295933699424));
#30789=CARTESIAN_POINT('Ctrl Pts',(4.71326839627705,-2.39621070233275,391.216805823965));
#30790=CARTESIAN_POINT('Ctrl Pts',(2.99978931370662,-4.35407725915487,391.137677948505));
#30791=CARTESIAN_POINT('Ctrl Pts',(0.559961558764467,-5.2576770305929,391.058550073045));
#30792=CARTESIAN_POINT('Ctrl Pts',(-2.01545149642842,-4.88821848640817,
390.979422197585));
#30793=CARTESIAN_POINT('Ctrl Pts',(-4.10285677321784,-3.33515981682715,
390.900294322126));
#30794=CARTESIAN_POINT('Ctrl Pts',(-4.96813235745424,-1.46802940120253,
390.837707974718));
#30795=CARTESIAN_POINT('Ctrl Pts',(-5.07348473216978,-0.313645979534272,
390.801497585797));
#30796=CARTESIAN_POINT('Ctrl Pts',(-5.0732856633921,-8.94725580950079E-5,
390.791663155363));
#30797=CARTESIAN_POINT('Origin',(0.,0.,402.208336844637));
#30798=CARTESIAN_POINT('',(-5.07393095917883,-7.88724074329838E-5,392.791663155363));
#30799=CARTESIAN_POINT('',(-5.07367047787857,-0.000126645267990005,392.708336844637));
#30800=CARTESIAN_POINT('',(-5.0736,-1.59740085886799E-13,402.208336844637));
#30801=CARTESIAN_POINT('Ctrl Pts',(-5.07367047787857,-0.000126645267989993,
392.708336844637));
#30802=CARTESIAN_POINT('Ctrl Pts',(-5.07298837013062,0.667375891727513,
392.687396638935));
#30803=CARTESIAN_POINT('Ctrl Pts',(-4.77363543308555,2.17624796267435,392.640080474746));
#30804=CARTESIAN_POINT('Ctrl Pts',(-3.32019468996614,4.11497654776232,392.566388352071));
#30805=CARTESIAN_POINT('Ctrl Pts',(-0.955614322062658,5.20033903081154,
392.487260476611));
#30806=CARTESIAN_POINT('Ctrl Pts',(1.64035202716895,5.02652663326038,392.408132601151));
#30807=CARTESIAN_POINT('Ctrl Pts',(3.83913464362559,3.63562511214056,392.329004725691));
#30808=CARTESIAN_POINT('Ctrl Pts',(5.10833519286426,1.36441794376124,392.249876850232));
#30809=CARTESIAN_POINT('Ctrl Pts',(5.14063804785052,-1.23716014683014,392.170748974772));
#30810=CARTESIAN_POINT('Ctrl Pts',(3.92822161400576,-3.53918065647562,392.091621099312));
#30811=CARTESIAN_POINT('Ctrl Pts',(1.76465219715718,-4.98424792631562,392.012493223852));
#30812=CARTESIAN_POINT('Ctrl Pts',(-0.826198153971171,-5.22246315241074,
391.933365348392));
#30813=CARTESIAN_POINT('Ctrl Pts',(-3.21699847841567,-4.19614651290735,
391.854237472933));
#30814=CARTESIAN_POINT('Ctrl Pts',(-4.74496408021847,-2.26010134957161,
391.779227971681));
#30815=CARTESIAN_POINT('Ctrl Pts',(-5.07311789947229,-0.7093324551461,391.730594428916));
#30816=CARTESIAN_POINT('Ctrl Pts',(-5.07379939980891,0.000111618004048301,
391.708336844637));
#30817=CARTESIAN_POINT('Ctrl Pts',(-5.07393095917883,-7.88724074328884E-5,
392.791663155363));
#30818=CARTESIAN_POINT('Ctrl Pts',(-5.07336361274665,0.758765898971362,
392.767853922809));
#30819=CARTESIAN_POINT('Ctrl Pts',(-4.7096061531202,2.35878746105711,392.717668731768));
#30820=CARTESIAN_POINT('Ctrl Pts',(-3.09291170420029,4.28842883762094,392.64110758224));
#30821=CARTESIAN_POINT('Ctrl Pts',(-0.67312059357683,5.24439065781915,392.561979706781));
#30822=CARTESIAN_POINT('Ctrl Pts',(1.90965537976903,4.9305112347339,392.482851831321));
#30823=CARTESIAN_POINT('Ctrl Pts',(4.03004033003705,3.4227912065437,392.403723955861));
#30824=CARTESIAN_POINT('Ctrl Pts',(5.17461860283211,1.0862996918631,392.324596080401));
#30825=CARTESIAN_POINT('Ctrl Pts',(5.06624976530063,-1.51322107469774,392.245468204942));
#30826=CARTESIAN_POINT('Ctrl Pts',(3.73117351397988,-3.74634073649114,392.166340329482));
#30827=CARTESIAN_POINT('Ctrl Pts',(1.49265617235166,-5.07234681941786,392.087212454022));
#30828=CARTESIAN_POINT('Ctrl Pts',(-1.10728282783815,-5.1701691891555,392.008084578562));
#30829=CARTESIAN_POINT('Ctrl Pts',(-3.43911186168285,-4.01612179946654,
391.928956703103));
#30830=CARTESIAN_POINT('Ctrl Pts',(-4.80583883513493,-2.07741741105628,
391.856816228703));
#30831=CARTESIAN_POINT('Ctrl Pts',(-5.07291449714329,-0.617966855796078,
391.811051712789));
#30832=CARTESIAN_POINT('Ctrl Pts',(-5.07351709598447,0.0001281802835865,
391.791663155363));
#30833=CARTESIAN_POINT('Origin',(0.,0.,402.208336844637));
#30834=CARTESIAN_POINT('',(-5.07318860167667,-3.10232113821807E-5,393.791663155363));
#30835=CARTESIAN_POINT('',(-5.07320934784751,5.14726455261062E-5,393.708336844637));
#30836=CARTESIAN_POINT('',(-5.0736,-1.59740085886799E-13,402.208336844637));
#30837=CARTESIAN_POINT('Ctrl Pts',(-5.07320934784751,5.14726455259906E-5,
393.708336844637));
#30838=CARTESIAN_POINT('Ctrl Pts',(-5.07333938414724,0.363095667172288,
393.696950765927));
#30839=CARTESIAN_POINT('Ctrl Pts',(-4.94587345760415,1.56704518273248,393.659188728731));
#30840=CARTESIAN_POINT('Ctrl Pts',(-4.00356958154437,3.45371616865744,393.595050733048));
#30841=CARTESIAN_POINT('Ctrl Pts',(-1.8716398630404,4.94506713715712,393.515922857588));
#30842=CARTESIAN_POINT('Ctrl Pts',(0.713476058729831,5.23905303289941,393.436794982128));
#30843=CARTESIAN_POINT('Ctrl Pts',(3.12583571869877,4.26449010171441,393.357667106669));
#30844=CARTESIAN_POINT('Ctrl Pts',(4.78132668327137,2.25735241283907,393.278539231209));
#30845=CARTESIAN_POINT('Ctrl Pts',(5.2790995798779,-0.296365304389928,393.199411355749));
#30846=CARTESIAN_POINT('Ctrl Pts',(4.49862704983328,-2.77832313355043,393.120283480289));
#30847=CARTESIAN_POINT('Ctrl Pts',(2.62888742685924,-4.58755661161959,393.041155604829));
#30848=CARTESIAN_POINT('Ctrl Pts',(0.122606802959192,-5.28599019482455,
392.96202772937));
#30849=CARTESIAN_POINT('Ctrl Pts',(-2.41336100201929,-4.70450990453263,
392.88289985391));
#30850=CARTESIAN_POINT('Ctrl Pts',(-4.3649739152189,-2.98391144093985,392.80377197845));
#30851=CARTESIAN_POINT('Ctrl Pts',(-5.02290836650147,-1.18734550240995,
392.745584308693));
#30852=CARTESIAN_POINT('Ctrl Pts',(-5.07384754247588,-0.173399956222615,
392.713772597422));
#30853=CARTESIAN_POINT('Ctrl Pts',(-5.07367047787857,-0.000126645267989993,
392.708336844637));
#30854=CARTESIAN_POINT('Ctrl Pts',(-5.07318860167666,-3.10232113822501E-5,
393.791663155363));
#30855=CARTESIAN_POINT('Ctrl Pts',(-5.07309097404724,0.454497176795154,
393.777408049801));
#30856=CARTESIAN_POINT('Ctrl Pts',(-4.90058989979703,1.75010317897161,393.736776985753));
#30857=CARTESIAN_POINT('Ctrl Pts',(-3.81103098253419,3.66507401773587,393.669769963218));
#30858=CARTESIAN_POINT('Ctrl Pts',(-1.60160528615343,5.03900637156607,393.590642087758));
#30859=CARTESIAN_POINT('Ctrl Pts',(0.995622269493122,5.19282784249655,393.511514212298));
#30860=CARTESIAN_POINT('Ctrl Pts',(3.3517765903209,4.08929314110579,393.432386336838));
#30861=CARTESIAN_POINT('Ctrl Pts',(4.89635442297923,1.99560468778007,393.353258461378));
#30862=CARTESIAN_POINT('Ctrl Pts',(5.2553621496497,-0.581285972088894,393.274130585919));
#30863=CARTESIAN_POINT('Ctrl Pts',(4.34187207029457,-3.01742798265574,393.195002710459));
#30864=CARTESIAN_POINT('Ctrl Pts',(2.37707048734272,-4.72295041298575,393.115874834999));
#30865=CARTESIAN_POINT('Ctrl Pts',(-0.163298847893048,-5.28488961016167,
393.03674695954));
#30866=CARTESIAN_POINT('Ctrl Pts',(-2.66412810582239,-4.56718142195876,
392.957619084079));
#30867=CARTESIAN_POINT('Ctrl Pts',(-4.51988342344183,-2.74360684935247,
392.87849120862));
#30868=CARTESIAN_POINT('Ctrl Pts',(-5.05214048257081,-1.00431002992741,
392.823172565714));
#30869=CARTESIAN_POINT('Ctrl Pts',(-5.07399212128462,-0.0818852283646697,
392.794229881295));
#30870=CARTESIAN_POINT('Ctrl Pts',(-5.07393095917883,-7.88724074328884E-5,
392.791663155363));
#30871=CARTESIAN_POINT('Origin',(0.,0.,402.208336844637));
#30872=CARTESIAN_POINT('',(-5.07374340439062,0.000119799015104727,394.791663155363));
#30873=CARTESIAN_POINT('',(-5.07397904538501,5.86126803115486E-5,394.708336844637));
#30874=CARTESIAN_POINT('',(-5.0736,-1.59740085886799E-13,402.208336844637));
#30875=CARTESIAN_POINT('Ctrl Pts',(-5.07397904538501,5.86126803111056E-5,
394.708336844637));
#30876=CARTESIAN_POINT('Ctrl Pts',(-5.07401332726156,0.0584447346541764,
394.706504892919));
#30877=CARTESIAN_POINT('Ctrl Pts',(-5.05881623778616,0.957440994697868,
394.678296982715));
#30878=CARTESIAN_POINT('Ctrl Pts',(-4.55744811727866,2.68074456564335,394.623713114025));
#30879=CARTESIAN_POINT('Ctrl Pts',(-2.72712679296628,4.52984593810856,394.544585238565));
#30880=CARTESIAN_POINT('Ctrl Pts',(-0.236477452813074,5.28212108742541,
394.465457363106));
#30881=CARTESIAN_POINT('Ctrl Pts',(2.31143093653793,4.75541920271268,394.386329487645));
#30882=CARTESIAN_POINT('Ctrl Pts',(4.29966508998112,3.07727231195273,394.307201612186));
#30883=CARTESIAN_POINT('Ctrl Pts',(5.2468074522505,0.654015540275394,394.228073736726));
#30884=CARTESIAN_POINT('Ctrl Pts',(4.92352338499734,-1.92760012588128,394.148945861266));
#30885=CARTESIAN_POINT('Ctrl Pts',(3.40809070325859,-4.04247974964323,394.069817985806));
#30886=CARTESIAN_POINT('Ctrl Pts',(1.06744601535546,-5.17854069909805,393.990690110347));
#30887=CARTESIAN_POINT('Ctrl Pts',(-1.53166282285958,-5.06070486839363,
393.911562234887));
#30888=CARTESIAN_POINT('Ctrl Pts',(-3.75990519627929,-3.71750422769163,
393.832434359427));
#30889=CARTESIAN_POINT('Ctrl Pts',(-4.88811881465991,-1.79697577151505,
393.764692562677));
#30890=CARTESIAN_POINT('Ctrl Pts',(-5.07303815383513,-0.477899626088436,
393.723326724414));
#30891=CARTESIAN_POINT('Ctrl Pts',(-5.07320934784751,5.14726455259906E-5,
393.708336844637));
#30892=CARTESIAN_POINT('Ctrl Pts',(-5.07374340439062,0.000119799015104727,
394.791663155363));
#30893=CARTESIAN_POINT('Ctrl Pts',(-5.07389328700639,0.149964795759533,
394.786962176793));
#30894=CARTESIAN_POINT('Ctrl Pts',(-5.03087783588661,1.1404650386697,394.755885239737));
#30895=CARTESIAN_POINT('Ctrl Pts',(-4.40588160918252,2.92317155691987,394.698432344195));
#30896=CARTESIAN_POINT('Ctrl Pts',(-2.47828569661807,4.67063429431767,394.619304468735));
#30897=CARTESIAN_POINT('Ctrl Pts',(0.0493855336599835,5.28718126929493,
394.540176593275));
#30898=CARTESIAN_POINT('Ctrl Pts',(2.56509888521489,4.623525972068,394.461048717816));
#30899=CARTESIAN_POINT('Ctrl Pts',(4.45971656139522,2.84036140259214,394.381920842355));
#30900=CARTESIAN_POINT('Ctrl Pts',(5.27448866684743,0.369450955630144,394.302792966896));
#30901=CARTESIAN_POINT('Ctrl Pts',(4.81213180090847,-2.19091584411711,394.223665091436));
#30902=CARTESIAN_POINT('Ctrl Pts',(3.18459792440514,-4.2207891164085,394.144537215977));
#30903=CARTESIAN_POINT('Ctrl Pts',(0.785967069903959,-5.22866909168525,
394.065409340517));
#30904=CARTESIAN_POINT('Ctrl Pts',(-1.8029725289961,-4.97051453724898,393.986281465057));
#30905=CARTESIAN_POINT('Ctrl Pts',(-3.95535256793798,-3.50883324890547,
393.907153589597));
#30906=CARTESIAN_POINT('Ctrl Pts',(-4.9347894212868,-1.61393147469998,393.842280819699));
#30907=CARTESIAN_POINT('Ctrl Pts',(-5.0732716126465,-0.386507955183392,
393.803784008288));
#30908=CARTESIAN_POINT('Ctrl Pts',(-5.07318860167666,-3.10232113822501E-5,
393.791663155363));
#30909=CARTESIAN_POINT('Origin',(0.,0.,402.208336844637));
#30910=CARTESIAN_POINT('',(-5.07372845053928,-0.000121538385184292,395.791663155363));
#30911=CARTESIAN_POINT('',(-5.07344883766069,-0.000122970527678777,395.708336844637));
#30912=CARTESIAN_POINT('',(-5.0736,-1.59740085886799E-13,402.208336844637));
#30913=CARTESIAN_POINT('Ctrl Pts',(-5.07344883766069,-0.000122970527678921,
395.708336844637));
#30914=CARTESIAN_POINT('Ctrl Pts',(-5.07290495347366,0.594570911737787,
395.689683061425));
#30915=CARTESIAN_POINT('Ctrl Pts',(-4.82050381961586,2.03059585572183,395.644653319727));
#30916=CARTESIAN_POINT('Ctrl Pts',(-3.49440419526435,3.96810585645496,395.573247619542));
#30917=CARTESIAN_POINT('Ctrl Pts',(-1.17878204811896,5.1543377509575,395.494119744082));
#30918=CARTESIAN_POINT('Ctrl Pts',(1.42226240243777,5.09253320328156,395.414991868623));
#30919=CARTESIAN_POINT('Ctrl Pts',(3.67892986523249,3.79765714811298,395.335863993163));
#30920=CARTESIAN_POINT('Ctrl Pts',(5.0448061610774,1.58324210563915,395.256736117703));
#30921=CARTESIAN_POINT('Ctrl Pts',(5.18916725226161,-1.01452845991075,395.177608242243));
#30922=CARTESIAN_POINT('Ctrl Pts',(4.07705852165763,-3.36664797371096,395.098480366784));
#30923=CARTESIAN_POINT('Ctrl Pts',(1.97775844702931,-4.90359014326416,395.019352491324));
#30924=CARTESIAN_POINT('Ctrl Pts',(-0.60042266624658,-5.25321019851391,
394.940224615864));
#30925=CARTESIAN_POINT('Ctrl Pts',(-3.03322150067462,-4.33085350661488,
394.861096740404));
#30926=CARTESIAN_POINT('Ctrl Pts',(-4.69225666341608,-2.40548544911562,
394.783800816662));
#30927=CARTESIAN_POINT('Ctrl Pts',(-5.07351974582911,-0.782183276838963,
394.732880851406));
#30928=CARTESIAN_POINT('Ctrl Pts',(-5.07397904538501,5.86126803111056E-5,
394.708336844637));
#30929=CARTESIAN_POINT('Ctrl Pts',(-5.07372845053928,-0.000121538385184274,
395.791663155363));
#30930=CARTESIAN_POINT('Ctrl Pts',(-5.07303742094413,0.685929840247112,
395.770140345299));
#30931=CARTESIAN_POINT('Ctrl Pts',(-4.76110728643783,2.2133386185757,395.722241576749));
#30932=CARTESIAN_POINT('Ctrl Pts',(-3.27480540051438,4.15118950351341,395.647966849712));
#30933=CARTESIAN_POINT('Ctrl Pts',(-0.898448588333209,5.21051963238218,
395.568838974252));
#30934=CARTESIAN_POINT('Ctrl Pts',(1.69545248148909,5.00820981872071,395.489711098793));
#30935=CARTESIAN_POINT('Ctrl Pts',(3.87882816762124,3.59324599093717,395.410583223333));
#30936=CARTESIAN_POINT('Ctrl Pts',(5.12301066540628,1.30823790934658,395.331455347873));
#30937=CARTESIAN_POINT('Ctrl Pts',(5.12674204938754,-1.29353804132683,395.252327472413));
#30938=CARTESIAN_POINT('Ctrl Pts',(3.88911882751359,-3.58210544942458,395.173199596953));
#30939=CARTESIAN_POINT('Ctrl Pts',(1.70981070658587,-5.00332609900278,395.094071721494));
#30940=CARTESIAN_POINT('Ctrl Pts',(-0.883499401435098,-5.21307524528295,
395.014943846034));
#30941=CARTESIAN_POINT('Ctrl Pts',(-3.26288494670713,-4.16056565022955,
394.935815970574));
#30942=CARTESIAN_POINT('Ctrl Pts',(-4.7577955410693,-2.22302453301642,394.861389073684));
#30943=CARTESIAN_POINT('Ctrl Pts',(-5.07305233493801,-0.690776202139344,
394.81333813528));
#30944=CARTESIAN_POINT('Ctrl Pts',(-5.07374340439062,0.000119799015104727,
394.791663155363));
#30945=CARTESIAN_POINT('Origin',(0.,0.,402.208336844637));
#30946=CARTESIAN_POINT('',(-5.07319204280361,3.5344916511082E-5,396.791663155363));
#30947=CARTESIAN_POINT('',(-5.07333567377535,0.000103933621521292,396.708336844637));
#30948=CARTESIAN_POINT('',(-5.0736,-1.59740085886799E-13,402.208336844637));
#30949=CARTESIAN_POINT('Ctrl Pts',(-5.07333567377534,0.000103933621520939,
396.708336844637));
#30950=CARTESIAN_POINT('Ctrl Pts',(-5.07355255518605,0.290225038825201,
396.699237188418));
#30951=CARTESIAN_POINT('Ctrl Pts',(-4.9781337482961,1.42114034886055,396.663761573712));
#30952=CARTESIAN_POINT('Ctrl Pts',(-4.14865431030898,3.27801650109757,396.601910000519));
#30953=CARTESIAN_POINT('Ctrl Pts',(-2.08295867375766,4.85983620416686,396.52278212506));
#30954=CARTESIAN_POINT('Ctrl Pts',(0.487090472013812,5.26492807548086,396.4436542496));
#30955=CARTESIAN_POINT('Ctrl Pts',(2.93919882905869,4.3952059122609,396.36452637414));
#30956=CARTESIAN_POINT('Ctrl Pts',(4.67962948341671,2.46125835008237,396.28539849868));
#30957=CARTESIAN_POINT('Ctrl Pts',(5.2869663411736,-0.0686416434144708,
396.206270623221));
#30958=CARTESIAN_POINT('Ctrl Pts',(4.61415296796628,-2.58192121415839,396.127142747761));
#30959=CARTESIAN_POINT('Ctrl Pts',(2.82409983825713,-4.47003186470401,396.048014872301));
#30960=CARTESIAN_POINT('Ctrl Pts',(0.350238296140284,-5.27579926682488,
395.968886996841));
#30961=CARTESIAN_POINT('Ctrl Pts',(-2.20842757548492,-4.80412035775031,
395.889759121382));
#30962=CARTESIAN_POINT('Ctrl Pts',(-4.23235974759556,-3.16920427471092,
395.810631245921));
#30963=CARTESIAN_POINT('Ctrl Pts',(-4.99595812955649,-1.33323876922698,
395.750157153674));
#30964=CARTESIAN_POINT('Ctrl Pts',(-5.07367399139889,-0.246310585215766,
395.716059019912));
#30965=CARTESIAN_POINT('Ctrl Pts',(-5.07344883766069,-0.000122970527678921,
395.708336844637));
#30966=CARTESIAN_POINT('Ctrl Pts',(-5.07319204280361,3.53449165107697E-5,
396.791663155363));
#30967=CARTESIAN_POINT('Ctrl Pts',(-5.07328550820695,0.381659555984483,
396.779694472291));
#30968=CARTESIAN_POINT('Ctrl Pts',(-4.93711373649749,1.60422160810075,396.741349830733));
#30969=CARTESIAN_POINT('Ctrl Pts',(-3.96540078941456,3.49747355738801,396.676629230689));
#30970=CARTESIAN_POINT('Ctrl Pts',(-1.81722218927578,4.96532256959422,396.597501355229));
#30971=CARTESIAN_POINT('Ctrl Pts',(0.770966287074601,5.23090199578547,396.51837347977));
#30972=CARTESIAN_POINT('Ctrl Pts',(3.17247820700774,4.22990623198423,396.43924560431));
#30973=CARTESIAN_POINT('Ctrl Pts',(4.8058277352491,2.20470961453625,396.36011772885));
#30974=CARTESIAN_POINT('Ctrl Pts',(5.275526676699,-0.354320460537079,396.28098985339));
#30975=CARTESIAN_POINT('Ctrl Pts',(4.46784531008081,-2.82755777845599,396.201861977931));
#30976=CARTESIAN_POINT('Ctrl Pts',(2.57835013256881,-4.61614940174172,396.122734102471));
#30977=CARTESIAN_POINT('Ctrl Pts',(0.0645507123742531,-5.2870178655694,
396.043606227011));
#30978=CARTESIAN_POINT('Ctrl Pts',(-2.46487858023149,-4.67772362266456,
395.964478351551));
#30979=CARTESIAN_POINT('Ctrl Pts',(-4.39747886350376,-2.93579705537622,
395.885350476092));
#30980=CARTESIAN_POINT('Ctrl Pts',(-5.02925481295834,-1.15017365368594,
395.827745410695));
#30981=CARTESIAN_POINT('Ctrl Pts',(-5.0738842698389,-0.154818306903111,
395.796516303786));
#30982=CARTESIAN_POINT('Ctrl Pts',(-5.07372845053928,-0.000121538385184274,
395.791663155363));
#30983=CARTESIAN_POINT('Origin',(0.,0.,402.208336844637));
#30984=CARTESIAN_POINT('',(-5.0739418421154,7.48951186854696E-5,397.791663155363));
#30985=CARTESIAN_POINT('',(-5.07403169783887,-1.51513653288439E-5,397.708336844637));
#30986=CARTESIAN_POINT('',(-5.0736,-1.59740085886799E-13,402.208336844637));
#30987=CARTESIAN_POINT('Ctrl Pts',(-5.07403169783887,-1.51513653288493E-5,
397.708336844637));
#30988=CARTESIAN_POINT('Ctrl Pts',(-5.07388968734652,0.82610348406882,397.682415356923));
#30989=CARTESIAN_POINT('Ctrl Pts',(-4.6586701596041,2.49296234041498,397.630117910723));
#30990=CARTESIAN_POINT('Ctrl Pts',(-2.91976153402742,4.40814216562114,397.551444506037));
#30991=CARTESIAN_POINT('Ctrl Pts',(-0.463836508948714,5.26702766851281,
397.472316630577));
#30992=CARTESIAN_POINT('Ctrl Pts',(2.10439874769627,4.85059075563045,397.393188755117));
#30993=CARTESIAN_POINT('Ctrl Pts',(4.16308914079174,3.25966464129901,397.314060879657));
#30994=CARTESIAN_POINT('Ctrl Pts',(5.21375731827273,0.87946540242969,397.234933004198));
#30995=CARTESIAN_POINT('Ctrl Pts',(5.00200160188481,-1.71368163398425,397.155805128738));
#30996=CARTESIAN_POINT('Ctrl Pts',(3.57909508696266,-3.89188940315535,397.076677253278));
#30997=CARTESIAN_POINT('Ctrl Pts',(1.28957072230382,-5.12774142484681,396.997549377819));
#30998=CARTESIAN_POINT('Ctrl Pts',(-1.31220156516579,-5.12199685867627,
396.918421502358));
#30999=CARTESIAN_POINT('Ctrl Pts',(-3.59624625077107,-3.87604665499891,
396.839293626899));
#31000=CARTESIAN_POINT('Ctrl Pts',(-4.84699459687274,-1.94278943218135,
396.769265407658));
#31001=CARTESIAN_POINT('Ctrl Pts',(-5.07292390999909,-0.550710271536964,
396.725613146904));
#31002=CARTESIAN_POINT('Ctrl Pts',(-5.07333567377534,0.000103933621520939,
396.708336844637));
#31003=CARTESIAN_POINT('Ctrl Pts',(-5.0739418421154,7.48951186850533E-5,
397.791663155363));
#31004=CARTESIAN_POINT('Ctrl Pts',(-5.07399707454689,0.0770308345755981,
397.789248599284));
#31005=CARTESIAN_POINT('Ctrl Pts',(-5.05354999565328,0.994603307815543,
397.760458084718));
#31006=CARTESIAN_POINT('Ctrl Pts',(-4.52773440061085,2.73063104480294,397.705291611666));
#31007=CARTESIAN_POINT('Ctrl Pts',(-2.67721733102668,4.55952103490808,397.626163736206));
#31008=CARTESIAN_POINT('Ctrl Pts',(-0.178456984770649,5.28439947486034,
397.547035860747));
#31009=CARTESIAN_POINT('Ctrl Pts',(2.36351372741711,4.72974920747697,397.467907985287));
#31010=CARTESIAN_POINT('Ctrl Pts',(4.33319922937441,3.02986949287705,397.388780109827));
#31011=CARTESIAN_POINT('Ctrl Pts',(5.25367321071018,0.596357694998765,397.309652234368));
#31012=CARTESIAN_POINT('Ctrl Pts',(4.90205833425909,-1.98155211711401,397.230524358907));
#31013=CARTESIAN_POINT('Ctrl Pts',(3.36349224536493,-4.07966231699243,397.151396483448));
#31014=CARTESIAN_POINT('Ctrl Pts',(1.01051291891753,-5.18995070747486,397.072268607988));
#31015=CARTESIAN_POINT('Ctrl Pts',(-1.58714516337332,-5.04357957562867,
396.993140732529));
#31016=CARTESIAN_POINT('Ctrl Pts',(-3.80050266261658,-3.67599023621695,
396.914012857068));
#31017=CARTESIAN_POINT('Ctrl Pts',(-4.89803666817087,-1.7598107945601,396.84685366468));
#31018=CARTESIAN_POINT('Ctrl Pts',(-5.07307953403386,-0.459343943622233,
396.806070430778));
#31019=CARTESIAN_POINT('Ctrl Pts',(-5.07319204280361,3.53449165107697E-5,
396.791663155363));
#31020=CARTESIAN_POINT('Origin',(0.,0.,402.208336844637));
#31021=CARTESIAN_POINT('',(-5.07350261625086,-0.000127405426567639,398.791663155363));
#31022=CARTESIAN_POINT('',(-5.07327504304777,-8.56681209023223E-5,398.708336844637));
#31023=CARTESIAN_POINT('',(-5.0736,-1.59740085886799E-13,402.208336844637));
#31024=CARTESIAN_POINT('Ctrl Pts',(-5.07327504304777,-8.56681209025073E-5,
398.708336844637));
#31025=CARTESIAN_POINT('Ctrl Pts',(-5.07295870657578,0.521766948573649,
398.691969483916));
#31026=CARTESIAN_POINT('Ctrl Pts',(-4.86376568515234,1.88483153888263,398.649226164708));
#31027=CARTESIAN_POINT('Ctrl Pts',(-3.66212405277363,3.81386578025083,398.580106887014));
#31028=CARTESIAN_POINT('Ctrl Pts',(-1.39976059402284,5.09876407058445,398.500979011554));
#31029=CARTESIAN_POINT('Ctrl Pts',(1.2015314169661,5.14908215334412,398.421851136094));
#31030=CARTESIAN_POINT('Ctrl Pts',(3.51189274640949,3.9526363487746,398.342723260634));
#31031=CARTESIAN_POINT('Ctrl Pts',(4.97190814582059,1.79912594262636,398.263595385175));
#31032=CARTESIAN_POINT('Ctrl Pts',(5.22805937238099,-0.790012637095727,
398.184467509715));
#31033=CARTESIAN_POINT('Ctrl Pts',(4.21832370253235,-3.18786290617544,398.105339634255));
#31034=CARTESIAN_POINT('Ctrl Pts',(2.18719169429123,-4.81382563667766,398.026211758795));
#31035=CARTESIAN_POINT('Ctrl Pts',(-0.37353210098369,-5.27420122269227,
397.947083883336));
#31036=CARTESIAN_POINT('Ctrl Pts',(-2.84381136257153,-4.45751743709679,
397.867956007876));
#31037=CARTESIAN_POINT('Ctrl Pts',(-4.62550939672404,-2.56152056184034,
397.788828132416));
#31038=CARTESIAN_POINT('Ctrl Pts',(-5.07044892396789,-0.869584543074369,
397.73562174467));
#31039=CARTESIAN_POINT('Ctrl Pts',(-5.07403418765037,-0.0144991493159696,
397.70879131541));
#31040=CARTESIAN_POINT('Ctrl Pts',(-5.07403169783887,-1.51513653288493E-5,
397.708336844637));
#31041=CARTESIAN_POINT('Ctrl Pts',(-5.07350261625086,-0.000127405426567848,
398.791663155363));
#31042=CARTESIAN_POINT('Ctrl Pts',(-5.07291128030502,0.613121580961722,
398.77242676779));
#31043=CARTESIAN_POINT('Ctrl Pts',(-4.80890661569317,2.06772180201207,398.72681442173));
#31044=CARTESIAN_POINT('Ctrl Pts',(-3.45061727711166,4.00624076891526,398.654826117184));
#31045=CARTESIAN_POINT('Ctrl Pts',(-1.12210802579434,5.16697186848109,398.575698241724));
#31046=CARTESIAN_POINT('Ctrl Pts',(1.47810086651078,5.07660738405961,398.496570366264));
#31047=CARTESIAN_POINT('Ctrl Pts',(3.72041242270134,3.75702756318667,398.417442490805));
#31048=CARTESIAN_POINT('Ctrl Pts',(5.06188850671742,1.52774652711538,398.338314615344));
#31049=CARTESIAN_POINT('Ctrl Pts',(5.17771318239863,-1.0714527081918,398.259186739885));
#31050=CARTESIAN_POINT('Ctrl Pts',(4.03984144729043,-3.41121763982034,398.180058864425));
#31051=CARTESIAN_POINT('Ctrl Pts',(1.92378985850489,-4.92501342998799,398.100930988965));
#31052=CARTESIAN_POINT('Ctrl Pts',(-0.658075180315041,-5.24629981628919,
398.021803113506));
#31053=CARTESIAN_POINT('Ctrl Pts',(-3.08059835091328,-4.29728268859095,
397.942675238046));
#31054=CARTESIAN_POINT('Ctrl Pts',(-4.70604526230202,-2.36846041862021,
397.865961918665));
#31055=CARTESIAN_POINT('Ctrl Pts',(-5.07339373038246,-0.763615063923845,
397.81562455777));
#31056=CARTESIAN_POINT('Ctrl Pts',(-5.0739418421154,7.48951186850533E-5,
397.791663155363));
#31057=CARTESIAN_POINT('Origin',(0.,0.,402.208336844637));
#31058=CARTESIAN_POINT('',(-5.07330191118131,0.000105688062508047,399.791663155363));
#31059=CARTESIAN_POINT('',(-5.07353386009457,0.000128968315485679,399.708336844637));
#31060=CARTESIAN_POINT('',(-5.0736,-1.59740085886799E-13,402.208336844637));
#31061=CARTESIAN_POINT('',(-1.31303618635556,-4.90075024188347,400.));
#31062=CARTESIAN_POINT('Ctrl Pts',(-1.31303618635555,-4.90075024188347,
400.));
#31063=CARTESIAN_POINT('Ctrl Pts',(-2.12521319086393,-4.68314727417224,
399.973624041513));
#31064=CARTESIAN_POINT('Ctrl Pts',(-3.63845957255092,-3.83644859241818,
399.92087212454));
#31065=CARTESIAN_POINT('Ctrl Pts',(-4.85784323874867,-1.90558193017489,
399.851426509661));
#31066=CARTESIAN_POINT('Ctrl Pts',(-5.07295978880057,-0.532132079631421,
399.808356853268));
#31067=CARTESIAN_POINT('Ctrl Pts',(-5.07330191118131,0.000105688062508012,
399.791663155363));
#31068=CARTESIAN_POINT('',(1.31318543090008,-4.90112867346845,400.));
#31069=CARTESIAN_POINT('Origin',(0.,0.,400.));
#31070=CARTESIAN_POINT('Ctrl Pts',(1.31318543090008,-4.90112867346845,400.));
#31071=CARTESIAN_POINT('Ctrl Pts',(0.546344064728336,-5.10618409880194,
399.975093589943));
#31072=CARTESIAN_POINT('Ctrl Pts',(-1.13368018453605,-5.15247589033718,
399.923811221401));
#31073=CARTESIAN_POINT('Ctrl Pts',(-3.42590833126468,-4.02739560525483,
399.84615289437));
#31074=CARTESIAN_POINT('Ctrl Pts',(-4.8023079180703,-2.08851222235156,399.77383825264));
#31075=CARTESIAN_POINT('Ctrl Pts',(-5.07291903260815,-0.623512076348425,
399.727899569395));
#31076=CARTESIAN_POINT('Ctrl Pts',(-5.07353386009457,0.000128968315485402,
399.708336844637));
#31077=CARTESIAN_POINT('Origin',(0.,0.,20.5));
#31078=CARTESIAN_POINT('',(4.51807726312575,-5.77016670283426E-5,39.6125833024919));
#31079=CARTESIAN_POINT('',(4.51743491291879,0.00013078575649096,39.887416697508));
#31080=CARTESIAN_POINT('',(4.51775,5.53264807684796E-16,20.5));
#31081=CARTESIAN_POINT('',(3.43378788736186,2.93584158413001,40.));
#31082=CARTESIAN_POINT('Ctrl Pts',(4.51743491291879,0.00013078575649096,
39.887416697508));
#31083=CARTESIAN_POINT('Ctrl Pts',(4.51757757737092,0.314458352690014,39.8984871683209));
#31084=CARTESIAN_POINT('Ctrl Pts',(4.48524528727997,0.628740973485904,39.9095576391338));
#31085=CARTESIAN_POINT('Ctrl Pts',(4.42014586550123,0.936043740039879,39.9206281099466));
#31086=CARTESIAN_POINT('Ctrl Pts',(4.26456488388791,1.67046602470259,39.9470854066311));
#31087=CARTESIAN_POINT('Ctrl Pts',(3.92183073605335,2.36502208507763,39.9735427033156));
#31088=CARTESIAN_POINT('Ctrl Pts',(3.43378788736169,2.9358415841302,40.));
#31089=CARTESIAN_POINT('',(4.51775,5.53264807684796E-16,40.));
#31090=CARTESIAN_POINT('Origin',(0.,0.,40.));
#31091=CARTESIAN_POINT('',(4.51775,-5.53264807684796E-16,41.));
#31092=CARTESIAN_POINT('',(4.51775,5.53264807684796E-16,20.5));
#31093=CARTESIAN_POINT('Origin',(0.,0.,41.));
#31094=CARTESIAN_POINT('',(-3.4340910891448,2.93606647242268,40.));
#31095=CARTESIAN_POINT('Origin',(0.,0.,40.));
#31096=CARTESIAN_POINT('Ctrl Pts',(-3.4340910891448,2.93606647242268,40.));
#31097=CARTESIAN_POINT('Ctrl Pts',(-2.96705577784696,3.4818800261268,39.974686898954));
#31098=CARTESIAN_POINT('Ctrl Pts',(-2.36757358452893,3.91460873741648,39.949373797908));
#31099=CARTESIAN_POINT('Ctrl Pts',(-1.70215900486053,4.18523117809469,39.9240606968621));
#31100=CARTESIAN_POINT('Ctrl Pts',(-1.00666654344796,4.46808621784234,39.8976034001776));
#31101=CARTESIAN_POINT('Ctrl Pts',(-0.239146468763622,4.57384880856985,
39.8711461034931));
#31102=CARTESIAN_POINT('Ctrl Pts',(0.506923795872781,4.48961228541996,39.8446888068086));
#31103=CARTESIAN_POINT('Ctrl Pts',(1.25299406050918,4.40537576227008,39.8182315101241));
#31104=CARTESIAN_POINT('Ctrl Pts',(1.97761451509765,4.1311401252428,39.7917742134397));
#31105=CARTESIAN_POINT('Ctrl Pts',(2.59252418705981,3.70032015205324,39.7653169167552));
#31106=CARTESIAN_POINT('Ctrl Pts',(3.2074338590219,3.26950017886373,39.7388596200708));
#31107=CARTESIAN_POINT('Ctrl Pts',(3.71263274835769,2.68209586951196,39.7124023233863));
#31108=CARTESIAN_POINT('Ctrl Pts',(4.0465897798431,2.00964543895381,39.6859450267018));
#31109=CARTESIAN_POINT('Ctrl Pts',(4.35525905337691,1.38811402527266,39.6614911186319));
#31110=CARTESIAN_POINT('Ctrl Pts',(4.51763802149368,0.693928511700309,39.6370372105619));
#31111=CARTESIAN_POINT('Ctrl Pts',(4.51807726312575,-5.77016670283426E-5,
39.6125833024919));
#31112=CARTESIAN_POINT('Origin',(0.,0.,20.5));
#31113=CARTESIAN_POINT('',(4.5173663293175,-1.61899228900975E-5,38.6125833024919));
#31114=CARTESIAN_POINT('',(4.51813342681501,1.37750411066654E-5,38.887416697508));
#31115=CARTESIAN_POINT('',(4.51775,5.53264807684796E-16,20.5));
#31116=CARTESIAN_POINT('Ctrl Pts',(4.51813342681501,1.37750411066654E-5,
38.887416697508));
#31117=CARTESIAN_POINT('Ctrl Pts',(4.51813570137199,0.0130379216071904,
38.8878756447561));
#31118=CARTESIAN_POINT('Ctrl Pts',(4.51808056261842,0.0260620488529043,
38.8883345920043));
#31119=CARTESIAN_POINT('Ctrl Pts',(4.51796789313227,0.039085678406741,38.8887935392524));
#31120=CARTESIAN_POINT('Ctrl Pts',(4.5114727457387,0.789869199672342,38.9152508359369));
#31121=CARTESIAN_POINT('Ctrl Pts',(4.31378754306059,1.53899875733816,38.9417081326213));
#31122=CARTESIAN_POINT('Ctrl Pts',(3.94899006576268,2.19523105353971,38.9681654293058));
#31123=CARTESIAN_POINT('Ctrl Pts',(3.58419258846473,2.85146334974134,38.9946227259902));
#31124=CARTESIAN_POINT('Ctrl Pts',(3.05228283654696,3.41479838447868,39.0210800226747));
#31125=CARTESIAN_POINT('Ctrl Pts',(2.4180469390752,3.81662285121831,39.0475373193592));
#31126=CARTESIAN_POINT('Ctrl Pts',(1.78381104160343,4.21844731795794,39.0739946160436));
#31127=CARTESIAN_POINT('Ctrl Pts',(1.04724899857768,4.45876121669985,39.1004519127281));
#31128=CARTESIAN_POINT('Ctrl Pts',(0.298073044029034,4.50829405706009,39.1269092094126));
#31129=CARTESIAN_POINT('Ctrl Pts',(-0.45110291051953,4.55782689742033,39.1533665060971));
#31130=CARTESIAN_POINT('Ctrl Pts',(-1.21289277659099,4.41657867939895,39.1798238027815));
#31131=CARTESIAN_POINT('Ctrl Pts',(-1.89451099954058,4.10175426806426,39.206281099466));
#31132=CARTESIAN_POINT('Ctrl Pts',(-2.57612922249017,3.78692985672956,39.2327383961504));
#31133=CARTESIAN_POINT('Ctrl Pts',(-3.17757580231788,3.29852925208155,39.2591956928349));
#31134=CARTESIAN_POINT('Ctrl Pts',(-3.62559595151898,2.69603724086566,39.2856529895194));
#31135=CARTESIAN_POINT('Ctrl Pts',(-4.07361610072013,2.0935452296497,39.3121102862039));
#31136=CARTESIAN_POINT('Ctrl Pts',(-4.36820981929462,1.37696181186582,39.3385675828883));
#31137=CARTESIAN_POINT('Ctrl Pts',(-4.4734945205513,0.633569578843569,39.3650248795728));
#31138=CARTESIAN_POINT('Ctrl Pts',(-4.57877922180797,-0.109822654178678,
39.3914821762572));
#31139=CARTESIAN_POINT('Ctrl Pts',(-4.49475490574683,-0.880023702439293,
39.4179394729417));
#31140=CARTESIAN_POINT('Ctrl Pts',(-4.23165828048028,-1.5832305850457,39.4443967696262));
#31141=CARTESIAN_POINT('Ctrl Pts',(-3.96856165521376,-2.28643746765202,
39.4708540663107));
#31142=CARTESIAN_POINT('Ctrl Pts',(-3.52639272074186,-2.92265018460415,
39.4973113629951));
#31143=CARTESIAN_POINT('Ctrl Pts',(-2.95900217961984,-3.41436616507676,
39.5237686596796));
#31144=CARTESIAN_POINT('Ctrl Pts',(-2.39161163849769,-3.90608214554949,
39.5502259563641));
#31145=CARTESIAN_POINT('Ctrl Pts',(-1.69899949072535,-4.25330138954263,
39.5766832530485));
#31146=CARTESIAN_POINT('Ctrl Pts',(-0.965534545329121,-4.41375671437606,
39.603140549733));
#31147=CARTESIAN_POINT('Ctrl Pts',(-0.232069599933061,-4.57421203920946,
39.6295978464175));
#31148=CARTESIAN_POINT('Ctrl Pts',(0.542248143086867,-4.54790344488323,
39.6560551431019));
#31149=CARTESIAN_POINT('Ctrl Pts',(1.26312545635919,-4.33799038903366,39.6825124397864));
#31150=CARTESIAN_POINT('Ctrl Pts',(1.98400276963152,-4.12807733318409,39.7089697364709));
#31151=CARTESIAN_POINT('Ctrl Pts',(2.65143965315624,-3.73455981581118,39.7354270331553));
#31152=CARTESIAN_POINT('Ctrl Pts',(3.18410908512153,-3.20545326780569,39.7618843298398));
#31153=CARTESIAN_POINT('Ctrl Pts',(3.71677851708688,-2.67634671980015,39.7883416265243));
#31154=CARTESIAN_POINT('Ctrl Pts',(4.11468049749276,-2.01165114116199,39.8147989232087));
#31155=CARTESIAN_POINT('Ctrl Pts',(4.32941757999969,-1.29215909736769,39.8412562198932));
#31156=CARTESIAN_POINT('Ctrl Pts',(4.45430267828147,-0.873722590951435,
39.8566430457648));
#31157=CARTESIAN_POINT('Ctrl Pts',(4.51723662387398,-0.436752488749845,
39.8720298716364));
#31158=CARTESIAN_POINT('Ctrl Pts',(4.51743491291879,0.00013078575649096,
39.887416697508));
#31159=CARTESIAN_POINT('Ctrl Pts',(4.51807726312575,-5.77016670283426E-5,
39.6125833024919));
#31160=CARTESIAN_POINT('Ctrl Pts',(4.51811324803589,-0.0569125845144851,
39.6105799138774));
#31161=CARTESIAN_POINT('Ctrl Pts',(4.51706233879025,-0.113766129714702,
39.6085765252629));
#31162=CARTESIAN_POINT('Ctrl Pts',(4.51491593042487,-0.170578278221581,
39.6065731366484));
#31163=CARTESIAN_POINT('Ctrl Pts',(4.48656987588623,-0.920855013074376,
39.580115839964));
#31164=CARTESIAN_POINT('Ctrl Pts',(4.26716259317389,-1.66391193101533,39.5536585432795));
#31165=CARTESIAN_POINT('Ctrl Pts',(3.88341809255801,-2.30924747945226,39.527201246595));
#31166=CARTESIAN_POINT('Ctrl Pts',(3.49967359194214,-2.9545830278892,39.5007439499106));
#31167=CARTESIAN_POINT('Ctrl Pts',(2.95159187342274,-3.50219720682209,39.4742866532261));
#31168=CARTESIAN_POINT('Ctrl Pts',(2.305928447501,-3.88539017854137,39.4478293565416));
#31169=CARTESIAN_POINT('Ctrl Pts',(1.66026502157934,-4.2685831502606,39.4213720598571));
#31170=CARTESIAN_POINT('Ctrl Pts',(0.917019888255395,-4.48735491476624,
39.3949147631727));
#31171=CARTESIAN_POINT('Ctrl Pts',(0.16671960730651,-4.51505986234427,39.3684574664882));
#31172=CARTESIAN_POINT('Ctrl Pts',(-0.58358067364246,-4.54276480992229,
39.3420001698038));
#31173=CARTESIAN_POINT('Ctrl Pts',(-1.34093610221634,-4.37940294057267,
39.3155428731193));
#31174=CARTESIAN_POINT('Ctrl Pts',(-2.0131016916631,-4.0448712583889,39.2890855764348));
#31175=CARTESIAN_POINT('Ctrl Pts',(-2.68526728110987,-3.71033957620513,
39.2626282797503));
#31176=CARTESIAN_POINT('Ctrl Pts',(-3.27224303142949,-3.20463808118724,
39.2361709830659));
#31177=CARTESIAN_POINT('Ctrl Pts',(-3.70253591076623,-2.58936080975925,
39.2097136863814));
#31178=CARTESIAN_POINT('Ctrl Pts',(-4.13282879010292,-1.97408353833133,
39.1832563896969));
#31179=CARTESIAN_POINT('Ctrl Pts',(-4.40643879845674,-1.24923049049336,
39.1567990930125));
#31180=CARTESIAN_POINT('Ctrl Pts',(-4.49004055820742,-0.503087883692005,
39.130341796328));
#31181=CARTESIAN_POINT('Ctrl Pts',(-4.5736423179581,0.243054723109393,39.1038844996435));
#31182=CARTESIAN_POINT('Ctrl Pts',(-4.46723582910558,1.01048688887427,39.0774272029591));
#31183=CARTESIAN_POINT('Ctrl Pts',(-4.18378127438633,1.70573618195759,39.0509699062746));
#31184=CARTESIAN_POINT('Ctrl Pts',(-3.90032671966707,2.40098547504095,39.0245126095901));
#31185=CARTESIAN_POINT('Ctrl Pts',(-3.43982409908106,3.02405189544285,38.9980553129056));
#31186=CARTESIAN_POINT('Ctrl Pts',(-2.85836212737563,3.49904666560209,38.9715980162212));
#31187=CARTESIAN_POINT('Ctrl Pts',(-2.27690015567025,3.97404143576128,38.9451407195367));
#31188=CARTESIAN_POINT('Ctrl Pts',(-1.5744788328455,4.30096455567782,38.9186834228523));
#31189=CARTESIAN_POINT('Ctrl Pts',(-0.836652295869176,4.43999713904635,
38.8922261261678));
#31190=CARTESIAN_POINT('Ctrl Pts',(-0.0988257588928058,4.57902972241489,
38.8657688294833));
#31191=CARTESIAN_POINT('Ctrl Pts',(0.67440599223512,4.53017176923538,38.8393115327988));
#31192=CARTESIAN_POINT('Ctrl Pts',(1.38886418452495,4.29937413054893,38.8128542361144));
#31193=CARTESIAN_POINT('Ctrl Pts',(2.10332237681477,4.06857649186248,38.7863969394299));
#31194=CARTESIAN_POINT('Ctrl Pts',(2.75900701026648,3.6558391676691,38.7599396427455));
#31195=CARTESIAN_POINT('Ctrl Pts',(3.27605642296661,3.11143310386805,38.733482346061));
#31196=CARTESIAN_POINT('Ctrl Pts',(3.79310583566678,2.56702704006697,38.7070250493765));
#31197=CARTESIAN_POINT('Ctrl Pts',(4.17152002761535,1.89095223665823,38.680567752692));
#31198=CARTESIAN_POINT('Ctrl Pts',(4.36520856862573,1.1655538582636,38.6541104560076));
#31199=CARTESIAN_POINT('Ctrl Pts',(4.46654587798484,0.786027431472861,38.6402680715023));
#31200=CARTESIAN_POINT('Ctrl Pts',(4.51731724698707,0.392999398715342,38.6264256869971));
#31201=CARTESIAN_POINT('Ctrl Pts',(4.5173663293175,-1.61899228900975E-5,
38.6125833024919));
#31202=CARTESIAN_POINT('Origin',(0.,0.,20.5));
#31203=CARTESIAN_POINT('',(4.51799626797168,8.54686663623316E-5,37.6125833024919));
#31204=CARTESIAN_POINT('',(4.51744515673179,-7.51896715610657E-5,37.887416697508));
#31205=CARTESIAN_POINT('',(4.51775,5.53264807684796E-16,20.5));
#31206=CARTESIAN_POINT('Ctrl Pts',(4.51744515673179,-7.51896715610657E-5,
37.887416697508));
#31207=CARTESIAN_POINT('Ctrl Pts',(4.51717073079397,0.462828384782965,37.9037214178759));
#31208=CARTESIAN_POINT('Ctrl Pts',(4.44640538068968,0.925813963613659,37.9200261382437));
#31209=CARTESIAN_POINT('Ctrl Pts',(4.30642900683072,1.36683241594085,37.9363308586115));
#31210=CARTESIAN_POINT('Ctrl Pts',(4.07929254766704,2.0824629679108,37.962788155296));
#31211=CARTESIAN_POINT('Ctrl Pts',(3.66991785444932,2.74025229569321,37.9892454519805));
#31212=CARTESIAN_POINT('Ctrl Pts',(3.12816631171535,3.26008238708871,38.0157027486649));
#31213=CARTESIAN_POINT('Ctrl Pts',(2.58641476898142,3.77991247848417,38.0421600453494));
#31214=CARTESIAN_POINT('Ctrl Pts',(1.91228637673127,4.16178333349271,38.0686173420339));
#31215=CARTESIAN_POINT('Ctrl Pts',(1.18788922711554,4.35918350473768,38.0950746387183));
#31216=CARTESIAN_POINT('Ctrl Pts',(0.463492077499819,4.55658367598265,38.1215319354028));
#31217=CARTESIAN_POINT('Ctrl Pts',(-0.311173829481454,4.56951316346404,
38.1479892320873));
#31218=CARTESIAN_POINT('Ctrl Pts',(-1.04175504380602,4.39639716966122,38.1744465287717));
#31219=CARTESIAN_POINT('Ctrl Pts',(-1.77233625813064,4.2232811758584,38.2009038254562));
#31220=CARTESIAN_POINT('Ctrl Pts',(-2.45883277979851,3.86411970077134,38.2273611221407));
#31221=CARTESIAN_POINT('Ctrl Pts',(-3.01763009204679,3.36265821505168,38.2538184188251));
#31222=CARTESIAN_POINT('Ctrl Pts',(-3.57642740429506,2.86119672933201,38.2802757155096));
#31223=CARTESIAN_POINT('Ctrl Pts',(-4.00752550712371,2.21743523297976,38.3067330121941));
#31224=CARTESIAN_POINT('Ctrl Pts',(-4.25841712907836,1.50978316287097,38.3331903088785));
#31225=CARTESIAN_POINT('Ctrl Pts',(-4.50930875103297,0.802131092762298,
38.359647605563));
#31226=CARTESIAN_POINT('Ctrl Pts',(-4.57999389211364,0.0305884488970126,
38.3861049022475));
#31227=CARTESIAN_POINT('Ctrl Pts',(-4.46186317968564,-0.710871726876464,
38.412562198932));
#31228=CARTESIAN_POINT('Ctrl Pts',(-4.34373246725763,-1.45233190264998,
38.4390194956164));
#31229=CARTESIAN_POINT('Ctrl Pts',(-4.03678590132095,-2.16370961033178,
38.4654767923008));
#31230=CARTESIAN_POINT('Ctrl Pts',(-3.57840923518433,-2.75835983566992,
38.4919340889853));
#31231=CARTESIAN_POINT('Ctrl Pts',(-3.12003256904766,-3.35301006100813,
38.5183913856698));
#31232=CARTESIAN_POINT('Ctrl Pts',(-2.51022580271103,-3.83093280400264,
38.5448486823543));
#31233=CARTESIAN_POINT('Ctrl Pts',(-1.82326272299569,-4.13391759737145,
38.5713059790388));
#31234=CARTESIAN_POINT('Ctrl Pts',(-1.13629964328034,-4.43690239074026,
38.5977632757232));
#31235=CARTESIAN_POINT('Ctrl Pts',(-0.372180250186292,-4.56494923448336,
38.6242205724077));
#31236=CARTESIAN_POINT('Ctrl Pts',(0.376026555300945,-4.50246217629699,
38.6506778690921));
#31237=CARTESIAN_POINT('Ctrl Pts',(1.12423336078818,-4.4399751181106,38.6771351657766));
#31238=CARTESIAN_POINT('Ctrl Pts',(1.85652757866858,-4.18695415799474,38.7035924624611));
#31239=CARTESIAN_POINT('Ctrl Pts',(2.48371659230794,-3.77421694705527,38.7300497591456));
#31240=CARTESIAN_POINT('Ctrl Pts',(3.1109056059473,-3.3614797361158,38.7565070558301));
#31241=CARTESIAN_POINT('Ctrl Pts',(3.63298941534561,-2.78902627435273,38.7829643525145));
#31242=CARTESIAN_POINT('Ctrl Pts',(3.98637877399025,-2.12658080103845,38.8094216491989));
#31243=CARTESIAN_POINT('Ctrl Pts',(4.33363798730682,-1.47562658212673,38.8354199986353));
#31244=CARTESIAN_POINT('Ctrl Pts',(4.51800457817832,-0.737775404274226,
38.8614183480717));
#31245=CARTESIAN_POINT('Ctrl Pts',(4.51813342681501,1.37750411066654E-5,
38.887416697508));
#31246=CARTESIAN_POINT('Ctrl Pts',(4.5173663293175,-1.61899228900975E-5,
38.6125833024919));
#31247=CARTESIAN_POINT('Ctrl Pts',(4.51741105927625,-0.358181153038861,
38.5999683903127));
#31248=CARTESIAN_POINT('Ctrl Pts',(4.4753302503181,-0.71633578114697,38.5873534781335));
#31249=CARTESIAN_POINT('Ctrl Pts',(4.39100556896819,-1.06425172631817,38.5747385659542));
#31250=CARTESIAN_POINT('Ctrl Pts',(4.21415113822809,-1.79393697912487,38.5482812692697));
#31251=CARTESIAN_POINT('Ctrl Pts',(3.85147938667571,-2.47858553135783,38.5218239725852));
#31252=CARTESIAN_POINT('Ctrl Pts',(3.34716333215496,-3.0348079465722,38.4953666759008));
#31253=CARTESIAN_POINT('Ctrl Pts',(2.84284727763424,-3.59103036178655,38.4689093792163));
#31254=CARTESIAN_POINT('Ctrl Pts',(2.19688692014516,-4.01882663998234,38.4424520825318));
#31255=CARTESIAN_POINT('Ctrl Pts',(1.48795951638629,-4.26609166819816,38.4159947858474));
#31256=CARTESIAN_POINT('Ctrl Pts',(0.779032112627345,-4.513356696414,38.3895374891629));
#31257=CARTESIAN_POINT('Ctrl Pts',(0.00713766259859555,-4.58009047464984,
38.3630801924784));
#31258=CARTESIAN_POINT('Ctrl Pts',(-0.733707943998393,-4.45816490243132,
38.336622895794));
#31259=CARTESIAN_POINT('Ctrl Pts',(-1.4745535505953,-4.33623933021282,38.3101655991095));
#31260=CARTESIAN_POINT('Ctrl Pts',(-2.18435031376045,-4.02565440754,38.283708302425));
#31261=CARTESIAN_POINT('Ctrl Pts',(-2.77664577327751,-3.56423903433536,
38.2572510057406));
#31262=CARTESIAN_POINT('Ctrl Pts',(-3.36894123279463,-3.10282366113066,
38.2307937090561));
#31263=CARTESIAN_POINT('Ctrl Pts',(-3.84373538866364,-2.49057783739411,
38.2043364123716));
#31264=CARTESIAN_POINT('Ctrl Pts',(-4.14319883817823,-1.80207242682554,
38.1778791156872));
#31265=CARTESIAN_POINT('Ctrl Pts',(-4.44266228769283,-1.11356701625697,
38.1514218190027));
#31266=CARTESIAN_POINT('Ctrl Pts',(-4.56679503085301,-0.348802018856373,
38.1249645223182));
#31267=CARTESIAN_POINT('Ctrl Pts',(-4.50047783691868,0.399075035061113,
38.0985072256338));
#31268=CARTESIAN_POINT('Ctrl Pts',(-4.43416064298434,1.14695208897856,38.0720499289493));
#31269=CARTESIAN_POINT('Ctrl Pts',(-4.17739351195555,1.87794119941278,38.0455926322648));
#31270=CARTESIAN_POINT('Ctrl Pts',(-3.76145039622188,2.50300870173274,38.0191353355804));
#31271=CARTESIAN_POINT('Ctrl Pts',(-3.34550728048821,3.1280762040527,37.9926780388959));
#31272=CARTESIAN_POINT('Ctrl Pts',(-2.77038818004956,3.64722209825836,37.9662207422114));
#31273=CARTESIAN_POINT('Ctrl Pts',(-2.10614196483595,3.99721498898437,37.9397634455269));
#31274=CARTESIAN_POINT('Ctrl Pts',(-1.4418957496223,4.34720787971039,37.9133061488425));
#31275=CARTESIAN_POINT('Ctrl Pts',(-0.688522419633467,4.52804776695686,
37.886848852158));
#31276=CARTESIAN_POINT('Ctrl Pts',(0.0622179873187612,4.51770855260138,
37.8603915554735));
#31277=CARTESIAN_POINT('Ctrl Pts',(0.812958394270905,4.5073693382459,37.8339342587891));
#31278=CARTESIAN_POINT('Ctrl Pts',(1.56106587818642,4.30585102228859,37.8074769621046));
#31279=CARTESIAN_POINT('Ctrl Pts',(2.21542177547896,3.93769831258472,37.7810196654202));
#31280=CARTESIAN_POINT('Ctrl Pts',(2.86977767277154,3.56954560288082,37.7545623687357));
#31281=CARTESIAN_POINT('Ctrl Pts',(3.43038198344099,3.03475849943036,37.7281050720512));
#31282=CARTESIAN_POINT('Ctrl Pts',(3.82895372288588,2.3984734795689,37.7016477753667));
#31283=CARTESIAN_POINT('Ctrl Pts',(4.22752546233078,1.76218845970743,37.6751904786822));
#31284=CARTESIAN_POINT('Ctrl Pts',(4.46406463055111,1.02440552343496,37.6487331819978));
#31285=CARTESIAN_POINT('Ctrl Pts',(4.50976101864303,0.274985815861593,37.6222758853133));
#31286=CARTESIAN_POINT('Ctrl Pts',(4.51534128170496,0.18346963073906,37.6190450243729));
#31287=CARTESIAN_POINT('Ctrl Pts',(4.51807563365308,0.0917799142062647,
37.6158141634324));
#31288=CARTESIAN_POINT('Ctrl Pts',(4.51799626797168,8.54686663623316E-5,
37.6125833024919));
#31289=CARTESIAN_POINT('Origin',(0.,0.,20.5));
#31290=CARTESIAN_POINT('',(4.51763788794132,-0.000113968307276224,36.612583302492));
#31291=CARTESIAN_POINT('',(4.51778606435352,0.000115791782295315,36.887416697508));
#31292=CARTESIAN_POINT('',(4.51775,5.53264807684796E-16,20.5));
#31293=CARTESIAN_POINT('Ctrl Pts',(4.51778606435352,0.000115791782295315,
36.887416697508));
#31294=CARTESIAN_POINT('Ctrl Pts',(4.51795287012522,0.16171502012428,36.8931098943111));
#31295=CARTESIAN_POINT('Ctrl Pts',(4.50945045543959,0.323296786803073,36.8988030911142));
#31296=CARTESIAN_POINT('Ctrl Pts',(4.49214571371295,0.483930295567246,36.9044962879172));
#31297=CARTESIAN_POINT('Ctrl Pts',(4.41172750549954,1.23042274011835,36.9309535846017));
#31298=CARTESIAN_POINT('Ctrl Pts',(4.14121195660595,1.9564363604895,36.9574108812862));
#31299=CARTESIAN_POINT('Ctrl Pts',(3.71354756149943,2.57354350122142,36.9838681779707));
#31300=CARTESIAN_POINT('Ctrl Pts',(3.28588316639293,3.1906506419533,37.0103254746552));
#31301=CARTESIAN_POINT('Ctrl Pts',(2.70106992507351,3.69885130304599,37.0367827713396));
#31302=CARTESIAN_POINT('Ctrl Pts',(2.0303374431028,4.03624720641988,37.0632400680241));
#31303=CARTESIAN_POINT('Ctrl Pts',(1.35960496113208,4.37364310979377,37.0896973647085));
#31304=CARTESIAN_POINT('Ctrl Pts',(0.602953238510051,4.54023425544888,37.116154661393));
#31305=CARTESIAN_POINT('Ctrl Pts',(-0.147458382357975,4.51573002621609,
37.1426119580775));
#31306=CARTESIAN_POINT('Ctrl Pts',(-0.897870003226045,4.49122579698331,
37.169069254762));
#31307=CARTESIAN_POINT('Ctrl Pts',(-1.64204152234013,4.27562619286261,37.1955265514464));
#31308=CARTESIAN_POINT('Ctrl Pts',(-2.28933367227002,3.89519100702498,37.2219838481309));
#31309=CARTESIAN_POINT('Ctrl Pts',(-2.93662582219991,3.51475582118734,37.2484411448154));
#31310=CARTESIAN_POINT('Ctrl Pts',(-3.48703860294563,2.96948505363274,37.2748984414998));
#31311=CARTESIAN_POINT('Ctrl Pts',(-3.87353234697123,2.32579208038141,37.3013557381843));
#31312=CARTESIAN_POINT('Ctrl Pts',(-4.26002609099678,1.68209910713015,37.3278130348688));
#31313=CARTESIAN_POINT('Ctrl Pts',(-4.48260079830228,0.939983928182159,
37.3542703315532));
#31314=CARTESIAN_POINT('Ctrl Pts',(-4.51414711586847,0.18983535101083,37.3807276282377));
#31315=CARTESIAN_POINT('Ctrl Pts',(-4.54569343343466,-0.560313226160541,
37.4071849249222));
#31316=CARTESIAN_POINT('Ctrl Pts',(-4.38621136126154,-1.31849520155516,
37.4336422216066));
#31317=CARTESIAN_POINT('Ctrl Pts',(-4.05512563923565,-1.99236484967302,
37.4600995182911));
#31318=CARTESIAN_POINT('Ctrl Pts',(-3.72403991720973,-2.66623449779091,
37.4865568149756));
#31319=CARTESIAN_POINT('Ctrl Pts',(-3.22135054533102,-3.25579181863192,
37.51301411166));
#31320=CARTESIAN_POINT('Ctrl Pts',(-2.60828453275295,-3.68922938300066,
37.5394714083445));
#31321=CARTESIAN_POINT('Ctrl Pts',(-1.99521852017489,-4.1226669473694,37.565928705029));
#31322=CARTESIAN_POINT('Ctrl Pts',(-1.27177586689746,-4.39998475526589,
37.5923860017135));
#31323=CARTESIAN_POINT('Ctrl Pts',(-0.52607108743212,-4.48740580460162,
37.6188432983979));
#31324=CARTESIAN_POINT('Ctrl Pts',(0.219633692033175,-4.57482685393735,
37.6453005950824));
#31325=CARTESIAN_POINT('Ctrl Pts',(0.987600597686399,-4.47235114471234,
37.6717578917668));
#31326=CARTESIAN_POINT('Ctrl Pts',(1.68429211034969,-4.19246010490277,37.6982151884513));
#31327=CARTESIAN_POINT('Ctrl Pts',(2.38098362301298,-3.9125690650932,37.7246724851358));
#31328=CARTESIAN_POINT('Ctrl Pts',(3.00639974268637,-3.45526269469905,37.7511297818202));
#31329=CARTESIAN_POINT('Ctrl Pts',(3.48436547816537,-2.87624040350849,37.7775870785047));
#31330=CARTESIAN_POINT('Ctrl Pts',(3.96233121364435,-2.29721811231796,37.8040443751892));
#31331=CARTESIAN_POINT('Ctrl Pts',(4.29284656492897,-1.596479900331,37.8305016718736));
#31332=CARTESIAN_POINT('Ctrl Pts',(4.43565512801649,-0.859374906258841,
37.8569589685581));
#31333=CARTESIAN_POINT('Ctrl Pts',(4.49045569410255,-0.576522323285484,
37.8671115448747));
#31334=CARTESIAN_POINT('Ctrl Pts',(4.51761603548433,-0.288314654125513,
37.8772641211914));
#31335=CARTESIAN_POINT('Ctrl Pts',(4.51744515673179,-7.51896715610657E-5,
37.887416697508));
#31336=CARTESIAN_POINT('Ctrl Pts',(4.51799626797168,8.54686663623316E-5,
37.6125833024919));
#31337=CARTESIAN_POINT('Ctrl Pts',(4.51742571357972,-0.659099555590392,
37.5893568667479));
#31338=CARTESIAN_POINT('Ctrl Pts',(4.37144018896989,-1.31852897836833,37.5661304310039));
#31339=CARTESIAN_POINT('Ctrl Pts',(4.09200051244546,-1.91548778391919,37.5429039952599));
#31340=CARTESIAN_POINT('Ctrl Pts',(3.77369001019247,-2.59548519725224,37.5164466985755));
#31341=CARTESIAN_POINT('Ctrl Pts',(3.282215397723,-3.19442354504401,37.489989401891));
#31342=CARTESIAN_POINT('Ctrl Pts',(2.67743773890556,-3.63935279939737,37.4635321052065));
#31343=CARTESIAN_POINT('Ctrl Pts',(2.07266008008816,-4.08428205375071,37.4370748085221));
#31344=CARTESIAN_POINT('Ctrl Pts',(1.3545793749228,-4.37520221466565,37.4106175118376));
#31345=CARTESIAN_POINT('Ctrl Pts',(0.610657058576267,-4.47667952851312,
37.3841602151531));
#31346=CARTESIAN_POINT('Ctrl Pts',(-0.133265257770265,-4.57815684236059,
37.3577029184686));
#31347=CARTESIAN_POINT('Ctrl Pts',(-0.903029185297969,-4.49019130914057,
37.3312456217842));
#31348=CARTESIAN_POINT('Ctrl Pts',(-1.60487832955574,-4.22349703344512,
37.3047883250997));
#31349=CARTESIAN_POINT('Ctrl Pts',(-2.30672747381355,-3.95680275774965,
37.2783310284153));
#31350=CARTESIAN_POINT('Ctrl Pts',(-2.94066183480143,-3.51137973957871,
37.2518737317308));
#31351=CARTESIAN_POINT('Ctrl Pts',(-3.42946890894599,-2.94148000958195,
37.2254164350463));
#31352=CARTESIAN_POINT('Ctrl Pts',(-3.91827598309049,-2.37158027958525,
37.1989591383619));
#31353=CARTESIAN_POINT('Ctrl Pts',(-4.26195577039172,-1.67720383776276,
37.1725018416774));
#31354=CARTESIAN_POINT('Ctrl Pts',(-4.41864845311754,-0.942924966240358,
37.1460445449929));
#31355=CARTESIAN_POINT('Ctrl Pts',(-4.57534113584337,-0.208646094717874,
37.1195872483085));
#31356=CARTESIAN_POINT('Ctrl Pts',(-4.54504671399375,0.565535206504528,
37.093129951624));
#31357=CARTESIAN_POINT('Ctrl Pts',(-4.33145501462218,1.28532451174858,37.0666726549395));
#31358=CARTESIAN_POINT('Ctrl Pts',(-4.11786331525061,2.00511381699263,37.040215358255));
#31359=CARTESIAN_POINT('Ctrl Pts',(-3.72097433835709,2.67051112625834,37.0137580615706));
#31360=CARTESIAN_POINT('Ctrl Pts',(-3.18912872207783,3.20047178369309,36.9873007648861));
#31361=CARTESIAN_POINT('Ctrl Pts',(-2.65728310579862,3.73043244112779,36.9608434682017));
#31362=CARTESIAN_POINT('Ctrl Pts',(-1.99048085013371,4.12495644673157,36.9343861715172));
#31363=CARTESIAN_POINT('Ctrl Pts',(-1.26993773185218,4.33599121325395,36.9079288748327));
#31364=CARTESIAN_POINT('Ctrl Pts',(-0.549394613570651,4.54702597977633,
36.8814715781482));
#31365=CARTESIAN_POINT('Ctrl Pts',(0.224889367327489,4.57457150721731,36.8550142814638));
#31366=CARTESIAN_POINT('Ctrl Pts',(0.958607278893124,4.41527278082006,36.8285569847793));
#31367=CARTESIAN_POINT('Ctrl Pts',(1.69232519045884,4.25597405442279,36.8020996880948));
#31368=CARTESIAN_POINT('Ctrl Pts',(2.38547703269204,3.90983107418726,36.7756423914104));
#31369=CARTESIAN_POINT('Ctrl Pts',(2.95363767834151,3.4190036720189,36.7491850947259));
#31370=CARTESIAN_POINT('Ctrl Pts',(3.52179832399097,2.92817626985055,36.7227277980414));
#31371=CARTESIAN_POINT('Ctrl Pts',(3.9649677730567,2.29266444574938,36.6962705013569));
#31372=CARTESIAN_POINT('Ctrl Pts',(4.22916847711195,1.58987283655014,36.6698132046725));
#31373=CARTESIAN_POINT('Ctrl Pts',(4.41966640325359,1.08313556444126,36.6507365706123));
#31374=CARTESIAN_POINT('Ctrl Pts',(4.51712003309545,0.541420116342586,36.6316599365521));
#31375=CARTESIAN_POINT('Ctrl Pts',(4.51763788794132,-0.000113968307276224,
36.612583302492));
#31376=CARTESIAN_POINT('Origin',(0.,0.,20.5));
#31377=CARTESIAN_POINT('',(4.51755220121239,0.000103541448102373,35.6125833024919));
#31378=CARTESIAN_POINT('',(4.51785557016588,-0.00011040733672244,35.887416697508));
#31379=CARTESIAN_POINT('',(4.51775,5.53264807684796E-16,20.5));
#31380=CARTESIAN_POINT('Ctrl Pts',(4.51785557016588,-0.000110407336722441,
35.887416697508));
#31381=CARTESIAN_POINT('Ctrl Pts',(4.51723269271139,0.611237967146432,35.9089556674308));
#31382=CARTESIAN_POINT('Ctrl Pts',(4.39224914626368,1.22283323831731,35.9304946373536));
#31383=CARTESIAN_POINT('Ctrl Pts',(4.1508481772843,1.78438254119822,35.9520336072764));
#31384=CARTESIAN_POINT('Ctrl Pts',(3.85432438440574,2.47415909794758,35.9784909039609));
#31385=CARTESIAN_POINT('Ctrl Pts',(3.38214618261964,3.08842466341222,36.0049482006454));
#31386=CARTESIAN_POINT('Ctrl Pts',(2.79182435432918,3.55236237154543,36.0314054973298));
#31387=CARTESIAN_POINT('Ctrl Pts',(2.20150252603872,4.01630007967864,36.0578627940143));
#31388=CARTESIAN_POINT('Ctrl Pts',(1.4930370712439,4.32990993048042,36.0843200906988));
#31389=CARTESIAN_POINT('Ctrl Pts',(0.752718298257879,4.45499459120493,36.1107773873832));
#31390=CARTESIAN_POINT('Ctrl Pts',(0.0123995252718205,4.58007925192944,
36.1372346840677));
#31391=CARTESIAN_POINT('Ctrl Pts',(-0.759772565905438,4.51663872257667,
36.1636919807522));
#31392=CARTESIAN_POINT('Ctrl Pts',(-1.46974826915546,4.27239998941016,36.1901492774366));
#31393=CARTESIAN_POINT('Ctrl Pts',(-2.17972397240549,4.02816125624364,36.2166065741211));
#31394=CARTESIAN_POINT('Ctrl Pts',(-2.82750328772828,3.60312431926339,36.2430638708056));
#31395=CARTESIAN_POINT('Ctrl Pts',(-3.33418741143512,3.04905820699195,36.26952116749));
#31396=CARTESIAN_POINT('Ctrl Pts',(-3.84087153514189,2.49499209472058,36.2959784641745));
#31397=CARTESIAN_POINT('Ctrl Pts',(-4.20646046723274,1.81189680715804,36.322435760859));
#31398=CARTESIAN_POINT('Ctrl Pts',(-4.3864258803877,1.08297259432656,36.3488930575434));
#31399=CARTESIAN_POINT('Ctrl Pts',(-4.56639129354267,0.354048381494999,
36.3753503542279));
#31400=CARTESIAN_POINT('Ctrl Pts',(-4.56073318776171,-0.420704756605515,
36.4018076509124));
#31401=CARTESIAN_POINT('Ctrl Pts',(-4.37014071406692,-1.14692274519782,
36.4282649475969));
#31402=CARTESIAN_POINT('Ctrl Pts',(-4.17954824037214,-1.87314073379008,
36.4547222442813));
#31403=CARTESIAN_POINT('Ctrl Pts',(-3.80402139876356,-2.55082357287414,
36.4811795409658));
#31404=CARTESIAN_POINT('Ctrl Pts',(-3.28929894294182,-3.09743024266232,
36.5076368376502));
#31405=CARTESIAN_POINT('Ctrl Pts',(-2.77457648712008,-3.64403691245051,
36.5340941343347));
#31406=CARTESIAN_POINT('Ctrl Pts',(-2.12065841708519,-4.05956741294281,
36.5605514310192));
#31407=CARTESIAN_POINT('Ctrl Pts',(-1.40719123005584,-4.29341058905986,
36.5870087277037));
#31408=CARTESIAN_POINT('Ctrl Pts',(-0.693724043026525,-4.52725376517689,
36.6134660243881));
#31409=CARTESIAN_POINT('Ctrl Pts',(0.0792922609972423,-4.57940961691868,
36.6399233210726));
#31410=CARTESIAN_POINT('Ctrl Pts',(0.817705151706661,-4.4435256192656,36.6663806177571));
#31411=CARTESIAN_POINT('Ctrl Pts',(1.55611804241612,-4.30764162161251,36.6928379144415));
#31412=CARTESIAN_POINT('Ctrl Pts',(2.25992751981123,-3.98371777456452,36.719295211126));
#31413=CARTESIAN_POINT('Ctrl Pts',(2.84341036847319,-3.51120764419544,36.7457525078105));
#31414=CARTESIAN_POINT('Ctrl Pts',(3.42689321713519,-3.03869751382634,36.7722098044949));
#31415=CARTESIAN_POINT('Ctrl Pts',(3.89004943706403,-2.41760110013612,36.7986671011794));
#31416=CARTESIAN_POINT('Ctrl Pts',(4.17646711326182,-1.72356725892547,36.8251243978639));
#31417=CARTESIAN_POINT('Ctrl Pts',(4.40125218133937,-1.17887865480133,36.8458884977453));
#31418=CARTESIAN_POINT('Ctrl Pts',(4.51717769407857,-0.589265294821556,
36.8666525976266));
#31419=CARTESIAN_POINT('Ctrl Pts',(4.51778606435352,0.000115791782295315,
36.887416697508));
#31420=CARTESIAN_POINT('Ctrl Pts',(4.51763788794132,-0.000113968307276224,
36.612583302492));
#31421=CARTESIAN_POINT('Ctrl Pts',(4.51783824361694,-0.209631033306269,
36.6052026398677));
#31422=CARTESIAN_POINT('Ctrl Pts',(4.50352846951492,-0.419120950359322,
36.5978219772434));
#31423=CARTESIAN_POINT('Ctrl Pts',(4.47448319596349,-0.626547502778321,
36.5904413146191));
#31424=CARTESIAN_POINT('Ctrl Pts',(4.37036525171502,-1.37010483861031,36.5639840179346));
#31425=CARTESIAN_POINT('Ctrl Pts',(4.07689740417331,-2.08714811597701,36.5375267212501));
#31426=CARTESIAN_POINT('Ctrl Pts',(3.62982371237891,-2.69034225726936,36.5110694245657));
#31427=CARTESIAN_POINT('Ctrl Pts',(3.18275002058453,-3.29353639856167,36.4846121278812));
#31428=CARTESIAN_POINT('Ctrl Pts',(2.58207048453748,-3.78288140377964,36.4581548311967));
#31429=CARTESIAN_POINT('Ctrl Pts',(1.90094720693747,-4.09877559286112,36.4316975345123));
#31430=CARTESIAN_POINT('Ctrl Pts',(1.21982392933739,-4.41466978194264,36.4052402378278));
#31431=CARTESIAN_POINT('Ctrl Pts',(0.458256910184331,-4.55711315488762,
36.3787829411434));
#31432=CARTESIAN_POINT('Ctrl Pts',(-0.290995830438852,-4.50875626651792,
36.3523256444589));
#31433=CARTESIAN_POINT('Ctrl Pts',(-1.04024857106204,-4.46039937814821,
36.3258683477744));
#31434=CARTESIAN_POINT('Ctrl Pts',(-1.77718703315534,-4.2212422284638,36.2994110510899));
#31435=CARTESIAN_POINT('Ctrl Pts',(-2.41205292762861,-3.82041389361357,
36.2729537544055));
#31436=CARTESIAN_POINT('Ctrl Pts',(-3.04691882210185,-3.41958555876337,
36.246496457721));
#31437=CARTESIAN_POINT('Ctrl Pts',(-3.57971214895505,-2.85708603874736,
36.2200391610366));
#31438=CARTESIAN_POINT('Ctrl Pts',(-3.94553927063653,-2.20142715256771,
36.1935818643521));
#31439=CARTESIAN_POINT('Ctrl Pts',(-4.311366392318,-1.54576826638806,36.1671245676676));
#31440=CARTESIAN_POINT('Ctrl Pts',(-4.51022730882774,-0.796950014044777,
36.1406672709831));
#31441=CARTESIAN_POINT('Ctrl Pts',(-4.51790098062044,-0.0461776299327186,
36.1142099742986));
#31442=CARTESIAN_POINT('Ctrl Pts',(-4.52557465241315,0.70459475417934,36.0877526776142));
#31443=CARTESIAN_POINT('Ctrl Pts',(-4.34206107948882,1.45732127006017,36.0612953809297));
#31444=CARTESIAN_POINT('Ctrl Pts',(-3.98971201192945,2.12032066114143,36.0348380842453));
#31445=CARTESIAN_POINT('Ctrl Pts',(-3.63736294437007,2.78332005222269,36.0083807875608));
#31446=CARTESIAN_POINT('Ctrl Pts',(-3.11617838217574,3.3565923185043,35.9819234908763));
#31447=CARTESIAN_POINT('Ctrl Pts',(-2.48963802821032,3.77031353241165,35.9554661941919));
#31448=CARTESIAN_POINT('Ctrl Pts',(-1.86309767424487,4.18403474631902,35.9290088975074));
#31449=CARTESIAN_POINT('Ctrl Pts',(-1.13120152850826,4.43820490785206,35.9025516008229));
#31450=CARTESIAN_POINT('Ctrl Pts',(-0.383093731539153,4.501866372634,35.8760943041385));
#31451=CARTESIAN_POINT('Ctrl Pts',(0.365014065429868,4.56552783741593,35.849637007454));
#31452=CARTESIAN_POINT('Ctrl Pts',(1.12933351363151,4.43868060544686,35.8231797107695));
#31453=CARTESIAN_POINT('Ctrl Pts',(1.81677135017102,4.13677452919484,35.7967224140851));
#31454=CARTESIAN_POINT('Ctrl Pts',(2.50420918671061,3.83486845294278,35.7702651174006));
#31455=CARTESIAN_POINT('Ctrl Pts',(3.11476541158806,3.35790353240771,35.7438078207161));
#31456=CARTESIAN_POINT('Ctrl Pts',(3.57407495233493,2.76397356703885,35.7173505240316));
#31457=CARTESIAN_POINT('Ctrl Pts',(4.03338449308179,2.17004360166999,35.6908932273472));
#31458=CARTESIAN_POINT('Ctrl Pts',(4.34144734969803,1.45914859146745,35.6644359306627));
#31459=CARTESIAN_POINT('Ctrl Pts',(4.46074180719067,0.717874761903989,35.6379786339782));
#31460=CARTESIAN_POINT('Ctrl Pts',(4.49891051264125,0.480701442593838,35.6295135234828));
#31461=CARTESIAN_POINT('Ctrl Pts',(4.51775492478579,0.240418231912197,35.6210484129874));
#31462=CARTESIAN_POINT('Ctrl Pts',(4.51755220121239,0.000103541448102373,
35.6125833024919));
#31463=CARTESIAN_POINT('Origin',(0.,0.,20.5));
#31464=CARTESIAN_POINT('',(4.51806911322653,-6.09724841136444E-5,34.6125833024919));
#31465=CARTESIAN_POINT('',(4.51740954388543,5.82741782004033E-5,34.887416697508));
#31466=CARTESIAN_POINT('',(4.51775,5.53264807684796E-16,20.5));
#31467=CARTESIAN_POINT('Ctrl Pts',(4.51740954388543,5.82741782004033E-5,
34.887416697508));
#31468=CARTESIAN_POINT('Ctrl Pts',(4.51755065915555,0.31030389790581,34.8983441438661));
#31469=CARTESIAN_POINT('Ctrl Pts',(4.48605373157874,0.620521268509011,34.9092715902241));
#31470=CARTESIAN_POINT('Ctrl Pts',(4.42263045256682,0.924067921868281,34.9201990365822));
#31471=CARTESIAN_POINT('Ctrl Pts',(4.26907138171545,1.65900851112936,34.9466563332667));
#31472=CARTESIAN_POINT('Ctrl Pts',(3.92835669717202,2.35484465771423,34.9731136299511));
#31473=CARTESIAN_POINT('Ctrl Pts',(3.44198507043434,2.92682428907246,34.9995709266356));
#31474=CARTESIAN_POINT('Ctrl Pts',(2.95561344369671,3.49880392043062,35.02602822332));
#31475=CARTESIAN_POINT('Ctrl Pts',(2.32358487476487,3.94692703656216,35.0524855200045));
#31476=CARTESIAN_POINT('Ctrl Pts',(1.62287974384894,4.21661273787411,35.078942816689));
#31477=CARTESIAN_POINT('Ctrl Pts',(0.922174612932932,4.48629843918609,35.1054001133734));
#31478=CARTESIAN_POINT('Ctrl Pts',(0.152792920032838,4.57754672567843,35.1318574100579));
#31479=CARTESIAN_POINT('Ctrl Pts',(-0.591555496154874,4.47924365704371,
35.1583147067424));
#31480=CARTESIAN_POINT('Ctrl Pts',(-1.3359039123425,4.380940588409,35.1847720034269));
#31481=CARTESIAN_POINT('Ctrl Pts',(-2.05521905181772,4.09308616464727,35.2112293001113));
#31482=CARTESIAN_POINT('Ctrl Pts',(-2.66188912668102,3.65074073599519,35.2376865967958));
#31483=CARTESIAN_POINT('Ctrl Pts',(-3.26855920154439,3.20839530734307,35.2641438934803));
#31484=CARTESIAN_POINT('Ctrl Pts',(-3.76258421179579,2.61155887380058,35.2906011901647));
#31485=CARTESIAN_POINT('Ctrl Pts',(-4.08379245793952,1.93292545243568,35.3170584868492));
#31486=CARTESIAN_POINT('Ctrl Pts',(-4.40500070408323,1.25429203107082,35.3435157835337));
#31487=CARTESIAN_POINT('Ctrl Pts',(-4.55339218611928,0.493861621883449,
35.3699730802181));
#31488=CARTESIAN_POINT('Ctrl Pts',(-4.51089298576514,-0.255746192879281,
35.3964303769026));
#31489=CARTESIAN_POINT('Ctrl Pts',(-4.468393785411,-1.00535400764205,35.4228876735871));
#31490=CARTESIAN_POINT('Ctrl Pts',(-4.23500390266671,-1.74413922798016,
35.4493449702715));
#31491=CARTESIAN_POINT('Ctrl Pts',(-3.83914996695061,-2.38211863169333,
35.475802266956));
#31492=CARTESIAN_POINT('Ctrl Pts',(-3.44329603123454,-3.02009803540644,
35.5022595636405));
#31493=CARTESIAN_POINT('Ctrl Pts',(-2.88497804254663,-3.55727162249458,
35.5287168603249));
#31494=CARTESIAN_POINT('Ctrl Pts',(-2.23219851400125,-3.92821224455706,
35.5551741570094));
#31495=CARTESIAN_POINT('Ctrl Pts',(-1.57941898545579,-4.29915286661958,
35.5816314536939));
#31496=CARTESIAN_POINT('Ctrl Pts',(-0.83217791705278,-4.50386052365648,
35.6080887503783));
#31497=CARTESIAN_POINT('Ctrl Pts',(-0.081488443928666,-4.51740204959703,
35.6345460470628));
#31498=CARTESIAN_POINT('Ctrl Pts',(0.669201029195319,-4.53094357553758,
35.6610033437473));
#31499=CARTESIAN_POINT('Ctrl Pts',(1.42333890704038,-4.35331897038184,35.6874606404318));
#31500=CARTESIAN_POINT('Ctrl Pts',(2.08907203071298,-4.00616271445508,35.7139179371162));
#31501=CARTESIAN_POINT('Ctrl Pts',(2.75480515438577,-3.65900645852822,35.7403752338007));
#31502=CARTESIAN_POINT('Ctrl Pts',(3.33213352388603,-3.14231855183025,35.7668325304851));
#31503=CARTESIAN_POINT('Ctrl Pts',(3.75073918275594,-2.51903100956234,35.7932898271696));
#31504=CARTESIAN_POINT('Ctrl Pts',(4.16934484162576,-1.89574346729458,35.8197471238541));
#31505=CARTESIAN_POINT('Ctrl Pts',(4.42922778986531,-1.16585628945694,35.8462044205385));
#31506=CARTESIAN_POINT('Ctrl Pts',(4.49873457199958,-0.4182689265211,35.872661717223));
#31507=CARTESIAN_POINT('Ctrl Pts',(4.51165566030144,-0.279294828839705,
35.8775800439847));
#31508=CARTESIAN_POINT('Ctrl Pts',(4.51799780142692,-0.139709054890449,
35.8824983707463));
#31509=CARTESIAN_POINT('Ctrl Pts',(4.51785557016588,-0.000110407336722441,
35.887416697508));
#31510=CARTESIAN_POINT('Ctrl Pts',(4.51755220121239,0.000103541448102373,
35.6125833024919));
#31511=CARTESIAN_POINT('Ctrl Pts',(4.51712132198412,-0.510673802465055,
35.5945911163029));
#31512=CARTESIAN_POINT('Ctrl Pts',(4.43064412559555,-1.02159335775301,35.5765989301139));
#31513=CARTESIAN_POINT('Ctrl Pts',(4.26078183149926,-1.50309674624197,35.5586067439248));
#31514=CARTESIAN_POINT('Ctrl Pts',(4.01100133994626,-2.21114177590013,35.5321494472404));
#31515=CARTESIAN_POINT('Ctrl Pts',(3.58091429847129,-2.85557918629222,35.5056921505559));
#31516=CARTESIAN_POINT('Ctrl Pts',(3.02290483273525,-3.35791721405148,35.4792348538714));
#31517=CARTESIAN_POINT('Ctrl Pts',(2.46489536699924,-3.86025524181071,35.452777557187));
#31518=CARTESIAN_POINT('Ctrl Pts',(1.77896347700217,-4.22049388693713,35.4263202605025));
#31519=CARTESIAN_POINT('Ctrl Pts',(1.04865490780343,-4.39475648114172,35.399862963818));
#31520=CARTESIAN_POINT('Ctrl Pts',(0.318346338604615,-4.56901907534632,
35.3734056671336));
#31521=CARTESIAN_POINT('Ctrl Pts',(-0.456338909795902,-4.55730561862904,
35.3469483704491));
#31522=CARTESIAN_POINT('Ctrl Pts',(-1.18104503151125,-4.36104279705439,
35.3204910737646));
#31523=CARTESIAN_POINT('Ctrl Pts',(-1.9057511532266,-4.16477997547974,35.2940337770802));
#31524=CARTESIAN_POINT('Ctrl Pts',(-2.5804781482568,-3.78396778904771,35.2675764803957));
#31525=CARTESIAN_POINT('Ctrl Pts',(-3.1230450153486,-3.26498874060901,35.2411191837112));
#31526=CARTESIAN_POINT('Ctrl Pts',(-3.66561188244036,-2.74600969217034,
35.2146618870268));
#31527=CARTESIAN_POINT('Ctrl Pts',(-4.07601862159375,-2.08886378172499,
35.1882045903423));
#31528=CARTESIAN_POINT('Ctrl Pts',(-4.30427814618982,-1.37359065388133,
35.1617472936578));
#31529=CARTESIAN_POINT('Ctrl Pts',(-4.53253767078589,-0.658317526037631,
35.1352899969733));
#31530=CARTESIAN_POINT('Ctrl Pts',(-4.57864998082464,0.115082819204295,
35.1088327002889));
#31531=CARTESIAN_POINT('Ctrl Pts',(-4.43699864797729,0.852411075740494,
35.0823754036044));
#31532=CARTESIAN_POINT('Ctrl Pts',(-4.29534731512995,1.58973933227665,35.0559181069199));
#31533=CARTESIAN_POINT('Ctrl Pts',(-3.9659323393965,2.29099550010699,35.0294608102355));
#31534=CARTESIAN_POINT('Ctrl Pts',(-3.48887610024745,2.87076735409185,35.003003513551));
#31535=CARTESIAN_POINT('Ctrl Pts',(-3.0118198610984,3.45053920807671,34.9765462168666));
#31536=CARTESIAN_POINT('Ctrl Pts',(-2.38712235853373,3.90882674821612,34.9500889201821));
#31537=CARTESIAN_POINT('Ctrl Pts',(-1.69087105699361,4.18981105932221,34.9236316234976));
#31538=CARTESIAN_POINT('Ctrl Pts',(-0.994619755453442,4.47079537042831,
34.8971743268131));
#31539=CARTESIAN_POINT('Ctrl Pts',(-0.22681465493779,4.57447645250109,34.8707170301287));
#31540=CARTESIAN_POINT('Ctrl Pts',(0.519026433064394,4.48822606449116,34.8442597334442));
#31541=CARTESIAN_POINT('Ctrl Pts',(1.26486752106653,4.40197567648124,34.8178024367597));
#31542=CARTESIAN_POINT('Ctrl Pts',(1.98874459655524,4.12579381838863,34.7913451400753));
#31543=CARTESIAN_POINT('Ctrl Pts',(2.60249023287332,3.69331913486993,34.7648878433908));
#31544=CARTESIAN_POINT('Ctrl Pts',(3.2162358691914,3.26084445135124,34.7384305467063));
#31545=CARTESIAN_POINT('Ctrl Pts',(3.71985006633887,2.67207694240644,34.7119732500218));
#31546=CARTESIAN_POINT('Ctrl Pts',(4.05199317246873,1.99872783901765,34.6855159533374));
#31547=CARTESIAN_POINT('Ctrl Pts',(4.35719035466755,1.38000583275685,34.6612050697222));
#31548=CARTESIAN_POINT('Ctrl Pts',(4.51760990627478,0.689869322963186,34.6368941861071));
#31549=CARTESIAN_POINT('Ctrl Pts',(4.51806911322653,-6.09724841136444E-5,
34.6125833024919));
#31550=CARTESIAN_POINT('Origin',(0.,0.,20.5));
#31551=CARTESIAN_POINT('',(4.5173649459528,-1.24327273773317E-5,33.6125833024919));
#31552=CARTESIAN_POINT('',(4.51813527504661,9.51052893547258E-6,33.887416697508));
#31553=CARTESIAN_POINT('',(4.51775,5.53264807684796E-16,20.5));
#31554=CARTESIAN_POINT('Ctrl Pts',(4.51813527504661,9.51052893547258E-6,
33.887416697508));
#31555=CARTESIAN_POINT('Ctrl Pts',(4.51813637042829,0.00897485417732503,
33.8877326203013));
#31556=CARTESIAN_POINT('Ctrl Pts',(4.51811024333632,0.0179401914138076,
33.8880485430946));
#31557=CARTESIAN_POINT('Ctrl Pts',(4.51805685504966,0.0269053663078375,
33.8883644658879));
#31558=CARTESIAN_POINT('Ctrl Pts',(4.51358579512714,0.777703653204736,33.9148217625724));
#31559=CARTESIAN_POINT('Ctrl Pts',(4.31792089423795,1.52736336648647,33.9412790592569));
#31560=CARTESIAN_POINT('Ctrl Pts',(3.95489392076193,2.18457678274711,33.9677363559413));
#31561=CARTESIAN_POINT('Ctrl Pts',(3.59186694728593,2.84179019900772,33.9941936526258));
#31562=CARTESIAN_POINT('Ctrl Pts',(3.06147790122311,3.40655731824726,34.0206509493103));
#31563=CARTESIAN_POINT('Ctrl Pts',(2.42832758138582,3.81009013038776,34.0471082459947));
#31564=CARTESIAN_POINT('Ctrl Pts',(1.79517726154854,4.21362294252827,34.0735655426792));
#31565=CARTESIAN_POINT('Ctrl Pts',(1.05926566793676,4.45592144756974,34.1000228393637));
#31566=CARTESIAN_POINT('Ctrl Pts',(0.310226018196078,4.50747395575744,34.1264801360482));
#31567=CARTESIAN_POINT('Ctrl Pts',(-0.438813631544642,4.55902646394514,
34.1529374327326));
#31568=CARTESIAN_POINT('Ctrl Pts',(-1.20098133741429,4.41983297527906,34.1793947294171));
#31569=CARTESIAN_POINT('Ctrl Pts',(-1.8834459163527,4.10684710262894,34.2058520261016));
#31570=CARTESIAN_POINT('Ctrl Pts',(-2.56591049529112,3.79386122997882,34.232309322786));
#31571=CARTESIAN_POINT('Ctrl Pts',(-3.16867194729824,3.30708297334475,34.2587666194705));
#31572=CARTESIAN_POINT('Ctrl Pts',(-3.61831459461467,2.70580138565192,34.2852239161549));
#31573=CARTESIAN_POINT('Ctrl Pts',(-4.06795724193109,2.10451979795912,34.3116812128394));
#31574=CARTESIAN_POINT('Ctrl Pts',(-4.36448108455674,1.38873487920764,34.3381385095239));
#31575=CARTESIAN_POINT('Ctrl Pts',(-4.47176984663203,0.645628440319887,
34.3645958062084));
#31576=CARTESIAN_POINT('Ctrl Pts',(-4.57905860870732,-0.0974779985678242,
34.3910531028928));
#31577=CARTESIAN_POINT('Ctrl Pts',(-4.49711229023226,-0.86790595759181,
34.4175103995773));
#31578=CARTESIAN_POINT('Ctrl Pts',(-4.23591186210457,-1.57181816399963,
34.4439676962618));
#31579=CARTESIAN_POINT('Ctrl Pts',(-3.97471143397686,-2.27573037040753,
34.4704249929462));
#31580=CARTESIAN_POINT('Ctrl Pts',(-3.53425689619645,-2.91312682419928,
34.4968822896307));
#31581=CARTESIAN_POINT('Ctrl Pts',(-2.96819512400025,-3.40637334272956,
34.5233395863152));
#31582=CARTESIAN_POINT('Ctrl Pts',(-2.40213335180411,-3.89961986125978,
34.5497968829996));
#31583=CARTESIAN_POINT('Ctrl Pts',(-1.71046434519219,-4.24871644452859,
34.5762541796841));
#31584=CARTESIAN_POINT('Ctrl Pts',(-0.977432623678127,-4.41114351504993,
34.6027114763686));
#31585=CARTESIAN_POINT('Ctrl Pts',(-0.244400902164024,-4.57357058557128,
34.629168773053));
#31586=CARTESIAN_POINT('Ctrl Pts',(0.529993534252376,-4.54932814334514,
34.6556260697375));
#31587=CARTESIAN_POINT('Ctrl Pts',(1.25143030026179,-4.34136889100478,34.682083366422));
#31588=CARTESIAN_POINT('Ctrl Pts',(1.97286706627129,-4.13340963866439,34.7085406631064));
#31589=CARTESIAN_POINT('Ctrl Pts',(2.64134616187382,-3.74173357620983,34.7349979597909));
#31590=CARTESIAN_POINT('Ctrl Pts',(3.17544757305189,-3.21404641456781,34.7614552564754));
#31591=CARTESIAN_POINT('Ctrl Pts',(3.70954898422987,-2.68635925292589,34.7879125531598));
#31592=CARTESIAN_POINT('Ctrl Pts',(4.10927271098332,-2.0226609920966,34.8143698498443));
#31593=CARTESIAN_POINT('Ctrl Pts',(4.3259328457804,-1.30378934571338,34.8408271465288));
#31594=CARTESIAN_POINT('Ctrl Pts',(4.45310757210366,-0.881827525298336,
34.8563569968552));
#31595=CARTESIAN_POINT('Ctrl Pts',(4.51720899391685,-0.440856093465167,
34.8718868471816));
#31596=CARTESIAN_POINT('Ctrl Pts',(4.51740954388543,5.82741782004033E-5,
34.887416697508));
#31597=CARTESIAN_POINT('Ctrl Pts',(4.51806911322653,-6.09724841136444E-5,
34.6125833024919));
#31598=CARTESIAN_POINT('Ctrl Pts',(4.51810965670567,-0.0609750645635587,
34.6104368894226));
#31599=CARTESIAN_POINT('Ctrl Pts',(4.51690328345783,-0.121887549168861,
34.6082904763533));
#31600=CARTESIAN_POINT('Ctrl Pts',(4.51443954418555,-0.182749134310292,
34.606144063284));
#31601=CARTESIAN_POINT('Ctrl Pts',(4.48407079466025,-0.932946306416683,
34.5796867665996));
#31602=CARTESIAN_POINT('Ctrl Pts',(4.26266128049739,-1.67540995279661,34.5532294699151));
#31603=CARTESIAN_POINT('Ctrl Pts',(3.87717843548116,-2.3197088230287,34.5267721732306));
#31604=CARTESIAN_POINT('Ctrl Pts',(3.49169559046496,-2.96400769326076,34.5003148765461));
#31605=CARTESIAN_POINT('Ctrl Pts',(2.94213941459544,-3.51014178734499,34.4738575798616));
#31606=CARTESIAN_POINT('Ctrl Pts',(2.2954452418825,-3.8915925770456,34.4474002831772));
#31607=CARTESIAN_POINT('Ctrl Pts',(1.64875106916955,-4.2730433667462,34.4209429864927));
#31608=CARTESIAN_POINT('Ctrl Pts',(0.904918899613214,-4.48981085206318,
34.3944856898083));
#31609=CARTESIAN_POINT('Ctrl Pts',(0.154546668243127,-4.51549299318827,
34.3680283931238));
#31610=CARTESIAN_POINT('Ctrl Pts',(-0.595825563126962,-4.54117513431336,
34.3415710964393));
#31611=CARTESIAN_POINT('Ctrl Pts',(-1.35273785631077,-4.37577193124655,
34.3151137997548));
#31612=CARTESIAN_POINT('Ctrl Pts',(-2.02399913169702,-4.03942931106451,
34.2886565030704));
#31613=CARTESIAN_POINT('Ctrl Pts',(-2.69526040708323,-3.70308669088248,
34.2621992063859));
#31614=CARTESIAN_POINT('Ctrl Pts',(-3.28087066467185,-3.19580465358524,
34.2357419097014));
#31615=CARTESIAN_POINT('Ctrl Pts',(-3.7095032232018,-2.57936958989069,34.209284613017));
#31616=CARTESIAN_POINT('Ctrl Pts',(-4.13813578173176,-1.9629345261961,34.1828273163325));
#31617=CARTESIAN_POINT('Ctrl Pts',(-4.40979064120305,-1.23734643610409,
34.1563700196481));
#31618=CARTESIAN_POINT('Ctrl Pts',(-4.49138054038088,-0.490981145957072,
34.1299127229636));
#31619=CARTESIAN_POINT('Ctrl Pts',(-4.57297043955872,0.255384144190028,
34.1034554262791));
#31620=CARTESIAN_POINT('Ctrl Pts',(-4.46449537844313,1.02252663439224,34.0769981295946));
#31621=CARTESIAN_POINT('Ctrl Pts',(-4.17916749942524,1.71700921836348,34.0505408329102));
#31622=CARTESIAN_POINT('Ctrl Pts',(-3.89383962040737,2.41149180233465,34.0240835362257));
#31623=CARTESIAN_POINT('Ctrl Pts',(-3.43165892348727,3.03331448007484,33.9976262395413));
#31624=CARTESIAN_POINT('Ctrl Pts',(-2.84891850603996,3.50673993762589,33.9711689428568));
#31625=CARTESIAN_POINT('Ctrl Pts',(-2.26617808859268,3.98016539517692,33.9447116461723));
#31626=CARTESIAN_POINT('Ctrl Pts',(-1.56287795061823,4.30519363253881,33.9182543494878));
#31627=CARTESIAN_POINT('Ctrl Pts',(-0.824679270557638,4.44223657011982,
33.8917970528033));
#31628=CARTESIAN_POINT('Ctrl Pts',(-0.0864805904969625,4.57927950770084,
33.8653397561189));
#31629=CARTESIAN_POINT('Ctrl Pts',(0.686616631649836,4.52833714550091,33.8388824594344));
#31630=CARTESIAN_POINT('Ctrl Pts',(1.40045000983613,4.2956142068565,33.81242516275));
#31631=CARTESIAN_POINT('Ctrl Pts',(2.11428338802235,4.0628912682121,33.7859678660655));
#31632=CARTESIAN_POINT('Ctrl Pts',(2.76885292224806,3.64838775312326,33.759510569381));
#31633=CARTESIAN_POINT('Ctrl Pts',(3.28443276767714,3.10258973098379,33.7330532726965));
#31634=CARTESIAN_POINT('Ctrl Pts',(3.80001261310627,2.55679170884426,33.7065959760121));
#31635=CARTESIAN_POINT('Ctrl Pts',(4.17660276973874,1.87969917965409,33.6801386793276));
#31636=CARTESIAN_POINT('Ctrl Pts',(4.36833497328078,1.15378126410918,33.6536813826432));
#31637=CARTESIAN_POINT('Ctrl Pts',(4.46761225473945,0.777907227895749,33.6399820225928));
#31638=CARTESIAN_POINT('Ctrl Pts',(4.51732765695876,0.388942719447438,33.6262826625424));
#31639=CARTESIAN_POINT('Ctrl Pts',(4.5173649459528,-1.24327273773317E-5,
33.6125833024919));
#31640=CARTESIAN_POINT('Origin',(0.,0.,20.5));
#31641=CARTESIAN_POINT('',(4.51800690475437,8.25810157162321E-5,32.6125833024919));
#31642=CARTESIAN_POINT('',(4.5174378855045,-7.22228901865168E-5,32.887416697508));
#31643=CARTESIAN_POINT('',(4.51775,5.53264807684796E-16,20.5));
#31644=CARTESIAN_POINT('Ctrl Pts',(4.5174378855045,-7.22228901865168E-5,
32.887416697508));
#31645=CARTESIAN_POINT('Ctrl Pts',(4.51717714450692,0.458772891828189,32.9035783934211));
#31646=CARTESIAN_POINT('Ctrl Pts',(4.44766773093088,0.917695233524441,32.9197400893341));
#31647=CARTESIAN_POINT('Ctrl Pts',(4.31009826091021,1.35521755651858,32.9359017852471));
#31648=CARTESIAN_POINT('Ctrl Pts',(4.08489192720295,2.07145785505129,32.9623590819316));
#31649=CARTESIAN_POINT('Ctrl Pts',(3.67729208498414,2.73034844367792,32.988816378616));
#31650=CARTESIAN_POINT('Ctrl Pts',(3.13694394393257,3.25163717791855,33.0152736753005));
#31651=CARTESIAN_POINT('Ctrl Pts',(2.596595802881,3.77292591215919,33.0417309719849));
#31652=CARTESIAN_POINT('Ctrl Pts',(1.92349936299679,4.15661279201376,33.0681882686694));
#31653=CARTESIAN_POINT('Ctrl Pts',(1.19963702572075,4.35596518015436,33.0946455653539));
#31654=CARTESIAN_POINT('Ctrl Pts',(0.475774688444753,4.55531756829496,33.1211028620384));
#31655=CARTESIAN_POINT('Ctrl Pts',(-0.298853546223071,4.57033546472152,
33.1475601587228));
#31656=CARTESIAN_POINT('Ctrl Pts',(-1.02989881660521,4.39918970627007,33.1740174554073));
#31657=CARTESIAN_POINT('Ctrl Pts',(-1.76094408698744,4.2280439478186,33.2004747520918));
#31658=CARTESIAN_POINT('Ctrl Pts',(-2.4484063930841,3.87073453448909,33.2269320487762));
#31659=CARTESIAN_POINT('Ctrl Pts',(-3.00855358684862,3.37078135737958,33.2533893454607));
#31660=CARTESIAN_POINT('Ctrl Pts',(-3.56870078061313,2.87082818027007,33.2798466421452));
#31661=CARTESIAN_POINT('Ctrl Pts',(-4.0015328620455,2.22823123938057,33.3063039388296));
#31662=CARTESIAN_POINT('Ctrl Pts',(-4.25433136265604,1.52125813092933,33.3327612355141));
#31663=CARTESIAN_POINT('Ctrl Pts',(-4.50712986326656,0.814285022478126,
33.3592185321986));
#31664=CARTESIAN_POINT('Ctrl Pts',(-4.57989478305528,0.0429357464651833,
33.3856758288831));
#31665=CARTESIAN_POINT('Ctrl Pts',(-4.46376343532313,-0.698840208967454,
33.4121331255675));
#31666=CARTESIAN_POINT('Ctrl Pts',(-4.34763208759097,-1.44061616440009,
33.438590422252));
#31667=CARTESIAN_POINT('Ctrl Pts',(-4.04260447233795,-2.15281879925242,
33.4650477189364));
#31668=CARTESIAN_POINT('Ctrl Pts',(-3.5858326155183,-2.74870262081633,33.4915050156209));
#31669=CARTESIAN_POINT('Ctrl Pts',(-3.12906075869862,-3.34458644238028,
33.5179623123054));
#31670=CARTESIAN_POINT('Ctrl Pts',(-2.52054466031228,-3.82415145065579,
33.5444196089899));
#31671=CARTESIAN_POINT('Ctrl Pts',(-1.83440090767899,-4.12898715838447,
33.5708769056743));
#31672=CARTESIAN_POINT('Ctrl Pts',(-1.14825715504573,-4.43382286611314,
33.5973342023588));
#31673=CARTESIAN_POINT('Ctrl Pts',(-0.384485748165517,-4.56392927329501,
33.6237914990433));
#31674=CARTESIAN_POINT('Ctrl Pts',(0.363886800893304,-4.50345956352814,
33.6502487957277));
#31675=CARTESIAN_POINT('Ctrl Pts',(1.11225934995217,-4.44298985376126,33.6767060924122));
#31676=CARTESIAN_POINT('Ctrl Pts',(1.84523304118964,-4.19194402704563,33.7031633890966));
#31677=CARTESIAN_POINT('Ctrl Pts',(2.47353249021786,-3.78089918723496,33.7296206857811));
#31678=CARTESIAN_POINT('Ctrl Pts',(3.10183193924602,-3.36985434742433,33.7560779824656));
#31679=CARTESIAN_POINT('Ctrl Pts',(3.62545714606495,-2.7988104945187,33.7825352791501));
#31680=CARTESIAN_POINT('Ctrl Pts',(3.98063113999648,-2.1373201378099,33.8089925758346));
#31681=CARTESIAN_POINT('Ctrl Pts',(4.3315640520969,-1.48372854278193,33.8351339497257));
#31682=CARTESIAN_POINT('Ctrl Pts',(4.51804463650222,-0.741837565236255,
33.8612753236169));
#31683=CARTESIAN_POINT('Ctrl Pts',(4.51813527504661,9.51052893547258E-6,
33.887416697508));
#31684=CARTESIAN_POINT('Ctrl Pts',(4.5173649459528,-1.24327273773317E-5,
33.6125833024919));
#31685=CARTESIAN_POINT('Ctrl Pts',(4.51739967243793,-0.362238490490815,
33.5998253658579));
#31686=CARTESIAN_POINT('Ctrl Pts',(4.47434946667155,-0.724456433726874,
33.5870674292238));
#31687=CARTESIAN_POINT('Ctrl Pts',(4.38812044853862,-1.07608576485082,33.5743094925897));
#31688=CARTESIAN_POINT('Ctrl Pts',(4.20929946980279,-1.80529157636637,33.5478521959053));
#31689=CARTESIAN_POINT('Ctrl Pts',(3.84478326187951,-2.48895989749788,33.5213948992208));
#31690=CARTESIAN_POINT('Ctrl Pts',(3.33896949547234,-3.04382068336861,33.4949376025364));
#31691=CARTESIAN_POINT('Ctrl Pts',(2.83315572906515,-3.59868146923937,33.4684803058519));
#31692=CARTESIAN_POINT('Ctrl Pts',(2.18604440417407,-4.02473471984934,33.4420230091674));
#31693=CARTESIAN_POINT('Ctrl Pts',(1.47645296399252,-4.27008762080067,33.4155657124829));
#31694=CARTESIAN_POINT('Ctrl Pts',(0.766861523811012,-4.51544052175197,
33.3891084157985));
#31695=CARTESIAN_POINT('Ctrl Pts',(-0.00521003166095199,-4.58009307304465,
33.362651119114));
#31696=CARTESIAN_POINT('Ctrl Pts',(-0.745724241442587,-4.45617066548424,
33.3361938224295));
#31697=CARTESIAN_POINT('Ctrl Pts',(-1.48623845122422,-4.33224825792383,
33.3097365257451));
#31698=CARTESIAN_POINT('Ctrl Pts',(-2.19519531531565,-4.01975089151028,
33.2832792290606));
#31699=CARTESIAN_POINT('Ctrl Pts',(-2.78624467229499,-3.55674039962226,
33.2568219323761));
#31700=CARTESIAN_POINT('Ctrl Pts',(-3.37729402927434,-3.09372990773425,
33.2303646356917));
#31701=CARTESIAN_POINT('Ctrl Pts',(-3.85043587914167,-2.48020629037183,
33.2039073390072));
#31702=CARTESIAN_POINT('Ctrl Pts',(-4.14804206822415,-1.7908960451238,33.1774500423227));
#31703=CARTESIAN_POINT('Ctrl Pts',(-4.44564825730663,-1.10158579987578,
33.1509927456383));
#31704=CARTESIAN_POINT('Ctrl Pts',(-4.56771878560417,-0.33648892674225,
33.1245354489538));
#31705=CARTESIAN_POINT('Ctrl Pts',(-4.49938559786941,0.411206621885727,
33.0980781522693));
#31706=CARTESIAN_POINT('Ctrl Pts',(-4.43105241013465,1.15890217051366,33.0716208555848));
#31707=CARTESIAN_POINT('Ctrl Pts',(-4.17231550636761,1.88919639463604,33.0451635589004));
#31708=CARTESIAN_POINT('Ctrl Pts',(-3.75468875509488,2.51314026599421,33.0187062622159));
#31709=CARTESIAN_POINT('Ctrl Pts',(-3.33706200382211,3.13708413735244,32.9922489655315));
#31710=CARTESIAN_POINT('Ctrl Pts',(-2.76054540504362,3.65467765594643,32.965791668847));
#31711=CARTESIAN_POINT('Ctrl Pts',(-2.09535804244172,4.00287850404833,32.9393343721625));
#31712=CARTESIAN_POINT('Ctrl Pts',(-1.43017067983982,4.35107935215023,32.912877075478));
#31713=CARTESIAN_POINT('Ctrl Pts',(-0.676312553414512,4.52988752976003,
32.8864197787936));
#31714=CARTESIAN_POINT('Ctrl Pts',(0.0743972513539278,4.51752439873747,
32.8599624821091));
#31715=CARTESIAN_POINT('Ctrl Pts',(0.825107056122282,4.50516126771491,32.8335051854247));
#31716=CARTESIAN_POINT('Ctrl Pts',(1.57266853923377,4.30162682806002,32.8070478887402));
#31717=CARTESIAN_POINT('Ctrl Pts',(2.22602953939506,3.93171134926485,32.7805905920557));
#31718=CARTESIAN_POINT('Ctrl Pts',(2.87939053955642,3.56179587046963,32.7541332953712));
#31719=CARTESIAN_POINT('Ctrl Pts',(3.43855105676757,3.02549935253409,32.7276759986868));
#31720=CARTESIAN_POINT('Ctrl Pts',(3.83540595887257,2.38814211780667,32.7012187020023));
#31721=CARTESIAN_POINT('Ctrl Pts',(4.23226086097758,1.75078488307926,32.6747614053179));
#31722=CARTESIAN_POINT('Ctrl Pts',(4.46681014797645,1.01236693155997,32.6483041086334));
#31723=CARTESIAN_POINT('Ctrl Pts',(4.51048597629574,0.262826752513661,32.6218468119489));
#31724=CARTESIAN_POINT('Ctrl Pts',(4.51558339111607,0.175347765528612,32.6187589754633));
#31725=CARTESIAN_POINT('Ctrl Pts',(4.51808086670496,0.0877172796610649,
32.6156711389776));
#31726=CARTESIAN_POINT('Ctrl Pts',(4.51800690475437,8.25810157162321E-5,
32.6125833024919));
#31727=CARTESIAN_POINT('Origin',(0.,0.,20.5));
#31728=CARTESIAN_POINT('',(4.51762600826661,-0.000112987348963034,31.612583302492));
#31729=CARTESIAN_POINT('',(4.51779894817057,0.000115094980599771,31.887416697508));
#31730=CARTESIAN_POINT('',(4.51775,5.53264807684796E-16,20.5));
#31731=CARTESIAN_POINT('Ctrl Pts',(4.51779894817057,0.000115094980599771,
31.887416697508));
#31732=CARTESIAN_POINT('Ctrl Pts',(4.51796156278444,0.157653334629133,31.8929668698563));
#31733=CARTESIAN_POINT('Ctrl Pts',(4.50988180917274,0.315174976505045,31.8985170422046));
#31734=CARTESIAN_POINT('Ctrl Pts',(4.49343403803756,0.471817962781026,31.9040672145528));
#31735=CARTESIAN_POINT('Ctrl Pts',(4.41502862404034,1.21852449753214,31.9305245112373));
#31736=CARTESIAN_POINT('Ctrl Pts',(4.14647135042176,1.94526477434642,31.9569818079218));
#31737=CARTESIAN_POINT('Ctrl Pts',(3.72047219588784,2.56352263181406,31.9834391046062));
#31738=CARTESIAN_POINT('Ctrl Pts',(3.29447304135392,3.1817804892817,32.0098964012907));
#31739=CARTESIAN_POINT('Ctrl Pts',(2.71103200590467,3.69155592740269,32.0363536979752));
#31740=CARTESIAN_POINT('Ctrl Pts',(2.04121156194539,4.0307588619983,32.0628109946597));
#31741=CARTESIAN_POINT('Ctrl Pts',(1.37139111798607,4.36996179659393,32.0892682913441));
#31742=CARTESIAN_POINT('Ctrl Pts',(0.615191265516699,4.53859222766416,32.1157255880286));
#31743=CARTESIAN_POINT('Ctrl Pts',(-0.135283690341923,4.51611115533319,
32.1421828847131));
#31744=CARTESIAN_POINT('Ctrl Pts',(-0.885758646200546,4.49363008300222,
32.1686401813975));
#31745=CARTESIAN_POINT('Ctrl Pts',(-1.63050870544842,4.28003750727005,32.195097478082));
#31746=CARTESIAN_POINT('Ctrl Pts',(-2.27882413510731,3.9013487674713,32.2215547747665));
#31747=CARTESIAN_POINT('Ctrl Pts',(-2.92713956476612,3.52266002767259,32.2480120714509));
#31748=CARTESIAN_POINT('Ctrl Pts',(-3.47902036483595,2.97887512380733,32.2744693681354));
#31749=CARTESIAN_POINT('Ctrl Pts',(-3.86724806465204,2.33622645534256,32.3009266648198));
#31750=CARTESIAN_POINT('Ctrl Pts',(-4.25547576446814,1.69357778687776,32.3273839615043));
#31751=CARTESIAN_POINT('Ctrl Pts',(-4.48005036403047,0.952065353813438,
32.3538412581888));
#31752=CARTESIAN_POINT('Ctrl Pts',(-4.51361892565606,0.202004549841869,
32.3802985548733));
#31753=CARTESIAN_POINT('Ctrl Pts',(-4.54718748728165,-0.548056254129699,
32.4067558515577));
#31754=CARTESIAN_POINT('Ctrl Pts',(-4.38975001097049,-1.30666542900852,
32.4332131482422));
#31755=CARTESIAN_POINT('Ctrl Pts',(-4.06048220709632,-1.98142521687081,
32.4596704449267));
#31756=CARTESIAN_POINT('Ctrl Pts',(-3.73121440322213,-2.65618500473315,
32.4861277416111));
#31757=CARTESIAN_POINT('Ctrl Pts',(-3.23011627178491,-3.24709540557894,
32.5125850382956));
#31758=CARTESIAN_POINT('Ctrl Pts',(-2.61822101061276,-3.68218418656418,
32.5390423349801));
#31759=CARTESIAN_POINT('Ctrl Pts',(-2.00632574944065,-4.11727296754938,
32.5654996316645));
#31760=CARTESIAN_POINT('Ctrl Pts',(-1.28363335853361,-4.39654012867405,
32.591956928349));
#31761=CARTESIAN_POINT('Ctrl Pts',(-0.538166971277905,-4.48597123878686,
32.6184142250335));
#31762=CARTESIAN_POINT('Ctrl Pts',(0.207299415977802,-4.57540234889968,
32.6448715217179));
#31763=CARTESIAN_POINT('Ctrl Pts',(0.975539799582185,-4.47499740800066,
32.6713288184024));
#31764=CARTESIAN_POINT('Ctrl Pts',(1.67298335104786,-4.19698562677001,32.6977861150869));
#31765=CARTESIAN_POINT('Ctrl Pts',(2.37042690251357,-3.91897384553935,32.7242434117713));
#31766=CARTESIAN_POINT('Ctrl Pts',(2.99707362184056,-3.46335522397704,32.7507007084558));
#31767=CARTESIAN_POINT('Ctrl Pts',(3.47659863214429,-2.88562360594202,32.7771580051403));
#31768=CARTESIAN_POINT('Ctrl Pts',(3.95612364244802,-2.30789198790701,32.8036153018248));
#31769=CARTESIAN_POINT('Ctrl Pts',(4.28852694372849,-1.60804737339928,32.8300725985092));
#31770=CARTESIAN_POINT('Ctrl Pts',(4.43332218177084,-0.871330061926005,
32.8565298951937));
#31771=CARTESIAN_POINT('Ctrl Pts',(4.48966784634383,-0.584643655117203,
32.8668254959651));
#31772=CARTESIAN_POINT('Ctrl Pts',(4.51760398720758,-0.292373608988289,
32.8771210967366));
#31773=CARTESIAN_POINT('Ctrl Pts',(4.5174378855045,-7.22228901865168E-5,
32.887416697508));
#31774=CARTESIAN_POINT('Ctrl Pts',(4.51800690475437,8.25810157162321E-5,
32.6125833024919));
#31775=CARTESIAN_POINT('Ctrl Pts',(4.51744714361788,-0.663157072879468,
32.5892138422931));
#31776=CARTESIAN_POINT('Ctrl Pts',(4.36960026846028,-1.32663802677704,32.5658443820943));
#31777=CARTESIAN_POINT('Ctrl Pts',(4.08682159368458,-1.92651262793442,32.5424749218955));
#31778=CARTESIAN_POINT('Ctrl Pts',(3.76667901311444,-2.60564942276291,32.516017625211));
#31779=CARTESIAN_POINT('Ctrl Pts',(3.27359148233441,-3.20326060584664,32.4895603285266));
#31780=CARTESIAN_POINT('Ctrl Pts',(2.66761651687815,-3.64655779648099,32.4631030318421));
#31781=CARTESIAN_POINT('Ctrl Pts',(2.06164155142182,-4.08985498711538,32.4366457351576));
#31782=CARTESIAN_POINT('Ctrl Pts',(1.34277915128922,-4.37883818530036,32.4101884384731));
#31783=CARTESIAN_POINT('Ctrl Pts',(0.598585961229044,-4.47830955732371,
32.3837311417887));
#31784=CARTESIAN_POINT('Ctrl Pts',(-0.14560722883109,-4.57778092934705,
32.3572738451042));
#31785=CARTESIAN_POINT('Ctrl Pts',(-0.915131208818801,-4.4877404752088,
32.3308165484198));
#31786=CARTESIAN_POINT('Ctrl Pts',(-1.6162588096278,-4.2191550225724,32.3043592517353));
#31787=CARTESIAN_POINT('Ctrl Pts',(-2.31738641043684,-3.95056956993598,
32.2779019550508));
#31788=CARTESIAN_POINT('Ctrl Pts',(-2.95011763206717,-3.5034391188014,32.2514446583663));
#31789=CARTESIAN_POINT('Ctrl Pts',(-3.4373865119876,-2.93222366326361,32.2249873616819));
#31790=CARTESIAN_POINT('Ctrl Pts',(-3.924655391908,-2.36100820772586,32.1985300649974));
#31791=CARTESIAN_POINT('Ctrl Pts',(-4.26646193011853,-1.66570774778492,
32.172072768313));
#31792=CARTESIAN_POINT('Ctrl Pts',(-4.42117446855311,-0.931009109950869,
32.1456154716285));
#31793=CARTESIAN_POINT('Ctrl Pts',(-4.57588700698769,-0.196310472116814,
32.119158174944));
#31794=CARTESIAN_POINT('Ctrl Pts',(-4.54350554564632,0.577786343610359,
32.0927008782595));
#31795=CARTESIAN_POINT('Ctrl Pts',(-4.3279741106828,1.2969972017922,32.0662435815751));
#31796=CARTESIAN_POINT('Ctrl Pts',(-4.11244267571929,2.01620805997403,32.0397862848906));
#31797=CARTESIAN_POINT('Ctrl Pts',(-3.71376126713363,2.68053296061054,32.0133289882062));
#31798=CARTESIAN_POINT('Ctrl Pts',(-3.18048883925839,3.2090578660333,31.9868716915217));
#31799=CARTESIAN_POINT('Ctrl Pts',(-2.64721641138316,3.73758277145606,31.9604143948372));
#31800=CARTESIAN_POINT('Ctrl Pts',(-1.97935296421834,4.13030768166508,31.9339570981527));
#31801=CARTESIAN_POINT('Ctrl Pts',(-1.25824352648329,4.33939913723781,31.9074998014683));
#31802=CARTESIAN_POINT('Ctrl Pts',(-0.537134088748201,4.54849059281056,
31.8810425047838));
#31803=CARTESIAN_POINT('Ctrl Pts',(0.237221339557133,4.57394859374701,31.8545852080993));
#31804=CARTESIAN_POINT('Ctrl Pts',(0.970507124268449,4.41267238370826,31.8281279114149));
#31805=CARTESIAN_POINT('Ctrl Pts',(1.70379290897972,4.25139617366952,31.8016706147304));
#31806=CARTESIAN_POINT('Ctrl Pts',(2.39600905009698,3.90338575265561,31.7752133180459));
#31807=CARTESIAN_POINT('Ctrl Pts',(2.96284438772936,3.41102840479202,31.7487560213615));
#31808=CARTESIAN_POINT('Ctrl Pts',(3.52967972536174,2.91867105692843,31.722298724677));
#31809=CARTESIAN_POINT('Ctrl Pts',(3.97113425950925,2.28196678221515,31.6958414279925));
#31810=CARTESIAN_POINT('Ctrl Pts',(4.23343931648423,1.57846545665177,31.669384131308));
#31811=CARTESIAN_POINT('Ctrl Pts',(4.42115243039411,1.07501948430126,31.6504505217027));
#31812=CARTESIAN_POINT('Ctrl Pts',(4.5171186342718,0.537365078236716,31.6315169120973));
#31813=CARTESIAN_POINT('Ctrl Pts',(4.51762600826661,-0.000112987348963034,
31.612583302492));
#31814=CARTESIAN_POINT('Origin',(0.,0.,20.5));
#31815=CARTESIAN_POINT('',(4.5175628644093,0.000105298910395568,30.612583302492));
#31816=CARTESIAN_POINT('',(4.51784283093286,-0.000111697445491984,30.8874166975081));
#31817=CARTESIAN_POINT('',(4.51775,5.53264807684796E-16,20.5));
#31818=CARTESIAN_POINT('Ctrl Pts',(4.51784283093286,-0.000111697445491984,
30.8874166975081));
#31819=CARTESIAN_POINT('Ctrl Pts',(4.51722105684837,0.607182099716009,30.908812642976));
#31820=CARTESIAN_POINT('Ctrl Pts',(4.39393696701912,1.21472067967305,30.930208588444));
#31821=CARTESIAN_POINT('Ctrl Pts',(4.15564368858641,1.77318560159654,30.951604533912));
#31822=CARTESIAN_POINT('Ctrl Pts',(3.86098057239723,2.46375906325124,30.9780618305965));
#31823=CARTESIAN_POINT('Ctrl Pts',(3.3904601122214,3.07929536251675,31.0045191272809));
#31824=CARTESIAN_POINT('Ctrl Pts',(2.80139117936865,3.54482285937575,31.0309764239654));
#31825=CARTESIAN_POINT('Ctrl Pts',(2.21232224651588,4.01035035623478,31.0574337206499));
#31826=CARTESIAN_POINT('Ctrl Pts',(1.50470484098616,4.32586905068731,31.0838910173343));
#31827=CARTESIAN_POINT('Ctrl Pts',(0.764725979630773,4.45294911494339,31.1103483140188));
#31828=CARTESIAN_POINT('Ctrl Pts',(0.0247471182753856,4.58002917919947,
31.1368056107033));
#31829=CARTESIAN_POINT('Ctrl Pts',(-0.747593198905696,4.51867061325911,
31.1632629073878));
#31830=CARTESIAN_POINT('Ctrl Pts',(-1.45822477605293,4.27634682254641,31.1897202040722));
#31831=CARTESIAN_POINT('Ctrl Pts',(-2.16885635320013,4.03402303183372,31.2161775007567));
#31832=CARTESIAN_POINT('Ctrl Pts',(-2.81777919031341,3.61073401634878,31.2426347974411));
#31833=CARTESIAN_POINT('Ctrl Pts',(-3.32595520401574,3.05803590971036,31.2690920941256));
#31834=CARTESIAN_POINT('Ctrl Pts',(-3.83413121771806,2.50533780307193,31.2955493908101));
#31835=CARTESIAN_POINT('Ctrl Pts',(-4.20156040800938,1.82323060527995,31.3220066874946));
#31836=CARTESIAN_POINT('Ctrl Pts',(-4.38349030615745,1.09479421811638,31.348463984179));
#31837=CARTESIAN_POINT('Ctrl Pts',(-4.56542020430551,0.366357830952816,
31.3749212808635));
#31838=CARTESIAN_POINT('Ctrl Pts',(-4.56185081031042,-0.408407745582352,
31.4013785775479));
#31839=CARTESIAN_POINT('Ctrl Pts',(-4.3732168724104,-1.13513692172461,31.4278358742324));
#31840=CARTESIAN_POINT('Ctrl Pts',(-4.18458293451036,-1.86186609786691,
31.4542931709169));
#31841=CARTESIAN_POINT('Ctrl Pts',(-3.81088445270536,-2.54055887361621,
31.4807504676013));
#31842=CARTESIAN_POINT('Ctrl Pts',(-3.29763748849549,-3.08855122001668,
31.5072077642858));
#31843=CARTESIAN_POINT('Ctrl Pts',(-2.78439052428562,-3.63654356641715,
31.5336650609703));
#31844=CARTESIAN_POINT('Ctrl Pts',(-2.13159507767086,-4.05383548346882,
31.5601223576548));
#31845=CARTESIAN_POINT('Ctrl Pts',(-1.4187609115798,-4.28960127750478,31.5865796543392));
#31846=CARTESIAN_POINT('Ctrl Pts',(-0.705926745488817,-4.52536707154071,
31.6130369510237));
#31847=CARTESIAN_POINT('Ctrl Pts',(0.0669461400784679,-4.57960674256098,
31.6394942477081));
#31848=CARTESIAN_POINT('Ctrl Pts',(0.805722683022508,-4.44571395866405,
31.6659515443926));
#31849=CARTESIAN_POINT('Ctrl Pts',(1.54449922596663,-4.31182117476711,31.6924088410771));
#31850=CARTESIAN_POINT('Ctrl Pts',(2.24917942628753,-3.98979593595292,31.7188661377616));
#31851=CARTESIAN_POINT('Ctrl Pts',(2.83393401547767,-3.51886055991368,31.745323434446));
#31852=CARTESIAN_POINT('Ctrl Pts',(3.41868860466777,-3.04792518387447,31.7717807311305));
#31853=CARTESIAN_POINT('Ctrl Pts',(3.88351758272714,-2.42807967061021,31.798238027815));
#31854=CARTESIAN_POINT('Ctrl Pts',(4.1718052945689,-1.73482051763412,31.8246953244994));
#31855=CARTESIAN_POINT('Ctrl Pts',(4.39961643899369,-1.18699223867807,31.8456024488356));
#31856=CARTESIAN_POINT('Ctrl Pts',(4.51718638990429,-0.593320812476893,
31.8665095731718));
#31857=CARTESIAN_POINT('Ctrl Pts',(4.51779894817057,0.000115094980599771,
31.887416697508));
#31858=CARTESIAN_POINT('Ctrl Pts',(4.51762600826661,-0.000112987348963034,
31.612583302492));
#31859=CARTESIAN_POINT('Ctrl Pts',(4.51782762450612,-0.213691742886314,
31.6050596154129));
#31860=CARTESIAN_POINT('Ctrl Pts',(4.50295585827573,-0.42724265346175,31.5975359283338));
#31861=CARTESIAN_POINT('Ctrl Pts',(4.47277779830256,-0.638608182854815,
31.5900122412547));
#31862=CARTESIAN_POINT('Ctrl Pts',(4.36665564334343,-1.38188212038452,31.5635549445702));
#31863=CARTESIAN_POINT('Ctrl Pts',(4.07125575362272,-2.09813161903045,31.5370976478857));
#31864=CARTESIAN_POINT('Ctrl Pts',(3.62255750878013,-2.70011828255321,31.5106403512012));
#31865=CARTESIAN_POINT('Ctrl Pts',(3.17385926393751,-3.302104946076,31.4841830545168));
#31866=CARTESIAN_POINT('Ctrl Pts',(2.57186266397298,-3.78982877447561,31.4577257578323));
#31867=CARTESIAN_POINT('Ctrl Pts',(1.88989022851381,-4.10388554523215,31.4312684611479));
#31868=CARTESIAN_POINT('Ctrl Pts',(1.20791779305463,-4.4179423159887,31.4048111644634));
#31869=CARTESIAN_POINT('Ctrl Pts',(0.44596952210079,-4.55833202910217,31.3783538677789));
#31870=CARTESIAN_POINT('Ctrl Pts',(-0.303150128217454,-4.50795537288904,
31.3518965710945));
#31871=CARTESIAN_POINT('Ctrl Pts',(-1.05226977853561,-4.45757871667591,
31.32543927441));
#31872=CARTESIAN_POINT('Ctrl Pts',(-1.7885608082182,-4.2164356911362,31.2989819777255));
#31873=CARTESIAN_POINT('Ctrl Pts',(-2.42234378472615,-3.81389724990016,
31.272524681041));
#31874=CARTESIAN_POINT('Ctrl Pts',(-3.05612676123416,-3.41135880866406,
31.2460673843566));
#31875=CARTESIAN_POINT('Ctrl Pts',(-3.58740168456753,-2.84742495173157,
31.2196100876721));
#31876=CARTESIAN_POINT('Ctrl Pts',(-3.95145985704278,-2.19078219875388,
31.1931527909876));
#31877=CARTESIAN_POINT('Ctrl Pts',(-4.31551802951802,-1.53413944577618,
31.1666954943032));
#31878=CARTESIAN_POINT('Ctrl Pts',(-4.51235945113515,-0.784787796753247,
31.1402381976187));
#31879=CARTESIAN_POINT('Ctrl Pts',(-4.51800905459174,-0.0339974532052471,
31.1137809009342));
#31880=CARTESIAN_POINT('Ctrl Pts',(-4.52365865804833,0.716792890342667,
31.0873236042498));
#31881=CARTESIAN_POINT('Ctrl Pts',(-4.33811644334446,1.46902192841556,31.0608663075653));
#31882=CARTESIAN_POINT('Ctrl Pts',(-3.98398124688566,2.13106899669175,31.0344090108808));
#31883=CARTESIAN_POINT('Ctrl Pts',(-3.62984605042683,2.79311606496798,31.0079517141964));
#31884=CARTESIAN_POINT('Ctrl Pts',(-3.10711787221305,3.36498116344739,30.9814944175119));
#31885=CARTESIAN_POINT('Ctrl Pts',(-2.47946442583117,3.77701175603613,30.9550371208274));
#31886=CARTESIAN_POINT('Ctrl Pts',(-1.85181097944929,4.18904234862487,30.928579824143));
#31887=CARTESIAN_POINT('Ctrl Pts',(-1.11923226489916,4.44123843532298,30.9021225274585));
#31888=CARTESIAN_POINT('Ctrl Pts',(-0.370955558845505,4.50288281188385,
30.875665230774));
#31889=CARTESIAN_POINT('Ctrl Pts',(0.377321147208236,4.56452718844472,30.8492079340895));
#31890=CARTESIAN_POINT('Ctrl Pts',(1.14129584476551,4.43561985486838,30.8227506374051));
#31891=CARTESIAN_POINT('Ctrl Pts',(1.82791726117872,4.13186158171862,30.7962933407206));
#31892=CARTESIAN_POINT('Ctrl Pts',(2.51453867759182,3.82810330856891,30.7698360440361));
#31893=CARTESIAN_POINT('Ctrl Pts',(3.12380681286076,3.34949409584584,30.7433787473517));
#31894=CARTESIAN_POINT('Ctrl Pts',(3.58151348240585,2.75432801596732,30.7169214506672));
#31895=CARTESIAN_POINT('Ctrl Pts',(4.039220151951,2.15916193608874,30.6904641539828));
#31896=CARTESIAN_POINT('Ctrl Pts',(4.34536535577227,1.44743898905468,30.6640068572983));
#31897=CARTESIAN_POINT('Ctrl Pts',(4.4626609468647,0.705846242127884,30.6375495606138));
#31898=CARTESIAN_POINT('Ctrl Pts',(4.49955602397321,0.47257983095123,30.6292274745732));
#31899=CARTESIAN_POINT('Ctrl Pts',(4.5177662531821,0.236358091141789,30.6209053885326));
#31900=CARTESIAN_POINT('Ctrl Pts',(4.5175628644093,0.000105298910395568,
30.612583302492));
#31901=CARTESIAN_POINT('Origin',(0.,0.,20.5));
#31902=CARTESIAN_POINT('',(4.51806064718817,-6.4525231641549E-5,29.612583302492));
#31903=CARTESIAN_POINT('',(4.51741540695923,6.15435095971417E-5,29.887416697508));
#31904=CARTESIAN_POINT('',(4.51775,5.53264807684796E-16,20.5));
#31905=CARTESIAN_POINT('Ctrl Pts',(4.51741540695923,6.15435095971417E-5,
29.887416697508));
#31906=CARTESIAN_POINT('Ctrl Pts',(4.51756272899121,0.306245363704865,29.8982011194113));
#31907=CARTESIAN_POINT('Ctrl Pts',(4.48689091473443,0.612400072796405,29.9089855413145));
#31908=CARTESIAN_POINT('Ctrl Pts',(4.42510561599225,0.912141398858333,29.9197699632178));
#31909=CARTESIAN_POINT('Ctrl Pts',(4.27352846199847,1.64749330398352,29.9462272599022));
#31910=CARTESIAN_POINT('Ctrl Pts',(3.93469095105298,2.34424546963053,29.9726845565867));
#31911=CARTESIAN_POINT('Ctrl Pts',(3.44986311698689,2.91753425314097,29.9991418532711));
#31912=CARTESIAN_POINT('Ctrl Pts',(2.96503528292081,3.49082303665141,30.0255991499556));
#31913=CARTESIAN_POINT('Ctrl Pts',(2.33421712573414,3.94064843802526,30.0520564466401));
#31914=CARTESIAN_POINT('Ctrl Pts',(1.63424159882604,4.21222222121102,30.0785137433246));
#31915=CARTESIAN_POINT('Ctrl Pts',(0.934266071917943,4.48379600439678,30.104971040009));
#31916=CARTESIAN_POINT('Ctrl Pts',(0.165133175288441,4.57711816939443,30.1314283366935));
#31917=CARTESIAN_POINT('Ctrl Pts',(-0.579477555476409,4.48082217978983,
30.157885633378));
#31918=CARTESIAN_POINT('Ctrl Pts',(-1.32408828624126,4.38452619018523,30.1843429300624));
#31919=CARTESIAN_POINT('Ctrl Pts',(-2.04417685114143,4.09861204597837,30.2108002267469));
#31920=CARTESIAN_POINT('Ctrl Pts',(-2.65203725991661,3.65790377350353,30.2372575234314));
#31921=CARTESIAN_POINT('Ctrl Pts',(-3.2598976686918,3.21719550102869,30.2637148201158));
#31922=CARTESIAN_POINT('Ctrl Pts',(-3.75552992134198,2.62169310028588,30.2901721168003));
#31923=CARTESIAN_POINT('Ctrl Pts',(-4.07856655802606,1.94392810462446,30.3166294134847));
#31924=CARTESIAN_POINT('Ctrl Pts',(-4.40160319471017,1.26616310896299,30.3430867101692));
#31925=CARTESIAN_POINT('Ctrl Pts',(-4.55204421542814,0.506135518382923,
30.3695440068537));
#31926=CARTESIAN_POINT('Ctrl Pts',(-4.51156607035432,-0.243584147729374,
30.3960013035382));
#31927=CARTESIAN_POINT('Ctrl Pts',(-4.47108792528051,-0.993303813841587,
30.4224586002227));
#31928=CARTESIAN_POINT('Ctrl Pts',(-4.2396906144149,-1.73271555548614,30.4489158969071));
#31929=CARTESIAN_POINT('Ctrl Pts',(-3.84555807412635,-2.37175984086058,
30.4753731935916));
#31930=CARTESIAN_POINT('Ctrl Pts',(-3.45142553383776,-3.01080412623509,
30.501830490276));
#31931=CARTESIAN_POINT('Ctrl Pts',(-2.89455776412619,-3.54948095533957,
30.5282877869605));
#31932=CARTESIAN_POINT('Ctrl Pts',(-2.24278064303953,-3.92218008655959,
30.554745083645));
#31933=CARTESIAN_POINT('Ctrl Pts',(-1.59100352195292,-4.29487921777957,
30.5812023803295));
#31934=CARTESIAN_POINT('Ctrl Pts',(-0.844317049491253,-4.5016006511151,
30.6076596770139));
#31935=CARTESIAN_POINT('Ctrl Pts',(-0.0936668116191134,-4.51716594477096,
30.6341169736984));
#31936=CARTESIAN_POINT('Ctrl Pts',(0.656983426253069,-4.53273123842682,
30.6605742703828));
#31937=CARTESIAN_POINT('Ctrl Pts',(1.4115974295357,-4.35714039240299,30.6870315670673));
#31938=CARTESIAN_POINT('Ctrl Pts',(2.07826404778386,-4.01178017741331,30.7134888637518));
#31939=CARTESIAN_POINT('Ctrl Pts',(2.74493066603195,-3.66641996242367,30.7399461604362));
#31940=CARTESIAN_POINT('Ctrl Pts',(3.32364989924556,-3.15129037846822,30.7664034571207));
#31941=CARTESIAN_POINT('Ctrl Pts',(3.74393438530595,-2.52913363876272,30.7928607538052));
#31942=CARTESIAN_POINT('Ctrl Pts',(4.16421887136636,-1.90697689905718,30.8193180504897));
#31943=CARTESIAN_POINT('Ctrl Pts',(4.42606861027353,-1.17779300360159,30.8457753471741));
#31944=CARTESIAN_POINT('Ctrl Pts',(4.49759059362584,-0.430395743851834,
30.8722326438586));
#31945=CARTESIAN_POINT('Ctrl Pts',(4.51127293924728,-0.287416660427361,
30.8772939950751));
#31946=CARTESIAN_POINT('Ctrl Pts',(4.51798991567019,-0.143771027837287,
30.8823553462916));
#31947=CARTESIAN_POINT('Ctrl Pts',(4.51784283093286,-0.000111697445491984,
30.8874166975081));
#31948=CARTESIAN_POINT('Ctrl Pts',(4.5175628644093,0.000105298910395568,
30.612583302492));
#31949=CARTESIAN_POINT('Ctrl Pts',(4.51711964642055,-0.514728858223211,
30.5944480918481));
#31950=CARTESIAN_POINT('Ctrl Pts',(4.42923445822943,-1.02971047605454,30.5763128812042));
#31951=CARTESIAN_POINT('Ctrl Pts',(4.25671408259971,-1.51457811392965,30.5581776705604));
#31952=CARTESIAN_POINT('Ctrl Pts',(4.00502564887872,-2.22194717624094,30.5317203738759));
#31953=CARTESIAN_POINT('Ctrl Pts',(3.57320280307314,-2.86522275404404,30.5052630771915));
#31954=CARTESIAN_POINT('Ctrl Pts',(3.01384108989026,-3.36605459389572,30.478805780507));
#31955=CARTESIAN_POINT('Ctrl Pts',(2.45447937670739,-3.86688643374739,30.4523484838226));
#31956=CARTESIAN_POINT('Ctrl Pts',(1.7675787961471,-4.22527453564767,30.425891187138));
#31957=CARTESIAN_POINT('Ctrl Pts',(1.03680307870754,-4.3975676254243,30.3994338904536));
#31958=CARTESIAN_POINT('Ctrl Pts',(0.306027361267937,-4.56986071520095,
30.3729765937691));
#31959=CARTESIAN_POINT('Ctrl Pts',(-0.468623493050924,-4.55605879285401,
30.3465192970847));
#31960=CARTESIAN_POINT('Ctrl Pts',(-1.19279786752355,-4.35784291725031,
30.3200620004002));
#31961=CARTESIAN_POINT('Ctrl Pts',(-1.91697224199613,-4.15962704164662,
30.2936047037158));
#31962=CARTESIAN_POINT('Ctrl Pts',(-2.59067013662245,-3.77699721278612,
30.2671474070313));
#31963=CARTESIAN_POINT('Ctrl Pts',(-3.1318358934393,-3.25655732035575,30.2406901103468));
#31964=CARTESIAN_POINT('Ctrl Pts',(-3.67300165025612,-2.73611742792542,
30.2142328136623));
#31965=CARTESIAN_POINT('Ctrl Pts',(-4.08163526926355,-2.0778674719253,30.1877755169779));
#31966=CARTESIAN_POINT('Ctrl Pts',(-4.30796562791422,-1.3619815684902,30.1613182202934));
#31967=CARTESIAN_POINT('Ctrl Pts',(-4.5342959865649,-0.64609566505506,30.1348609236089));
#31968=CARTESIAN_POINT('Ctrl Pts',(-4.5783230848587,0.127426185815075,30.1084036269244));
#31969=CARTESIAN_POINT('Ctrl Pts',(-4.4346844709496,0.864369878764792,30.08194633024));
#31970=CARTESIAN_POINT('Ctrl Pts',(-4.29104585704049,1.60131357171455,30.0554890335555));
#31971=CARTESIAN_POINT('Ctrl Pts',(-3.95974153092847,2.30167910674398,30.029031736871));
#31972=CARTESIAN_POINT('Ctrl Pts',(-3.48112399286914,2.88016273680294,30.0025744401866));
#31973=CARTESIAN_POINT('Ctrl Pts',(-3.00250645480984,3.45864636686186,29.9761171435021));
#31974=CARTESIAN_POINT('Ctrl Pts',(-2.37657570480325,3.91524809195029,29.9496598468177));
#31975=CARTESIAN_POINT('Ctrl Pts',(-1.67956941546306,4.19435432728787,29.9232025501332));
#31976=CARTESIAN_POINT('Ctrl Pts',(-0.982563126122875,4.47346056262544,
29.8967452534487));
#31977=CARTESIAN_POINT('Ctrl Pts',(-0.214481297449103,4.57507130821215,
29.8702879567642));
#31978=CARTESIAN_POINT('Ctrl Pts',(0.53112455388596,4.48681048769132,29.8438306600798));
#31979=CARTESIAN_POINT('Ctrl Pts',(1.27673040522102,4.39854966717049,29.8173733633953));
#31980=CARTESIAN_POINT('Ctrl Pts',(1.99986027921735,4.12041728054213,29.7909160667108));
#31981=CARTESIAN_POINT('Ctrl Pts',(2.61243775753263,3.68628954467976,29.7644587700264));
#31982=CARTESIAN_POINT('Ctrl Pts',(3.22501523584791,3.25216180881739,29.7380014733419));
#31983=CARTESIAN_POINT('Ctrl Pts',(3.72704031848211,2.66203872372102,29.7115441766574));
#31984=CARTESIAN_POINT('Ctrl Pts',(4.05736690597726,1.98779662804773,29.685086879973));
#31985=CARTESIAN_POINT('Ctrl Pts',(4.35910923962182,1.37189893439675,29.6609190208126));
#31986=CARTESIAN_POINT('Ctrl Pts',(4.51758267646005,0.685810539097339,29.6367511616523));
#31987=CARTESIAN_POINT('Ctrl Pts',(4.51806064718817,-6.4525231641549E-5,
29.612583302492));
#31988=CARTESIAN_POINT('Origin',(0.,0.,20.5));
#31989=CARTESIAN_POINT('',(4.51736349586412,-8.67285085925565E-6,28.612583302492));
#31990=CARTESIAN_POINT('',(4.51813672578305,5.21363961469835E-6,28.8874166975081));
#31991=CARTESIAN_POINT('',(4.51775,5.53264807684796E-16,20.5));
#31992=CARTESIAN_POINT('Ctrl Pts',(4.51813645424719,5.20997890686523E-6,
28.8874166975081));
#31993=CARTESIAN_POINT('Ctrl Pts',(4.51813678764949,0.00491176269805106,
28.8875895958466));
#31994=CARTESIAN_POINT('Ctrl Pts',(4.51812896220818,0.00981831434884656,
28.887762494185));
#31995=CARTESIAN_POINT('Ctrl Pts',(4.51811297150728,0.0147248393885022,
28.8879353925235));
#31996=CARTESIAN_POINT('Ctrl Pts',(4.51566603811481,0.7655324515643,28.914392689208));
#31997=CARTESIAN_POINT('Ctrl Pts',(4.32202288903541,1.51571694218793,28.9408499858924));
#31998=CARTESIAN_POINT('Ctrl Pts',(3.96076904551605,2.17390667055403,28.9673072825769));
#31999=CARTESIAN_POINT('Ctrl Pts',(3.59951520199672,2.83209639892005,28.9937645792614));
#32000=CARTESIAN_POINT('Ctrl Pts',(3.07065066403746,3.39829136502856,29.0202218759458));
#32001=CARTESIAN_POINT('Ctrl Pts',(2.43859054705081,3.8035296486332,29.0466791726303));
#32002=CARTESIAN_POINT('Ctrl Pts',(1.80653043006408,4.20876793223789,29.0731364693148));
#32003=CARTESIAN_POINT('Ctrl Pts',(1.07127473404993,4.45304953333867,29.0995937659992));
#32004=CARTESIAN_POINT('Ctrl Pts',(0.32237678905244,4.50662122327555,29.1260510626837));
#32005=CARTESIAN_POINT('Ctrl Pts',(-0.426521155945046,4.56019291321243,
29.1525083593682));
#32006=CARTESIAN_POINT('Ctrl Pts',(-1.18906134992587,4.42305469198539,29.1789656560527));
#32007=CARTESIAN_POINT('Ctrl Pts',(-1.87236724119019,4.11190984316476,29.2054229527371));
#32008=CARTESIAN_POINT('Ctrl Pts',(-2.55567313245444,3.80076499434415,29.2318802494216));
#32009=CARTESIAN_POINT('Ctrl Pts',(-3.15974472100221,3.31561351792999,29.258337546106));
#32010=CARTESIAN_POINT('Ctrl Pts',(-3.61100675589329,2.7155463268172,29.2847948427905));
#32011=CARTESIAN_POINT('Ctrl Pts',(-4.06226879078437,2.11547913570442,29.311252139475));
#32012=CARTESIAN_POINT('Ctrl Pts',(-4.36072127201875,1.40049622989302,29.3377094361595));
#32013=CARTESIAN_POINT('Ctrl Pts',(-4.47001301768878,0.657681736016911,
29.3641667328439));
#32014=CARTESIAN_POINT('Ctrl Pts',(-4.57930476335883,-0.0851327578592831,
29.3906240295284));
#32015=CARTESIAN_POINT('Ctrl Pts',(-4.49943577346447,-0.855778839800193,
29.4170813262128));
#32016=CARTESIAN_POINT('Ctrl Pts',(-4.24013400258134,-1.56039266992349,
29.4435386228973));
#32017=CARTESIAN_POINT('Ctrl Pts',(-3.98083223169821,-2.26500650004679,
29.4699959195818));
#32018=CARTESIAN_POINT('Ctrl Pts',(-3.54209767982631,-2.90358807835248,
29.4964532162663));
#32019=CARTESIAN_POINT('Ctrl Pts',(-2.97736772982241,-3.39835887534109,
29.5229105129507));
#32020=CARTESIAN_POINT('Ctrl Pts',(-2.41263777981851,-3.8931296723297,29.5493678096352));
#32021=CARTESIAN_POINT('Ctrl Pts',(-1.72191243168261,-4.24408968800123,
29.5758251063197));
#32022=CARTESIAN_POINT('Ctrl Pts',(-0.989321268370363,-4.40849238086531,
29.6022824030041));
#32023=CARTESIAN_POINT('Ctrl Pts',(-0.256730105058199,-4.57289507372936,
29.6287396996886));
#32024=CARTESIAN_POINT('Ctrl Pts',(0.517726873430306,-4.55074044378599,
29.655196996373));
#32025=CARTESIAN_POINT('Ctrl Pts',(1.23972166423099,-4.34472690044308,29.6816542930575));
#32026=CARTESIAN_POINT('Ctrl Pts',(1.96171645503171,-4.13871335710016,29.708111589742));
#32027=CARTESIAN_POINT('Ctrl Pts',(2.63124905814461,-3.74884090035768,29.7345688864265));
#32028=CARTESIAN_POINT('Ctrl Pts',(3.16677114350317,-3.22259556396285,29.761026183111));
#32029=CARTESIAN_POINT('Ctrl Pts',(3.70229322886173,-2.69635022756802,29.7874834797954));
#32030=CARTESIAN_POINT('Ctrl Pts',(4.10380479646594,-2.03373201152084,29.8139407764799));
#32031=CARTESIAN_POINT('Ctrl Pts',(4.32240218174702,-1.31544708119558,29.8403980731643));
#32032=CARTESIAN_POINT('Ctrl Pts',(4.45189573839702,-0.889946702056473,
29.8560709479456));
#32033=CARTESIAN_POINT('Ctrl Pts',(4.51720130556553,-0.444911837263118,
29.8717438227268));
#32034=CARTESIAN_POINT('Ctrl Pts',(4.51741540695923,6.15435095971417E-5,
29.887416697508));
#32035=CARTESIAN_POINT('Ctrl Pts',(4.51806064718817,-6.4525231641549E-5,
29.612583302492));
#32036=CARTESIAN_POINT('Ctrl Pts',(4.51810592567614,-0.065037930559881,
29.6102938649678));
#32037=CARTESIAN_POINT('Ctrl Pts',(4.51673336863491,-0.130009421477303,
29.6080044274437));
#32038=CARTESIAN_POINT('Ctrl Pts',(4.51393045695516,-0.194919147263631,
29.6057149899196));
#32039=CARTESIAN_POINT('Ctrl Pts',(4.48153932808183,-0.945031720651385,
29.5792576932351));
#32040=CARTESIAN_POINT('Ctrl Pts',(4.25812897797913,-1.68689576117669,29.5528003965506));
#32041=CARTESIAN_POINT('Ctrl Pts',(3.87091054003435,-2.33015304974767,29.5263430998662));
#32042=CARTESIAN_POINT('Ctrl Pts',(3.48369210208957,-2.97341033831866,29.4998858031817));
#32043=CARTESIAN_POINT('Ctrl Pts',(2.9326655763027,-3.51806087493531,29.4734285064972));
#32044=CARTESIAN_POINT('Ctrl Pts',(2.28494538367634,-3.89776682701949,29.4469712098128));
#32045=CARTESIAN_POINT('Ctrl Pts',(1.63722519105001,-4.27747277910364,29.4205139131283));
#32046=CARTESIAN_POINT('Ctrl Pts',(0.892811331584192,-4.49223414665534,
29.3940566164438));
#32047=CARTESIAN_POINT('Ctrl Pts',(0.142372589495739,-4.5158932327899,29.3675993197594));
#32048=CARTESIAN_POINT('Ctrl Pts',(-0.608066152592799,-4.53955231892447,
29.3411420230749));
#32049=CARTESIAN_POINT('Ctrl Pts',(-1.36452977730397,-4.37210912364185,
29.3146847263904));
#32050=CARTESIAN_POINT('Ctrl Pts',(-2.03488185234987,-4.03395804281286,
29.288227429706));
#32051=CARTESIAN_POINT('Ctrl Pts',(-2.70523392739576,-3.69580696198387,
29.2617701330215));
#32052=CARTESIAN_POINT('Ctrl Pts',(-3.28947445277638,-3.18694799560851,
29.235312836337));
#32053=CARTESIAN_POINT('Ctrl Pts',(-3.71644357909758,-2.56935960262119,
29.2088555396525));
#32054=CARTESIAN_POINT('Ctrl Pts',(-4.14341270541876,-1.95177120963391,
29.1823982429681));
#32055=CARTESIAN_POINT('Ctrl Pts',(-4.41311043268056,-1.22545339003468,
29.1559409462836));
#32056=CARTESIAN_POINT('Ctrl Pts',(-4.49268787618537,-0.478870850412086,
29.1294836495992));
#32057=CARTESIAN_POINT('Ctrl Pts',(-4.57226531969018,0.267711689210511,
29.1030263529147));
#32058=CARTESIAN_POINT('Ctrl Pts',(-4.46172247943801,1.03455894885648,29.0765690562302));
#32059=CARTESIAN_POINT('Ctrl Pts',(-4.17452335103036,1.72826978099475,29.0501117595457));
#32060=CARTESIAN_POINT('Ctrl Pts',(-3.88732422262269,2.42198061313306,29.0236544628612));
#32061=CARTESIAN_POINT('Ctrl Pts',(-3.42346880605953,3.04255501776367,28.9971971661768));
#32062=CARTESIAN_POINT('Ctrl Pts',(-2.83945417771499,3.51440771921163,28.9707398694923));
#32063=CARTESIAN_POINT('Ctrl Pts',(-2.25543954937045,3.98626042065959,28.9442825728079));
#32064=CARTESIAN_POINT('Ctrl Pts',(-1.55126570924453,4.3093914189249,28.9178252761234));
#32065=CARTESIAN_POINT('Ctrl Pts',(-0.812700251733401,4.44444371603802,
28.8913679794389));
#32066=CARTESIAN_POINT('Ctrl Pts',(-0.0741347942223568,4.57949601315112,
28.8649106827545));
#32067=CARTESIAN_POINT('Ctrl Pts',(0.698822280673891,4.52646960911207,28.83845338607));
#32068=CARTESIAN_POINT('Ctrl Pts',(1.41202565668872,4.29182306124684,28.8119960893855));
#32069=CARTESIAN_POINT('Ctrl Pts',(2.12522903270359,4.05717651338159,28.785538792701));
#32070=CARTESIAN_POINT('Ctrl Pts',(2.77867870983704,3.64090982169015,28.7590814960166));
#32071=CARTESIAN_POINT('Ctrl Pts',(3.29278524060738,3.09372380852518,28.7326241993321));
#32072=CARTESIAN_POINT('Ctrl Pts',(3.80689177137772,2.54653779536021,28.7061669026477));
#32073=CARTESIAN_POINT('Ctrl Pts',(4.18165515578495,1.86843246072172,28.6797096059632));
#32074=CARTESIAN_POINT('Ctrl Pts',(4.37142962837061,1.14200028388831,28.6532523092787));
#32075=CARTESIAN_POINT('Ctrl Pts',(4.46866731930057,0.769786958618117,28.6396959736831));
#32076=CARTESIAN_POINT('Ctrl Pts',(4.517338221792,0.384885956569512,28.6261396380875));
#32077=CARTESIAN_POINT('Ctrl Pts',(4.51736392670147,-8.66318320566495E-6,
28.612583302492));
#32078=CARTESIAN_POINT('Origin',(0.,0.,20.5));
#32079=CARTESIAN_POINT('',(4.51801726226543,7.95831363512023E-5,27.612583302492));
#32080=CARTESIAN_POINT('',(4.51743092439869,-6.91819792334251E-5,27.8874166975081));
#32081=CARTESIAN_POINT('',(4.51775,5.53264807684796E-16,20.5));
#32082=CARTESIAN_POINT('Ctrl Pts',(4.51743092439869,-6.91819792334251E-5,
27.8874166975081));
#32083=CARTESIAN_POINT('Ctrl Pts',(4.51718386244179,0.454717345983238,27.9034353689663));
#32084=CARTESIAN_POINT('Ctrl Pts',(4.44891863177309,0.909576397762494,27.9194540404245));
#32085=CARTESIAN_POINT('Ctrl Pts',(4.31373618863887,1.34359284719174,27.9354727118827));
#32086=CARTESIAN_POINT('Ctrl Pts',(4.09046161721975,2.06043768656892,27.9619300085671));
#32087=CARTESIAN_POINT('Ctrl Pts',(3.68463958850139,2.72042474717273,27.9883873052516));
#32088=CARTESIAN_POINT('Ctrl Pts',(3.14569877644576,3.24316833544992,28.0148446019361));
#32089=CARTESIAN_POINT('Ctrl Pts',(2.60675796439011,3.76591192372714,28.0413018986205));
#32090=CARTESIAN_POINT('Ctrl Pts',(1.93469836899718,4.15141203967772,28.067759195305));
#32091=CARTESIAN_POINT('Ctrl Pts',(1.21137610519651,4.3527151958239,28.0942164919895));
#32092=CARTESIAN_POINT('Ctrl Pts',(0.48805384139591,4.55401835197006,28.1206737886739));
#32093=CARTESIAN_POINT('Ctrl Pts',(-0.286531090812426,4.57112454831186,
28.1471310853584));
#32094=CARTESIAN_POINT('Ctrl Pts',(-1.01803510394287,4.40195026906682,28.1735883820429));
#32095=CARTESIAN_POINT('Ctrl Pts',(-1.7495391170734,4.23277598982176,28.2000456787273));
#32096=CARTESIAN_POINT('Ctrl Pts',(-2.43796221112602,3.87732123498983,28.2265029754118));
#32097=CARTESIAN_POINT('Ctrl Pts',(-2.99945521514446,3.37888000031668,28.2529602720963));
#32098=CARTESIAN_POINT('Ctrl Pts',(-3.56094821916288,2.88043876564355,28.2794175687807));
#32099=CARTESIAN_POINT('Ctrl Pts',(-3.99551113314713,2.23901105112923,28.3058748654652));
#32100=CARTESIAN_POINT('Ctrl Pts',(-4.25021467511827,1.53272204251347,28.3323321621497));
#32101=CARTESIAN_POINT('Ctrl Pts',(-4.50491821708942,0.826433033897707,
28.3587894588341));
#32102=CARTESIAN_POINT('Ctrl Pts',(-4.57976238704747,0.0552827311804979,
28.3852467555186));
#32103=CARTESIAN_POINT('Ctrl Pts',(-4.4656312479239,-0.686803612223317,
28.4117040522031));
#32104=CARTESIAN_POINT('Ctrl Pts',(-4.35150010880033,-1.42888995562718,
28.4381613488875));
#32105=CARTESIAN_POINT('Ctrl Pts',(-4.04839366059513,-2.14191233971764,
28.464618645572));
#32106=CARTESIAN_POINT('Ctrl Pts',(-3.59322993324233,-2.73902542723662,
28.4910759422565));
#32107=CARTESIAN_POINT('Ctrl Pts',(-3.13806620588952,-3.3361385147556,28.517533238941));
#32108=CARTESIAN_POINT('Ctrl Pts',(-2.5308451993891,-3.8173423057031,28.5439905356254));
#32109=CARTESIAN_POINT('Ctrl Pts',(-1.84552576030239,-4.12402671090497,
28.5704478323099));
#32110=CARTESIAN_POINT('Ctrl Pts',(-1.16020632121576,-4.4307111161068,28.5969051289944));
#32111=CARTESIAN_POINT('Ctrl Pts',(-0.396788449542842,-4.56287613556305,
28.6233624256788));
#32112=CARTESIAN_POINT('Ctrl Pts',(0.351744402845005,-4.50442421617509,
28.6498197223633));
#32113=CARTESIAN_POINT('Ctrl Pts',(1.10027725523294,-4.44597229678712,28.6762770190477));
#32114=CARTESIAN_POINT('Ctrl Pts',(1.8339250883358,-4.19690343855492,28.7027343157322));
#32115=CARTESIAN_POINT('Ctrl Pts',(2.46333040803262,-3.78755395275886,28.7291916124167));
#32116=CARTESIAN_POINT('Ctrl Pts',(3.09273572772936,-3.37820446696285,28.7556489091012));
#32117=CARTESIAN_POINT('Ctrl Pts',(3.61789853402009,-2.80857435360303,28.7821062057856));
#32118=CARTESIAN_POINT('Ctrl Pts',(3.97485457831268,-2.14804393005918,28.8085635024701));
#32119=CARTESIAN_POINT('Ctrl Pts',(4.32947791614233,-1.49183007045257,28.8348479008161));
#32120=CARTESIAN_POINT('Ctrl Pts',(4.51808576967277,-0.745900085055985,
28.8611322991621));
#32121=CARTESIAN_POINT('Ctrl Pts',(4.51813645424719,5.20997890686523E-6,
28.8874166975081));
#32122=CARTESIAN_POINT('Ctrl Pts',(4.51736392670147,-8.66318320566495E-6,
28.612583302492));
#32123=CARTESIAN_POINT('Ctrl Pts',(4.5173883889195,-0.366295738162854,28.5996823414031));
#32124=CARTESIAN_POINT('Ctrl Pts',(4.47335741760473,-0.732577033027994,
28.5867813803142));
#32125=CARTESIAN_POINT('Ctrl Pts',(4.38520343465814,-1.08791198212899,28.5738804192253));
#32126=CARTESIAN_POINT('Ctrl Pts',(4.20441720759592,-1.81663305228457,28.5474231225409));
#32127=CARTESIAN_POINT('Ctrl Pts',(3.8380591927074,-2.49931617356742,28.5209658258564));
#32128=CARTESIAN_POINT('Ctrl Pts',(3.33075139074614,-3.05281129735201,28.4945085291719));
#32129=CARTESIAN_POINT('Ctrl Pts',(2.82344358878484,-3.60630642113663,28.4680512324875));
#32130=CARTESIAN_POINT('Ctrl Pts',(2.17518599975079,-4.03061354742298,28.441593935803));
#32131=CARTESIAN_POINT('Ctrl Pts',(1.46493568054142,-4.27405253782332,28.4151366391185));
#32132=CARTESIAN_POINT('Ctrl Pts',(0.754685361332094,-4.51749152822365,
28.388679342434));
#32133=CARTESIAN_POINT('Ctrl Pts',(-0.0175576880525484,-4.580062382738,
28.3622220457496));
#32134=CARTESIAN_POINT('Ctrl Pts',(-0.757735118862955,-4.45414404053564,
28.3357647490651));
#32135=CARTESIAN_POINT('Ctrl Pts',(-1.49791254967336,-4.32822569833327,
28.3093074523807));
#32136=CARTESIAN_POINT('Ctrl Pts',(-2.20602436190953,-4.01381815941419,
28.2828501556962));
#32137=CARTESIAN_POINT('Ctrl Pts',(-2.79582332053056,-3.54921591405409,
28.2563928590117));
#32138=CARTESIAN_POINT('Ctrl Pts',(-3.38562227915162,-3.08461366869397,
28.2299355623272));
#32139=CARTESIAN_POINT('Ctrl Pts',(-3.85710838415752,-2.46981671689283,
28.2034782656428));
#32140=CARTESIAN_POINT('Ctrl Pts',(-4.15285514976694,-1.77970664696505,
28.1770209689583));
#32141=CARTESIAN_POINT('Ctrl Pts',(-4.44860191537634,-1.08959657703732,
28.1505636722738));
#32142=CARTESIAN_POINT('Ctrl Pts',(-4.56860934158928,-0.32417338898296,
28.1241063755894));
#32143=CARTESIAN_POINT('Ctrl Pts',(-4.49826065670898,0.423335220010742,
28.0976490789049));
#32144=CARTESIAN_POINT('Ctrl Pts',(-4.42791197182868,1.17084382900444,28.0711917822204));
#32145=CARTESIAN_POINT('Ctrl Pts',(-4.16720717585513,1.90043785893749,28.0447344855359));
#32146=CARTESIAN_POINT('Ctrl Pts',(-3.7478998244078,2.52325356442854,28.0182771888515));
#32147=CARTESIAN_POINT('Ctrl Pts',(-3.32859247296047,3.14606926991958,27.991819892167));
#32148=CARTESIAN_POINT('Ctrl Pts',(-2.75068256603934,3.66210665096863,27.9653625954826));
#32149=CARTESIAN_POINT('Ctrl Pts',(-2.08455889071647,4.00851292567859,27.9389052987981));
#32150=CARTESIAN_POINT('Ctrl Pts',(-1.41843521539359,4.35491920038855,27.9124480021136));
#32151=CARTESIAN_POINT('Ctrl Pts',(-0.664097771668966,4.53169436875941,
27.8859907054291));
#32152=CARTESIAN_POINT('Ctrl Pts',(0.0865759746605513,4.51730741092622,
27.8595334087447));
#32153=CARTESIAN_POINT('Ctrl Pts',(0.837249720990026,4.50292045309303,27.8330761120602));
#32154=CARTESIAN_POINT('Ctrl Pts',(1.58425976992439,4.2973713690558,27.8066188153758));
#32155=CARTESIAN_POINT('Ctrl Pts',(2.23662112424281,3.92569580976267,27.7801615186913));
#32156=CARTESIAN_POINT('Ctrl Pts',(2.88898247856131,3.5540202504695,27.7537042220068));
#32157=CARTESIAN_POINT('Ctrl Pts',(3.44669513826383,3.0162182159204,27.7272469253223));
#32158=CARTESIAN_POINT('Ctrl Pts',(3.84183031863663,2.37779339872113,27.7007896286379));
#32159=CARTESIAN_POINT('Ctrl Pts',(4.23696549900942,1.73936858152187,27.6743323319534));
#32160=CARTESIAN_POINT('Ctrl Pts',(4.46952320005248,1.00032098167245,27.647875035269));
#32161=CARTESIAN_POINT('Ctrl Pts',(4.51117815115764,0.250665778907488,27.6214177385845));
#32162=CARTESIAN_POINT('Ctrl Pts',(4.51581452813225,0.167225898922454,27.6184729265537));
#32163=CARTESIAN_POINT('Ctrl Pts',(4.51808587645197,0.0836546049852204,
27.6155281145228));
#32164=CARTESIAN_POINT('Ctrl Pts',(4.51801726226543,7.95831363512023E-5,
27.612583302492));
#32165=CARTESIAN_POINT('Origin',(0.,0.,20.5));
#32166=CARTESIAN_POINT('',(4.51761428595877,-0.000111883206665997,26.612583302492));
#32167=CARTESIAN_POINT('',(4.51781182322151,0.000114263439177032,26.8874166975081));
#32168=CARTESIAN_POINT('',(4.51775,5.53264807684796E-16,20.5));
#32169=CARTESIAN_POINT('Ctrl Pts',(4.51781182322151,0.000114263439177032,
26.8874166975081));
#32170=CARTESIAN_POINT('Ctrl Pts',(4.51797007849026,0.153591581624792,26.8928238454015));
#32171=CARTESIAN_POINT('Ctrl Pts',(4.51030214935632,0.307053160819986,26.898230993295));
#32172=CARTESIAN_POINT('Ctrl Pts',(4.49468970350708,0.459702200761322,26.9036381411884));
#32173=CARTESIAN_POINT('Ctrl Pts',(4.41829765358665,1.20661739855353,26.9300954378729));
#32174=CARTESIAN_POINT('Ctrl Pts',(4.1517006071518,1.93407904976938,26.9565527345573));
#32175=CARTESIAN_POINT('Ctrl Pts',(3.727369789407,2.55348313039531,26.9830100312418));
#32176=CARTESIAN_POINT('Ctrl Pts',(3.30303897166215,3.17288721102131,27.0094673279263));
#32177=CARTESIAN_POINT('Ctrl Pts',(2.72097438260733,3.68423372105737,27.0359246246107));
#32178=CARTESIAN_POINT('Ctrl Pts',(2.05207084500035,4.02524122150424,27.0623819212952));
#32179=CARTESIAN_POINT('Ctrl Pts',(1.38316730739341,4.36624872195109,27.0888392179797));
#32180=CARTESIAN_POINT('Ctrl Pts',(0.627424821234327,4.53691721280878,27.1152965146642));
#32181=CARTESIAN_POINT('Ctrl Pts',(-0.123108015066531,4.51645946077497,
27.1417538113486));
#32182=CARTESIAN_POINT('Ctrl Pts',(-0.873640851367389,4.49600170874117,
27.1682111080331));
#32183=CARTESIAN_POINT('Ctrl Pts',(-1.61896403781002,4.28441771381588,27.1946684047176));
#32184=CARTESIAN_POINT('Ctrl Pts',(-2.26829803515817,3.9074781724144,27.221125701402));
#32185=CARTESIAN_POINT('Ctrl Pts',(-2.91763203250632,3.53053863101291,27.2475829980865));
#32186=CARTESIAN_POINT('Ctrl Pts',(-3.47097684075998,2.98824354313522,27.274040294771));
#32187=CARTESIAN_POINT('Ctrl Pts',(-3.86093567467783,2.34664385030993,27.3004975914554));
#32188=CARTESIAN_POINT('Ctrl Pts',(-4.25089450859569,1.70504415748464,27.3269548881399));
#32189=CARTESIAN_POINT('Ctrl Pts',(-4.47746736817774,0.96413985971173,27.3534121848244));
#32190=CARTESIAN_POINT('Ctrl Pts',(-4.51305792988216,0.214172280478033,
27.3798694815088));
#32191=CARTESIAN_POINT('Ctrl Pts',(-4.54864849158657,-0.535795298755707,
27.4063267781933));
#32192=CARTESIAN_POINT('Ctrl Pts',(-4.39325675541333,-1.29482615945024,
27.4327840748778));
#32193=CARTESIAN_POINT('Ctrl Pts',(-4.06580926285144,-1.97047118281612,
27.4592413715622));
#32194=CARTESIAN_POINT('Ctrl Pts',(-3.73836177028958,-2.64611620618197,
27.4856986682467));
#32195=CARTESIAN_POINT('Ctrl Pts',(-3.23885852133909,-3.23837539221917,
27.5121559649312));
#32196=CARTESIAN_POINT('Ctrl Pts',(-2.62813845890629,-3.67511222754014,
27.5386132616156));
#32197=CARTESIAN_POINT('Ctrl Pts',(-2.0174183964735,-4.11184906286111,27.5650705583001));
#32198=CARTESIAN_POINT('Ctrl Pts',(-1.29548152055841,-4.39306354746584,
27.5915278549846));
#32199=CARTESIAN_POINT('Ctrl Pts',(-0.550258943657392,-4.48450406835833,
27.617985151669));
#32200=CARTESIAN_POINT('Ctrl Pts',(0.194963633243671,-4.57594458925083,
27.6444424483535));
#32201=CARTESIAN_POINT('Ctrl Pts',(0.963471911130666,-4.47761114643107,
27.670899745038));
#32202=CARTESIAN_POINT('Ctrl Pts',(1.66166243228906,-4.20148064440581,27.6973570417224));
#32203=CARTESIAN_POINT('Ctrl Pts',(2.35985295344741,-3.92535014238055,27.7238143384069));
#32204=CARTESIAN_POINT('Ctrl Pts',(2.98772571787716,-3.47142258114982,27.7502716350914));
#32205=CARTESIAN_POINT('Ctrl Pts',(3.46880651775718,-2.89498583529569,27.7767289317758));
#32206=CARTESIAN_POINT('Ctrl Pts',(3.94988731763719,-2.31854908944157,27.8031862284603));
#32207=CARTESIAN_POINT('Ctrl Pts',(4.28417615296746,-1.61960315896406,27.8296435251448));
#32208=CARTESIAN_POINT('Ctrl Pts',(4.43095701357266,-0.883278884650025,
27.8561008218292));
#32209=CARTESIAN_POINT('Ctrl Pts',(4.48886884079068,-0.592764958142916,
27.8665394470555));
#32210=CARTESIAN_POINT('Ctrl Pts',(4.517591923217,-0.296432468768919,27.8769780722818));
#32211=CARTESIAN_POINT('Ctrl Pts',(4.51743092439869,-6.91819792334251E-5,
27.8874166975081));
#32212=CARTESIAN_POINT('Ctrl Pts',(4.51801726226543,7.95831363512023E-5,
27.612583302492));
#32213=CARTESIAN_POINT('Ctrl Pts',(4.5174694208443,-0.667214763012837,27.5890708178383));
#32214=CARTESIAN_POINT('Ctrl Pts',(4.36774838447631,-1.33474676446109,27.5655583331847));
#32215=CARTESIAN_POINT('Ctrl Pts',(4.08161297138008,-1.93752346980862,27.5420458485311));
#32216=CARTESIAN_POINT('Ctrl Pts',(3.7596406393301,-2.61579471007933,27.5155885518466));
#32217=CARTESIAN_POINT('Ctrl Pts',(3.26494377406285,-3.21207438494031,27.4891312551621));
#32218=CARTESIAN_POINT('Ctrl Pts',(2.65777590627143,-3.65373628991481,27.4626739584777));
#32219=CARTESIAN_POINT('Ctrl Pts',(2.05060803847998,-4.09539819488933,27.4362166617932));
#32220=CARTESIAN_POINT('Ctrl Pts',(1.33096916816432,-4.38244232997737,27.4097593651087));
#32221=CARTESIAN_POINT('Ctrl Pts',(0.586510513282131,-4.47990703720589,
27.3833020684243));
#32222=CARTESIAN_POINT('Ctrl Pts',(-0.15794814160006,-4.57737174443442,
27.3568447717398));
#32223=CARTESIAN_POINT('Ctrl Pts',(-0.927226581048814,-4.48525702380344,
27.3303874750553));
#32224=CARTESIAN_POINT('Ctrl Pts',(-1.62762754252371,-4.21478234633956,
27.3039301783709));
#32225=CARTESIAN_POINT('Ctrl Pts',(-2.32802850399852,-3.94430766887572,
27.2774728816864));
#32226=CARTESIAN_POINT('Ctrl Pts',(-2.95955198749952,-3.49547303457901,
27.2510155850019));
#32227=CARTESIAN_POINT('Ctrl Pts',(-3.44527913166303,-2.92294600516749,
27.2245582883174));
#32228=CARTESIAN_POINT('Ctrl Pts',(-3.93100627582659,-2.35041897575591,
27.198100991633));
#32229=CARTESIAN_POINT('Ctrl Pts',(-4.27093708065265,-1.65419955122946,
27.1716436949485));
#32230=CARTESIAN_POINT('Ctrl Pts',(-4.42366835032541,-0.919086486967716,
27.1451863982641));
#32231=CARTESIAN_POINT('Ctrl Pts',(-4.57639961999816,-0.183973422706017,
27.1187291015796));
#32232=CARTESIAN_POINT('Ctrl Pts',(-4.54193135451766,0.590033281290875,
27.0922718048951));
#32233=CARTESIAN_POINT('Ctrl Pts',(-4.32446175047231,1.30866046509374,27.0658145082107));
#32234=CARTESIAN_POINT('Ctrl Pts',(-4.10699214642695,2.02728764889665,27.0393572115262));
#32235=CARTESIAN_POINT('Ctrl Pts',(-3.7065212038167,2.69053531250543,27.0128999148417));
#32236=CARTESIAN_POINT('Ctrl Pts',(-3.17182584023783,3.21762062452939,26.9864426181572));
#32237=CARTESIAN_POINT('Ctrl Pts',(-2.63713047665899,3.74470593655333,26.9599853214728));
#32238=CARTESIAN_POINT('Ctrl Pts',(-1.96821069211152,4.13562889699249,26.9335280247883));
#32239=CARTESIAN_POINT('Ctrl Pts',(-1.2465401760389,4.34277552191203,26.9070707281038));
#32240=CARTESIAN_POINT('Ctrl Pts',(-0.524869659966319,4.54992214683155,
26.8806134314194));
#32241=CARTESIAN_POINT('Ctrl Pts',(0.249551587631431,4.57329243623147,26.8541561347349));
#32242=CARTESIAN_POINT('Ctrl Pts',(0.982399915873105,4.41003991472752,26.8276988380504));
#32243=CARTESIAN_POINT('Ctrl Pts',(1.71524824411482,4.24678739322355,26.801241541366));
#32244=CARTESIAN_POINT('Ctrl Pts',(2.40652365300059,3.89691206081561,26.7747842446815));
#32245=CARTESIAN_POINT('Ctrl Pts',(2.97202956278397,3.40302834577314,26.748326947997));
#32246=CARTESIAN_POINT('Ctrl Pts',(3.53753547256739,2.90914463073064,26.7218696513126));
#32247=CARTESIAN_POINT('Ctrl Pts',(3.97727188324847,2.27125253305366,26.6954123546281));
#32248=CARTESIAN_POINT('Ctrl Pts',(4.23767938667642,1.56704660426395,26.6689550579436));
#32249=CARTESIAN_POINT('Ctrl Pts',(4.42262682954492,1.06690323639616,26.6501644727931));
#32250=CARTESIAN_POINT('Ctrl Pts',(4.5171177314681,0.533310047910147,26.6313738876425));
#32251=CARTESIAN_POINT('Ctrl Pts',(4.51761428595877,-0.000111883206665997,
26.612583302492));
#32252=CARTESIAN_POINT('Origin',(0.,0.,20.5));
#32253=CARTESIAN_POINT('',(4.51757373878986,0.000106944042679857,25.612583302492));
#32254=CARTESIAN_POINT('',(4.51783003468408,-0.000112853895665516,25.8874166975081));
#32255=CARTESIAN_POINT('',(4.51775,5.53264807684796E-16,20.5));
#32256=CARTESIAN_POINT('Ctrl Pts',(4.51783003468408,-0.000112853895665516,
25.8874166975081));
#32257=CARTESIAN_POINT('Ctrl Pts',(4.51721010591009,0.603126320584693,25.9086696185212));
#32258=CARTESIAN_POINT('Ctrl Pts',(4.39561298077165,1.20660788106352,25.9299225395344));
#32259=CARTESIAN_POINT('Ctrl Pts',(4.16040899613699,1.76197577425452,25.9511754605476));
#32260=CARTESIAN_POINT('Ctrl Pts',(3.86760869828648,2.45334112163804,25.977632757232));
#32261=CARTESIAN_POINT('Ctrl Pts',(3.39874939952398,3.0701436809076,26.0040900539165));
#32262=CARTESIAN_POINT('Ctrl Pts',(2.81093764353751,3.53725758297881,26.030547350601));
#32263=CARTESIAN_POINT('Ctrl Pts',(2.22312588755105,4.00437148505003,26.0570046472854));
#32264=CARTESIAN_POINT('Ctrl Pts',(1.51636167434063,4.32179672992291,26.0834619439699));
#32265=CARTESIAN_POINT('Ctrl Pts',(0.776728102877261,4.45087127407636,26.1099192406544));
#32266=CARTESIAN_POINT('Ctrl Pts',(0.0370945314138876,4.57994581822981,
26.1363765373388));
#32267=CARTESIAN_POINT('Ctrl Pts',(-0.735408398302442,4.52066966166383,
26.1628338340233));
#32268=CARTESIAN_POINT('Ctrl Pts',(-1.4466906843854,4.28026257464538,26.1892911307078));
#32269=CARTESIAN_POINT('Ctrl Pts',(-2.15797297046839,4.03985548762692,26.2157484273923));
#32270=CARTESIAN_POINT('Ctrl Pts',(-2.80803461291801,3.61831747015598,26.2422057240767));
#32271=CARTESIAN_POINT('Ctrl Pts',(-3.31769882312739,3.06699138623123,26.2686630207612));
#32272=CARTESIAN_POINT('Ctrl Pts',(-3.82736303333674,2.51566530230651,26.2951203174456));
#32273=CARTESIAN_POINT('Ctrl Pts',(-4.19662981130587,1.834551151928,26.3215776141301));
#32274=CARTESIAN_POINT('Ctrl Pts',(-4.38052287215722,1.1066078848015,26.3480349108146));
#32275=CARTESIAN_POINT('Ctrl Pts',(-4.56441593300857,0.378664617674993,
26.3744922074991));
#32276=CARTESIAN_POINT('Ctrl Pts',(-4.56293527674215,-0.396107766199503,
26.4009495041835));
#32277=CARTESIAN_POINT('Ctrl Pts',(-4.3762612456525,-1.12334284793087,26.427406800868));
#32278=CARTESIAN_POINT('Ctrl Pts',(-4.18958721456285,-1.85057792966224,
26.4538640975524));
#32279=CARTESIAN_POINT('Ctrl Pts',(-3.81771980864998,-2.53027570925048,
26.4803213942369));
#32280=CARTESIAN_POINT('Ctrl Pts',(-3.30595206639681,-3.0796497493845,26.5067786909214));
#32281=CARTESIAN_POINT('Ctrl Pts',(-2.79418432414364,-3.62902378951853,
26.5332359876059));
#32282=CARTESIAN_POINT('Ctrl Pts',(-2.14251624555017,-4.04807409019834,
26.5596932842903));
#32283=CARTESIAN_POINT('Ctrl Pts',(-1.43032028136767,-4.28576078857718,
26.5861505809748));
#32284=CARTESIAN_POINT('Ctrl Pts',(-0.718124317185119,-4.52344748695604,
26.6126078776593));
#32285=CARTESIAN_POINT('Ctrl Pts',(0.0545995325864684,-4.57977058303392,
26.6390651743437));
#32286=CARTESIAN_POINT('Ctrl Pts',(0.793734358242524,-4.44786998604306,
26.6655224710282));
#32287=CARTESIAN_POINT('Ctrl Pts',(1.53286918389854,-4.31596938905221,26.6919797677127));
#32288=CARTESIAN_POINT('Ctrl Pts',(2.23841498543902,-3.99584509899264,26.7184370643971));
#32289=CARTESIAN_POINT('Ctrl Pts',(2.82443706508592,-3.52648790010206,26.7448943610816));
#32290=CARTESIAN_POINT('Ctrl Pts',(3.41045914473281,-3.05713070121148,26.7713516577661));
#32291=CARTESIAN_POINT('Ctrl Pts',(3.87695750248613,-2.43854059348989,26.7978089544505));
#32292=CARTESIAN_POINT('Ctrl Pts',(4.1671131546598,-1.74606116744478,26.824266251135));
#32293=CARTESIAN_POINT('Ctrl Pts',(4.39796892664792,-1.19510559829445,26.845316399926));
#32294=CARTESIAN_POINT('Ctrl Pts',(4.51719573188836,-0.59737640031138,26.8663665487171));
#32295=CARTESIAN_POINT('Ctrl Pts',(4.51781182322151,0.000114263439177032,
26.8874166975081));
#32296=CARTESIAN_POINT('Ctrl Pts',(4.51761428595877,-0.000111883206665997,
26.612583302492));
#32297=CARTESIAN_POINT('Ctrl Pts',(4.51781688422861,-0.217752368533235,
26.604916590958));
#32298=CARTESIAN_POINT('Ctrl Pts',(4.50237218377303,-0.435364344536763,
26.5972498794241));
#32299=CARTESIAN_POINT('Ctrl Pts',(4.47103989191871,-0.65066422144523,26.5895831678902));
#32300=CARTESIAN_POINT('Ctrl Pts',(4.36291429755835,-1.39364935846232,26.5631258712058));
#32301=CARTESIAN_POINT('Ctrl Pts',(4.06558451266292,-2.10909987259421,26.5366685745213));
#32302=CARTESIAN_POINT('Ctrl Pts',(3.61526497596852,-2.70987468303106,26.5102112778368));
#32303=CARTESIAN_POINT('Ctrl Pts',(3.16494543927413,-3.31064949346792,26.4837539811524));
#32304=CARTESIAN_POINT('Ctrl Pts',(2.56163615078078,-3.79674860020972,26.4572966844679));
#32305=CARTESIAN_POINT('Ctrl Pts',(1.87881951412572,-4.10896567003641,26.4308393877834));
#32306=CARTESIAN_POINT('Ctrl Pts',(1.19600287747066,-4.4211827398631,26.4043820910989));
#32307=CARTESIAN_POINT('Ctrl Pts',(0.433678892653904,-4.55951777277466,
26.3779247944145));
#32308=CARTESIAN_POINT('Ctrl Pts',(-0.315302222661645,-4.50712171486216,
26.35146749773));
#32309=CARTESIAN_POINT('Ctrl Pts',(-1.06428333797715,-4.45472565694967,
26.3250102010456));
#32310=CARTESIAN_POINT('Ctrl Pts',(-1.79992158379143,-4.21159850821314,
26.2985529043611));
#32311=CARTESIAN_POINT('Ctrl Pts',(-2.43261703591816,-3.80735288629228,
26.2720956076766));
#32312=CARTESIAN_POINT('Ctrl Pts',(-3.06531248804499,-3.40310726437134,
26.2456383109922));
#32313=CARTESIAN_POINT('Ctrl Pts',(-3.59506514648422,-2.83774316926603,
26.2191810143077));
#32314=CARTESIAN_POINT('Ctrl Pts',(-3.95735172373175,-2.18012132205405,
26.1927237176232));
#32315=CARTESIAN_POINT('Ctrl Pts',(-4.31963830097924,-1.52249947484215,
26.1662664209387));
#32316=CARTESIAN_POINT('Ctrl Pts',(-4.51445879703509,-0.772619875523507,
26.1398091242543));
#32317=CARTESIAN_POINT('Ctrl Pts',(-4.51808429109356,-0.0218170293801812,
26.1133518275698));
#32318=CARTESIAN_POINT('Ctrl Pts',(-4.52170978515203,0.728985816763102,
26.0868945308853));
#32319=CARTESIAN_POINT('Ctrl Pts',(-4.33414027721319,1.48071190973118,26.0604372342009));
#32320=CARTESIAN_POINT('Ctrl Pts',(-3.97822152575495,2.1418018433593,26.0339799375164));
#32321=CARTESIAN_POINT('Ctrl Pts',(-3.62230277429665,2.80289177698754,26.0075226408319));
#32322=CARTESIAN_POINT('Ctrl Pts',(-3.09803477931891,3.37334555127578,25.9810653441475));
#32323=CARTESIAN_POINT('Ctrl Pts',(-2.46927280238623,3.78368252785471,25.954608047463));
#32324=CARTESIAN_POINT('Ctrl Pts',(-1.84051082545367,4.19401950443358,25.9281507507785));
#32325=CARTESIAN_POINT('Ctrl Pts',(-1.10725486656624,4.44423968330318,25.9016934540941));
#32326=CARTESIAN_POINT('Ctrl Pts',(-0.358814689999135,4.50386652360371,
25.8752361574096));
#32327=CARTESIAN_POINT('Ctrl Pts',(0.389625486568016,4.56349336390425,25.8487788607251));
#32328=CARTESIAN_POINT('Ctrl Pts',(1.15324988081482,4.43252686563568,25.8223215640406));
#32329=CARTESIAN_POINT('Ctrl Pts',(1.83904988664902,4.1269186033424,25.7958642673562));
#32330=CARTESIAN_POINT('Ctrl Pts',(2.52484989248321,3.82131034104913,25.7694069706717));
#32331=CARTESIAN_POINT('Ctrl Pts',(3.13282550990476,3.34106031473115,25.7429496739873));
#32332=CARTESIAN_POINT('Ctrl Pts',(3.58892598157735,2.74466244608629,25.7164923773028));
#32333=CARTESIAN_POINT('Ctrl Pts',(4.04502645324994,2.14826457744144,25.6900350806183));
#32334=CARTESIAN_POINT('Ctrl Pts',(4.34925177917356,1.43571886646971,25.6635777839338));
#32335=CARTESIAN_POINT('Ctrl Pts',(4.46454765134638,0.693812592170858,25.6371204872494));
#32336=CARTESIAN_POINT('Ctrl Pts',(4.50019044774909,0.464458203445785,25.6289414256636));
#32337=CARTESIAN_POINT('Ctrl Pts',(4.51777748758952,0.232297861633777,25.6207623640778));
#32338=CARTESIAN_POINT('Ctrl Pts',(4.51757373878986,0.000106944042679857,
25.612583302492));
#32339=CARTESIAN_POINT('Origin',(0.,0.,20.5));
#32340=CARTESIAN_POINT('',(4.51805179992706,-6.79869438786201E-5,24.612583302492));
#32341=CARTESIAN_POINT('',(4.51742159705025,6.47500723078405E-5,24.8874166975081));
#32342=CARTESIAN_POINT('',(4.51775,5.53264807684796E-16,20.5));
#32343=CARTESIAN_POINT('Ctrl Pts',(4.51742159705025,6.47500723078405E-5,
24.8874166975081));
#32344=CARTESIAN_POINT('Ctrl Pts',(4.51757480489056,0.3021867342129,24.8980580949565));
#32345=CARTESIAN_POINT('Ctrl Pts',(4.4877169204789,0.604278844221435,24.9086994924049));
#32346=CARTESIAN_POINT('Ctrl Pts',(4.42754861718235,0.90020824628754,24.9193408898533));
#32347=CARTESIAN_POINT('Ctrl Pts',(4.27795448172836,1.63596612264488,24.9457981865378));
#32348=CARTESIAN_POINT('Ctrl Pts',(3.94099660709531,2.33362924326996,24.9722554832222));
#32349=CARTESIAN_POINT('Ctrl Pts',(3.4577160894917,2.90822301219621,24.9987127799067));
#32350=CARTESIAN_POINT('Ctrl Pts',(2.97443557188809,3.48281678112246,25.0251700765912));
#32351=CARTESIAN_POINT('Ctrl Pts',(2.34483241131392,3.93434119834988,25.0516273732757));
#32352=CARTESIAN_POINT('Ctrl Pts',(1.64559157592564,4.20780108957635,25.0780846699601));
#32353=CARTESIAN_POINT('Ctrl Pts',(0.946350740537367,4.48126098080282,25.1045419666446));
#32354=CARTESIAN_POINT('Ctrl Pts',(0.177472230334982,4.57665634602833,25.1309992633291));
#32355=CARTESIAN_POINT('Ctrl Pts',(-0.567395403080719,4.48236813534545,
25.1574565600135));
#32356=CARTESIAN_POINT('Ctrl Pts',(-1.31226303649646,4.38807992466257,25.183913856698));
#32357=CARTESIAN_POINT('Ctrl Pts',(-2.03311979312552,4.10410813807126,25.2103711533825));
#32358=CARTESIAN_POINT('Ctrl Pts',(-2.64216611780515,3.66504022489793,25.2368284500669));
#32359=CARTESIAN_POINT('Ctrl Pts',(-3.25121244248478,3.22597231172459,25.2632857467514));
#32360=CARTESIAN_POINT('Ctrl Pts',(-3.74844833521498,2.63180827196922,25.2897430434359));
#32361=CARTESIAN_POINT('Ctrl Pts',(-4.07331101456769,1.95491662809413,25.3162003401203));
#32362=CARTESIAN_POINT('Ctrl Pts',(-4.39817369392037,1.27802498421911,25.3426576368048));
#32363=CARTESIAN_POINT('Ctrl Pts',(-4.55066315989561,0.518405736224393,
25.3691149334893));
#32364=CARTESIAN_POINT('Ctrl Pts',(-4.51220636430247,-0.231420332178628,
25.3955722301737));
#32365=CARTESIAN_POINT('Ctrl Pts',(-4.47374956870933,-0.981246400581734,
25.4220295268582));
#32366=CARTESIAN_POINT('Ctrl Pts',(-4.24434651154778,-1.72127928939314,
25.4484868235427));
#32367=CARTESIAN_POINT('Ctrl Pts',(-3.85193823129256,-2.36138381177311,
25.4749441202271));
#32368=CARTESIAN_POINT('Ctrl Pts',(-3.45952995103737,-3.00148833415305,
25.5014014169116));
#32369=CARTESIAN_POINT('Ctrl Pts',(-2.90411644768853,-3.54166449010157,
25.5278587135961));
#32370=CARTESIAN_POINT('Ctrl Pts',(-2.25334647126047,-3.91611942165396,
25.5543160102806));
#32371=CARTESIAN_POINT('Ctrl Pts',(-1.60257649483241,-4.29057435320635,
25.580773306965));
#32372=CARTESIAN_POINT('Ctrl Pts',(-0.856450045325122,-4.49930806036262,
25.6072306036495));
#32373=CARTESIAN_POINT('Ctrl Pts',(-0.105844498527155,-4.51689700860324,
25.6336879003339));
#32374=CARTESIAN_POINT('Ctrl Pts',(0.644761048270813,-4.53448595684386,
25.6601451970184));
#32375=CARTESIAN_POINT('Ctrl Pts',(1.39984569235946,-4.36093014616883,25.6866024937029));
#32376=CARTESIAN_POINT('Ctrl Pts',(2.06744095976455,-4.01736848223874,25.7130597903874));
#32377=CARTESIAN_POINT('Ctrl Pts',(2.73503622716964,-3.67380681830865,25.7395170870718));
#32378=CARTESIAN_POINT('Ctrl Pts',(3.31514211789117,-3.16023930112349,25.7659743837563));
#32379=CARTESIAN_POINT('Ctrl Pts',(3.73710237646057,-2.53921788589521,25.7924316804407));
#32380=CARTESIAN_POINT('Ctrl Pts',(4.15906263502999,-1.9181964706669,25.8188889771252));
#32381=CARTESIAN_POINT('Ctrl Pts',(4.42287726144725,-1.18972115739545,25.8453462738097));
#32382=CARTESIAN_POINT('Ctrl Pts',(4.49641392618663,-0.442519433010954,
25.8718035704942));
#32383=CARTESIAN_POINT('Ctrl Pts',(4.51087921466574,-0.295538487742104,
25.8770079461655));
#32384=CARTESIAN_POINT('Ctrl Pts',(4.51798184168639,-0.147832938193592,
25.8822123218368));
#32385=CARTESIAN_POINT('Ctrl Pts',(4.51783003468408,-0.000112853895665516,
25.8874166975081));
#32386=CARTESIAN_POINT('Ctrl Pts',(4.51757373878986,0.000106944042679857,
25.612583302492));
#32387=CARTESIAN_POINT('Ctrl Pts',(4.51711840923619,-0.518783901194552,
25.5943050673933));
#32388=CARTESIAN_POINT('Ctrl Pts',(4.42781321686835,-1.03782744645157,25.5760268322946));
#32389=CARTESIAN_POINT('Ctrl Pts',(4.25261539535607,-1.52604847346927,25.557748597196));
#32390=CARTESIAN_POINT('Ctrl Pts',(3.99902084877091,-2.2327364271846,25.5312913005115));
#32391=CARTESIAN_POINT('Ctrl Pts',(3.56546533717857,-2.87484549698929,25.504834003827));
#32392=CARTESIAN_POINT('Ctrl Pts',(3.00475544206156,-3.3741675088233,25.4783767071426));
#32393=CARTESIAN_POINT('Ctrl Pts',(2.44404554694452,-3.87348952065733,25.4519194104581));
#32394=CARTESIAN_POINT('Ctrl Pts',(1.7561812683028,-4.23002447452067,25.4254621137736));
#32395=CARTESIAN_POINT('Ctrl Pts',(1.0249437139941,-4.40034680762112,25.3990048170892));
#32396=CARTESIAN_POINT('Ctrl Pts',(0.293706159685441,-4.57066914072155,
25.3725475204047));
#32397=CARTESIAN_POINT('Ctrl Pts',(-0.4809046702902,-4.55477885305912,25.3460902237202));
#32398=CARTESIAN_POINT('Ctrl Pts',(-1.20454203412779,-4.35461136408482,
25.3196329270358));
#32399=CARTESIAN_POINT('Ctrl Pts',(-1.92817939796537,-4.15444387511052,
25.2931756303513));
#32400=CARTESIAN_POINT('Ctrl Pts',(-2.60084329566491,-3.76999918482436,
25.2667183336669));
#32401=CARTESIAN_POINT('Ctrl Pts',(-3.14060400894472,-3.24810223102625,
25.2402610369824));
#32402=CARTESIAN_POINT('Ctrl Pts',(-3.68036472222457,-2.72620527722811,
25.2138037402979));
#32403=CARTESIAN_POINT('Ctrl Pts',(-4.08722225108469,-2.066856059918,25.1873464436134));
#32404=CARTESIAN_POINT('Ctrl Pts',(-4.31162179879184,-1.35036258404192,
25.1608891469289));
#32405=CARTESIAN_POINT('Ctrl Pts',(-4.53602134649897,-0.633869108165933,
25.1344318502445));
#32406=CARTESIAN_POINT('Ctrl Pts',(-4.57796291305318,0.139768626276003,
25.1079745535601));
#32407=CARTESIAN_POINT('Ctrl Pts',(-4.4323380620662,0.876322399437911,25.0815172568756));
#32408=CARTESIAN_POINT('Ctrl Pts',(-4.28671321107921,1.6128761725999,25.0550599601911));
#32409=CARTESIAN_POINT('Ctrl Pts',(-3.95352194255099,2.31234598448186,25.0286026635066));
#32410=CARTESIAN_POINT('Ctrl Pts',(-3.4733465842351,2.88953718612163,25.0021453668221));
#32411=CARTESIAN_POINT('Ctrl Pts',(-2.99317122591925,3.46672838776137,24.9756880701377));
#32412=CARTESIAN_POINT('Ctrl Pts',(-2.36601177781574,3.92164097915893,24.9492307734532));
#32413=CARTESIAN_POINT('Ctrl Pts',(-1.66825556660664,4.19886711014808,24.9227734767688));
#32414=CARTESIAN_POINT('Ctrl Pts',(-0.970499355397546,4.47609324113723,
24.8963161800843));
#32415=CARTESIAN_POINT('Ctrl Pts',(-0.202146381082855,4.57563291171796,
24.8698588833998));
#32416=CARTESIAN_POINT('Ctrl Pts',(0.543218814426126,4.4853623001772,24.8434015867153));
#32417=CARTESIAN_POINT('Ctrl Pts',(1.28858400993515,4.39509168863642,24.8169442900309));
#32418=CARTESIAN_POINT('Ctrl Pts',(2.01096142663846,4.11501079497414,24.7904869933464));
#32419=CARTESIAN_POINT('Ctrl Pts',(2.62236629465924,3.67923316206414,24.7640296966619));
#32420=CARTESIAN_POINT('Ctrl Pts',(3.23377116267999,3.24345552915417,24.7375723999775));
#32421=CARTESIAN_POINT('Ctrl Pts',(3.73420348201823,2.65198115699651,24.711115103293));
#32422=CARTESIAN_POINT('Ctrl Pts',(4.06271115002261,1.97685096951678,24.6846578066085));
#32423=CARTESIAN_POINT('Ctrl Pts',(4.36101609468216,1.3637916931913,24.660632971903));
#32424=CARTESIAN_POINT('Ctrl Pts',(4.51755636187948,0.681751967669245,24.6366081371975));
#32425=CARTESIAN_POINT('Ctrl Pts',(4.51805179992706,-6.79869438786201E-5,
24.612583302492));
#32426=CARTESIAN_POINT('Origin',(0.,0.,20.5));
#32427=CARTESIAN_POINT('',(4.5173631353831,-4.88662610135722E-6,23.612583302492));
#32428=CARTESIAN_POINT('',(4.51813699104787,9.0065690785813E-7,23.8874166975081));
#32429=CARTESIAN_POINT('',(4.51775,5.53264807684796E-16,20.5));
#32430=CARTESIAN_POINT('Ctrl Pts',(4.51813695063288,9.0056284873609E-7,
23.8874166975081));
#32431=CARTESIAN_POINT('Ctrl Pts',(4.51814591729222,0.751660275924123,23.9139038680762));
#32432=CARTESIAN_POINT('Ctrl Pts',(4.32649937043261,1.5033152188212,23.9403910386443));
#32433=CARTESIAN_POINT('Ctrl Pts',(3.96661538289285,2.16322075812818,23.9668782092125));
#32434=CARTESIAN_POINT('Ctrl Pts',(3.6071372949696,2.8223820147924,23.9933355058969));
#32435=CARTESIAN_POINT('Ctrl Pts',(3.07980110896882,3.39000071259223,24.0197928025814));
#32436=CARTESIAN_POINT('Ctrl Pts',(2.44883578872663,3.7969415223372,24.0462500992659));
#32437=CARTESIAN_POINT('Ctrl Pts',(1.81787046848448,4.20388233208215,24.0727073959503));
#32438=CARTESIAN_POINT('Ctrl Pts',(1.08327601400093,4.45014525377226,24.0991646926348));
#32439=CARTESIAN_POINT('Ctrl Pts',(0.334525216833109,4.50573573609242,24.1256219893193));
#32440=CARTESIAN_POINT('Ctrl Pts',(-0.414225580334709,4.56132621841258,
24.1520792860037));
#32441=CARTESIAN_POINT('Ctrl Pts',(-1.17713272018679,4.4262442613628,24.1785365826882));
#32442=CARTESIAN_POINT('Ctrl Pts',(-1.86127495742213,4.11694269781237,24.2049938793727));
#32443=CARTESIAN_POINT('Ctrl Pts',(-2.54541719465748,3.80764113426195,24.2314511760572));
#32444=CARTESIAN_POINT('Ctrl Pts',(-3.15079452927609,3.32411996421088,24.2579084727416));
#32445=CARTESIAN_POINT('Ctrl Pts',(-3.6036726719115,2.72527153104338,24.2843657694261));
#32446=CARTESIAN_POINT('Ctrl Pts',(-4.05655081454692,2.12642309787588,24.3108230661106));
#32447=CARTESIAN_POINT('Ctrl Pts',(-4.35692976519914,1.41224740159195,24.337280362795));
#32448=CARTESIAN_POINT('Ctrl Pts',(-4.46822370011745,0.669730251598438,
24.3637376594795));
#32449=CARTESIAN_POINT('Ctrl Pts',(-4.57951763503577,-0.0727868983951169,
24.390194956164));
#32450=CARTESIAN_POINT('Ctrl Pts',(-4.50172655422016,-0.843645502098255,
24.4166522528484));
#32451=CARTESIAN_POINT('Ctrl Pts',(-4.24432532522016,-1.54895583471323,
24.4431095495329));
#32452=CARTESIAN_POINT('Ctrl Pts',(-3.98692409622017,-2.25426616732816,
24.4695668462174));
#32453=CARTESIAN_POINT('Ctrl Pts',(-3.54991271903582,-2.89402822885493,
24.4960241429018));
#32454=CARTESIAN_POINT('Ctrl Pts',(-2.98651869575401,-3.39031970824422,
24.5224814395863));
#32455=CARTESIAN_POINT('Ctrl Pts',(-2.42312467247219,-3.88661118763352,
24.5489387362708));
#32456=CARTESIAN_POINT('Ctrl Pts',(-1.73334800309291,-4.23943208488534,
24.5753960329552));
#32457=CARTESIAN_POINT('Ctrl Pts',(-1.00120272254919,-4.40580920519233,
24.6018533296397));
#32458=CARTESIAN_POINT('Ctrl Pts',(-0.269057442005433,-4.57218632549932,
24.6283106263242));
#32459=CARTESIAN_POINT('Ctrl Pts',(0.505456449702776,-4.55211966886146,
24.6547679230086));
#32460=CARTESIAN_POINT('Ctrl Pts',(1.22800401774408,-4.34805333184884,24.6812252196931));
#32461=CARTESIAN_POINT('Ctrl Pts',(1.95055158578534,-4.14398699483623,24.7076825163776));
#32462=CARTESIAN_POINT('Ctrl Pts',(2.6211328301597,-3.75592097744887,24.7341398130621));
#32463=CARTESIAN_POINT('Ctrl Pts',(3.15807169745557,-3.23112129111977,24.7605971097465));
#32464=CARTESIAN_POINT('Ctrl Pts',(3.69501056475143,-2.70632160479067,24.787054406431));
#32465=CARTESIAN_POINT('Ctrl Pts',(4.0983070549688,-2.04478824951983,24.8135117031154));
#32466=CARTESIAN_POINT('Ctrl Pts',(4.31884010194003,-1.32709525583961,24.8399689997999));
#32467=CARTESIAN_POINT('Ctrl Pts',(4.45067248416388,-0.898065782199879,
24.855784899036));
#32468=CARTESIAN_POINT('Ctrl Pts',(4.51719389013711,-0.448967520484957,
24.871600798272));
#32469=CARTESIAN_POINT('Ctrl Pts',(4.51742159705025,6.47500723078405E-5,
24.8874166975081));
#32470=CARTESIAN_POINT('Ctrl Pts',(4.51805179992706,-6.79869438786201E-5,
24.612583302492));
#32471=CARTESIAN_POINT('Ctrl Pts',(4.51810196194601,-0.0691007664161157,
24.610150840513));
#32472=CARTESIAN_POINT('Ctrl Pts',(4.51655248974293,-0.13813129299046,24.6077183785341));
#32473=CARTESIAN_POINT('Ctrl Pts',(4.51338856189906,-0.207087743519482,
24.6052859165551));
#32474=CARTESIAN_POINT('Ctrl Pts',(4.47897528910062,-0.957110266274211,
24.5788286198707));
#32475=CARTESIAN_POINT('Ctrl Pts',(4.25356572683319,-1.69836930898188,24.5523713231862));
#32476=CARTESIAN_POINT('Ctrl Pts',(3.8646145103131,-2.3405803406153,24.5259140265017));
#32477=CARTESIAN_POINT('Ctrl Pts',(3.47566329379301,-2.98279137224871,24.4994567298173));
#32478=CARTESIAN_POINT('Ctrl Pts',(2.92317042302025,-3.52595439280789,24.4729994331328));
#32479=CARTESIAN_POINT('Ctrl Pts',(2.27442891819395,-3.90391274752403,24.4465421364483));
#32480=CARTESIAN_POINT('Ctrl Pts',(1.62568741336761,-4.2818711022402,24.4200848397639));
#32481=CARTESIAN_POINT('Ctrl Pts',(0.88069727448771,-4.49462479111332,24.3936275430794));
#32482=CARTESIAN_POINT('Ctrl Pts',(0.130197475965773,-4.51626065030008,
24.3671702463949));
#32483=CARTESIAN_POINT('Ctrl Pts',(-0.620302322556121,-4.53789650948684,
24.3407129497104));
#32484=CARTESIAN_POINT('Ctrl Pts',(-1.37631178072007,-4.36841453898727,
24.314255653026));
#32485=CARTESIAN_POINT('Ctrl Pts',(-2.04574978322055,-4.02845745523667,
24.2877983563415));
#32486=CARTESIAN_POINT('Ctrl Pts',(-2.71518778572104,-3.68850037148608,
24.2613410596571));
#32487=CARTESIAN_POINT('Ctrl Pts',(-3.29805433255807,-3.17806817448446,
24.2348837629726));
#32488=CARTESIAN_POINT('Ctrl Pts',(-3.72335692340428,-2.55933094091641,
24.2084264662881));
#32489=CARTESIAN_POINT('Ctrl Pts',(-4.14865951425051,-1.94059370734831,
24.1819691696036));
#32490=CARTESIAN_POINT('Ctrl Pts',(-4.41639814910591,-1.21355143721374,
24.1555118729192));
#32491=CARTESIAN_POINT('Ctrl Pts',(-4.49396255855832,-0.466757074372799,
24.1290545762347));
#32492=CARTESIAN_POINT('Ctrl Pts',(-4.57152696801073,0.280037288468098,
24.1025972795502));
#32493=CARTESIAN_POINT('Ctrl Pts',(-4.4589171520602,1.04658374401527,24.0761399828658));
#32494=CARTESIAN_POINT('Ctrl Pts',(-4.16984886166344,1.73951778234053,24.0496826861813));
#32495=CARTESIAN_POINT('Ctrl Pts',(-3.88078057126667,2.43245182066584,24.0232253894968));
#32496=CARTESIAN_POINT('Ctrl Pts',(-3.41525380642364,3.05177344176913,23.9967680928124));
#32497=CARTESIAN_POINT('Ctrl Pts',(-2.82996921187404,3.52204995762946,23.9703107961279));
#32498=CARTESIAN_POINT('Ctrl Pts',(-2.24468461732448,3.99232647348976,23.9438534994434));
#32499=CARTESIAN_POINT('Ctrl Pts',(-1.53964219306833,4.31355788410714,23.917396202759));
#32500=CARTESIAN_POINT('Ctrl Pts',(-0.800715326097399,4.44661855917222,
23.8909389060745));
#32501=CARTESIAN_POINT('Ctrl Pts',(-0.0617884591264724,4.5796792342373,
23.86448160939));
#32502=CARTESIAN_POINT('Ctrl Pts',(0.711022850559258,4.5245691737501,23.8380243127056));
#32503=CARTESIAN_POINT('Ctrl Pts',(1.42359104075306,4.28800072211045,23.8115670160211));
#32504=CARTESIAN_POINT('Ctrl Pts',(2.13615923094691,4.05143227047079,23.7851097193366));
#32505=CARTESIAN_POINT('Ctrl Pts',(2.78848430164884,3.63340542767864,23.7586524226522));
#32506=CARTESIAN_POINT('Ctrl Pts',(3.30111378116074,3.08483540049647,23.7321951259677));
#32507=CARTESIAN_POINT('Ctrl Pts',(3.81374326067261,2.53626537331434,23.7057378292832));
#32508=CARTESIAN_POINT('Ctrl Pts',(4.18667714899447,1.85715216174218,23.6792805325988));
#32509=CARTESIAN_POINT('Ctrl Pts',(4.37449251133263,1.13021100344109,23.6528232359143));
#32510=CARTESIAN_POINT('Ctrl Pts',(4.46971107890219,0.761666625925485,23.6394099247735));
#32511=CARTESIAN_POINT('Ctrl Pts',(4.51734893340559,0.380829109202114,23.6259966136328));
#32512=CARTESIAN_POINT('Ctrl Pts',(4.51736327228765,-4.88489681080284E-6,
23.612583302492));
#32513=CARTESIAN_POINT('Origin',(0.,0.,20.5));
#32514=CARTESIAN_POINT('',(4.51802736372575,7.65320072124154E-5,22.612583302492));
#32515=CARTESIAN_POINT('',(4.51742427980126,-6.60698246896739E-5,22.8874166975081));
#32516=CARTESIAN_POINT('',(4.51775,5.53264807684796E-16,20.5));
#32517=CARTESIAN_POINT('Ctrl Pts',(4.51742427980126,-6.60698246896739E-5,
22.8874166975081));
#32518=CARTESIAN_POINT('Ctrl Pts',(4.51719087600353,0.450661745130009,22.9032923445115));
#32519=CARTESIAN_POINT('Ctrl Pts',(4.450158091451,0.901457458944964,22.9191679915148));
#32520=CARTESIAN_POINT('Ctrl Pts',(4.31734276296,1.3319583722546,22.9350436385182));
#32521=CARTESIAN_POINT('Ctrl Pts',(4.09600157608532,2.04940254217993,22.9615009352027));
#32522=CARTESIAN_POINT('Ctrl Pts',(3.69196031163168,2.71048127828687,22.9879582318872));
#32523=CARTESIAN_POINT('Ctrl Pts',(3.15443074594463,3.23467592132643,23.0144155285716));
#32524=CARTESIAN_POINT('Ctrl Pts',(2.61690118025762,3.75887056436596,23.0408728252561));
#32525=CARTESIAN_POINT('Ctrl Pts',(1.94588331333721,4.14618111433815,23.0673301219406));
#32526=CARTESIAN_POINT('Ctrl Pts',(1.22310638006181,4.34943357534335,23.093787418625));
#32527=CARTESIAN_POINT('Ctrl Pts',(0.500329446786407,4.55268603634856,23.1202447153095));
#32528=CARTESIAN_POINT('Ctrl Pts',(-0.274206552844009,4.5718804083868,23.146702011994));
#32529=CARTESIAN_POINT('Ctrl Pts',(-1.00616399197876,4.4046788379547,23.1731593086784));
#32530=CARTESIAN_POINT('Ctrl Pts',(-1.73812143111355,4.23747726752258,23.1996166053629));
#32531=CARTESIAN_POINT('Ctrl Pts',(-2.4275003097527,3.88387975462009,23.2260739020474));
#32532=CARTESIAN_POINT('Ctrl Pts',(-2.99033504306372,3.38695408510429,23.2525311987318));
#32533=CARTESIAN_POINT('Ctrl Pts',(-3.55316977637471,2.89002841558852,23.2789884954163));
#32534=CARTESIAN_POINT('Ctrl Pts',(-3.98946036435762,2.24977458945944,23.3054457921008));
#32535=CARTESIAN_POINT('Ctrl Pts',(-4.24606709644918,1.54417481408558,23.3319030887853));
#32536=CARTESIAN_POINT('Ctrl Pts',(-4.50267382854076,0.838575038711681,
23.3583603854697));
#32537=CARTESIAN_POINT('Ctrl Pts',(-4.57959670474098,0.0676293140930979,
23.3848176821541));
#32538=CARTESIAN_POINT('Ctrl Pts',(-4.46746660375748,-0.674762023707061,
23.4112749788386));
#32539=CARTESIAN_POINT('Ctrl Pts',(-4.35533650277398,-1.41715336150718,
23.4377322755231));
#32540=CARTESIAN_POINT('Ctrl Pts',(-4.05415342460676,-2.13099031248878,
23.4641895722076));
#32541=CARTESIAN_POINT('Ctrl Pts',(-3.60060113490302,-2.72932832606618,
23.4906468688921));
#32542=CARTESIAN_POINT('Ctrl Pts',(-3.14704884519929,-3.32766633964359,
23.5171041655765));
#32543=CARTESIAN_POINT('Ctrl Pts',(-2.54112734395902,-3.81050541581682,
23.543561462261));
#32544=CARTESIAN_POINT('Ctrl Pts',(-1.85663719941186,-4.11903628947138,
23.5700187589454));
#32545=CARTESIAN_POINT('Ctrl Pts',(-1.17214705486469,-4.42756716312594,
23.5964760556299));
#32546=CARTESIAN_POINT('Ctrl Pts',(-0.409088267010601,-4.56178983426184,
23.6229333523144));
#32547=CARTESIAN_POINT('Ctrl Pts',(0.339599448275288,-4.50535613008826,
23.6493906489989));
#32548=CARTESIAN_POINT('Ctrl Pts',(1.08828716356118,-4.44892242591468,23.6758479456834));
#32549=CARTESIAN_POINT('Ctrl Pts',(1.82260380627889,-4.20183234643162,23.7023052423678));
#32550=CARTESIAN_POINT('Ctrl Pts',(2.45311042204474,-3.7941811898551,23.7287625390522));
#32551=CARTESIAN_POINT('Ctrl Pts',(3.08361703781062,-3.38653003327857,23.7552198357367));
#32552=CARTESIAN_POINT('Ctrl Pts',(3.61031362662464,-2.81831779960855,23.7816771324212));
#32553=CARTESIAN_POINT('Ctrl Pts',(3.96904912687646,-2.15875211004929,23.8081344291057));
#32554=CARTESIAN_POINT('Ctrl Pts',(4.32737956599415,-1.49993115979256,23.8345618519065));
#32555=CARTESIAN_POINT('Ctrl Pts',(4.51812800419987,-0.749962938110063,
23.8609892747073));
#32556=CARTESIAN_POINT('Ctrl Pts',(4.51813695063288,9.0056284873609E-7,
23.8874166975081));
#32557=CARTESIAN_POINT('Ctrl Pts',(4.51736327228765,-4.88489681080284E-6,
23.612583302492));
#32558=CARTESIAN_POINT('Ctrl Pts',(4.51737721635919,-0.370352896766723,
23.5995393169483));
#32559=CARTESIAN_POINT('Ctrl Pts',(4.47235409625982,-0.740697577327283,
23.5864953314046));
#32560=CARTESIAN_POINT('Ctrl Pts',(4.38225454858748,-1.09973029228254,23.5734513458609));
#32561=CARTESIAN_POINT('Ctrl Pts',(4.19950438714968,-1.82796132467507,23.5469940491764));
#32562=CARTESIAN_POINT('Ctrl Pts',(3.83130722791959,-2.50965428443002,23.5205367524919));
#32563=CARTESIAN_POINT('Ctrl Pts',(3.3225090776327,-3.06177972318861,23.4940794558075));
#32564=CARTESIAN_POINT('Ctrl Pts',(2.81371092734586,-3.61390516194714,23.467622159123));
#32565=CARTESIAN_POINT('Ctrl Pts',(2.16431178600224,-4.03646307970933,23.4411648624385));
#32566=CARTESIAN_POINT('Ctrl Pts',(1.45340774986053,-4.27798639033802,23.4147075657541));
#32567=CARTESIAN_POINT('Ctrl Pts',(0.742503713718783,-4.51950970096672,
23.3882502690696));
#32568=CARTESIAN_POINT('Ctrl Pts',(-0.0299052172210591,-4.5799984044619,
23.3617929723851));
#32569=CARTESIAN_POINT('Ctrl Pts',(-0.769740489176251,-4.4520850425719,
23.3353356757007));
#32570=CARTESIAN_POINT('Ctrl Pts',(-1.50957576113144,-4.32417168068191,
23.3088783790162));
#32571=CARTESIAN_POINT('Ctrl Pts',(-2.21683737410199,-4.00785625340675,
23.2824210823318));
#32572=CARTESIAN_POINT('Ctrl Pts',(-2.80538164796902,-3.54166563180954,
23.2559637856473));
#32573=CARTESIAN_POINT('Ctrl Pts',(-3.39392592183609,-3.0754750102123,23.2295064889628));
#32574=CARTESIAN_POINT('Ctrl Pts',(-3.86375285659963,-2.459409194293,23.2030491922783));
#32575=CARTESIAN_POINT('Ctrl Pts',(-4.15763804857074,-1.76850431465145,
23.1765918955939));
#32576=CARTESIAN_POINT('Ctrl Pts',(-4.45152324054182,-1.07759943500997,
23.1501345989094));
#32577=CARTESIAN_POINT('Ctrl Pts',(-4.56946668972051,-0.311855491646258,
23.123677302225));
#32578=CARTESIAN_POINT('Ctrl Pts',(-4.49710302020607,0.435460743133651,
23.0972200055405));
#32579=CARTESIAN_POINT('Ctrl Pts',(-4.42473935069162,1.18277697791365,23.070762708856));
#32580=CARTESIAN_POINT('Ctrl Pts',(-4.162068562484,1.91166550410983,23.0443054121715));
#32581=CARTESIAN_POINT('Ctrl Pts',(-3.74108365616062,2.53334852003347,23.017848115487));
#32582=CARTESIAN_POINT('Ctrl Pts',(-3.32009874983724,3.15503153595711,22.9913908188026));
#32583=CARTESIAN_POINT('Ctrl Pts',(-2.74079972539808,3.66950904160819,22.9649335221181));
#32584=CARTESIAN_POINT('Ctrl Pts',(-2.07374458313369,4.01411821952858,22.9384762254337));
#32585=CARTESIAN_POINT('Ctrl Pts',(-1.40668944086933,4.35872739744894,22.9120189287492));
#32586=CARTESIAN_POINT('Ctrl Pts',(-0.651878180779734,4.53346824763863,
22.8855616320647));
#32587=CARTESIAN_POINT('Ctrl Pts',(0.0987540592506666,4.51705757827173,
22.8591043353802));
#32588=CARTESIAN_POINT('Ctrl Pts',(0.849386299281067,4.50064690890482,22.8326470386958));
#32589=CARTESIAN_POINT('Ctrl Pts',(1.59583951925228,4.29308471998132,22.8061897420113));
#32590=CARTESIAN_POINT('Ctrl Pts',(2.24719647092532,3.91965176135188,22.7797324453269));
#32591=CARTESIAN_POINT('Ctrl Pts',(2.89855342259837,3.54621880272245,22.7532751486424));
#32592=CARTESIAN_POINT('Ctrl Pts',(3.45481410597325,3.00691507438708,22.7268178519579));
#32593=CARTESIAN_POINT('Ctrl Pts',(3.8482267217168,2.3674273530564,22.7003605552734));
#32594=CARTESIAN_POINT('Ctrl Pts',(4.24163933746037,1.72793963172568,22.673903258589));
#32595=CARTESIAN_POINT('Ctrl Pts',(4.47220388557259,0.988267917399649,22.6474459619045));
#32596=CARTESIAN_POINT('Ctrl Pts',(4.51183760195935,0.238503067401548,22.6209886652201));
#32597=CARTESIAN_POINT('Ctrl Pts',(4.51603475238966,0.159104107382582,22.618186877644));
#32598=CARTESIAN_POINT('Ctrl Pts',(4.51809071117569,0.0795919580082339,
22.615385090068));
#32599=CARTESIAN_POINT('Ctrl Pts',(4.51802736372575,7.65320072124154E-5,
22.612583302492));
#32600=CARTESIAN_POINT('Origin',(0.,0.,20.5));
#32601=CARTESIAN_POINT('',(4.51732076945549,-0.00048196737157627,21.612583302492));
#32602=CARTESIAN_POINT('',(4.51782520267197,0.000113471772791779,21.8874166975081));
#32603=CARTESIAN_POINT('',(4.51775,5.53264807684796E-16,20.5));
#32604=CARTESIAN_POINT('Ctrl Pts',(4.51782520267197,0.000113471772791779,
21.8874166975081));
#32605=CARTESIAN_POINT('Ctrl Pts',(4.51797972979194,0.149530198200455,21.8926808209467));
#32606=CARTESIAN_POINT('Ctrl Pts',(4.51071347097486,0.298931999583376,21.8979449443854));
#32607=CARTESIAN_POINT('Ctrl Pts',(4.49591510340165,0.447583892947329,21.903209067824));
#32608=CARTESIAN_POINT('Ctrl Pts',(4.4215390356869,1.19470300808371,21.9296663645084));
#32609=CARTESIAN_POINT('Ctrl Pts',(4.15689950898611,1.92287920852908,21.9561236611929));
#32610=CARTESIAN_POINT('Ctrl Pts',(3.73423901960025,2.54342464869698,21.9825809578774));
#32611=CARTESIAN_POINT('Ctrl Pts',(3.3115785302144,3.16397008886483,22.0090382545618));
#32612=CARTESIAN_POINT('Ctrl Pts',(2.7308970781435,3.67688476875521,22.0354955512463));
#32613=CARTESIAN_POINT('Ctrl Pts',(2.06291588716907,4.0196945481291,22.0619528479308));
#32614=CARTESIAN_POINT('Ctrl Pts',(1.39493469619467,4.36250432750298,22.0884101446153));
#32615=CARTESIAN_POINT('Ctrl Pts',(0.639653766316767,4.53520920636039,22.1148674412997));
#32616=CARTESIAN_POINT('Ctrl Pts',(-0.110931801888053,4.51677482186132,
22.1413247379842));
#32617=CARTESIAN_POINT('Ctrl Pts',(-0.861517370093001,4.49834043736225,
22.1677820346687));
#32618=CARTESIAN_POINT('Ctrl Pts',(-1.60740757662484,4.28876678950664,22.1942393313531));
#32619=CARTESIAN_POINT('Ctrl Pts',(-2.25775525993264,3.91357923987666,22.2206966280376));
#32620=CARTESIAN_POINT('Ctrl Pts',(-2.90810294324037,3.53839169024672,22.2471539247221));
#32621=CARTESIAN_POINT('Ctrl Pts',(-3.46290810332406,2.99759023884246,22.2736112214065));
#32622=CARTESIAN_POINT('Ctrl Pts',(-3.85459532302061,2.35704415643024,22.300068518091));
#32623=CARTESIAN_POINT('Ctrl Pts',(-4.24628254271713,1.71649807401806,22.3265258147755));
#32624=CARTESIAN_POINT('Ctrl Pts',(-4.4748518220265,0.976207360597959,22.3529831114599));
#32625=CARTESIAN_POINT('Ctrl Pts',(-4.51246407961468,0.226338472032797,
22.3794404081444));
#32626=CARTESIAN_POINT('Ctrl Pts',(-4.55007633720287,-0.523530416532452,
22.4058977048289));
#32627=CARTESIAN_POINT('Ctrl Pts',(-4.39673157306978,-1.28297748024285,
22.4323550015133));
#32628=CARTESIAN_POINT('Ctrl Pts',(-4.07110679585725,-1.95950283641873,
22.4588122981978));
#32629=CARTESIAN_POINT('Ctrl Pts',(-3.74548201864475,-2.63602819259453,
22.4852695948823));
#32630=CARTESIAN_POINT('Ctrl Pts',(-3.24757722835284,-3.22963184123592,
22.5117268915668));
#32631=CARTESIAN_POINT('Ctrl Pts',(-2.63803679068419,-3.66801355240642,
22.5381841882512));
#32632=CARTESIAN_POINT('Ctrl Pts',(-2.02849635301547,-4.10639526357697,
22.5646414849357));
#32633=CARTESIAN_POINT('Ctrl Pts',(-1.30732026797,-4.38955503727659,22.5910987816201));
#32634=CARTESIAN_POINT('Ctrl Pts',(-0.562346924558367,-4.48300430658586,
22.6175560783046));
#32635=CARTESIAN_POINT('Ctrl Pts',(0.182626418853268,-4.57645357589513,
22.6440133749891));
#32636=CARTESIAN_POINT('Ctrl Pts',(0.951397020631046,-4.48019234081406,
22.6704706716736));
#32637=CARTESIAN_POINT('Ctrl Pts',(1.65032944052472,-4.20594512376056,22.696927968358));
#32638=CARTESIAN_POINT('Ctrl Pts',(2.34926186041832,-3.93169790670708,22.7233852650425));
#32639=CARTESIAN_POINT('Ctrl Pts',(2.97835609842781,-3.47946470768123,22.749842561727));
#32640=CARTESIAN_POINT('Ctrl Pts',(3.46098918943069,-2.90432702425209,22.7762998584114));
#32641=CARTESIAN_POINT('Ctrl Pts',(3.94362228043359,-2.32918934082292,22.8027571550959));
#32642=CARTESIAN_POINT('Ctrl Pts',(4.27979422442984,-1.63114717299047,22.8292144517804));
#32643=CARTESIAN_POINT('Ctrl Pts',(4.42855964178011,-0.89522128720241,22.8556717484648));
#32644=CARTESIAN_POINT('Ctrl Pts',(4.48805867336429,-0.600886230695128,
22.8662533981459));
#32645=CARTESIAN_POINT('Ctrl Pts',(4.51757985123852,-0.300491232865703,
22.876835047827));
#32646=CARTESIAN_POINT('Ctrl Pts',(4.51742427980126,-6.60698246896739E-5,
22.8874166975081));
#32647=CARTESIAN_POINT('Ctrl Pts',(4.51802736372575,7.65320072124154E-5,
22.612583302492));
#32648=CARTESIAN_POINT('Ctrl Pts',(4.51749252083047,-0.671272680948583,
22.5889277933835));
#32649=CARTESIAN_POINT('Ctrl Pts',(4.36588431242158,-1.34285546610394,22.5652722842751));
#32650=CARTESIAN_POINT('Ctrl Pts',(4.07637456299432,-1.94852038806885,22.5416167751666));
#32651=CARTESIAN_POINT('Ctrl Pts',(3.75257492298122,-2.62592100787102,22.5151594784822));
#32652=CARTESIAN_POINT('Ctrl Pts',(3.2562727582937,-3.22086426180528,22.4887021817977));
#32653=CARTESIAN_POINT('Ctrl Pts',(2.64791620593777,-3.66088792814019,22.4622448851133));
#32654=CARTESIAN_POINT('Ctrl Pts',(2.03955965358178,-4.10091159447515,22.4357875884288));
#32655=CARTESIAN_POINT('Ctrl Pts',(1.31914871355735,-4.38601567321071,22.4093302917443));
#32656=CARTESIAN_POINT('Ctrl Pts',(0.574430373257849,-4.48147252184727,
22.3828729950598));
#32657=CARTESIAN_POINT('Ctrl Pts',(-0.17028796704161,-4.57692937048383,
22.3564156983754));
#32658=CARTESIAN_POINT('Ctrl Pts',(-0.939313707616121,-4.48273898902142,
22.3299584016909));
#32659=CARTESIAN_POINT('Ctrl Pts',(-1.63898363511379,-4.21037796912979,
22.3035011050064));
#32660=CARTESIAN_POINT('Ctrl Pts',(-2.33865356261146,-3.93801694923817,
22.277043808322));
#32661=CARTESIAN_POINT('Ctrl Pts',(-2.96896767703227,-3.48748529091735,
22.2505865116375));
#32662=CARTESIAN_POINT('Ctrl Pts',(-3.4531482409959,-2.91364911818973,22.224129214953));
#32663=CARTESIAN_POINT('Ctrl Pts',(-3.93732880495957,-2.33981294546208,
22.1976719182685));
#32664=CARTESIAN_POINT('Ctrl Pts',(-4.27537581846602,-1.64267225832765,
22.1712146215841));
#32665=CARTESIAN_POINT('Ctrl Pts',(-4.42612719062429,-0.907153378338295,
22.1447573248996));
#32666=CARTESIAN_POINT('Ctrl Pts',(-4.57687856278254,-0.171634498348981,
22.1183000282152));
#32667=CARTESIAN_POINT('Ctrl Pts',(-4.5403342935926,0.602262574495347,22.0918427315307));
#32668=CARTESIAN_POINT('Ctrl Pts',(-4.32092341583129,1.32030703112007,22.0653854348462));
#32669=CARTESIAN_POINT('Ctrl Pts',(-4.10151253806998,2.03835148774475,22.0389281381617));
#32670=CARTESIAN_POINT('Ctrl Pts',(-3.69923505173734,2.70054332814993,22.0124708414773));
#32671=CARTESIAN_POINT('Ctrl Pts',(-3.16312948534619,3.2261735651419,21.9860135447928));
#32672=CARTESIAN_POINT('Ctrl Pts',(-2.62702391895502,3.7518038021339,21.9595562481083));
#32673=CARTESIAN_POINT('Ctrl Pts',(-1.95709027250536,4.14087243571266,21.9330989514239));
#32674=CARTESIAN_POINT('Ctrl Pts',(-1.23484721910289,4.34609472311248,21.9066416547394));
#32675=CARTESIAN_POINT('Ctrl Pts',(-0.512604165700429,4.5513170105123,21.880184358055));
#32676=CARTESIAN_POINT('Ctrl Pts',(0.261948294654812,4.57269295173318,21.8537270613705));
#32677=CARTESIAN_POINT('Ctrl Pts',(0.994322299916156,4.40742376897541,21.827269764686));
#32678=CARTESIAN_POINT('Ctrl Pts',(1.72669630517754,4.24215458621763,21.8008124680015));
#32679=CARTESIAN_POINT('Ctrl Pts',(2.41689185534501,3.89024027948119,21.7743551713171));
#32680=CARTESIAN_POINT('Ctrl Pts',(2.9811237744369,3.39491220205643,21.7478978746326));
#32681=CARTESIAN_POINT('Ctrl Pts',(3.54535569352876,2.8995841246317,21.7214405779481));
#32682=CARTESIAN_POINT('Ctrl Pts',(3.98362398154505,2.26084227651867,21.6949832812637));
#32683=CARTESIAN_POINT('Ctrl Pts',(4.24201965646871,1.55578891217676,21.6685259845792));
#32684=CARTESIAN_POINT('Ctrl Pts',(4.42414140114732,1.05885509606931,21.6498784238835));
#32685=CARTESIAN_POINT('Ctrl Pts',(4.51690828804801,0.528979877711725,21.6312308631877));
#32686=CARTESIAN_POINT('Ctrl Pts',(4.51732076945549,-0.00048196737157627,
21.612583302492));
#32687=CARTESIAN_POINT('Origin',(0.,0.,20.5));
#32688=CARTESIAN_POINT('',(4.52133925202235,0.00376432143610439,20.612583302492));
#32689=CARTESIAN_POINT('',(4.50983715083838,-0.000439487622834945,20.8874166975081));
#32690=CARTESIAN_POINT('',(4.51775,5.53264807684796E-16,20.5));
#32691=CARTESIAN_POINT('Ctrl Pts',(4.50983715083838,-0.000439487622834945,
20.8874166975081));
#32692=CARTESIAN_POINT('Ctrl Pts',(4.51223989494407,0.600272225419278,20.9085265940664));
#32693=CARTESIAN_POINT('Ctrl Pts',(4.40045147683232,1.20075832380094,20.9296364906248));
#32694=CARTESIAN_POINT('Ctrl Pts',(4.16995632188889,1.7527710518725,20.9507463871831));
#32695=CARTESIAN_POINT('Ctrl Pts',(3.88107386896856,2.44461548985082,20.9772036838676));
#32696=CARTESIAN_POINT('Ctrl Pts',(3.40572780474968,3.06031833788172,21.0036609805521));
#32697=CARTESIAN_POINT('Ctrl Pts',(2.81753981467946,3.528620768205,21.0301182772365));
#32698=CARTESIAN_POINT('Ctrl Pts',(2.22935182460931,3.99692319852822,21.056575573921));
#32699=CARTESIAN_POINT('Ctrl Pts',(1.52832190868785,4.31782521114387,21.0830328706055));
#32700=CARTESIAN_POINT('Ctrl Pts',(0.790149843231595,4.44924273175288,21.1094901672899));
#32701=CARTESIAN_POINT('Ctrl Pts',(0.051977777775257,4.58066025236192,21.1359474639744));
#32702=CARTESIAN_POINT('Ctrl Pts',(-0.723336437215882,4.52259328096428,
21.1624047606589));
#32703=CARTESIAN_POINT('Ctrl Pts',(-1.43588412720356,4.28390166798379,21.1888620573433));
#32704=CARTESIAN_POINT('Ctrl Pts',(-2.14843181719121,4.04521005500332,21.2153193540278));
#32705=CARTESIAN_POINT('Ctrl Pts',(-2.7982129821754,3.62589380044002,21.2417766507123));
#32706=CARTESIAN_POINT('Ctrl Pts',(-3.30902952393807,3.07605344225317,21.2682339473967));
#32707=CARTESIAN_POINT('Ctrl Pts',(-3.81984606570073,2.52621308406631,21.2946912440812));
#32708=CARTESIAN_POINT('Ctrl Pts',(-4.19169798424187,1.84584862225589,21.3211485407657));
#32709=CARTESIAN_POINT('Ctrl Pts',(-4.37772925931563,1.11834540158705,21.3476058374502));
#32710=CARTESIAN_POINT('Ctrl Pts',(-4.56376053438938,0.390842180918212,
21.3740631341346));
#32711=CARTESIAN_POINT('Ctrl Pts',(-4.56397116599575,-0.383799798609046,
21.4005204308191));
#32712=CARTESIAN_POINT('Ctrl Pts',(-4.37916492462626,-1.11150455739398,
21.4269777275035));
#32713=CARTESIAN_POINT('Ctrl Pts',(-4.19435868325677,-1.83920931617892,
21.453435024188));
#32714=CARTESIAN_POINT('Ctrl Pts',(-3.82453556891143,-2.51997685422154,
21.4798923208725));
#32715=CARTESIAN_POINT('Ctrl Pts',(-3.31430027943462,-3.07074498667336,
21.5063496175569));
#32716=CARTESIAN_POINT('Ctrl Pts',(-2.80406498995777,-3.62151311912521,
21.5328069142414));
#32717=CARTESIAN_POINT('Ctrl Pts',(-2.15341752534944,-4.04228184598626,
21.5592642109259));
#32718=CARTESIAN_POINT('Ctrl Pts',(-1.44183871719702,-4.28187903967218,
21.5857215076104));
#32719=CARTESIAN_POINT('Ctrl Pts',(-0.730259909044641,-4.5214762333581,
21.6121788042948));
#32720=CARTESIAN_POINT('Ctrl Pts',(0.0422502426518133,-4.57990189386891,
21.6386361009793));
#32721=CARTESIAN_POINT('Ctrl Pts',(0.781724091400323,-4.44999904027082,
21.6650933976638));
#32722=CARTESIAN_POINT('Ctrl Pts',(1.52119794014883,-4.32009618667273,21.6915506943482));
#32723=CARTESIAN_POINT('Ctrl Pts',(2.2276354859494,-4.00186481896572,21.7180079910327));
#32724=CARTESIAN_POINT('Ctrl Pts',(2.81492815165366,-3.53408677354305,21.7444652877172));
#32725=CARTESIAN_POINT('Ctrl Pts',(3.40222081735796,-3.06630872812035,21.7709225844016));
#32726=CARTESIAN_POINT('Ctrl Pts',(3.87036860296593,-2.44898400498197,21.7973798810861));
#32727=CARTESIAN_POINT('Ctrl Pts',(4.16238619140555,-1.75729062849908,21.8238371777706));
#32728=CARTESIAN_POINT('Ctrl Pts',(4.39630197715038,-1.20322126398217,21.8450303510164));
#32729=CARTESIAN_POINT('Ctrl Pts',(4.51720308199739,-0.601432940640185,
21.8662235242623));
#32730=CARTESIAN_POINT('Ctrl Pts',(4.51782520267197,0.000113471772791779,
21.8874166975081));
#32731=CARTESIAN_POINT('Ctrl Pts',(4.51732076945549,-0.00048196737157627,
21.612583302492));
#32732=CARTESIAN_POINT('Ctrl Pts',(4.51749351971195,-0.222224494111391,
21.6047735665033));
#32733=CARTESIAN_POINT('Ctrl Pts',(4.50146734240306,-0.44389451533626,21.5969638305145));
#32734=CARTESIAN_POINT('Ctrl Pts',(4.46902189478939,-0.663041834113329,
21.5891540945258));
#32735=CARTESIAN_POINT('Ctrl Pts',(4.35910539635538,-1.40545433549076,21.5626967978413));
#32736=CARTESIAN_POINT('Ctrl Pts',(4.06074933765633,-2.11891445767478,21.5362395011569));
#32737=CARTESIAN_POINT('Ctrl Pts',(3.60841564297682,-2.71899122382358,21.5097822044724));
#32738=CARTESIAN_POINT('Ctrl Pts',(3.15608194829734,-3.31906798997234,21.4833249077879));
#32739=CARTESIAN_POINT('Ctrl Pts',(2.54977061763742,-3.80576140008588,21.4568676111035));
#32740=CARTESIAN_POINT('Ctrl Pts',(1.86683275295722,-4.11521969441498,21.430410314419));
#32741=CARTESIAN_POINT('Ctrl Pts',(1.18389488827701,-4.42467798874409,21.4039530177345));
#32742=CARTESIAN_POINT('Ctrl Pts',(0.424330489576522,-4.55690116728877,
21.37749572105));
#32743=CARTESIAN_POINT('Ctrl Pts',(-0.325633495564533,-4.50373822059831,
21.3510384243656));
#32744=CARTESIAN_POINT('Ctrl Pts',(-1.07559748070559,-4.45057527390784,
21.3245811276811));
#32745=CARTESIAN_POINT('Ctrl Pts',(-1.81596105228721,-4.21202620198225,
21.2981238309967));
#32746=CARTESIAN_POINT('Ctrl Pts',(-2.44569775560519,-3.80516814017082,
21.2716665343122));
#32747=CARTESIAN_POINT('Ctrl Pts',(-3.70517116224116,-2.99145201654798,
21.2187519409433));
#32748=CARTESIAN_POINT('Ctrl Pts',(-4.52213709582257,-1.50449993338184,
21.1658373475743));
#32749=CARTESIAN_POINT('Ctrl Pts',(-4.5251392293927,-0.0110172863203392,
21.1129227542054));
#32750=CARTESIAN_POINT('Ctrl Pts',(-4.52814136296284,1.4824653607412,21.0600081608364));
#32751=CARTESIAN_POINT('Ctrl Pts',(-3.71717969652165,2.98247857169809,21.0070935674675));
#32752=CARTESIAN_POINT('Ctrl Pts',(-2.46290199004371,3.79700220422752,20.9541789740986));
#32753=CARTESIAN_POINT('Ctrl Pts',(-1.20862428356581,4.61152583675692,20.9012643807296));
#32754=CARTESIAN_POINT('Ctrl Pts',(0.488969462948824,4.7405598908589,20.8483497873607));
#32755=CARTESIAN_POINT('Ctrl Pts',(1.85305394748095,4.12790602103174,20.7954351939918));
#32756=CARTESIAN_POINT('Ctrl Pts',(3.21713843201311,3.51525215120457,20.7425206006228));
#32757=CARTESIAN_POINT('Ctrl Pts',(4.24771365456276,2.16091035744822,20.6896060072539));
#32758=CARTESIAN_POINT('Ctrl Pts',(4.47332054780559,0.68305737845925,20.636691413885));
#32759=CARTESIAN_POINT('Ctrl Pts',(4.5075830310957,0.458618699879782,20.628655376754));
#32760=CARTESIAN_POINT('Ctrl Pts',(4.52327979691323,0.231331370382945,20.620619339623));
#32761=CARTESIAN_POINT('Ctrl Pts',(4.52133925202235,0.00376432143610439,
20.612583302492));
#32762=CARTESIAN_POINT('Origin',(0.,0.,20.5));
#32763=CARTESIAN_POINT('',(4.51048356578783,0.00141370502139415,19.612583302492));
#32764=CARTESIAN_POINT('',(4.51474283421141,-0.0038924084009401,19.8874166975081));
#32765=CARTESIAN_POINT('',(4.51775,5.53264807684796E-16,20.5));
#32766=CARTESIAN_POINT('Ctrl Pts',(4.51474283421141,-0.00389240840094011,
19.8874166975081));
#32767=CARTESIAN_POINT('Ctrl Pts',(4.50621483686762,1.04654996357473,19.9243723671861));
#32768=CARTESIAN_POINT('Ctrl Pts',(4.14085607956887,2.10234645737149,19.9613280368642));
#32769=CARTESIAN_POINT('Ctrl Pts',(3.4708839066554,2.90334883526624,19.9982837065423));
#32770=CARTESIAN_POINT('Ctrl Pts',(2.51159118088301,4.05025580469952,20.0511982999112));
#32771=CARTESIAN_POINT('Ctrl Pts',(0.927790752426727,4.6747928461432,20.1041128932802));
#32772=CARTESIAN_POINT('Ctrl Pts',(-0.556105607180406,4.49092827001162,
20.1570274866491));
#32773=CARTESIAN_POINT('Ctrl Pts',(-2.04000196678754,4.30706369388004,20.209942080018));
#32774=CARTESIAN_POINT('Ctrl Pts',(-3.42399425754553,3.3147975001732,20.262856673387));
#32775=CARTESIAN_POINT('Ctrl Pts',(-4.07445610293379,1.9687487323051,20.3157712667559));
#32776=CARTESIAN_POINT('Ctrl Pts',(-4.72491794832207,0.622699964436965,
20.3686858601248));
#32777=CARTESIAN_POINT('Ctrl Pts',(-4.64184934834058,-1.07713137759245,
20.4216004534938));
#32778=CARTESIAN_POINT('Ctrl Pts',(-3.86404219126196,-2.3542716484918,20.4745150468627));
#32779=CARTESIAN_POINT('Ctrl Pts',(-3.08623503418336,-3.63141191939111,
20.5274296402316));
#32780=CARTESIAN_POINT('Ctrl Pts',(-1.61368932000766,-4.48586111916038,
20.5803442336006));
#32781=CARTESIAN_POINT('Ctrl Pts',(-0.118635503777389,-4.52427204848619,
20.6332588269695));
#32782=CARTESIAN_POINT('Ctrl Pts',(1.37641831245292,-4.56268297781199,20.6861734203384));
#32783=CARTESIAN_POINT('Ctrl Pts',(2.89398023073781,-3.78505563669429,20.7390880137074));
#32784=CARTESIAN_POINT('Ctrl Pts',(3.73680595955696,-2.55211434826229,20.7920026070763));
#32785=CARTESIAN_POINT('Ctrl Pts',(4.24339242394412,-1.81104612176332,20.8238073038869));
#32786=CARTESIAN_POINT('Ctrl Pts',(4.50621711662441,-0.905486741220779,
20.8556120006975));
#32787=CARTESIAN_POINT('Ctrl Pts',(4.50983715083838,-0.000439487622834945,
20.8874166975081));
#32788=CARTESIAN_POINT('Ctrl Pts',(4.52133925202235,0.00376432143610439,
20.612583302492));
#32789=CARTESIAN_POINT('Ctrl Pts',(4.51050196349347,-1.26712087204873,20.567704746254));
#32790=CARTESIAN_POINT('Ctrl Pts',(3.94958417430038,-2.54673008347757,20.5228261900161));
#32791=CARTESIAN_POINT('Ctrl Pts',(3.00029299713898,-3.38761451526673,20.4779476337781));
#32792=CARTESIAN_POINT('Ctrl Pts',(1.88101998929342,-4.37906926578227,20.4250330404092));
#32793=CARTESIAN_POINT('Ctrl Pts',(0.221835409666229,-4.76061460259175,
20.3721184470403));
#32794=CARTESIAN_POINT('Ctrl Pts',(-1.21815646492133,-4.35804593593179,
20.3192038536714));
#32795=CARTESIAN_POINT('Ctrl Pts',(-2.65814833950885,-3.95547726927185,
20.2662892603024));
#32796=CARTESIAN_POINT('Ctrl Pts',(-3.87894750905677,-2.76879459914251,
20.2133746669335));
#32797=CARTESIAN_POINT('Ctrl Pts',(-4.32195458228653,-1.34081481536639,
20.1604600735645));
#32798=CARTESIAN_POINT('Ctrl Pts',(-4.76496165551631,0.0871649684097867,
20.1075454801956));
#32799=CARTESIAN_POINT('Ctrl Pts',(-4.43017663242789,1.75644186583272,20.0546308868267));
#32800=CARTESIAN_POINT('Ctrl Pts',(-3.47088390665552,2.90334883526609,20.0017162934577));
#32801=CARTESIAN_POINT('Ctrl Pts',(-2.51159118088318,4.05025580469941,19.9488017000888));
#32802=CARTESIAN_POINT('Ctrl Pts',(-0.927790752426926,4.67479284614316,
19.8958871067198));
#32803=CARTESIAN_POINT('Ctrl Pts',(0.556105607180211,4.49092827001165,19.8429725133509));
#32804=CARTESIAN_POINT('Ctrl Pts',(2.04000196678735,4.30706369388013,19.790057919982));
#32805=CARTESIAN_POINT('Ctrl Pts',(3.42399425754539,3.31479750017334,19.737143326613));
#32806=CARTESIAN_POINT('Ctrl Pts',(4.07445610293371,1.96874873230528,19.6842287332441));
#32807=CARTESIAN_POINT('Ctrl Pts',(4.36802741054216,1.36123992961467,19.6603469229934));
#32808=CARTESIAN_POINT('Ctrl Pts',(4.51218113590681,0.681666855829588,19.6364651127427));
#32809=CARTESIAN_POINT('Ctrl Pts',(4.51048356578783,0.00141370502139415,
19.612583302492));
#32810=CARTESIAN_POINT('Origin',(0.,0.,20.5));
#32811=CARTESIAN_POINT('',(4.51751172608841,-5.0340792907555E-5,18.612583302492));
#32812=CARTESIAN_POINT('',(4.52514732618828,-0.0014363825736758,18.8874166975081));
#32813=CARTESIAN_POINT('',(4.51775,5.53264807684796E-16,20.5));
#32814=CARTESIAN_POINT('Ctrl Pts',(4.52514732618828,-0.0014363825736758,
18.8874166975081));
#32815=CARTESIAN_POINT('Ctrl Pts',(4.52467107616349,1.48887736965158,18.9402181403059));
#32816=CARTESIAN_POINT('Ctrl Pts',(3.71449759637046,2.98422031831989,18.9930195831037));
#32817=CARTESIAN_POINT('Ctrl Pts',(2.46290199004355,3.79700220422763,19.0458210259014));
#32818=CARTESIAN_POINT('Ctrl Pts',(1.20862428356557,4.611525836757,19.0987356192704));
#32819=CARTESIAN_POINT('Ctrl Pts',(-0.488969462949119,4.74055989085888,
19.1516502126393));
#32820=CARTESIAN_POINT('Ctrl Pts',(-1.85305394748124,4.12790602103161,19.2045648060083));
#32821=CARTESIAN_POINT('Ctrl Pts',(-3.21713843201331,3.51525215120436,19.2574793993772));
#32822=CARTESIAN_POINT('Ctrl Pts',(-4.24771365456286,2.16091035744797,19.3103939927461));
#32823=CARTESIAN_POINT('Ctrl Pts',(-4.47332054780562,0.683057378459056,
19.3633085861151));
#32824=CARTESIAN_POINT('Ctrl Pts',(-4.69892744104839,-0.794795600529883,
19.416223179484));
#32825=CARTESIAN_POINT('Ctrl Pts',(-4.1195660049844,-2.3961597647514,19.4691377728529));
#32826=CARTESIAN_POINT('Ctrl Pts',(-3.00029299713883,-3.38761451526686,
19.5220523662219));
#32827=CARTESIAN_POINT('Ctrl Pts',(-1.8810199892932,-4.37906926578239,19.5749669595908));
#32828=CARTESIAN_POINT('Ctrl Pts',(-0.221835409665938,-4.76061460259178,
19.6278815529597));
#32829=CARTESIAN_POINT('Ctrl Pts',(1.21815646492164,-4.35804593593171,19.6807961463287));
#32830=CARTESIAN_POINT('Ctrl Pts',(2.6581483395091,-3.95547726927166,19.7337107396976));
#32831=CARTESIAN_POINT('Ctrl Pts',(3.8789475090569,-2.76879459914231,19.7866253330665));
#32832=CARTESIAN_POINT('Ctrl Pts',(4.32195458228659,-1.3408148153662,19.8395399264355));
#32833=CARTESIAN_POINT('Ctrl Pts',(4.45556453043254,-0.910139288059504,
19.8554988501263));
#32834=CARTESIAN_POINT('Ctrl Pts',(4.51842556165299,-0.457515081242471,
19.8714577738172));
#32835=CARTESIAN_POINT('Ctrl Pts',(4.51474283421141,-0.00389240840094011,
19.8874166975081));
#32836=CARTESIAN_POINT('Ctrl Pts',(4.51048356578783,0.00141370502139415,
19.612583302492));
#32837=CARTESIAN_POINT('Ctrl Pts',(4.50841985350745,-0.825560548001291,
19.5835505193738));
#32838=CARTESIAN_POINT('Ctrl Pts',(4.29080360170741,-1.65353988177363,19.5545177362555));
#32839=CARTESIAN_POINT('Ctrl Pts',(3.86404219126206,-2.35427164849163,19.5254849531373));
#32840=CARTESIAN_POINT('Ctrl Pts',(3.08623503418352,-3.63141191939097,19.4725703597684));
#32841=CARTESIAN_POINT('Ctrl Pts',(1.61368932000785,-4.48586111916031,19.4196557663994));
#32842=CARTESIAN_POINT('Ctrl Pts',(0.118635503777585,-4.52427204848618,
19.3667411730305));
#32843=CARTESIAN_POINT('Ctrl Pts',(-1.37641831245272,-4.56268297781205,
19.3138265796616));
#32844=CARTESIAN_POINT('Ctrl Pts',(-2.89398023073765,-3.78505563669441,
19.2609119862926));
#32845=CARTESIAN_POINT('Ctrl Pts',(-3.73680595955685,-2.55211434826245,
19.2079973929237));
#32846=CARTESIAN_POINT('Ctrl Pts',(-4.57963168837605,-1.3191730598305,19.1550827995547));
#32847=CARTESIAN_POINT('Ctrl Pts',(-4.74772122772955,0.369082175915713,
19.1021682061858));
#32848=CARTESIAN_POINT('Ctrl Pts',(-4.16995632188897,1.75277105187232,19.0492536128169));
#32849=CARTESIAN_POINT('Ctrl Pts',(-3.88107386896868,2.44461548985061,19.0227963161324));
#32850=CARTESIAN_POINT('Ctrl Pts',(-3.40572780474986,3.0603183378815,18.9963390194479));
#32851=CARTESIAN_POINT('Ctrl Pts',(-2.81753981467971,3.5286207682048,18.9698817227635));
#32852=CARTESIAN_POINT('Ctrl Pts',(-2.22935182460953,3.99692319852811,18.943424426079));
#32853=CARTESIAN_POINT('Ctrl Pts',(-1.52832190868799,4.31782521114383,18.9169671293945));
#32854=CARTESIAN_POINT('Ctrl Pts',(-0.790149843231659,4.44924273175287,
18.8905098327101));
#32855=CARTESIAN_POINT('Ctrl Pts',(-0.0519777777753676,4.58066025236191,
18.8640525360256));
#32856=CARTESIAN_POINT('Ctrl Pts',(0.72333643721573,4.5225932809643,18.8375952393411));
#32857=CARTESIAN_POINT('Ctrl Pts',(1.43588412720338,4.28390166798386,18.8111379426567));
#32858=CARTESIAN_POINT('Ctrl Pts',(2.14843181719103,4.04521005500342,18.7846806459722));
#32859=CARTESIAN_POINT('Ctrl Pts',(2.79821298217524,3.62589380044014,18.7582233492877));
#32860=CARTESIAN_POINT('Ctrl Pts',(3.30902952393793,3.07605344225331,18.7317660526033));
#32861=CARTESIAN_POINT('Ctrl Pts',(3.81984606570062,2.52621308406647,18.7053087559188));
#32862=CARTESIAN_POINT('Ctrl Pts',(4.19169798424179,1.84584862225607,18.6788514592343));
#32863=CARTESIAN_POINT('Ctrl Pts',(4.37772925931557,1.11834540158724,18.6523941625499));
#32864=CARTESIAN_POINT('Ctrl Pts',(4.47103767181987,0.753448850803234,18.6391238758639));
#32865=CARTESIAN_POINT('Ctrl Pts',(4.51759801973486,0.3766933068382,18.625853589178));
#32866=CARTESIAN_POINT('Ctrl Pts',(4.51751172608841,-5.0340792907555E-5,
18.612583302492));
#32867=CARTESIAN_POINT('Origin',(0.,0.,20.5));
#32868=CARTESIAN_POINT('',(4.51803700570725,7.32895604327321E-5,17.612583302492));
#32869=CARTESIAN_POINT('',(4.51742050630483,-6.62530376704942E-5,17.8874166975081));
#32870=CARTESIAN_POINT('',(4.51775,5.53264807684796E-16,20.5));
#32871=CARTESIAN_POINT('Ctrl Pts',(4.51742050630483,-6.62530376705099E-5,
17.8874166975081));
#32872=CARTESIAN_POINT('Ctrl Pts',(4.5172038153436,0.446598657046559,17.9031493200567));
#32873=CARTESIAN_POINT('Ctrl Pts',(4.4513943616742,0.893327565156709,17.9188819426052));
#32874=CARTESIAN_POINT('Ctrl Pts',(4.32092341583127,1.32030703112013,17.9346145651538));
#32875=CARTESIAN_POINT('Ctrl Pts',(4.10151253806993,2.03835148774488,17.9610718618383));
#32876=CARTESIAN_POINT('Ctrl Pts',(3.6992350517372,2.70054332815014,17.9875291585227));
#32877=CARTESIAN_POINT('Ctrl Pts',(3.16312948534596,3.22617356514213,18.0139864552072));
#32878=CARTESIAN_POINT('Ctrl Pts',(2.62702391895476,3.75180380213408,18.0404437518917));
#32879=CARTESIAN_POINT('Ctrl Pts',(1.95709027250505,4.1408724357128,18.0669010485761));
#32880=CARTESIAN_POINT('Ctrl Pts',(1.23484721910258,4.34609472311257,18.0933583452606));
#32881=CARTESIAN_POINT('Ctrl Pts',(0.51260416570011,4.55131701051233,18.1198156419451));
#32882=CARTESIAN_POINT('Ctrl Pts',(-0.261948294655145,4.57269295173316,
18.1462729386295));
#32883=CARTESIAN_POINT('Ctrl Pts',(-0.994322299916471,4.40742376897534,
18.172730235314));
#32884=CARTESIAN_POINT('Ctrl Pts',(-1.72669630517784,4.24215458621751,18.1991875319985));
#32885=CARTESIAN_POINT('Ctrl Pts',(-2.41689185534529,3.89024027948101,18.225644828683));
#32886=CARTESIAN_POINT('Ctrl Pts',(-2.98112377443714,3.39491220205621,18.2521021253674));
#32887=CARTESIAN_POINT('Ctrl Pts',(-3.54535569352893,2.89958412463147,18.2785594220519));
#32888=CARTESIAN_POINT('Ctrl Pts',(-3.98362398154516,2.26084227651845,18.3050167187363));
#32889=CARTESIAN_POINT('Ctrl Pts',(-4.24201965646877,1.55578891217658,18.3314740154208));
#32890=CARTESIAN_POINT('Ctrl Pts',(-4.50041533139241,0.85073554783464,18.3579313121053));
#32891=CARTESIAN_POINT('Ctrl Pts',(-4.5789383932234,0.0793706672638789,
18.3843886087897));
#32892=CARTESIAN_POINT('Ctrl Pts',(-4.46902189478936,-0.663041834113523,
18.4108459054742));
#32893=CARTESIAN_POINT('Ctrl Pts',(-4.35910539635533,-1.4054543354909,18.4373032021587));
#32894=CARTESIAN_POINT('Ctrl Pts',(-4.06074933765627,-2.11891445767488,
18.4637604988432));
#32895=CARTESIAN_POINT('Ctrl Pts',(-3.60841564297678,-2.71899122382363,
18.4902177955276));
#32896=CARTESIAN_POINT('Ctrl Pts',(-3.15608194829727,-3.31906798997241,
18.5166750922121));
#32897=CARTESIAN_POINT('Ctrl Pts',(-2.54977061763729,-3.80576140008597,
18.5431323888965));
#32898=CARTESIAN_POINT('Ctrl Pts',(-1.86683275295704,-4.11521969441507,
18.569589685581));
#32899=CARTESIAN_POINT('Ctrl Pts',(-1.18389488827682,-4.42467798874415,
18.5960469822655));
#32900=CARTESIAN_POINT('Ctrl Pts',(-0.424330489576326,-4.55690116728879,
18.62250427895));
#32901=CARTESIAN_POINT('Ctrl Pts',(0.325633495564726,-4.5037382205983,18.6489615756344));
#32902=CARTESIAN_POINT('Ctrl Pts',(1.07559748070578,-4.4505752739078,18.6754188723189));
#32903=CARTESIAN_POINT('Ctrl Pts',(1.8159610522874,-4.21202620198217,18.7018761690034));
#32904=CARTESIAN_POINT('Ctrl Pts',(2.44569775560536,-3.80516814017072,18.7283334656878));
#32905=CARTESIAN_POINT('Ctrl Pts',(3.70517116224129,-2.99145201654782,18.7812480590567));
#32906=CARTESIAN_POINT('Ctrl Pts',(4.52213709582263,-1.50449993338164,18.8341626524257));
#32907=CARTESIAN_POINT('Ctrl Pts',(4.5251392293927,-0.0110172863201459,
18.8870772457947));
#32908=CARTESIAN_POINT('Ctrl Pts',(4.52514564904193,-0.00782367934410926,
18.8871903963658));
#32909=CARTESIAN_POINT('Ctrl Pts',(4.52514834676573,-0.00463004250646042,
18.887303546937));
#32910=CARTESIAN_POINT('Ctrl Pts',(4.52514732618828,-0.00143638257367575,
18.8874166975081));
#32911=CARTESIAN_POINT('Ctrl Pts',(4.51751172608841,-5.0340792907555E-5,
18.612583302492));
#32912=CARTESIAN_POINT('Ctrl Pts',(4.51742597397124,-0.374429761958339,
18.5993962924935));
#32913=CARTESIAN_POINT('Ctrl Pts',(4.47127719829474,-0.748797435630456,
18.586209282495));
#32914=CARTESIAN_POINT('Ctrl Pts',(4.37916492462631,-1.11150455739379,18.5730222724965));
#32915=CARTESIAN_POINT('Ctrl Pts',(4.19435868325684,-1.83920931617878,18.546564975812));
#32916=CARTESIAN_POINT('Ctrl Pts',(3.8245355689115,-2.51997685422145,18.5201076791275));
#32917=CARTESIAN_POINT('Ctrl Pts',(3.31430027943466,-3.07074498667331,18.493650382443));
#32918=CARTESIAN_POINT('Ctrl Pts',(2.80406498995785,-3.62151311912514,18.4671930857586));
#32919=CARTESIAN_POINT('Ctrl Pts',(2.15341752534957,-4.04228184598617,18.4407357890741));
#32920=CARTESIAN_POINT('Ctrl Pts',(1.4418387171972,-4.28187903967212,18.4142784923896));
#32921=CARTESIAN_POINT('Ctrl Pts',(0.730259909044834,-4.52147623335806,
18.3878211957052));
#32922=CARTESIAN_POINT('Ctrl Pts',(-0.0422502426516132,-4.57990189386892,
18.3613638990207));
#32923=CARTESIAN_POINT('Ctrl Pts',(-0.781724091400131,-4.44999904027085,
18.3349066023362));
#32924=CARTESIAN_POINT('Ctrl Pts',(-1.52119794014869,-4.32009618667279,
18.3084493056518));
#32925=CARTESIAN_POINT('Ctrl Pts',(-2.2276354859493,-4.00186481896578,18.2819920089673));
#32926=CARTESIAN_POINT('Ctrl Pts',(-2.81492815165361,-3.53408677354309,
18.2555347122828));
#32927=CARTESIAN_POINT('Ctrl Pts',(-3.40222081735788,-3.06630872812042,
18.2290774155984));
#32928=CARTESIAN_POINT('Ctrl Pts',(-3.87036860296584,-2.4489840049821,18.2026201189139));
#32929=CARTESIAN_POINT('Ctrl Pts',(-4.16238619140547,-1.75729062849926,
18.1761628222294));
#32930=CARTESIAN_POINT('Ctrl Pts',(-4.45440377984509,-1.06559725201643,
18.149705525545));
#32931=CARTESIAN_POINT('Ctrl Pts',(-4.57029117111638,-0.299535222189059,
18.1232482288605));
#32932=CARTESIAN_POINT('Ctrl Pts',(-4.49591510340165,0.447583892947263,
18.096790932176));
#32933=CARTESIAN_POINT('Ctrl Pts',(-4.42153903568692,1.19470300808361,18.0703336354916));
#32934=CARTESIAN_POINT('Ctrl Pts',(-4.15689950898618,1.92287920852894,18.0438763388071));
#32935=CARTESIAN_POINT('Ctrl Pts',(-3.73423901960036,2.54342464869681,18.0174190421226));
#32936=CARTESIAN_POINT('Ctrl Pts',(-3.31157853021454,3.16397008886469,17.9909617454381));
#32937=CARTESIAN_POINT('Ctrl Pts',(-2.73089707814366,3.67688476875509,17.9645044487537));
#32938=CARTESIAN_POINT('Ctrl Pts',(-2.06291588716924,4.01969454812901,17.9380471520692));
#32939=CARTESIAN_POINT('Ctrl Pts',(-1.39493469619478,4.36250432750296,17.9115898553848));
#32940=CARTESIAN_POINT('Ctrl Pts',(-0.639653766316788,4.53520920636039,
17.8851325587003));
#32941=CARTESIAN_POINT('Ctrl Pts',(0.110931801888114,4.51677482186132,17.8586752620158));
#32942=CARTESIAN_POINT('Ctrl Pts',(0.861517370092973,4.49834043736224,17.8322179653313));
#32943=CARTESIAN_POINT('Ctrl Pts',(1.60740757662473,4.28876678950667,17.8057606686469));
#32944=CARTESIAN_POINT('Ctrl Pts',(2.25775525993247,3.91357923987676,17.7793033719624));
#32945=CARTESIAN_POINT('Ctrl Pts',(2.90810294324022,3.53839169024685,17.7528460752779));
#32946=CARTESIAN_POINT('Ctrl Pts',(3.46290810332394,2.99759023884261,17.7263887785935));
#32947=CARTESIAN_POINT('Ctrl Pts',(3.8545953230205,2.35704415643041,17.699931481909));
#32948=CARTESIAN_POINT('Ctrl Pts',(4.24628254271708,1.71649807401819,17.6734741852245));
#32949=CARTESIAN_POINT('Ctrl Pts',(4.47485182202649,0.976207360598019,17.6470168885401));
#32950=CARTESIAN_POINT('Ctrl Pts',(4.51246407961468,0.226338472032798,17.6205595918556));
#32951=CARTESIAN_POINT('Ctrl Pts',(4.51624383400808,0.150982181084616,17.6179008287344));
#32952=CARTESIAN_POINT('Ctrl Pts',(4.5180951579083,0.0755291623761646,17.6152420656132));
#32953=CARTESIAN_POINT('Ctrl Pts',(4.51803700570725,7.32895604327322E-5,
17.612583302492));
#32954=CARTESIAN_POINT('Origin',(0.,0.,20.5));
#32955=CARTESIAN_POINT('',(4.51759135405446,-0.000109312323752775,16.612583302492));
#32956=CARTESIAN_POINT('',(4.51783748975292,0.000112199089269072,16.8874166975081));
#32957=CARTESIAN_POINT('',(4.51775,5.53264807684796E-16,20.5));
#32958=CARTESIAN_POINT('Ctrl Pts',(4.51783748975292,0.000112199089269072,
16.8874166975081));
#32959=CARTESIAN_POINT('Ctrl Pts',(4.5179865637855,0.145467881021208,16.8925377964919));
#32960=CARTESIAN_POINT('Ctrl Pts',(4.51110979946378,0.290809516813962,16.8976588954757));
#32961=CARTESIAN_POINT('Ctrl Pts',(4.49710302020602,0.435460743134165,16.9027799944596));
#32962=CARTESIAN_POINT('Ctrl Pts',(4.42473935069149,1.18277697791411,16.929237291144));
#32963=CARTESIAN_POINT('Ctrl Pts',(4.16206856248382,1.91166550411022,16.9556945878285));
#32964=CARTESIAN_POINT('Ctrl Pts',(3.7410836561604,2.53334852003379,16.9821518845129));
#32965=CARTESIAN_POINT('Ctrl Pts',(3.320098749837,3.15503153595733,17.0086091811974));
#32966=CARTESIAN_POINT('Ctrl Pts',(2.74079972539787,3.66950904160833,17.0350664778819));
#32967=CARTESIAN_POINT('Ctrl Pts',(2.07374458313351,4.01411821952866,17.0615237745663));
#32968=CARTESIAN_POINT('Ctrl Pts',(1.40668944086914,4.358727397449,17.0879810712508));
#32969=CARTESIAN_POINT('Ctrl Pts',(0.651878180779539,4.53346824763866,17.1144383679353));
#32970=CARTESIAN_POINT('Ctrl Pts',(-0.0987540592508608,4.51705757827172,
17.1408956646198));
#32971=CARTESIAN_POINT('Ctrl Pts',(-0.849386299281262,4.50064690890479,
17.1673529613042));
#32972=CARTESIAN_POINT('Ctrl Pts',(-1.59583951925246,4.29308471998125,17.1938102579887));
#32973=CARTESIAN_POINT('Ctrl Pts',(-2.24719647092549,3.91965176135179,17.2202675546731));
#32974=CARTESIAN_POINT('Ctrl Pts',(-2.89855342259852,3.54621880272232,17.2467248513576));
#32975=CARTESIAN_POINT('Ctrl Pts',(-3.45481410597338,3.00691507438693,17.2731821480421));
#32976=CARTESIAN_POINT('Ctrl Pts',(-3.8482267217169,2.36742735305624,17.2996394447266));
#32977=CARTESIAN_POINT('Ctrl Pts',(-4.24163933746045,1.7279396317255,17.326096741411));
#32978=CARTESIAN_POINT('Ctrl Pts',(-4.47220388557264,0.988267917399458,
17.3525540380955));
#32979=CARTESIAN_POINT('Ctrl Pts',(-4.51183760195937,0.238503067401354,
17.37901133478));
#32980=CARTESIAN_POINT('Ctrl Pts',(-4.55147131834609,-0.511261782596708,
17.4054686314644));
#32981=CARTESIAN_POINT('Ctrl Pts',(-4.40017420300738,-1.27111976826683,
17.4319259281489));
#32982=CARTESIAN_POINT('Ctrl Pts',(-4.07637456299423,-1.94852038806902,
17.4583832248334));
#32983=CARTESIAN_POINT('Ctrl Pts',(-3.75257492298108,-2.62592100787122,
17.4848405215178));
#32984=CARTESIAN_POINT('Ctrl Pts',(-3.25627275829351,-3.22086426180549,
17.5112978182023));
#32985=CARTESIAN_POINT('Ctrl Pts',(-2.64791620593751,-3.66088792814038,
17.5377551148868));
#32986=CARTESIAN_POINT('Ctrl Pts',(-2.0395596535815,-4.10091159447528,17.5642124115712));
#32987=CARTESIAN_POINT('Ctrl Pts',(-1.31914871355708,-4.38601567321079,
17.5906697082557));
#32988=CARTESIAN_POINT('Ctrl Pts',(-0.574430373257593,-4.48147252184731,
17.6171270049402));
#32989=CARTESIAN_POINT('Ctrl Pts',(0.17028796704189,-4.57692937048383,17.6435843016246));
#32990=CARTESIAN_POINT('Ctrl Pts',(0.939313707616428,-4.48273898902136,
17.6700415983091));
#32991=CARTESIAN_POINT('Ctrl Pts',(1.63898363511409,-4.21037796912968,17.6964988949936));
#32992=CARTESIAN_POINT('Ctrl Pts',(2.33865356261174,-3.93801694923801,17.7229561916781));
#32993=CARTESIAN_POINT('Ctrl Pts',(2.96896767703252,-3.48748529091713,17.7494134883625));
#32994=CARTESIAN_POINT('Ctrl Pts',(3.45314824099611,-2.91364911818949,17.775870785047));
#32995=CARTESIAN_POINT('Ctrl Pts',(3.9373288049597,-2.33981294546184,17.8023280817315));
#32996=CARTESIAN_POINT('Ctrl Pts',(4.27537581846611,-1.64267225832742,17.8287853784159));
#32997=CARTESIAN_POINT('Ctrl Pts',(4.42612719062433,-0.907153378338104,
17.8552426751004));
#32998=CARTESIAN_POINT('Ctrl Pts',(4.48723544976425,-0.609004992176015,
17.8659673492363));
#32999=CARTESIAN_POINT('Ctrl Pts',(4.51756822102564,-0.304550492318464,
17.8766920233722));
#33000=CARTESIAN_POINT('Ctrl Pts',(4.51742050630483,-6.62530376704943E-5,
17.8874166975081));
#33001=CARTESIAN_POINT('Ctrl Pts',(4.51803700570725,7.32895604327322E-5,
17.612583302492));
#33002=CARTESIAN_POINT('Ctrl Pts',(4.5175164865615,-0.675330663287972,17.5887847689287));
#33003=CARTESIAN_POINT('Ctrl Pts',(4.36400868534142,-1.35096328729663,17.5649862353655));
#33004=CARTESIAN_POINT('Ctrl Pts',(4.07110679585739,-1.95950283641844,17.5411877018022));
#33005=CARTESIAN_POINT('Ctrl Pts',(3.74548201864491,-2.63602819259433,17.5147304051177));
#33006=CARTESIAN_POINT('Ctrl Pts',(3.24757722835295,-3.22963184123583,17.4882731084333));
#33007=CARTESIAN_POINT('Ctrl Pts',(2.63803679068424,-3.66801355240638,17.4618158117488));
#33008=CARTESIAN_POINT('Ctrl Pts',(2.02849635301557,-4.10639526357692,17.4353585150643));
#33009=CARTESIAN_POINT('Ctrl Pts',(1.30732026797015,-4.38955503727653,17.4089012183799));
#33010=CARTESIAN_POINT('Ctrl Pts',(0.562346924558562,-4.48300430658583,
17.3824439216954));
#33011=CARTESIAN_POINT('Ctrl Pts',(-0.182626418853022,-4.57645357589513,
17.3559866250109));
#33012=CARTESIAN_POINT('Ctrl Pts',(-0.95139702063077,-4.48019234081411,
17.3295293283265));
#33013=CARTESIAN_POINT('Ctrl Pts',(-1.65032944052442,-4.20594512376068,
17.303072031642));
#33014=CARTESIAN_POINT('Ctrl Pts',(-2.34926186041808,-3.93169790670724,
17.2766147349575));
#33015=CARTESIAN_POINT('Ctrl Pts',(-2.97835609842763,-3.47946470768139,
17.2501574382731));
#33016=CARTESIAN_POINT('Ctrl Pts',(-3.46098918943056,-2.90432702425224,
17.2237001415886));
#33017=CARTESIAN_POINT('Ctrl Pts',(-3.94362228043348,-2.32918934082309,
17.1972428449041));
#33018=CARTESIAN_POINT('Ctrl Pts',(-4.27979422442977,-1.63114717299066,
17.1707855482197));
#33019=CARTESIAN_POINT('Ctrl Pts',(-4.42855964178007,-0.895221287202602,
17.1443282515352));
#33020=CARTESIAN_POINT('Ctrl Pts',(-4.57732505913038,-0.159295401414506,
17.1178709548507));
#33021=CARTESIAN_POINT('Ctrl Pts',(-4.53868394983468,0.614514202329214,
17.0914136581662));
#33022=CARTESIAN_POINT('Ctrl Pts',(-4.31734276296002,1.33195837225454,17.0649563614818));
#33023=CARTESIAN_POINT('Ctrl Pts',(-4.09600157608536,2.04940254217985,17.0384990647973));
#33024=CARTESIAN_POINT('Ctrl Pts',(-3.69196031163174,2.71048127828677,17.0120417681128));
#33025=CARTESIAN_POINT('Ctrl Pts',(-3.15443074594472,3.23467592132634,16.9855844714284));
#33026=CARTESIAN_POINT('Ctrl Pts',(-2.61690118025774,3.75887056436587,16.9591271747439));
#33027=CARTESIAN_POINT('Ctrl Pts',(-1.94588331333737,4.14618111433807,16.9326698780594));
#33028=CARTESIAN_POINT('Ctrl Pts',(-1.223106380062,4.3494335753433,16.906212581375));
#33029=CARTESIAN_POINT('Ctrl Pts',(-0.500329446786581,4.55268603634855,
16.8797552846905));
#33030=CARTESIAN_POINT('Ctrl Pts',(0.274206552843852,4.57188040838682,16.853297988006));
#33031=CARTESIAN_POINT('Ctrl Pts',(1.00616399197863,4.40467883795473,16.8268406913216));
#33032=CARTESIAN_POINT('Ctrl Pts',(1.73812143111341,4.23747726752264,16.8003833946371));
#33033=CARTESIAN_POINT('Ctrl Pts',(2.42750030975254,3.88387975462018,16.7739260979526));
#33034=CARTESIAN_POINT('Ctrl Pts',(2.99033504306357,3.38695408510442,16.7474688012682));
#33035=CARTESIAN_POINT('Ctrl Pts',(3.55316977637459,2.89002841558867,16.7210115045837));
#33036=CARTESIAN_POINT('Ctrl Pts',(3.98946036435752,2.24977458945961,16.6945542078992));
#33037=CARTESIAN_POINT('Ctrl Pts',(4.24606709644911,1.54417481408576,16.6680969112148));
#33038=CARTESIAN_POINT('Ctrl Pts',(4.42554078305754,1.05067025197154,16.6495923749738));
#33039=CARTESIAN_POINT('Ctrl Pts',(4.51711737210933,0.525199995180907,16.6310878387329));
#33040=CARTESIAN_POINT('Ctrl Pts',(4.51759135405446,-0.000109312323752775,
16.612583302492));
#33041=CARTESIAN_POINT('Origin',(0.,0.,20.5));
#33042=CARTESIAN_POINT('',(4.51759608459634,0.0001098887360651,15.612583302492));
#33043=CARTESIAN_POINT('',(4.5178043285159,-0.000114763987914418,15.8874166975081));
#33044=CARTESIAN_POINT('',(4.51775,5.53264807684796E-16,20.5));
#33045=CARTESIAN_POINT('Ctrl Pts',(4.5178043285159,-0.000114763987914418,
15.8874166975081));
#33046=CARTESIAN_POINT('Ctrl Pts',(4.51719021324072,0.595015005655344,15.9083835696116));
#33047=CARTESIAN_POINT('Ctrl Pts',(4.39892963080694,1.19038158256103,15.9293504417152));
#33048=CARTESIAN_POINT('Ctrl Pts',(4.16984886166331,1.73951778234083,15.9503173138187));
#33049=CARTESIAN_POINT('Ctrl Pts',(3.88078057126651,2.43245182066608,15.9767746105032));
#33050=CARTESIAN_POINT('Ctrl Pts',(3.41525380642348,3.05177344176931,16.0032319071877));
#33051=CARTESIAN_POINT('Ctrl Pts',(2.82996921187389,3.52204995762958,16.0296892038721));
#33052=CARTESIAN_POINT('Ctrl Pts',(2.2446846173243,3.99232647348986,16.0561465005566));
#33053=CARTESIAN_POINT('Ctrl Pts',(1.53964219306814,4.3135578841072,16.082603797241));
#33054=CARTESIAN_POINT('Ctrl Pts',(0.800715326097207,4.44661855917225,16.1090610939255));
#33055=CARTESIAN_POINT('Ctrl Pts',(0.0617884591262693,4.57967923423731,
16.13551839061));
#33056=CARTESIAN_POINT('Ctrl Pts',(-0.711022850559448,4.52456917375008,
16.1619756872944));
#33057=CARTESIAN_POINT('Ctrl Pts',(-1.42359104075325,4.28800072211039,16.1884329839789));
#33058=CARTESIAN_POINT('Ctrl Pts',(-2.13615923094709,4.0514322704707,16.2148902806634));
#33059=CARTESIAN_POINT('Ctrl Pts',(-2.788484301649,3.63340542767853,16.2413475773478));
#33060=CARTESIAN_POINT('Ctrl Pts',(-3.30111378116087,3.08483540049633,16.2678048740323));
#33061=CARTESIAN_POINT('Ctrl Pts',(-3.81374326067272,2.53626537331417,16.2942621707168));
#33062=CARTESIAN_POINT('Ctrl Pts',(-4.18667714899455,1.857152161742,16.3207194674013));
#33063=CARTESIAN_POINT('Ctrl Pts',(-4.37449251133268,1.1302110034409,16.3471767640857));
#33064=CARTESIAN_POINT('Ctrl Pts',(-4.56230787367082,0.403269845139789,
16.3736340607702));
#33065=CARTESIAN_POINT('Ctrl Pts',(-4.56500471002526,-0.371499259890255,
16.4000913574546));
#33066=CARTESIAN_POINT('Ctrl Pts',(-4.38225454858744,-1.09973029228273,
16.4265486541391));
#33067=CARTESIAN_POINT('Ctrl Pts',(-4.19950438714961,-1.82796132467523,
16.4530059508236));
#33068=CARTESIAN_POINT('Ctrl Pts',(-3.8313072279195,-2.50965428443015,16.4794632475081));
#33069=CARTESIAN_POINT('Ctrl Pts',(-3.3225090776326,-3.06177972318871,16.5059205441925));
#33070=CARTESIAN_POINT('Ctrl Pts',(-2.81371092734571,-3.61390516194727,
16.532377840877));
#33071=CARTESIAN_POINT('Ctrl Pts',(-2.16431178600201,-4.03646307970946,
16.5588351375615));
#33072=CARTESIAN_POINT('Ctrl Pts',(-1.45340774986022,-4.27798639033812,
16.5852924342459));
#33073=CARTESIAN_POINT('Ctrl Pts',(-0.742503713718461,-4.51950970096678,
16.6117497309304));
#33074=CARTESIAN_POINT('Ctrl Pts',(0.0299052172213853,-4.5799984044619,
16.6382070276149));
#33075=CARTESIAN_POINT('Ctrl Pts',(0.769740489176569,-4.45208504257185,
16.6646643242993));
#33076=CARTESIAN_POINT('Ctrl Pts',(1.50957576113175,-4.32417168068181,16.6911216209838));
#33077=CARTESIAN_POINT('Ctrl Pts',(2.21683737410228,-4.00785625340658,16.7175789176683));
#33078=CARTESIAN_POINT('Ctrl Pts',(2.80538164796928,-3.54166563180933,16.7440362143527));
#33079=CARTESIAN_POINT('Ctrl Pts',(3.39392592183629,-3.07547501021207,16.7704935110372));
#33080=CARTESIAN_POINT('Ctrl Pts',(3.86375285659978,-2.45940919429276,16.7969508077217));
#33081=CARTESIAN_POINT('Ctrl Pts',(4.15763804857084,-1.76850431465121,16.8234081044061));
#33082=CARTESIAN_POINT('Ctrl Pts',(4.39463854911208,-1.21133162689784,16.8447443021068));
#33083=CARTESIAN_POINT('Ctrl Pts',(4.51721639786597,-0.605487805208481,
16.8660804998074));
#33084=CARTESIAN_POINT('Ctrl Pts',(4.51783748975292,0.000112199089269072,
16.8874166975081));
#33085=CARTESIAN_POINT('Ctrl Pts',(4.51759135405446,-0.000109312323752775,
16.612583302492));
#33086=CARTESIAN_POINT('Ctrl Pts',(4.51779505896309,-0.225873364281351,
16.6046305420484));
#33087=CARTESIAN_POINT('Ctrl Pts',(4.50117162820754,-0.451607688050524,
16.5966777816049));
#33088=CARTESIAN_POINT('Ctrl Pts',(4.46746660375751,-0.674762023706868,
16.5887250211614));
#33089=CARTESIAN_POINT('Ctrl Pts',(4.35533650277404,-1.417153361507,16.5622677244769));
#33090=CARTESIAN_POINT('Ctrl Pts',(4.05415342460685,-2.1309903124886,16.5358104277924));
#33091=CARTESIAN_POINT('Ctrl Pts',(3.60060113490314,-2.72932832606603,16.509353131108));
#33092=CARTESIAN_POINT('Ctrl Pts',(3.14704884519943,-3.32766633964346,16.4828958344235));
#33093=CARTESIAN_POINT('Ctrl Pts',(2.54112734395919,-3.81050541581671,16.456438537739));
#33094=CARTESIAN_POINT('Ctrl Pts',(1.85663719941204,-4.1190362894713,16.4299812410546));
#33095=CARTESIAN_POINT('Ctrl Pts',(1.17214705486486,-4.4275671631259,16.4035239443701));
#33096=CARTESIAN_POINT('Ctrl Pts',(0.409088267010757,-4.56178983426182,
16.3770666476856));
#33097=CARTESIAN_POINT('Ctrl Pts',(-0.33959944827516,-4.50535613008826,
16.3506093510012));
#33098=CARTESIAN_POINT('Ctrl Pts',(-1.08828716356108,-4.4489224259147,16.3241520543167));
#33099=CARTESIAN_POINT('Ctrl Pts',(-1.82260380627881,-4.20183234643166,
16.2976947576322));
#33100=CARTESIAN_POINT('Ctrl Pts',(-2.45311042204468,-3.79418118985514,
16.2712374609477));
#33101=CARTESIAN_POINT('Ctrl Pts',(-3.08361703781053,-3.38653003327864,
16.2447801642633));
#33102=CARTESIAN_POINT('Ctrl Pts',(-3.61031362662454,-2.81831779960867,
16.2183228675788));
#33103=CARTESIAN_POINT('Ctrl Pts',(-3.96904912687637,-2.15875211004946,
16.1918655708943));
#33104=CARTESIAN_POINT('Ctrl Pts',(-4.3277846271282,-1.49918642049025,16.1654082742099));
#33105=CARTESIAN_POINT('Ctrl Pts',(-4.51855903881786,-0.748267275041791,
16.1389509775254));
#33106=CARTESIAN_POINT('Ctrl Pts',(-4.51813624973985,0.00254420544672257,
16.1124936808409));
#33107=CARTESIAN_POINT('Ctrl Pts',(-4.51771346066184,0.753355685935258,
16.0860363841565));
#33108=CARTESIAN_POINT('Ctrl Pts',(-4.32609347081614,1.50405950146385,16.059579087472));
#33109=CARTESIAN_POINT('Ctrl Pts',(-3.96661538289292,2.16322075812806,16.0331217907875));
#33110=CARTESIAN_POINT('Ctrl Pts',(-3.6071372949697,2.82238201479228,16.0066644941031));
#33111=CARTESIAN_POINT('Ctrl Pts',(-3.07980110896895,3.39000071259211,15.9802071974186));
#33112=CARTESIAN_POINT('Ctrl Pts',(-2.4488357887268,3.7969415223371,15.9537499007341));
#33113=CARTESIAN_POINT('Ctrl Pts',(-1.81787046848466,4.20388233208208,15.9272926040497));
#33114=CARTESIAN_POINT('Ctrl Pts',(-1.08327601400112,4.45014525377221,15.9008353073652));
#33115=CARTESIAN_POINT('Ctrl Pts',(-0.334525216833305,4.50573573609241,
15.8743780106807));
#33116=CARTESIAN_POINT('Ctrl Pts',(0.41422558033451,4.5613262184126,15.8479207139963));
#33117=CARTESIAN_POINT('Ctrl Pts',(1.1771327201866,4.42624426136285,15.8214634173118));
#33118=CARTESIAN_POINT('Ctrl Pts',(1.86127495742196,4.11694269781245,15.7950061206273));
#33119=CARTESIAN_POINT('Ctrl Pts',(2.54541719465734,3.80764113426205,15.7685488239429));
#33120=CARTESIAN_POINT('Ctrl Pts',(3.15079452927597,3.32411996421099,15.7420915272584));
#33121=CARTESIAN_POINT('Ctrl Pts',(3.60367267191142,2.72527153104349,15.7156342305739));
#33122=CARTESIAN_POINT('Ctrl Pts',(4.05655081454687,2.12642309787598,15.6891769338895));
#33123=CARTESIAN_POINT('Ctrl Pts',(4.35692976519912,1.41224740159204,15.662719637205));
#33124=CARTESIAN_POINT('Ctrl Pts',(4.46822370011744,0.669730251598505,15.6362623405205));
#33125=CARTESIAN_POINT('Ctrl Pts',(4.50142605066627,0.448214903788299,15.6283693278443));
#33126=CARTESIAN_POINT('Ctrl Pts',(4.51779965427679,0.224177139537577,15.6204763151682));
#33127=CARTESIAN_POINT('Ctrl Pts',(4.51759608459634,0.0001098887360651,
15.612583302492));
#33128=CARTESIAN_POINT('Origin',(0.,0.,20.5));
#33129=CARTESIAN_POINT('',(4.51803303654689,-7.46219232266102E-5,14.612583302492));
#33130=CARTESIAN_POINT('',(4.51743493951217,7.09613961932946E-5,14.8874166975081));
#33131=CARTESIAN_POINT('',(4.51775,5.53264807684796E-16,20.5));
#33132=CARTESIAN_POINT('Ctrl Pts',(4.51743493951217,7.09613961932946E-5,
14.8874166975081));
#33133=CARTESIAN_POINT('Ctrl Pts',(4.51759894908653,0.294069189408427,14.8977720460469));
#33134=CARTESIAN_POINT('Ctrl Pts',(4.48933542297813,0.588036293354993,14.9081273945857));
#33135=CARTESIAN_POINT('Ctrl Pts',(4.43233806206614,0.876322399438229,14.9184827431245));
#33136=CARTESIAN_POINT('Ctrl Pts',(4.2867132110791,1.61287617260017,14.9449400398089));
#33137=CARTESIAN_POINT('Ctrl Pts',(3.95352194255086,2.31234598448206,14.9713973364934));
#33138=CARTESIAN_POINT('Ctrl Pts',(3.47334658423498,2.88953718612178,14.9978546331779));
#33139=CARTESIAN_POINT('Ctrl Pts',(2.99317122591908,3.46672838776151,15.0243119298623));
#33140=CARTESIAN_POINT('Ctrl Pts',(2.36601177781554,3.92164097915906,15.0507692265468));
#33141=CARTESIAN_POINT('Ctrl Pts',(1.6682555666064,4.19886711014818,15.0772265232313));
#33142=CARTESIAN_POINT('Ctrl Pts',(0.97049935539727,4.4760932411373,15.1036838199157));
#33143=CARTESIAN_POINT('Ctrl Pts',(0.20214638108255,4.57563291171798,15.1301411166002));
#33144=CARTESIAN_POINT('Ctrl Pts',(-0.543218814426446,4.48536230017716,
15.1565984132847));
#33145=CARTESIAN_POINT('Ctrl Pts',(-1.28858400993542,4.39509168863634,15.1830557099691));
#33146=CARTESIAN_POINT('Ctrl Pts',(-2.01096142663867,4.11501079497402,15.2095130066536));
#33147=CARTESIAN_POINT('Ctrl Pts',(-2.6223662946594,3.67923316206403,15.2359703033381));
#33148=CARTESIAN_POINT('Ctrl Pts',(-3.23377116268013,3.24345552915403,15.2624276000225));
#33149=CARTESIAN_POINT('Ctrl Pts',(-3.73420348201834,2.65198115699635,15.288884896707));
#33150=CARTESIAN_POINT('Ctrl Pts',(-4.06271115002269,1.9768509695166,15.3153421933915));
#33151=CARTESIAN_POINT('Ctrl Pts',(-4.39121881802704,1.30172078203686,15.3417994900759));
#33152=CARTESIAN_POINT('Ctrl Pts',(-4.54780183469754,0.542934779235054,
15.3682567867604));
#33153=CARTESIAN_POINT('Ctrl Pts',(-4.51338856189906,-0.207087743519677,
15.3947140834449));
#33154=CARTESIAN_POINT('Ctrl Pts',(-4.47897528910057,-0.957110266274451,
15.4211713801293));
#33155=CARTESIAN_POINT('Ctrl Pts',(-4.2535657268331,-1.69836930898215,15.4476286768138));
#33156=CARTESIAN_POINT('Ctrl Pts',(-3.86461451031294,-2.34058034061557,
15.4740859734983));
#33157=CARTESIAN_POINT('Ctrl Pts',(-3.4756632937928,-2.98279137224897,15.5005432701827));
#33158=CARTESIAN_POINT('Ctrl Pts',(-2.92317042302,-3.5259543928081,15.5270005668672));
#33159=CARTESIAN_POINT('Ctrl Pts',(-2.27442891819367,-3.9039127475242,15.5534578635517));
#33160=CARTESIAN_POINT('Ctrl Pts',(-1.62568741336734,-4.28187110224029,
15.5799151602362));
#33161=CARTESIAN_POINT('Ctrl Pts',(-0.880697274487477,-4.49462479111335,
15.6063724569206));
#33162=CARTESIAN_POINT('Ctrl Pts',(-0.130197475965578,-4.51626065030008,
15.6328297536051));
#33163=CARTESIAN_POINT('Ctrl Pts',(0.620302322556342,-4.53789650948681,
15.6592870502896));
#33164=CARTESIAN_POINT('Ctrl Pts',(1.3763117807203,-4.3684145389872,15.685744346974));
#33165=CARTESIAN_POINT('Ctrl Pts',(2.04574978322079,-4.02845745523656,15.7122016436585));
#33166=CARTESIAN_POINT('Ctrl Pts',(2.71518778572125,-3.68850037148593,15.738658940343));
#33167=CARTESIAN_POINT('Ctrl Pts',(3.29805433255825,-3.17806817448428,15.7651162370274));
#33168=CARTESIAN_POINT('Ctrl Pts',(3.72335692340443,-2.55933094091619,15.7915735337119));
#33169=CARTESIAN_POINT('Ctrl Pts',(4.14865951425061,-1.94059370734809,15.8180308303964));
#33170=CARTESIAN_POINT('Ctrl Pts',(4.41639814910596,-1.21355143721353,15.8444881270808));
#33171=CARTESIAN_POINT('Ctrl Pts',(4.49396255855834,-0.466757074372606,
15.8709454237653));
#33172=CARTESIAN_POINT('Ctrl Pts',(4.51005874349141,-0.311782128309925,
15.8764358483462));
#33173=CARTESIAN_POINT('Ctrl Pts',(4.51796514189739,-0.155956565280692,
15.8819262729272));
#33174=CARTESIAN_POINT('Ctrl Pts',(4.5178043285159,-0.000114763987914418,
15.8874166975081));
#33175=CARTESIAN_POINT('Ctrl Pts',(4.51759608459634,0.0001098887360651,
15.612583302492));
#33176=CARTESIAN_POINT('Ctrl Pts',(4.5171172908178,-0.526893962833933,15.5940190184837));
#33177=CARTESIAN_POINT('Ctrl Pts',(4.42493597400368,-1.05406092973462,15.5754547344754));
#33178=CARTESIAN_POINT('Ctrl Pts',(4.24432532522022,-1.54895583471304,15.5568904504671));
#33179=CARTESIAN_POINT('Ctrl Pts',(3.98692409622027,-2.25426616732798,15.5304331537826));
#33180=CARTESIAN_POINT('Ctrl Pts',(3.54991271903595,-2.89402822885477,15.5039758570982));
#33181=CARTESIAN_POINT('Ctrl Pts',(2.98651869575415,-3.39031970824409,15.4775185604137));
#33182=CARTESIAN_POINT('Ctrl Pts',(2.42312467247236,-3.88661118763341,15.4510612637292));
#33183=CARTESIAN_POINT('Ctrl Pts',(1.73334800309309,-4.23943208488526,15.4246039670448));
#33184=CARTESIAN_POINT('Ctrl Pts',(1.00120272254938,-4.40580920519228,15.3981466703603));
#33185=CARTESIAN_POINT('Ctrl Pts',(0.269057442005672,-4.5721863254993,15.3716893736758));
#33186=CARTESIAN_POINT('Ctrl Pts',(-0.505456449702493,-4.55211966886149,
15.3452320769914));
#33187=CARTESIAN_POINT('Ctrl Pts',(-1.22800401774377,-4.34805333184893,
15.3187747803069));
#33188=CARTESIAN_POINT('Ctrl Pts',(-1.95055158578508,-4.14398699483636,
15.2923174836224));
#33189=CARTESIAN_POINT('Ctrl Pts',(-2.62113283015951,-3.75592097744901,
15.265860186938));
#33190=CARTESIAN_POINT('Ctrl Pts',(-3.15807169745543,-3.23112129111991,
15.2394028902535));
#33191=CARTESIAN_POINT('Ctrl Pts',(-3.69501056475133,-2.70632160479082,
15.212945593569));
#33192=CARTESIAN_POINT('Ctrl Pts',(-4.09830705496871,-2.04478824952003,
15.1864882968846));
#33193=CARTESIAN_POINT('Ctrl Pts',(-4.31884010193997,-1.3270952558398,15.1600310002001));
#33194=CARTESIAN_POINT('Ctrl Pts',(-4.53937314891122,-0.609402262159613,
15.1335737035156));
#33195=CARTESIAN_POINT('Ctrl Pts',(-4.57714275263633,0.164450369930026,
15.1071164068312));
#33196=CARTESIAN_POINT('Ctrl Pts',(-4.42754861718238,0.90020824628735,15.0806591101467));
#33197=CARTESIAN_POINT('Ctrl Pts',(-4.27795448172842,1.63596612264472,15.0542018134622));
#33198=CARTESIAN_POINT('Ctrl Pts',(-3.94099660709542,2.33362924326977,15.0277445167778));
#33199=CARTESIAN_POINT('Ctrl Pts',(-3.45771608949183,2.90822301219606,15.0012872200933));
#33200=CARTESIAN_POINT('Ctrl Pts',(-2.97443557188824,3.48281678112233,14.9748299234088));
#33201=CARTESIAN_POINT('Ctrl Pts',(-2.34483241131409,3.93434119834979,14.9483726267244));
#33202=CARTESIAN_POINT('Ctrl Pts',(-1.64559157592583,4.20780108957628,14.9219153300399));
#33203=CARTESIAN_POINT('Ctrl Pts',(-0.946350740537523,4.4812609808028,14.8954580333554));
#33204=CARTESIAN_POINT('Ctrl Pts',(-0.17747223033509,4.57665634602833,14.8690007366709));
#33205=CARTESIAN_POINT('Ctrl Pts',(0.567395403080653,4.48236813534546,14.8425434399865));
#33206=CARTESIAN_POINT('Ctrl Pts',(1.31226303649637,4.38807992466259,14.816086143302));
#33207=CARTESIAN_POINT('Ctrl Pts',(2.03311979312542,4.10410813807131,14.7896288466175));
#33208=CARTESIAN_POINT('Ctrl Pts',(2.64216611780504,3.665040224898,14.7631715499331));
#33209=CARTESIAN_POINT('Ctrl Pts',(3.25121244248463,3.22597231172472,14.7367142532486));
#33210=CARTESIAN_POINT('Ctrl Pts',(3.74844833521482,2.63180827196943,14.7102569565641));
#33211=CARTESIAN_POINT('Ctrl Pts',(4.07331101456755,1.95491662809442,14.6837996598797));
#33212=CARTESIAN_POINT('Ctrl Pts',(4.36479376317213,1.347576205805,14.6600608740838));
#33213=CARTESIAN_POINT('Ctrl Pts',(4.51750642932664,0.673635432917883,14.6363220882879));
#33214=CARTESIAN_POINT('Ctrl Pts',(4.51803303654689,-7.46219232266102E-5,
14.612583302492));
#33215=CARTESIAN_POINT('Origin',(0.,0.,20.5));
#33216=CARTESIAN_POINT('',(4.51736301819297,2.68279993319077E-6,13.612583302492));
#33217=CARTESIAN_POINT('',(4.51813640225623,-7.72658854479727E-6,13.8874166975081));
#33218=CARTESIAN_POINT('',(4.51775,5.53264807684796E-16,20.5));
#33219=CARTESIAN_POINT('Ctrl Pts',(4.51813584929441,-7.71553139285741E-6,
13.8874166975081));
#33220=CARTESIAN_POINT('Ctrl Pts',(4.5180616865618,0.743534623094937,13.9136178191666));
#33221=CARTESIAN_POINT('Ctrl Pts',(4.33069406362294,1.48711296925487,13.9398189408251));
#33222=CARTESIAN_POINT('Ctrl Pts',(3.97822152575483,2.14180184335953,13.9660200624836));
#33223=CARTESIAN_POINT('Ctrl Pts',(3.62230277429653,2.80289177698769,13.9924773591681));
#33224=CARTESIAN_POINT('Ctrl Pts',(3.0980347793188,3.37334555127586,14.0189346558525));
#33225=CARTESIAN_POINT('Ctrl Pts',(2.46927280238618,3.78368252785474,14.045391952537));
#33226=CARTESIAN_POINT('Ctrl Pts',(1.84051082545358,4.19401950443362,14.0718492492215));
#33227=CARTESIAN_POINT('Ctrl Pts',(1.10725486656609,4.44423968330323,14.0983065459059));
#33228=CARTESIAN_POINT('Ctrl Pts',(0.358814689998941,4.50386652360373,14.1247638425904));
#33229=CARTESIAN_POINT('Ctrl Pts',(-0.389625486568206,4.56349336390423,
14.1512211392749));
#33230=CARTESIAN_POINT('Ctrl Pts',(-1.15324988081502,4.43252686563563,14.1776784359594));
#33231=CARTESIAN_POINT('Ctrl Pts',(-1.83904988664919,4.12691860334233,14.2041357326438));
#33232=CARTESIAN_POINT('Ctrl Pts',(-2.52484989248339,3.82131034104901,14.2305930293283));
#33233=CARTESIAN_POINT('Ctrl Pts',(-3.13282550990494,3.34106031473099,14.2570503260128));
#33234=CARTESIAN_POINT('Ctrl Pts',(-3.58892598157751,2.74466244608609,14.2835076226972));
#33235=CARTESIAN_POINT('Ctrl Pts',(-4.04502645325008,2.14826457744119,14.3099649193817));
#33236=CARTESIAN_POINT('Ctrl Pts',(-4.34925177917366,1.43571886646941,14.3364222160662));
#33237=CARTESIAN_POINT('Ctrl Pts',(-4.46454765134644,0.693812592170538,
14.3628795127506));
#33238=CARTESIAN_POINT('Ctrl Pts',(-4.57984352351921,-0.0480936821283345,
14.3893368094351));
#33239=CARTESIAN_POINT('Ctrl Pts',(-4.50620994194118,-0.819360519754252,
14.4157941061196));
#33240=CARTESIAN_POINT('Ctrl Pts',(-4.25261539535597,-1.52604847346958,
14.442251402804));
#33241=CARTESIAN_POINT('Ctrl Pts',(-3.99902084877075,-2.23273642718488,
14.4687086994885));
#33242=CARTESIAN_POINT('Ctrl Pts',(-3.56546533717836,-2.87484549698955,
14.495165996173));
#33243=CARTESIAN_POINT('Ctrl Pts',(-3.00475544206132,-3.37416750882351,
14.5216232928574));
#33244=CARTESIAN_POINT('Ctrl Pts',(-2.44404554694427,-3.87348952065748,
14.5480805895419));
#33245=CARTESIAN_POINT('Ctrl Pts',(-1.75618126830258,-4.23002447452076,
14.5745378862264));
#33246=CARTESIAN_POINT('Ctrl Pts',(-1.02494371399391,-4.40034680762116,
14.6009951829108));
#33247=CARTESIAN_POINT('Ctrl Pts',(-0.293706159685227,-4.57066914072157,
14.6274524795953));
#33248=CARTESIAN_POINT('Ctrl Pts',(0.480904670290444,-4.5547788530591,14.6539097762798));
#33249=CARTESIAN_POINT('Ctrl Pts',(1.20454203412804,-4.35461136408475,14.6803670729642));
#33250=CARTESIAN_POINT('Ctrl Pts',(1.92817939796561,-4.15444387511041,14.7068243696487));
#33251=CARTESIAN_POINT('Ctrl Pts',(2.60084329566512,-3.76999918482422,14.7332816663332));
#33252=CARTESIAN_POINT('Ctrl Pts',(3.14060400894491,-3.24810223102607,14.7597389630176));
#33253=CARTESIAN_POINT('Ctrl Pts',(3.68036472222471,-2.72620527722791,14.7861962597021));
#33254=CARTESIAN_POINT('Ctrl Pts',(4.08722225108478,-2.0668560599178,14.8126535563866));
#33255=CARTESIAN_POINT('Ctrl Pts',(4.3116217987919,-1.35036258404174,14.839110853071));
#33256=CARTESIAN_POINT('Ctrl Pts',(4.44819168059748,-0.91430364223594,14.8552128012167));
#33257=CARTESIAN_POINT('Ctrl Pts',(4.51717991442519,-0.457078713927616,
14.8713147493624));
#33258=CARTESIAN_POINT('Ctrl Pts',(4.51743493951217,7.09613961932946E-5,
14.8874166975081));
#33259=CARTESIAN_POINT('Ctrl Pts',(4.51803303654689,-7.46219232266102E-5,
14.612583302492));
#33260=CARTESIAN_POINT('Ctrl Pts',(4.51809334238876,-0.0772263404472327,
14.6098647916034));
#33261=CARTESIAN_POINT('Ctrl Pts',(4.51615783443211,-0.154375033265316,
14.6071462807148));
#33262=CARTESIAN_POINT('Ctrl Pts',(4.51220636430248,-0.231420332178498,
14.6044277698263));
#33263=CARTESIAN_POINT('Ctrl Pts',(4.47374956870936,-0.981246400581585,
14.5779704731418));
#33264=CARTESIAN_POINT('Ctrl Pts',(4.24434651154784,-1.72127928939297,14.5515131764573));
#33265=CARTESIAN_POINT('Ctrl Pts',(3.85193823129266,-2.36138381177295,14.5250558797729));
#33266=CARTESIAN_POINT('Ctrl Pts',(3.4595299510375,-3.0014883341529,14.4985985830884));
#33267=CARTESIAN_POINT('Ctrl Pts',(2.90411644768869,-3.54166449010144,14.4721412864039));
#33268=CARTESIAN_POINT('Ctrl Pts',(2.25334647126064,-3.91611942165386,14.4456839897195));
#33269=CARTESIAN_POINT('Ctrl Pts',(1.60257649483259,-4.29057435320629,14.419226693035));
#33270=CARTESIAN_POINT('Ctrl Pts',(0.856450045325319,-4.49930806036259,
14.3927693963505));
#33271=CARTESIAN_POINT('Ctrl Pts',(0.10584449852735,-4.51689700860324,14.3663120996661));
#33272=CARTESIAN_POINT('Ctrl Pts',(-0.644761048270598,-4.53448595684389,
14.3398548029816));
#33273=CARTESIAN_POINT('Ctrl Pts',(-1.39984569235923,-4.36093014616891,
14.3133975062971));
#33274=CARTESIAN_POINT('Ctrl Pts',(-2.06744095976432,-4.01736848223886,
14.2869402096127));
#33275=CARTESIAN_POINT('Ctrl Pts',(-2.73503622716945,-3.67380681830879,
14.2604829129282));
#33276=CARTESIAN_POINT('Ctrl Pts',(-3.31514211789102,-3.16023930112366,
14.2340256162437));
#33277=CARTESIAN_POINT('Ctrl Pts',(-3.73710237646046,-2.53921788589538,
14.2075683195593));
#33278=CARTESIAN_POINT('Ctrl Pts',(-4.15906263502989,-1.91819647066709,
14.1811110228748));
#33279=CARTESIAN_POINT('Ctrl Pts',(-4.42287726144721,-1.18972115739562,
14.1546537261903));
#33280=CARTESIAN_POINT('Ctrl Pts',(-4.49641392618661,-0.442519433011148,
14.1281964295058));
#33281=CARTESIAN_POINT('Ctrl Pts',(-4.56995059092601,0.3046822913733,14.1017391328214));
#33282=CARTESIAN_POINT('Ctrl Pts',(-4.45320929398754,1.07061042687079,14.0752818361369));
#33283=CARTESIAN_POINT('Ctrl Pts',(-4.16040899613706,1.76197577425433,14.0488245394525));
#33284=CARTESIAN_POINT('Ctrl Pts',(-3.86760869828659,2.45334112163787,14.022367242768));
#33285=CARTESIAN_POINT('Ctrl Pts',(-3.39874939952411,3.07014368090745,13.9959099460835));
#33286=CARTESIAN_POINT('Ctrl Pts',(-2.81093764353767,3.53725758297869,13.969452649399));
#33287=CARTESIAN_POINT('Ctrl Pts',(-2.22312588755121,4.00437148504995,13.9429953527146));
#33288=CARTESIAN_POINT('Ctrl Pts',(-1.51636167434084,4.32179672992284,13.9165380560301));
#33289=CARTESIAN_POINT('Ctrl Pts',(-0.776728102877452,4.45087127407632,
13.8900807593456));
#33290=CARTESIAN_POINT('Ctrl Pts',(-0.0370945314140622,4.5799458182298,
13.8636234626612));
#33291=CARTESIAN_POINT('Ctrl Pts',(0.735408398302354,4.52066966166384,13.8371661659767));
#33292=CARTESIAN_POINT('Ctrl Pts',(1.44669068438533,4.2802625746454,13.8107088692922));
#33293=CARTESIAN_POINT('Ctrl Pts',(2.15797297046829,4.03985548762697,13.7842515726078));
#33294=CARTESIAN_POINT('Ctrl Pts',(2.80803461291788,3.61831747015607,13.7577942759233));
#33295=CARTESIAN_POINT('Ctrl Pts',(3.31769882312725,3.06699138623137,13.7313369792388));
#33296=CARTESIAN_POINT('Ctrl Pts',(3.82736303333661,2.51566530230669,13.7048796825544));
#33297=CARTESIAN_POINT('Ctrl Pts',(4.19662981130577,1.83455115192822,13.6784223858699));
#33298=CARTESIAN_POINT('Ctrl Pts',(4.38052287215716,1.10660788480175,13.6519650891854));
#33299=CARTESIAN_POINT('Ctrl Pts',(4.47176471220886,0.745425777992701,13.6388378269543));
#33300=CARTESIAN_POINT('Ctrl Pts',(4.5173707651647,0.372715156596874,13.6257105647231));
#33301=CARTESIAN_POINT('Ctrl Pts',(4.51736305946108,2.68251383689355E-6,
13.612583302492));
#33302=CARTESIAN_POINT('Origin',(0.,0.,20.5));
#33303=CARTESIAN_POINT('',(4.51804648040592,6.99590604930078E-5,12.612583302492));
#33304=CARTESIAN_POINT('',(4.51741195309898,-5.96473381690886E-5,12.8874166975081));
#33305=CARTESIAN_POINT('',(4.51775,5.53264807684796E-16,20.5));
#33306=CARTESIAN_POINT('Ctrl Pts',(4.51741195309898,-5.96473381690886E-5,
12.8874166975081));
#33307=CARTESIAN_POINT('Ctrl Pts',(4.51720574953279,0.442550368129689,12.9030062956018));
#33308=CARTESIAN_POINT('Ctrl Pts',(4.45260272288938,0.885219283315433,12.9185958936956));
#33309=CARTESIAN_POINT('Ctrl Pts',(4.32446175047221,1.30866046509405,12.9341854917894));
#33310=CARTESIAN_POINT('Ctrl Pts',(4.10699214642681,2.02728764889691,12.9606427884738));
#33311=CARTESIAN_POINT('Ctrl Pts',(3.70652120381657,2.69053531250561,12.9871000851583));
#33312=CARTESIAN_POINT('Ctrl Pts',(3.1718258402377,3.21762062452953,13.0135573818428));
#33313=CARTESIAN_POINT('Ctrl Pts',(2.63713047665883,3.74470593655345,13.0400146785272));
#33314=CARTESIAN_POINT('Ctrl Pts',(1.96821069211135,4.13562889699258,13.0664719752117));
#33315=CARTESIAN_POINT('Ctrl Pts',(1.24654017603871,4.34277552191208,13.0929292718962));
#33316=CARTESIAN_POINT('Ctrl Pts',(0.524869659966072,4.54992214683159,13.1193865685806));
#33317=CARTESIAN_POINT('Ctrl Pts',(-0.249551587631711,4.57329243623147,
13.1458438652651));
#33318=CARTESIAN_POINT('Ctrl Pts',(-0.98239991587342,4.41003991472745,13.1723011619496));
#33319=CARTESIAN_POINT('Ctrl Pts',(-1.71524824411517,4.24678739322342,13.198758458634));
#33320=CARTESIAN_POINT('Ctrl Pts',(-2.40652365300083,3.89691206081547,13.2252157553185));
#33321=CARTESIAN_POINT('Ctrl Pts',(-2.97202956278422,3.40302834577293,13.251673052003));
#33322=CARTESIAN_POINT('Ctrl Pts',(-3.53753547256757,2.90914463073042,13.2781303486874));
#33323=CARTESIAN_POINT('Ctrl Pts',(-3.97727188324865,2.27125253305334,13.3045876453719));
#33324=CARTESIAN_POINT('Ctrl Pts',(-4.23767938667653,1.56704660426365,13.3310449420564));
#33325=CARTESIAN_POINT('Ctrl Pts',(-4.49808689010441,0.862840675473956,
13.3575022387408));
#33326=CARTESIAN_POINT('Ctrl Pts',(-4.57916548627907,0.0923209155716644,
13.3839595354253));
#33327=CARTESIAN_POINT('Ctrl Pts',(-4.47103989191868,-0.650664221445422,
13.4104168321098));
#33328=CARTESIAN_POINT('Ctrl Pts',(-4.36291429755829,-1.39364935846249,
13.4368741287942));
#33329=CARTESIAN_POINT('Ctrl Pts',(-4.06558451266282,-2.1090998725944,13.4633314254787));
#33330=CARTESIAN_POINT('Ctrl Pts',(-3.61526497596841,-2.70987468303122,
13.4897887221632));
#33331=CARTESIAN_POINT('Ctrl Pts',(-3.16494543927398,-3.31064949346807,
13.5162460188477));
#33332=CARTESIAN_POINT('Ctrl Pts',(-2.56163615078063,-3.79674860020983,
13.5427033155321));
#33333=CARTESIAN_POINT('Ctrl Pts',(-1.87881951412554,-4.10896567003649,
13.5691606122166));
#33334=CARTESIAN_POINT('Ctrl Pts',(-1.19600287747047,-4.42118273986315,
13.5956179089011));
#33335=CARTESIAN_POINT('Ctrl Pts',(-0.43367889265364,-4.55951777277468,
13.6220752055855));
#33336=CARTESIAN_POINT('Ctrl Pts',(0.315302222661903,-4.50712171486214,
13.64853250227));
#33337=CARTESIAN_POINT('Ctrl Pts',(1.06428333797747,-4.4547256569496,13.6749897989545));
#33338=CARTESIAN_POINT('Ctrl Pts',(1.7999215837918,-4.211598508213,13.7014470956389));
#33339=CARTESIAN_POINT('Ctrl Pts',(2.43261703591854,-3.80735288629203,13.7279043923234));
#33340=CARTESIAN_POINT('Ctrl Pts',(3.06531248804526,-3.40310726437108,13.7543616890079));
#33341=CARTESIAN_POINT('Ctrl Pts',(3.59506514648438,-2.8377431692658,13.7808189856923));
#33342=CARTESIAN_POINT('Ctrl Pts',(3.95735172373184,-2.18012132205388,13.8072762823768));
#33343=CARTESIAN_POINT('Ctrl Pts',(4.3196383009793,-1.52249947484199,13.8337335790613));
#33344=CARTESIAN_POINT('Ctrl Pts',(4.51445879703509,-0.772619875523486,
13.8601908757457));
#33345=CARTESIAN_POINT('Ctrl Pts',(4.51808429109356,-0.0218170293801791,
13.8866481724302));
#33346=CARTESIAN_POINT('Ctrl Pts',(4.51811939524822,-0.0145473169490636,
13.8869043474562));
#33347=CARTESIAN_POINT('Ctrl Pts',(4.5181365744023,-0.0072775179612929,
13.8871605224821));
#33348=CARTESIAN_POINT('Ctrl Pts',(4.51813584929441,-7.71553139285741E-6,
13.8874166975081));
#33349=CARTESIAN_POINT('Ctrl Pts',(4.51736305946108,2.68251383689355E-6,
13.612583302492));
#33350=CARTESIAN_POINT('Ctrl Pts',(4.51735523473014,-0.378466950622669,
13.5992532680387));
#33351=CARTESIAN_POINT('Ctrl Pts',(4.47031360843327,-0.756938494124053,
13.5859232335853));
#33352=CARTESIAN_POINT('Ctrl Pts',(4.37626124565255,-1.12334284793068,13.572593199132));
#33353=CARTESIAN_POINT('Ctrl Pts',(4.18958721456293,-1.85057792966208,13.5461359024476));
#33354=CARTESIAN_POINT('Ctrl Pts',(3.81771980865007,-2.53027570925035,13.5196786057631));
#33355=CARTESIAN_POINT('Ctrl Pts',(3.3059520663969,-3.07964974938441,13.4932213090786));
#33356=CARTESIAN_POINT('Ctrl Pts',(2.79418432414376,-3.62902378951843,13.4667640123941));
#33357=CARTESIAN_POINT('Ctrl Pts',(2.14251624555032,-4.04807409019825,13.4403067157097));
#33358=CARTESIAN_POINT('Ctrl Pts',(1.43032028136785,-4.28576078857712,13.4138494190252));
#33359=CARTESIAN_POINT('Ctrl Pts',(0.718124317185353,-4.523447486956,13.3873921223408));
#33360=CARTESIAN_POINT('Ctrl Pts',(-0.0545995325861841,-4.57977058303392,
13.3609348256563));
#33361=CARTESIAN_POINT('Ctrl Pts',(-0.793734358242206,-4.44786998604312,
13.3344775289718));
#33362=CARTESIAN_POINT('Ctrl Pts',(-1.53286918389827,-4.31596938905231,
13.3080202322873));
#33363=CARTESIAN_POINT('Ctrl Pts',(-2.23841498543881,-3.99584509899276,
13.2815629356029));
#33364=CARTESIAN_POINT('Ctrl Pts',(-2.82443706508576,-3.52648790010218,
13.2551056389184));
#33365=CARTESIAN_POINT('Ctrl Pts',(-3.41045914473268,-3.05713070121163,
13.2286483422339));
#33366=CARTESIAN_POINT('Ctrl Pts',(-3.87695750248602,-2.43854059349005,
13.2021910455495));
#33367=CARTESIAN_POINT('Ctrl Pts',(-4.16711315465972,-1.74606116744496,
13.175733748865));
#33368=CARTESIAN_POINT('Ctrl Pts',(-4.45726880683343,-1.05358174139987,
13.1492764521805));
#33369=CARTESIAN_POINT('Ctrl Pts',(-4.57108175342749,-0.287212997031258,
13.1228191554961));
#33370=CARTESIAN_POINT('Ctrl Pts',(-4.49468970350711,0.459702200761001,
13.0963618588116));
#33371=CARTESIAN_POINT('Ctrl Pts',(-4.41829765358673,1.20661739855328,13.0699045621271));
#33372=CARTESIAN_POINT('Ctrl Pts',(-4.15170060715189,1.93407904976921,13.0434472654427));
#33373=CARTESIAN_POINT('Ctrl Pts',(-3.72736978940707,2.5534831303952,13.0169899687582));
#33374=CARTESIAN_POINT('Ctrl Pts',(-3.30303897166226,3.1728872110212,12.9905326720737));
#33375=CARTESIAN_POINT('Ctrl Pts',(-2.72097438260746,3.68423372105726,12.9640753753893));
#33376=CARTESIAN_POINT('Ctrl Pts',(-2.05207084500052,4.02524122150415,12.9376180787048));
#33377=CARTESIAN_POINT('Ctrl Pts',(-1.3831673073936,4.36624872195103,12.9111607820203));
#33378=CARTESIAN_POINT('Ctrl Pts',(-0.627424821234523,4.53691721280875,
12.8847034853359));
#33379=CARTESIAN_POINT('Ctrl Pts',(0.123108015066336,4.51645946077498,12.8582461886514));
#33380=CARTESIAN_POINT('Ctrl Pts',(0.873640851367194,4.49600170874121,12.8317888919669));
#33381=CARTESIAN_POINT('Ctrl Pts',(1.61896403780984,4.28441771381596,12.8053315952824));
#33382=CARTESIAN_POINT('Ctrl Pts',(2.268298035158,3.9074781724145,12.778874298598));
#33383=CARTESIAN_POINT('Ctrl Pts',(2.91763203250619,3.53053863101303,12.7524170019135));
#33384=CARTESIAN_POINT('Ctrl Pts',(3.47097684075988,2.98824354313534,12.7259597052291));
#33385=CARTESIAN_POINT('Ctrl Pts',(3.86093567467777,2.34664385031004,12.6995024085446));
#33386=CARTESIAN_POINT('Ctrl Pts',(4.25089450859566,1.70504415748472,12.6730451118601));
#33387=CARTESIAN_POINT('Ctrl Pts',(4.47746736817774,0.964139859711776,12.6465878151756));
#33388=CARTESIAN_POINT('Ctrl Pts',(4.51305792988216,0.214172280478037,12.6201305184912));
#33389=CARTESIAN_POINT('Ctrl Pts',(4.51644212114351,0.142860291950876,12.6176147798248));
#33390=CARTESIAN_POINT('Ctrl Pts',(4.51809954743677,0.0714663578345357,
12.6150990411584));
#33391=CARTESIAN_POINT('Ctrl Pts',(4.51804648040592,6.99590604930078E-5,
12.612583302492));
#33392=CARTESIAN_POINT('Origin',(0.,0.,20.5));
#33393=CARTESIAN_POINT('',(4.5175801641472,-0.000107849321499542,11.612583302492));
#33394=CARTESIAN_POINT('',(4.5178502562812,0.000110962492481057,11.8874166975081));
#33395=CARTESIAN_POINT('',(4.51775,5.53264807684796E-16,20.5));
#33396=CARTESIAN_POINT('Ctrl Pts',(4.5178502562812,0.000110962492481057,
11.8874166975081));
#33397=CARTESIAN_POINT('Ctrl Pts',(4.51799453028332,0.141405931765494,11.8923947720371));
#33398=CARTESIAN_POINT('Ctrl Pts',(4.51149711848843,0.282687684813822,11.8973728465661));
#33399=CARTESIAN_POINT('Ctrl Pts',(4.49826065670895,0.423335220010937,11.9023509210951));
#33400=CARTESIAN_POINT('Ctrl Pts',(4.42791197182862,1.17084382900464,11.9288082177796));
#33401=CARTESIAN_POINT('Ctrl Pts',(4.16720717585505,1.90043785893767,11.955265514464));
#33402=CARTESIAN_POINT('Ctrl Pts',(3.7478998244077,2.5232535644287,11.9817228111485));
#33403=CARTESIAN_POINT('Ctrl Pts',(3.32859247296032,3.14606926991974,12.008180107833));
#33404=CARTESIAN_POINT('Ctrl Pts',(2.75068256603915,3.66210665096878,12.0346374045175));
#33405=CARTESIAN_POINT('Ctrl Pts',(2.08455889071624,4.00851292567871,12.0610947012019));
#33406=CARTESIAN_POINT('Ctrl Pts',(1.41843521539332,4.35491920038864,12.0875519978864));
#33407=CARTESIAN_POINT('Ctrl Pts',(0.664097771668666,4.53169436875946,12.1140092945709));
#33408=CARTESIAN_POINT('Ctrl Pts',(-0.0865759746608722,4.51730741092621,
12.1404665912553));
#33409=CARTESIAN_POINT('Ctrl Pts',(-0.83724972099039,4.50292045309296,12.1669238879398));
#33410=CARTESIAN_POINT('Ctrl Pts',(-1.58425976992479,4.29737136905566,12.1933811846243));
#33411=CARTESIAN_POINT('Ctrl Pts',(-2.23662112424321,3.92569580976245,12.2198384813087));
#33412=CARTESIAN_POINT('Ctrl Pts',(-2.88898247856163,3.55402025046923,12.2462957779932));
#33413=CARTESIAN_POINT('Ctrl Pts',(-3.44669513826407,3.01621821592011,12.2727530746777));
#33414=CARTESIAN_POINT('Ctrl Pts',(-3.84183031863679,2.37779339872086,12.2992103713621));
#33415=CARTESIAN_POINT('Ctrl Pts',(-4.23696549900952,1.7393685815216,12.3256676680466));
#33416=CARTESIAN_POINT('Ctrl Pts',(-4.46952320005253,1.00032098167222,12.3521249647311));
#33417=CARTESIAN_POINT('Ctrl Pts',(-4.51117815115765,0.250665778907295,
12.3785822614155));
#33418=CARTESIAN_POINT('Ctrl Pts',(-4.55283310226278,-0.498989423857626,
12.4050395581));
#33419=CARTESIAN_POINT('Ctrl Pts',(-4.40358530343001,-1.25925222953809,
12.4314968547845));
#33420=CARTESIAN_POINT('Ctrl Pts',(-4.08161297138,-1.93752346980879,12.4579541514689));
#33421=CARTESIAN_POINT('Ctrl Pts',(-3.75964063932998,-2.61579471007952,
12.4844114481534));
#33422=CARTESIAN_POINT('Ctrl Pts',(-3.26494377406269,-3.21207438494048,
12.5108687448379));
#33423=CARTESIAN_POINT('Ctrl Pts',(-2.65777590627122,-3.65373628991496,
12.5373260415223));
#33424=CARTESIAN_POINT('Ctrl Pts',(-2.05060803847976,-4.09539819488944,
12.5637833382068));
#33425=CARTESIAN_POINT('Ctrl Pts',(-1.33096916816412,-4.38244232997743,
12.5902406348913));
#33426=CARTESIAN_POINT('Ctrl Pts',(-0.586510513281939,-4.47990703720592,
12.6166979315757));
#33427=CARTESIAN_POINT('Ctrl Pts',(0.15794814160022,-4.57737174443441,12.6431552282602));
#33428=CARTESIAN_POINT('Ctrl Pts',(0.927226581048916,-4.48525702380341,
12.6696125249447));
#33429=CARTESIAN_POINT('Ctrl Pts',(1.62762754252377,-4.21478234633953,12.6960698216291));
#33430=CARTESIAN_POINT('Ctrl Pts',(2.32802850399863,-3.94430766887566,12.7225271183136));
#33431=CARTESIAN_POINT('Ctrl Pts',(2.95955198749964,-3.49547303457892,12.7489844149981));
#33432=CARTESIAN_POINT('Ctrl Pts',(3.44527913166315,-2.92294600516735,12.7754417116826));
#33433=CARTESIAN_POINT('Ctrl Pts',(3.93100627582668,-2.35041897575576,12.801899008367));
#33434=CARTESIAN_POINT('Ctrl Pts',(4.2709370806527,-1.65419955122932,12.8283563050515));
#33435=CARTESIAN_POINT('Ctrl Pts',(4.42366835032544,-0.919086486967588,
12.854813601736));
#33436=CARTESIAN_POINT('Ctrl Pts',(4.48640482049374,-0.617128682745771,
12.8656813003267));
#33437=CARTESIAN_POINT('Ctrl Pts',(4.51755570011492,-0.308608476653881,
12.8765489989174));
#33438=CARTESIAN_POINT('Ctrl Pts',(4.51741195309898,-5.96473381690886E-5,
12.8874166975081));
#33439=CARTESIAN_POINT('Ctrl Pts',(4.51804648040592,6.99590604930078E-5,
12.612583302492));
#33440=CARTESIAN_POINT('Ctrl Pts',(4.51754145680588,-0.679388939577024,
12.5886417444739));
#33441=CARTESIAN_POINT('Ctrl Pts',(4.36212083370235,-1.35907105681478,12.5647001864558));
#33442=CARTESIAN_POINT('Ctrl Pts',(4.06580926285153,-1.97047118281595,12.5407586284378));
#33443=CARTESIAN_POINT('Ctrl Pts',(3.73836177028969,-2.64611620618181,12.5143013317533));
#33444=CARTESIAN_POINT('Ctrl Pts',(3.23885852133923,-3.23837539221903,12.4878440350688));
#33445=CARTESIAN_POINT('Ctrl Pts',(2.62813845890645,-3.67511222754003,12.4613867383844));
#33446=CARTESIAN_POINT('Ctrl Pts',(2.01741839647366,-4.11184906286103,12.4349294416999));
#33447=CARTESIAN_POINT('Ctrl Pts',(1.29548152055856,-4.3930635474658,12.4084721450154));
#33448=CARTESIAN_POINT('Ctrl Pts',(0.550258943657521,-4.48450406835832,
12.382014848331));
#33449=CARTESIAN_POINT('Ctrl Pts',(-0.194963633243496,-4.57594458925083,
12.3555575516465));
#33450=CARTESIAN_POINT('Ctrl Pts',(-0.963471911130448,-4.47761114643111,
12.329100254962));
#33451=CARTESIAN_POINT('Ctrl Pts',(-1.66166243228881,-4.2014806444059,12.3026429582776));
#33452=CARTESIAN_POINT('Ctrl Pts',(-2.35985295344718,-3.92535014238069,
12.2761856615931));
#33453=CARTESIAN_POINT('Ctrl Pts',(-2.98772571787696,-3.47142258114999,
12.2497283649086));
#33454=CARTESIAN_POINT('Ctrl Pts',(-3.46880651775701,-2.89498583529589,
12.2232710682242));
#33455=CARTESIAN_POINT('Ctrl Pts',(-3.94988731763707,-2.31854908944178,
12.1968137715397));
#33456=CARTESIAN_POINT('Ctrl Pts',(-4.28417615296739,-1.61960315896426,
12.1703564748552));
#33457=CARTESIAN_POINT('Ctrl Pts',(-4.43095701357263,-0.883278884650216,
12.1438991781708));
#33458=CARTESIAN_POINT('Ctrl Pts',(-4.57773787417786,-0.146954610336191,
12.1174418814863));
#33459=CARTESIAN_POINT('Ctrl Pts',(-4.53701076005802,0.626748007814359,
12.0909845848018));
#33460=CARTESIAN_POINT('Ctrl Pts',(-4.31373618863893,1.34359284719155,12.0645272881174));
#33461=CARTESIAN_POINT('Ctrl Pts',(-4.09046161721984,2.06043768656874,12.0380699914329));
#33462=CARTESIAN_POINT('Ctrl Pts',(-3.6846395885015,2.72042474717257,12.0116126947484));
#33463=CARTESIAN_POINT('Ctrl Pts',(-3.1456987764459,3.24316833544978,11.985155398064));
#33464=CARTESIAN_POINT('Ctrl Pts',(-2.60675796439029,3.76591192372701,11.9586981013795));
#33465=CARTESIAN_POINT('Ctrl Pts',(-1.9346983689974,4.15141203967762,11.932240804695));
#33466=CARTESIAN_POINT('Ctrl Pts',(-1.21137610519676,4.35271519582384,11.9057835080105));
#33467=CARTESIAN_POINT('Ctrl Pts',(-0.488053841396109,4.55401835197005,
11.8793262113261));
#33468=CARTESIAN_POINT('Ctrl Pts',(0.286531090812296,4.57112454831187,11.8528689146416));
#33469=CARTESIAN_POINT('Ctrl Pts',(1.0180351039428,4.40195026906683,11.8264116179572));
#33470=CARTESIAN_POINT('Ctrl Pts',(1.74953911707329,4.2327759898218,11.7999543212727));
#33471=CARTESIAN_POINT('Ctrl Pts',(2.43796221112589,3.8773212349899,11.7734970245882));
#33472=CARTESIAN_POINT('Ctrl Pts',(2.99945521514432,3.37888000031681,11.7470397279037));
#33473=CARTESIAN_POINT('Ctrl Pts',(3.56094821916276,2.88043876564371,11.7205824312193));
#33474=CARTESIAN_POINT('Ctrl Pts',(3.99551113314703,2.23901105112941,11.6941251345348));
#33475=CARTESIAN_POINT('Ctrl Pts',(4.2502146751182,1.53272204251365,11.6676678378503));
#33476=CARTESIAN_POINT('Ctrl Pts',(4.42698035695052,1.0425535226241,11.6493063260642));
#33477=CARTESIAN_POINT('Ctrl Pts',(4.51711789485057,0.521144965264365,11.6309448142781));
#33478=CARTESIAN_POINT('Ctrl Pts',(4.5175801641472,-0.000107849321499542,
11.612583302492));
#33479=CARTESIAN_POINT('Origin',(0.,0.,20.5));
#33480=CARTESIAN_POINT('',(4.517607537138,0.000111184246189833,10.612583302492));
#33481=CARTESIAN_POINT('',(4.51779144669394,-0.000115517084662978,10.8874166975081));
#33482=CARTESIAN_POINT('',(4.51775,5.53264807684796E-16,20.5));
#33483=CARTESIAN_POINT('Ctrl Pts',(4.51779144669394,-0.000115517084662978,
10.8874166975081));
#33484=CARTESIAN_POINT('Ctrl Pts',(4.51718124885461,0.590959459307199,10.9082405451568));
#33485=CARTESIAN_POINT('Ctrl Pts',(4.40057028871007,1.18226809182004,10.9290643928055));
#33486=CARTESIAN_POINT('Ctrl Pts',(4.17452335103026,1.72826978099499,10.9498882404543));
#33487=CARTESIAN_POINT('Ctrl Pts',(3.88732422262257,2.42198061313325,10.9763455371387));
#33488=CARTESIAN_POINT('Ctrl Pts',(3.42346880605941,3.0425550177638,11.0028028338232));
#33489=CARTESIAN_POINT('Ctrl Pts',(2.83945417771489,3.51440771921171,11.0292601305077));
#33490=CARTESIAN_POINT('Ctrl Pts',(2.25543954937037,3.98626042065963,11.0557174271921));
#33491=CARTESIAN_POINT('Ctrl Pts',(1.55126570924448,4.30939141892491,11.0821747238766));
#33492=CARTESIAN_POINT('Ctrl Pts',(0.812700251733397,4.44444371603802,11.1086320205611));
#33493=CARTESIAN_POINT('Ctrl Pts',(0.0741347942222902,4.57949601315113,
11.1350893172455));
#33494=CARTESIAN_POINT('Ctrl Pts',(-0.698822280674023,4.52646960911206,
11.16154661393));
#33495=CARTESIAN_POINT('Ctrl Pts',(-1.41202565668891,4.29182306124677,11.1880039106145));
#33496=CARTESIAN_POINT('Ctrl Pts',(-2.12522903270377,4.0571765133815,11.2144612072989));
#33497=CARTESIAN_POINT('Ctrl Pts',(-2.7786787098372,3.64090982169003,11.2409185039834));
#33498=CARTESIAN_POINT('Ctrl Pts',(-3.29278524060752,3.09372380852504,11.2673758006679));
#33499=CARTESIAN_POINT('Ctrl Pts',(-3.80689177137783,2.54653779536005,11.2938330973523));
#33500=CARTESIAN_POINT('Ctrl Pts',(-4.18165515578503,1.86843246072154,11.3202903940368));
#33501=CARTESIAN_POINT('Ctrl Pts',(-4.37142962837066,1.14200028388812,11.3467476907213));
#33502=CARTESIAN_POINT('Ctrl Pts',(-4.56120410095629,0.415568107054687,
11.3732049874058));
#33503=CARTESIAN_POINT('Ctrl Pts',(-4.56598966172034,-0.359190911973653,
11.3996622840902));
#33504=CARTESIAN_POINT('Ctrl Pts',(-4.38520343465808,-1.08791198212924,
11.4261195807747));
#33505=CARTESIAN_POINT('Ctrl Pts',(-4.20441720759582,-1.81663305228484,
11.4525768774592));
#33506=CARTESIAN_POINT('Ctrl Pts',(-3.83805919270723,-2.49931617356768,
11.4790341741436));
#33507=CARTESIAN_POINT('Ctrl Pts',(-3.33075139074592,-3.05281129735225,
11.5054914708281));
#33508=CARTESIAN_POINT('Ctrl Pts',(-2.82344358878461,-3.6063064211368,11.5319487675126));
#33509=CARTESIAN_POINT('Ctrl Pts',(-2.17518599975058,-4.03061354742309,
11.558406064197));
#33510=CARTESIAN_POINT('Ctrl Pts',(-1.46493568054124,-4.27405253782339,
11.5848633608815));
#33511=CARTESIAN_POINT('Ctrl Pts',(-0.7546853613319,-4.51749152822369,11.611320657566));
#33512=CARTESIAN_POINT('Ctrl Pts',(0.017557688052746,-4.580062382738,11.6377779542504));
#33513=CARTESIAN_POINT('Ctrl Pts',(0.757735118863148,-4.4541440405356,11.6642352509349));
#33514=CARTESIAN_POINT('Ctrl Pts',(1.49791254967357,-4.3282256983332,11.6906925476194));
#33515=CARTESIAN_POINT('Ctrl Pts',(2.20602436190975,-4.01381815941408,11.7171498443038));
#33516=CARTESIAN_POINT('Ctrl Pts',(2.79582332053076,-3.54921591405394,11.7436071409883));
#33517=CARTESIAN_POINT('Ctrl Pts',(3.38562227915178,-3.0846136686938,11.7700644376728));
#33518=CARTESIAN_POINT('Ctrl Pts',(3.85710838415764,-2.46981671689265,11.7965217343572));
#33519=CARTESIAN_POINT('Ctrl Pts',(4.15285514976701,-1.77970664696488,11.8229790310417));
#33520=CARTESIAN_POINT('Ctrl Pts',(4.39295566177474,-1.21944428605644,11.8444582531972));
#33521=CARTESIAN_POINT('Ctrl Pts',(4.51722774785459,-0.609543637247958,
11.8659374753526));
#33522=CARTESIAN_POINT('Ctrl Pts',(4.5178502562812,0.000110962492481057,
11.8874166975081));
#33523=CARTESIAN_POINT('Ctrl Pts',(4.5175801641472,-0.000107849321499542,
11.612583302492));
#33524=CARTESIAN_POINT('Ctrl Pts',(4.51778398357309,-0.229933732598545,
11.6044875175936));
#33525=CARTESIAN_POINT('Ctrl Pts',(4.50055473854231,-0.45972933914648,11.5963917326953));
#33526=CARTESIAN_POINT('Ctrl Pts',(4.46563124792392,-0.686803612223187,
11.5882959477969));
#33527=CARTESIAN_POINT('Ctrl Pts',(4.35150010880038,-1.42888995562703,11.5618386511125));
#33528=CARTESIAN_POINT('Ctrl Pts',(4.04839366059521,-2.14191233971748,11.535381354428));
#33529=CARTESIAN_POINT('Ctrl Pts',(3.59322993324244,-2.73902542723646,11.5089240577435));
#33530=CARTESIAN_POINT('Ctrl Pts',(3.13806620588969,-3.33613851475543,11.4824667610591));
#33531=CARTESIAN_POINT('Ctrl Pts',(2.53084519938934,-3.81734230570294,11.4560094643746));
#33532=CARTESIAN_POINT('Ctrl Pts',(1.84552576030269,-4.12402671090484,11.4295521676901));
#33533=CARTESIAN_POINT('Ctrl Pts',(1.16020632121604,-4.43071111610674,11.4030948710056));
#33534=CARTESIAN_POINT('Ctrl Pts',(0.396788449543078,-4.56287613556304,
11.3766375743212));
#33535=CARTESIAN_POINT('Ctrl Pts',(-0.351744402844812,-4.50442421617511,
11.3501802776367));
#33536=CARTESIAN_POINT('Ctrl Pts',(-1.10027725523272,-4.44597229678718,
11.3237229809523));
#33537=CARTESIAN_POINT('Ctrl Pts',(-1.83392508833558,-4.196903438555,11.2972656842678));
#33538=CARTESIAN_POINT('Ctrl Pts',(-2.4633304080324,-3.787553952759,11.2708083875833));
#33539=CARTESIAN_POINT('Ctrl Pts',(-3.0927357277292,-3.378204466963,11.2443510908988));
#33540=CARTESIAN_POINT('Ctrl Pts',(-3.61789853401999,-2.80857435360317,
11.2178937942144));
#33541=CARTESIAN_POINT('Ctrl Pts',(-3.97485457831262,-2.1480439300593,11.1914364975299));
#33542=CARTESIAN_POINT('Ctrl Pts',(-4.33181062260526,-1.48751350651541,
11.1649792008454));
#33543=CARTESIAN_POINT('Ctrl Pts',(-4.52055990489972,-0.736082772787468,
11.138521904161));
#33544=CARTESIAN_POINT('Ctrl Pts',(-4.51811297150728,0.0147248393883086,
11.1120646074765));
#33545=CARTESIAN_POINT('Ctrl Pts',(-4.51566603811484,0.765532451564064,
11.085607310792));
#33546=CARTESIAN_POINT('Ctrl Pts',(-4.32202288903552,1.5157169421876,11.0591500141076));
#33547=CARTESIAN_POINT('Ctrl Pts',(-3.96076904551623,2.17390667055369,11.0326927174231));
#33548=CARTESIAN_POINT('Ctrl Pts',(-3.59951520199693,2.83209639891979,11.0062354207386));
#33549=CARTESIAN_POINT('Ctrl Pts',(-3.07065066403766,3.3982913650284,10.9797781240542));
#33550=CARTESIAN_POINT('Ctrl Pts',(-2.43859054705097,3.8035296486331,10.9533208273697));
#33551=CARTESIAN_POINT('Ctrl Pts',(-1.8065304300643,4.20876793223779,10.9268635306852));
#33552=CARTESIAN_POINT('Ctrl Pts',(-1.0712747340502,4.4530495333386,10.9004062340008));
#33553=CARTESIAN_POINT('Ctrl Pts',(-0.322376789052762,4.50662122327553,
10.8739489373163));
#33554=CARTESIAN_POINT('Ctrl Pts',(0.426521155944698,4.56019291321245,10.8474916406318));
#33555=CARTESIAN_POINT('Ctrl Pts',(1.18906134992551,4.42305469198549,10.8210343439474));
#33556=CARTESIAN_POINT('Ctrl Pts',(1.87236724118984,4.11190984316492,10.7945770472629));
#33557=CARTESIAN_POINT('Ctrl Pts',(2.55567313245417,3.80076499434435,10.7681197505784));
#33558=CARTESIAN_POINT('Ctrl Pts',(3.15974472100203,3.31561351793017,10.741662453894));
#33559=CARTESIAN_POINT('Ctrl Pts',(3.61100675589317,2.71554632681736,10.7152051572095));
#33560=CARTESIAN_POINT('Ctrl Pts',(4.0622687907843,2.11547913570456,10.688747860525));
#33561=CARTESIAN_POINT('Ctrl Pts',(4.36072127201872,1.40049622989312,10.6622905638405));
#33562=CARTESIAN_POINT('Ctrl Pts',(4.47001301768877,0.657681736016976,10.6358332671561));
#33563=CARTESIAN_POINT('Ctrl Pts',(4.5020272386327,0.440093233047143,10.6280832789347));
#33564=CARTESIAN_POINT('Ctrl Pts',(4.51781057668589,0.220116648612125,10.6203332907133));
#33565=CARTESIAN_POINT('Ctrl Pts',(4.517607537138,0.000111184246189833,
10.612583302492));
#33566=CARTESIAN_POINT('Origin',(0.,0.,20.5));
#33567=CARTESIAN_POINT('',(4.51802315729813,-7.77880120685776E-5,9.61258330249199));
#33568=CARTESIAN_POINT('',(4.5174420818448,7.39595355181285E-5,9.88741669750808));
#33569=CARTESIAN_POINT('',(4.51775,5.53264807684796E-16,20.5));
#33570=CARTESIAN_POINT('Ctrl Pts',(4.5174420818448,7.39595355181285E-5,
9.88741669750808));
#33571=CARTESIAN_POINT('Ctrl Pts',(4.51761100468578,0.290010274247371,9.89762902159206));
#33572=CARTESIAN_POINT('Ctrl Pts',(4.49012793116805,0.579914973420611,9.90784134567604));
#33573=CARTESIAN_POINT('Ctrl Pts',(4.43468447094956,0.864369878764984,9.91805366976002));
#33574=CARTESIAN_POINT('Ctrl Pts',(4.29104585704042,1.60131357171471,9.94451096644449));
#33575=CARTESIAN_POINT('Ctrl Pts',(3.95974153092839,2.30167910674412,9.97096826312895));
#33576=CARTESIAN_POINT('Ctrl Pts',(3.48112399286906,2.88016273680304,9.99742555981342));
#33577=CARTESIAN_POINT('Ctrl Pts',(3.00250645480973,3.45864636686196,10.0238828564979));
#33578=CARTESIAN_POINT('Ctrl Pts',(2.3765757048031,3.91524809195038,10.0503401531824));
#33579=CARTESIAN_POINT('Ctrl Pts',(1.67956941546288,4.19435432728793,10.0767974498668));
#33580=CARTESIAN_POINT('Ctrl Pts',(0.982563126122689,4.47346056262548,10.1032547465513));
#33581=CARTESIAN_POINT('Ctrl Pts',(0.214481297448898,4.57507130821216,10.1297120432358));
#33582=CARTESIAN_POINT('Ctrl Pts',(-0.531124553886154,4.4868104876913,10.1561693399202));
#33583=CARTESIAN_POINT('Ctrl Pts',(-1.27673040522121,4.39854966717044,10.1826266366047));
#33584=CARTESIAN_POINT('Ctrl Pts',(-1.99986027921753,4.12041728054204,10.2090839332892));
#33585=CARTESIAN_POINT('Ctrl Pts',(-2.61243775753278,3.68628954467964,10.2355412299736));
#33586=CARTESIAN_POINT('Ctrl Pts',(-3.22501523584806,3.25216180881724,10.2619985266581));
#33587=CARTESIAN_POINT('Ctrl Pts',(-3.72704031848226,2.66203872372082,10.2884558233426));
#33588=CARTESIAN_POINT('Ctrl Pts',(-4.05736690597737,1.9877966280475,10.314913120027));
#33589=CARTESIAN_POINT('Ctrl Pts',(-4.38769349347249,1.31355453237416,10.3413704167115));
#33590=CARTESIAN_POINT('Ctrl Pts',(-4.54632158582851,0.555193426123966,
10.367827713396));
#33591=CARTESIAN_POINT('Ctrl Pts',(-4.51393045695515,-0.194919147263826,
10.3942850100804));
#33592=CARTESIAN_POINT('Ctrl Pts',(-4.48153932808179,-0.945031720651576,
10.4207423067649));
#33593=CARTESIAN_POINT('Ctrl Pts',(-4.25812897797905,-1.68689576117688,
10.4471996034494));
#33594=CARTESIAN_POINT('Ctrl Pts',(-3.87091054003425,-2.33015304974784,
10.4736569001339));
#33595=CARTESIAN_POINT('Ctrl Pts',(-3.48369210208944,-2.9734103383188,10.5001141968183));
#33596=CARTESIAN_POINT('Ctrl Pts',(-2.93266557630255,-3.51806087493544,
10.5265714935028));
#33597=CARTESIAN_POINT('Ctrl Pts',(-2.28494538367617,-3.89776682701959,
10.5530287901872));
#33598=CARTESIAN_POINT('Ctrl Pts',(-1.63722519104977,-4.27747277910375,
10.5794860868717));
#33599=CARTESIAN_POINT('Ctrl Pts',(-0.892811331583869,-4.49223414665542,
10.6059433835562));
#33600=CARTESIAN_POINT('Ctrl Pts',(-0.142372589495352,-4.51589323278992,
10.6324006802407));
#33601=CARTESIAN_POINT('Ctrl Pts',(0.608066152593165,-4.53955231892441,
10.6588579769251));
#33602=CARTESIAN_POINT('Ctrl Pts',(1.36452977730431,-4.37210912364174,10.6853152736096));
#33603=CARTESIAN_POINT('Ctrl Pts',(2.03488185235016,-4.03395804281271,10.7117725702941));
#33604=CARTESIAN_POINT('Ctrl Pts',(2.70523392739599,-3.6958069619837,10.7382298669785));
#33605=CARTESIAN_POINT('Ctrl Pts',(3.28947445277654,-3.18694799560833,10.764687163663));
#33606=CARTESIAN_POINT('Ctrl Pts',(3.71644357909769,-2.56935960262103,10.7911444603475));
#33607=CARTESIAN_POINT('Ctrl Pts',(4.14341270541885,-1.95177120963373,10.8176017570319));
#33608=CARTESIAN_POINT('Ctrl Pts',(4.41311043268061,-1.22545339003449,10.8440590537164));
#33609=CARTESIAN_POINT('Ctrl Pts',(4.49268787618539,-0.478870850411892,
10.8705163504009));
#33610=CARTESIAN_POINT('Ctrl Pts',(4.50963199098762,-0.319903940901298,
10.8761497994366));
#33611=CARTESIAN_POINT('Ctrl Pts',(4.51795652273981,-0.160018279147252,
10.8817832484723));
#33612=CARTESIAN_POINT('Ctrl Pts',(4.51779144669394,-0.000115517084662978,
10.8874166975081));
#33613=CARTESIAN_POINT('Ctrl Pts',(4.517607537138,0.000111184246189833,
10.612583302492));
#33614=CARTESIAN_POINT('Ctrl Pts',(4.51711743014117,-0.530948988737395,
10.5938759940289));
#33615=CARTESIAN_POINT('Ctrl Pts',(4.42347995325767,-1.06217743558981,10.5751686855658));
#33616=CARTESIAN_POINT('Ctrl Pts',(4.24013400258143,-1.56039266992325,10.5564613771027));
#33617=CARTESIAN_POINT('Ctrl Pts',(3.98083223169834,-2.26500650004656,10.5300040804182));
#33618=CARTESIAN_POINT('Ctrl Pts',(3.54209767982647,-2.90358807835227,10.5035467837338));
#33619=CARTESIAN_POINT('Ctrl Pts',(2.9773677298226,-3.39835887534092,10.4770894870493));
#33620=CARTESIAN_POINT('Ctrl Pts',(2.41263777981875,-3.89312967232955,10.4506321903648));
#33621=CARTESIAN_POINT('Ctrl Pts',(1.7219124316829,-4.24408968800111,10.4241748936803));
#33622=CARTESIAN_POINT('Ctrl Pts',(0.989321268370679,-4.40849238086523,
10.3977175969959));
#33623=CARTESIAN_POINT('Ctrl Pts',(0.256730105058482,-4.57289507372935,
10.3712603003114));
#33624=CARTESIAN_POINT('Ctrl Pts',(-0.517726873430066,-4.55074044378602,
10.3448030036269));
#33625=CARTESIAN_POINT('Ctrl Pts',(-1.2397216642308,-4.34472690044313,10.3183457069425));
#33626=CARTESIAN_POINT('Ctrl Pts',(-1.96171645503154,-4.13871335710024,
10.291888410258));
#33627=CARTESIAN_POINT('Ctrl Pts',(-2.63124905814445,-3.74884090035779,
10.2654311135735));
#33628=CARTESIAN_POINT('Ctrl Pts',(-3.16677114350303,-3.22259556396298,
10.2389738168891));
#33629=CARTESIAN_POINT('Ctrl Pts',(-3.70229322886161,-2.69635022756818,
10.2125165202046));
#33630=CARTESIAN_POINT('Ctrl Pts',(-4.10380479646586,-2.033732011521,10.1860592235201));
#33631=CARTESIAN_POINT('Ctrl Pts',(-4.32240218174696,-1.31544708119576,
10.1596019268357));
#33632=CARTESIAN_POINT('Ctrl Pts',(-4.54099956702807,-0.597162150870509,
10.1331446301512));
#33633=CARTESIAN_POINT('Ctrl Pts',(-4.57668276998605,0.176789493732823,
10.1066873334667));
#33634=CARTESIAN_POINT('Ctrl Pts',(-4.42510561599232,0.912141398858014,
10.0802300367823));
#33635=CARTESIAN_POINT('Ctrl Pts',(-4.27352846199858,1.64749330398323,10.0537727400978));
#33636=CARTESIAN_POINT('Ctrl Pts',(-3.93469095105313,2.34424546963029,10.0273154434133));
#33637=CARTESIAN_POINT('Ctrl Pts',(-3.44986311698706,2.91753425314077,10.0008581467289));
#33638=CARTESIAN_POINT('Ctrl Pts',(-2.965035282921,3.49082303665126,9.97440085004439));
#33639=CARTESIAN_POINT('Ctrl Pts',(-2.33421712573433,3.94064843802516,9.94794355335992));
#33640=CARTESIAN_POINT('Ctrl Pts',(-1.63424159882622,4.21222222121095,9.92148625667545));
#33641=CARTESIAN_POINT('Ctrl Pts',(-0.93426607191815,4.48379600439673,9.89502895999098));
#33642=CARTESIAN_POINT('Ctrl Pts',(-0.165133175288626,4.57711816939442,
9.86857166330652));
#33643=CARTESIAN_POINT('Ctrl Pts',(0.579477555476215,4.48082217978985,9.84211436662205));
#33644=CARTESIAN_POINT('Ctrl Pts',(1.32408828624107,4.38452619018528,9.81565706993759));
#33645=CARTESIAN_POINT('Ctrl Pts',(2.04417685114126,4.09861204597845,9.78919977325312));
#33646=CARTESIAN_POINT('Ctrl Pts',(2.65203725991646,3.65790377350364,9.76274247656865));
#33647=CARTESIAN_POINT('Ctrl Pts',(3.25989766869166,3.21719550102883,9.73628517988418));
#33648=CARTESIAN_POINT('Ctrl Pts',(3.75552992134187,2.62169310028604,9.70982788319971));
#33649=CARTESIAN_POINT('Ctrl Pts',(4.07856655802598,1.94392810462463,9.68337058651525));
#33650=CARTESIAN_POINT('Ctrl Pts',(4.36666460048778,1.33946797123696,9.65977482517416));
#33651=CARTESIAN_POINT('Ctrl Pts',(4.51748278690866,0.669577455247932,9.63617906383307));
#33652=CARTESIAN_POINT('Ctrl Pts',(4.51802315729813,-7.77880120685776E-5,
9.61258330249199));
#33653=CARTESIAN_POINT('Origin',(0.,0.,20.5));
#33654=CARTESIAN_POINT('',(4.51736326149566,6.46810088806768E-6,8.61258330249198));
#33655=CARTESIAN_POINT('',(4.51813428255233,-1.20076389504314E-5,8.88741669750808));
#33656=CARTESIAN_POINT('',(4.51775,5.53264807684796E-16,20.5));
#33657=CARTESIAN_POINT('Ctrl Pts',(4.51813428255233,-1.20076389504314E-5,
8.88741669750808));
#33658=CARTESIAN_POINT('Ctrl Pts',(4.51802118875718,0.73947229319191,8.91347479471178));
#33659=CARTESIAN_POINT('Ctrl Pts',(4.3327730937107,1.47901118956561,8.93953289191547));
#33660=CARTESIAN_POINT('Ctrl Pts',(3.9839812468855,2.13106899669204,8.96559098911917));
#33661=CARTESIAN_POINT('Ctrl Pts',(3.62984605042663,2.79311606496825,8.99204828580364));
#33662=CARTESIAN_POINT('Ctrl Pts',(3.10711787221281,3.36498116344761,9.01850558248812));
#33663=CARTESIAN_POINT('Ctrl Pts',(2.47946442583089,3.77701175603631,9.04496287917258));
#33664=CARTESIAN_POINT('Ctrl Pts',(1.85181097944898,4.189042348625,9.07142017585705));
#33665=CARTESIAN_POINT('Ctrl Pts',(1.11923226489897,4.44123843532303,9.09787747254152));
#33666=CARTESIAN_POINT('Ctrl Pts',(0.370955558845314,4.50288281188386,9.12433476922598));
#33667=CARTESIAN_POINT('Ctrl Pts',(-0.377321147208358,4.5645271884447,9.15079206591045));
#33668=CARTESIAN_POINT('Ctrl Pts',(-1.14129584476571,4.43561985486832,9.17724936259492));
#33669=CARTESIAN_POINT('Ctrl Pts',(-1.82791726117885,4.13186158171856,9.20370665927939));
#33670=CARTESIAN_POINT('Ctrl Pts',(-2.51453867759199,3.82810330856881,9.23016395596386));
#33671=CARTESIAN_POINT('Ctrl Pts',(-3.12380681286095,3.34949409584567,9.25662125264832));
#33672=CARTESIAN_POINT('Ctrl Pts',(-3.58151348240605,2.75432801596707,9.28307854933279));
#33673=CARTESIAN_POINT('Ctrl Pts',(-4.03922015195113,2.15916193608848,9.30953584601726));
#33674=CARTESIAN_POINT('Ctrl Pts',(-4.34536535577235,1.44743898905445,9.33599314270173));
#33675=CARTESIAN_POINT('Ctrl Pts',(-4.46266094686473,0.705846242127692,
9.3624504393862));
#33676=CARTESIAN_POINT('Ctrl Pts',(-4.57995653795712,-0.0357465047990668,
9.38890773607066));
#33677=CARTESIAN_POINT('Ctrl Pts',(-4.50840251632067,-0.807209051618545,
9.41536503275513));
#33678=CARTESIAN_POINT('Ctrl Pts',(-4.25671408259964,-1.51457811392983,
9.4418223294396));
#33679=CARTESIAN_POINT('Ctrl Pts',(-4.00502564887861,-2.22194717624114,
9.46827962612407));
#33680=CARTESIAN_POINT('Ctrl Pts',(-3.57320280307299,-2.86522275404424,
9.49473692280854));
#33681=CARTESIAN_POINT('Ctrl Pts',(-3.01384108989007,-3.36605459389589,
9.521194219493));
#33682=CARTESIAN_POINT('Ctrl Pts',(-2.45447937670717,-3.86688643374753,
9.54765151617747));
#33683=CARTESIAN_POINT('Ctrl Pts',(-1.76757879614698,-4.22527453564772,
9.57410881286193));
#33684=CARTESIAN_POINT('Ctrl Pts',(-1.03680307870741,-4.39756762542433,
9.6005661095464));
#33685=CARTESIAN_POINT('Ctrl Pts',(-0.306027361267855,-4.56986071520094,
9.62702340623087));
#33686=CARTESIAN_POINT('Ctrl Pts',(0.468623493051109,-4.55605879285398,
9.65348070291534));
#33687=CARTESIAN_POINT('Ctrl Pts',(1.19279786752367,-4.35784291725027,9.67993799959981));
#33688=CARTESIAN_POINT('Ctrl Pts',(1.91697224199627,-4.15962704164656,9.70639529628428));
#33689=CARTESIAN_POINT('Ctrl Pts',(2.59067013662248,-3.7769972127861,9.73285259296875));
#33690=CARTESIAN_POINT('Ctrl Pts',(3.13183589343935,-3.25655732035571,9.75930988965321));
#33691=CARTESIAN_POINT('Ctrl Pts',(3.67300165025619,-2.73611742792533,9.78576718633768));
#33692=CARTESIAN_POINT('Ctrl Pts',(4.08163526926369,-2.07786747192505,9.81222448302215));
#33693=CARTESIAN_POINT('Ctrl Pts',(4.30796562791432,-1.3619815684899,9.83868177970662));
#33694=CARTESIAN_POINT('Ctrl Pts',(4.44693411433176,-0.922422416809593,
9.8549267523071));
#33695=CARTESIAN_POINT('Ctrl Pts',(4.51717337249904,-0.461134228693464,
9.87117172490759));
#33696=CARTESIAN_POINT('Ctrl Pts',(4.5174420818448,7.39595355181285E-5,
9.88741669750808));
#33697=CARTESIAN_POINT('Ctrl Pts',(4.51802315729813,-7.77880120685776E-5,
9.61258330249199));
#33698=CARTESIAN_POINT('Ctrl Pts',(4.51808868978702,-0.081289075021137,
9.60972176714861));
#33699=CARTESIAN_POINT('Ctrl Pts',(4.51594405515544,-0.162496901825208,
9.60686023180522));
#33700=CARTESIAN_POINT('Ctrl Pts',(4.51156607035433,-0.243584147729178,
9.60399869646184));
#33701=CARTESIAN_POINT('Ctrl Pts',(4.47108792528055,-0.993303813841435,
9.57754139977738));
#33702=CARTESIAN_POINT('Ctrl Pts',(4.23969061441499,-1.73271555548592,9.5510841030929));
#33703=CARTESIAN_POINT('Ctrl Pts',(3.84555807412645,-2.37175984086041,9.52462680640843));
#33704=CARTESIAN_POINT('Ctrl Pts',(3.45142553383792,-3.0108041262349,9.49816950972396));
#33705=CARTESIAN_POINT('Ctrl Pts',(2.8945577641264,-3.54948095533939,9.47171221303951));
#33706=CARTESIAN_POINT('Ctrl Pts',(2.24278064303981,-3.92218008655942,9.44525491635504));
#33707=CARTESIAN_POINT('Ctrl Pts',(1.59100352195321,-4.29487921777947,9.41879761967057));
#33708=CARTESIAN_POINT('Ctrl Pts',(0.844317049491529,-4.50160065111505,
9.3923403229861));
#33709=CARTESIAN_POINT('Ctrl Pts',(0.0936668116193721,-4.51716594477095,
9.36588302630163));
#33710=CARTESIAN_POINT('Ctrl Pts',(-0.656983426252764,-4.53273123842686,
9.33942572961716));
#33711=CARTESIAN_POINT('Ctrl Pts',(-1.41159742953537,-4.3571403924031,9.3129684329327));
#33712=CARTESIAN_POINT('Ctrl Pts',(-2.07826404778352,-4.01178017741349,
9.28651113624823));
#33713=CARTESIAN_POINT('Ctrl Pts',(-2.74493066603167,-3.66641996242389,
9.26005383956376));
#33714=CARTESIAN_POINT('Ctrl Pts',(-3.32364989924536,-3.15129037846845,
9.23359654287929));
#33715=CARTESIAN_POINT('Ctrl Pts',(-3.7439343853058,-2.52913363876293,9.20713924619482));
#33716=CARTESIAN_POINT('Ctrl Pts',(-4.16421887136626,-1.9069768990574,9.18068194951035));
#33717=CARTESIAN_POINT('Ctrl Pts',(-4.42606861027347,-1.1777930036018,9.15422465282589));
#33718=CARTESIAN_POINT('Ctrl Pts',(-4.49759059362582,-0.430395743852028,
9.12776735614142));
#33719=CARTESIAN_POINT('Ctrl Pts',(-4.56911257697816,0.317001515897712,
9.10131005945695));
#33720=CARTESIAN_POINT('Ctrl Pts',(-4.45030680477565,1.08261213994165,9.07485276277248));
#33721=CARTESIAN_POINT('Ctrl Pts',(-4.15564368858649,1.77318560159636,9.04839546608801));
#33722=CARTESIAN_POINT('Ctrl Pts',(-3.86098057239734,2.46375906325108,9.02193816940354));
#33723=CARTESIAN_POINT('Ctrl Pts',(-3.39046011222153,3.0792953625166,8.99548087271908));
#33724=CARTESIAN_POINT('Ctrl Pts',(-2.8013911793688,3.54482285937563,8.96902357603462));
#33725=CARTESIAN_POINT('Ctrl Pts',(-2.21232224651606,4.01035035623468,8.94256627935015));
#33726=CARTESIAN_POINT('Ctrl Pts',(-1.50470484098639,4.32586905068723,8.91610898266568));
#33727=CARTESIAN_POINT('Ctrl Pts',(-0.76472597963103,4.45294911494335,8.88965168598121));
#33728=CARTESIAN_POINT('Ctrl Pts',(-0.0247471182756658,4.58002917919947,
8.86319438929674));
#33729=CARTESIAN_POINT('Ctrl Pts',(0.747593198905389,4.51867061325916,8.83673709261227));
#33730=CARTESIAN_POINT('Ctrl Pts',(1.45822477605263,4.27634682254651,8.8102797959278));
#33731=CARTESIAN_POINT('Ctrl Pts',(2.16885635319985,4.03402303183387,8.78382249924334));
#33732=CARTESIAN_POINT('Ctrl Pts',(2.81777919031325,3.6107340163489,8.75736520255887));
#33733=CARTESIAN_POINT('Ctrl Pts',(3.3259552040156,3.0580359097105,8.7309079058744));
#33734=CARTESIAN_POINT('Ctrl Pts',(3.83413121771795,2.5053378030721,8.70445060918993));
#33735=CARTESIAN_POINT('Ctrl Pts',(4.20156040800925,1.82323060528026,8.67799331250546));
#33736=CARTESIAN_POINT('Ctrl Pts',(4.38349030615737,1.0947942181167,8.65153601582099));
#33737=CARTESIAN_POINT('Ctrl Pts',(4.47277460017851,0.737305266442263,8.63855177804465));
#33738=CARTESIAN_POINT('Ctrl Pts',(4.51738186963902,0.368658049377594,8.62556754026832));
#33739=CARTESIAN_POINT('Ctrl Pts',(4.51736350124836,6.46409108656654E-6,
8.61258330249198));
#33740=CARTESIAN_POINT('Origin',(0.,0.,20.5));
#33741=CARTESIAN_POINT('',(4.51805554098247,6.65521552928316E-5,7.61258330249197));
#33742=CARTESIAN_POINT('',(4.51740628246061,-5.63430382605529E-5,7.88741669750807));
#33743=CARTESIAN_POINT('',(4.51775,5.53264807684796E-16,20.5));
#33744=CARTESIAN_POINT('Ctrl Pts',(4.51740628246061,-5.63430382605529E-5,
7.88741669750807));
#33745=CARTESIAN_POINT('Ctrl Pts',(4.51721359264065,0.438494588092411,7.90286327114702));
#33746=CARTESIAN_POINT('Ctrl Pts',(4.45380791076361,0.877100051477632,7.91830984478598));
#33747=CARTESIAN_POINT('Ctrl Pts',(4.32797411068275,1.29699720179238,7.93375641842493));
#33748=CARTESIAN_POINT('Ctrl Pts',(4.1124426757192,2.01620805997421,7.9602137151094));
#33749=CARTESIAN_POINT('Ctrl Pts',(3.71376126713352,2.68053296061069,7.98667101179386));
#33750=CARTESIAN_POINT('Ctrl Pts',(3.18048883925826,3.20905786603343,8.01312830847833));
#33751=CARTESIAN_POINT('Ctrl Pts',(2.64721641138298,3.73758277145619,8.0395856051628));
#33752=CARTESIAN_POINT('Ctrl Pts',(1.97935296421813,4.13030768166519,8.06604290184727));
#33753=CARTESIAN_POINT('Ctrl Pts',(1.25824352648304,4.33939913723789,8.09250019853174));
#33754=CARTESIAN_POINT('Ctrl Pts',(0.53713408874796,4.54849059281059,8.11895749521621));
#33755=CARTESIAN_POINT('Ctrl Pts',(-0.237221339557352,4.57394859374699,
8.14541479190067));
#33756=CARTESIAN_POINT('Ctrl Pts',(-0.970507124268639,4.41267238370822,
8.17187208858514));
#33757=CARTESIAN_POINT('Ctrl Pts',(-1.70379290897991,4.25139617366945,8.19832938526961));
#33758=CARTESIAN_POINT('Ctrl Pts',(-2.39600905009715,3.90338575265551,8.22478668195408));
#33759=CARTESIAN_POINT('Ctrl Pts',(-2.96284438772951,3.4110284047919,8.25124397863854));
#33760=CARTESIAN_POINT('Ctrl Pts',(-3.52967972536187,2.91867105692828,8.27770127532301));
#33761=CARTESIAN_POINT('Ctrl Pts',(-3.97113425950935,2.28196678221498,8.30415857200748));
#33762=CARTESIAN_POINT('Ctrl Pts',(-4.2334393164843,1.57846545665159,8.33061586869195));
#33763=CARTESIAN_POINT('Ctrl Pts',(-4.49574437345926,0.874964131088192,
8.35707316537641));
#33764=CARTESIAN_POINT('Ctrl Pts',(-4.57889995326168,0.104665754674698,
8.38353046206088));
#33765=CARTESIAN_POINT('Ctrl Pts',(-4.47277779830253,-0.638608182855007,
8.40998775874535));
#33766=CARTESIAN_POINT('Ctrl Pts',(-4.36665564334337,-1.38188212038471,
8.43644505542982));
#33767=CARTESIAN_POINT('Ctrl Pts',(-4.07125575362263,-2.09813161903063,
8.46290235211428));
#33768=CARTESIAN_POINT('Ctrl Pts',(-3.62255750878001,-2.70011828255337,
8.48935964879875));
#33769=CARTESIAN_POINT('Ctrl Pts',(-3.17385926393738,-3.30210494607612,
8.51581694548322));
#33770=CARTESIAN_POINT('Ctrl Pts',(-2.57186266397286,-3.78982877447569,
8.54227424216769));
#33771=CARTESIAN_POINT('Ctrl Pts',(-1.88989022851369,-4.10388554523221,
8.56873153885216));
#33772=CARTESIAN_POINT('Ctrl Pts',(-1.20791779305452,-4.41794231598872,
8.59518883553663));
#33773=CARTESIAN_POINT('Ctrl Pts',(-0.445969522100707,-4.55833202910218,
8.62164613222109));
#33774=CARTESIAN_POINT('Ctrl Pts',(0.30315012821752,-4.50795537288903,8.64810342890556));
#33775=CARTESIAN_POINT('Ctrl Pts',(1.05226977853573,-4.45757871667589,8.67456072559003));
#33776=CARTESIAN_POINT('Ctrl Pts',(1.78856080821834,-4.21643569113615,8.7010180222745));
#33777=CARTESIAN_POINT('Ctrl Pts',(2.42234378472631,-3.81389724990005,8.72747531895897));
#33778=CARTESIAN_POINT('Ctrl Pts',(3.05612676123428,-3.41135880866395,8.75393261564343));
#33779=CARTESIAN_POINT('Ctrl Pts',(3.58740168456759,-2.84742495173149,8.78038991232789));
#33780=CARTESIAN_POINT('Ctrl Pts',(3.95145985704281,-2.19078219875382,8.80684720901236));
#33781=CARTESIAN_POINT('Ctrl Pts',(4.31551802951803,-1.53413944577613,8.83330450569683));
#33782=CARTESIAN_POINT('Ctrl Pts',(4.51235945113515,-0.78478779675323,8.85976180238131));
#33783=CARTESIAN_POINT('Ctrl Pts',(4.51800905459174,-0.0339974532052447,
8.88621909906578));
#33784=CARTESIAN_POINT('Ctrl Pts',(4.51809429832594,-0.0226691939774265,
8.88661829854654));
#33785=CARTESIAN_POINT('Ctrl Pts',(4.5181360151034,-0.0113406072147017,
8.88701749802731));
#33786=CARTESIAN_POINT('Ctrl Pts',(4.51813428255233,-1.20076389504314E-5,
8.88741669750808));
#33787=CARTESIAN_POINT('Ctrl Pts',(4.51736350124836,6.46409108656654E-6,
8.61258330249198));
#33788=CARTESIAN_POINT('Ctrl Pts',(4.5173444413379,-0.382523847714403,8.59911024358385));
#33789=CARTESIAN_POINT('Ctrl Pts',(4.46927642784078,-0.765058862836159,
8.58563718467573));
#33790=CARTESIAN_POINT('Ctrl Pts',(4.37321687241043,-1.13513692172449,8.5721641257676));
#33791=CARTESIAN_POINT('Ctrl Pts',(4.18458293451042,-1.86186609786678,8.54570682908313));
#33792=CARTESIAN_POINT('Ctrl Pts',(3.81088445270546,-2.54055887361605,8.51924953239865));
#33793=CARTESIAN_POINT('Ctrl Pts',(3.29763748849563,-3.08855122001653,8.49279223571418));
#33794=CARTESIAN_POINT('Ctrl Pts',(2.78439052428581,-3.636543566417,8.46633493902971));
#33795=CARTESIAN_POINT('Ctrl Pts',(2.13159507767111,-4.05383548346868,8.43987764234525));
#33796=CARTESIAN_POINT('Ctrl Pts',(1.4187609115801,-4.28960127750468,8.41342034566079));
#33797=CARTESIAN_POINT('Ctrl Pts',(0.705926745489094,-4.52536707154067,
8.38696304897632));
#33798=CARTESIAN_POINT('Ctrl Pts',(-0.0669461400782259,-4.57960674256099,
8.36050575229184));
#33799=CARTESIAN_POINT('Ctrl Pts',(-0.805722683022316,-4.44571395866409,
8.33404845560738));
#33800=CARTESIAN_POINT('Ctrl Pts',(-1.54449922596642,-4.31182117476718,
8.30759115892291));
#33801=CARTESIAN_POINT('Ctrl Pts',(-2.24917942628729,-3.98979593595305,
8.28113386223845));
#33802=CARTESIAN_POINT('Ctrl Pts',(-2.83393401547744,-3.51886055991386,
8.25467656555398));
#33803=CARTESIAN_POINT('Ctrl Pts',(-3.41868860466758,-3.04792518387468,
8.22821926886951));
#33804=CARTESIAN_POINT('Ctrl Pts',(-3.88351758272698,-2.42807967061047,
8.20176197218504));
#33805=CARTESIAN_POINT('Ctrl Pts',(-4.17180529456878,-1.73482051763438,
8.17530467550057));
#33806=CARTESIAN_POINT('Ctrl Pts',(-4.46009300641058,-1.0415613646583,8.1488473788161));
#33807=CARTESIAN_POINT('Ctrl Pts',(-4.57183945203477,-0.274888571970355,
8.12239008213164));
#33808=CARTESIAN_POINT('Ctrl Pts',(-4.49343403803759,0.471817962780769,
8.09593278544718));
#33809=CARTESIAN_POINT('Ctrl Pts',(-4.41502862404041,1.21852449753188,8.06947548876271));
#33810=CARTESIAN_POINT('Ctrl Pts',(-4.14647135042187,1.94526477434618,8.04301819207824));
#33811=CARTESIAN_POINT('Ctrl Pts',(-3.72047219588799,2.56352263181385,8.01656089539377));
#33812=CARTESIAN_POINT('Ctrl Pts',(-3.2944730413541,3.18178048928153,7.9901035987093));
#33813=CARTESIAN_POINT('Ctrl Pts',(-2.71103200590485,3.69155592740257,7.96364630202483));
#33814=CARTESIAN_POINT('Ctrl Pts',(-2.04121156194556,4.03075886199821,7.93718900534037));
#33815=CARTESIAN_POINT('Ctrl Pts',(-1.37139111798628,4.36996179659386,7.9107317086559));
#33816=CARTESIAN_POINT('Ctrl Pts',(-0.615191265516958,4.53859222766412,
7.88427441197143));
#33817=CARTESIAN_POINT('Ctrl Pts',(0.135283690341632,4.5161111553332,7.85781711528696));
#33818=CARTESIAN_POINT('Ctrl Pts',(0.885758646200222,4.49363008300228,7.83135981860249));
#33819=CARTESIAN_POINT('Ctrl Pts',(1.63050870544808,4.28003750727018,7.80490252191802));
#33820=CARTESIAN_POINT('Ctrl Pts',(2.27882413510697,3.90134876747149,7.77844522523355));
#33821=CARTESIAN_POINT('Ctrl Pts',(2.92713956476585,3.52266002767282,7.75198792854908));
#33822=CARTESIAN_POINT('Ctrl Pts',(3.47902036483576,2.97887512380756,7.72553063186463));
#33823=CARTESIAN_POINT('Ctrl Pts',(3.8672480646519,2.33622645534278,7.69907333518016));
#33824=CARTESIAN_POINT('Ctrl Pts',(4.25547576446805,1.69357778687799,7.67261603849569));
#33825=CARTESIAN_POINT('Ctrl Pts',(4.48005036403042,0.952065353813674,7.64615874181121));
#33826=CARTESIAN_POINT('Ctrl Pts',(4.51361892565605,0.202004549842097,7.61970144512674));
#33827=CARTESIAN_POINT('Ctrl Pts',(4.51662938451667,0.134738420941428,7.61732873091515));
#33828=CARTESIAN_POINT('Ctrl Pts',(4.51810364598245,0.0674035403653694,
7.61495601670356));
#33829=CARTESIAN_POINT('Ctrl Pts',(4.51805554098247,6.65521552928316E-5,
7.61258330249197));
#33830=CARTESIAN_POINT('Origin',(0.,0.,20.5));
#33831=CARTESIAN_POINT('',(4.51756917096255,-0.000106270599391639,6.61258330249198));
#33832=CARTESIAN_POINT('',(4.5178629555887,0.000109594847417262,6.88741669750807));
#33833=CARTESIAN_POINT('',(4.51775,5.53264807684796E-16,20.5));
#33834=CARTESIAN_POINT('Ctrl Pts',(4.5178629555887,0.000109594847417262,
6.88741669750807));
#33835=CARTESIAN_POINT('Ctrl Pts',(4.51800230500779,0.137343923060939,6.89225174758228));
#33836=CARTESIAN_POINT('Ctrl Pts',(4.5118734339612,0.274565850873291,6.89708679765648));
#33837=CARTESIAN_POINT('Ctrl Pts',(4.4993855978694,0.411206621885887,6.90192184773068));
#33838=CARTESIAN_POINT('Ctrl Pts',(4.43105241013461,1.15890217051388,6.92837914441515));
#33839=CARTESIAN_POINT('Ctrl Pts',(4.17231550636749,1.88919639463632,6.95483644109962));
#33840=CARTESIAN_POINT('Ctrl Pts',(3.75468875509468,2.51314026599451,6.98129373778408));
#33841=CARTESIAN_POINT('Ctrl Pts',(3.33706200382187,3.13708413735269,7.00775103446855));
#33842=CARTESIAN_POINT('Ctrl Pts',(2.76054540504339,3.6546776559466,7.03420833115302));
#33843=CARTESIAN_POINT('Ctrl Pts',(2.09535804244149,4.00287850404845,7.06066562783749));
#33844=CARTESIAN_POINT('Ctrl Pts',(1.4301706798396,4.35107935215029,7.08712292452196));
#33845=CARTESIAN_POINT('Ctrl Pts',(0.676312553414283,4.52988752976006,7.11358022120642));
#33846=CARTESIAN_POINT('Ctrl Pts',(-0.074397251354124,4.51752439873747,
7.14003751789089));
#33847=CARTESIAN_POINT('Ctrl Pts',(-0.82510705612252,4.50516126771487,7.16649481457536));
#33848=CARTESIAN_POINT('Ctrl Pts',(-1.57266853923404,4.30162682805993,7.19295211125983));
#33849=CARTESIAN_POINT('Ctrl Pts',(-2.22602953939534,3.93171134926469,7.2194094079443));
#33850=CARTESIAN_POINT('Ctrl Pts',(-2.87939053955664,3.56179587046945,7.24586670462877));
#33851=CARTESIAN_POINT('Ctrl Pts',(-3.43855105676772,3.0254993525339,7.27232400131323));
#33852=CARTESIAN_POINT('Ctrl Pts',(-3.83540595887268,2.38814211780651,7.2987812979977));
#33853=CARTESIAN_POINT('Ctrl Pts',(-4.23226086097764,1.7507848830791,7.32523859468216));
#33854=CARTESIAN_POINT('Ctrl Pts',(-4.46681014797648,1.01236693155982,7.35169589136664));
#33855=CARTESIAN_POINT('Ctrl Pts',(-4.51048597629575,0.26282675251353,7.37815318805111));
#33856=CARTESIAN_POINT('Ctrl Pts',(-4.55416180461501,-0.486713426532748,
7.40461048473557));
#33857=CARTESIAN_POINT('Ctrl Pts',(-4.40696417425471,-1.24737583310602,
7.43106778142003));
#33858=CARTESIAN_POINT('Ctrl Pts',(-4.08682159368453,-1.92651262793454,
7.4575250781045));
#33859=CARTESIAN_POINT('Ctrl Pts',(-3.76667901311434,-2.60564942276306,
7.48398237478897));
#33860=CARTESIAN_POINT('Ctrl Pts',(-3.27359148233425,-3.20326060584682,
7.51043967147344));
#33861=CARTESIAN_POINT('Ctrl Pts',(-2.66761651687792,-3.64655779648116,
7.53689696815791));
#33862=CARTESIAN_POINT('Ctrl Pts',(-2.06164155142159,-4.0898549871155,7.56335426484238));
#33863=CARTESIAN_POINT('Ctrl Pts',(-1.342779151289,-4.37883818530042,7.58981156152685));
#33864=CARTESIAN_POINT('Ctrl Pts',(-0.59858596122885,-4.47830955732374,
7.61626885821132));
#33865=CARTESIAN_POINT('Ctrl Pts',(0.145607228831289,-4.57778092934705,
7.64272615489578));
#33866=CARTESIAN_POINT('Ctrl Pts',(0.915131208818995,-4.48774047520876,
7.66918345158024));
#33867=CARTESIAN_POINT('Ctrl Pts',(1.61625880962798,-4.21915502257233,7.69564074826471));
#33868=CARTESIAN_POINT('Ctrl Pts',(2.31738641043699,-3.95056956993589,7.72209804494918));
#33869=CARTESIAN_POINT('Ctrl Pts',(2.95011763206728,-3.5034391188013,7.74855534163365));
#33870=CARTESIAN_POINT('Ctrl Pts',(3.43738651198769,-2.93222366326352,7.77501263831812));
#33871=CARTESIAN_POINT('Ctrl Pts',(3.92465539190809,-2.36100820772573,7.80146993500259));
#33872=CARTESIAN_POINT('Ctrl Pts',(4.2664619301186,-1.66570774778476,7.82792723168706));
#33873=CARTESIAN_POINT('Ctrl Pts',(4.42117446855315,-0.931009109950678,
7.85438452837153));
#33874=CARTESIAN_POINT('Ctrl Pts',(4.4855611265208,-0.625249858747316,7.86539525141704));
#33875=CARTESIAN_POINT('Ctrl Pts',(4.51754363682092,-0.312666955391513,
7.87640597446256));
#33876=CARTESIAN_POINT('Ctrl Pts',(4.51740628246061,-5.63430382605529E-5,
7.88741669750807));
#33877=CARTESIAN_POINT('Ctrl Pts',(4.51805554098247,6.65521552928316E-5,
7.61258330249197));
#33878=CARTESIAN_POINT('Ctrl Pts',(4.51756724414766,-0.683447390694716,
7.58849872001909));
#33879=CARTESIAN_POINT('Ctrl Pts',(4.36022097756292,-1.36717849491845,7.56441413754622));
#33880=CARTESIAN_POINT('Ctrl Pts',(4.06048220709641,-1.98142521687064,7.54032955507335));
#33881=CARTESIAN_POINT('Ctrl Pts',(3.73121440322227,-2.65618500473295,7.51387225838888));
#33882=CARTESIAN_POINT('Ctrl Pts',(3.23011627178511,-3.24709540557874,7.48741496170441));
#33883=CARTESIAN_POINT('Ctrl Pts',(2.61822101061302,-3.68218418656399,7.46095766501995));
#33884=CARTESIAN_POINT('Ctrl Pts',(2.00632574944092,-4.11727296754925,7.43450036833548));
#33885=CARTESIAN_POINT('Ctrl Pts',(1.28363335853389,-4.39654012867397,7.40804307165101));
#33886=CARTESIAN_POINT('Ctrl Pts',(0.538166971278164,-4.48597123878683,
7.38158577496654));
#33887=CARTESIAN_POINT('Ctrl Pts',(-0.207299415977548,-4.57540234889969,
7.35512847828207));
#33888=CARTESIAN_POINT('Ctrl Pts',(-0.975539799581951,-4.47499740800071,
7.3286711815976));
#33889=CARTESIAN_POINT('Ctrl Pts',(-1.67298335104765,-4.1969856267701,7.30221388491313));
#33890=CARTESIAN_POINT('Ctrl Pts',(-2.37042690251334,-3.91897384553948,
7.27575658822867));
#33891=CARTESIAN_POINT('Ctrl Pts',(-2.99707362184033,-3.46335522397723,
7.2492992915442));
#33892=CARTESIAN_POINT('Ctrl Pts',(-3.47659863214408,-2.88562360594227,
7.22284199485973));
#33893=CARTESIAN_POINT('Ctrl Pts',(-3.95612364244783,-2.30789198790732,
7.19638469817527));
#33894=CARTESIAN_POINT('Ctrl Pts',(-4.28852694372834,-1.60804737339967,
7.1699274014908));
#33895=CARTESIAN_POINT('Ctrl Pts',(-4.43332218177076,-0.871330061926449,
7.14347010480633));
#33896=CARTESIAN_POINT('Ctrl Pts',(-4.57811741981318,-0.134612750453221,
7.11701280812186));
#33897=CARTESIAN_POINT('Ctrl Pts',(-4.53530459461751,0.63897725798557,7.09055551143739));
#33898=CARTESIAN_POINT('Ctrl Pts',(-4.31009826091029,1.3552175565183,7.06409821475293));
#33899=CARTESIAN_POINT('Ctrl Pts',(-4.08489192720307,2.07145785505103,7.03764091806846));
#33900=CARTESIAN_POINT('Ctrl Pts',(-3.67729208498431,2.7303484436777,7.01118362138399));
#33901=CARTESIAN_POINT('Ctrl Pts',(-3.13694394393276,3.25163717791837,6.98472632469952));
#33902=CARTESIAN_POINT('Ctrl Pts',(-2.59659580288121,3.77292591215904,6.95826902801505));
#33903=CARTESIAN_POINT('Ctrl Pts',(-1.92349936299689,4.15661279201372,6.93181173133059));
#33904=CARTESIAN_POINT('Ctrl Pts',(-1.19963702572085,4.35596518015434,6.90535443464612));
#33905=CARTESIAN_POINT('Ctrl Pts',(-0.475774688444814,4.55531756829496,
6.87889713796165));
#33906=CARTESIAN_POINT('Ctrl Pts',(0.298853546222961,4.57033546472154,6.85243984127718));
#33907=CARTESIAN_POINT('Ctrl Pts',(1.02989881660515,4.39918970627009,6.82598254459271));
#33908=CARTESIAN_POINT('Ctrl Pts',(1.76094408698735,4.22804394781863,6.79952524790824));
#33909=CARTESIAN_POINT('Ctrl Pts',(2.44840639308396,3.87073453448917,6.77306795122378));
#33910=CARTESIAN_POINT('Ctrl Pts',(3.00855358684847,3.37078135737971,6.74661065453931));
#33911=CARTESIAN_POINT('Ctrl Pts',(3.56870078061298,2.87082818027025,6.72015335785485));
#33912=CARTESIAN_POINT('Ctrl Pts',(4.00153286204536,2.22823123938082,6.69369606117038));
#33913=CARTESIAN_POINT('Ctrl Pts',(4.25433136265593,1.52125813092963,6.66723876448591));
#33914=CARTESIAN_POINT('Ctrl Pts',(4.42840834170919,1.03443663992461,6.6490202771546));
#33915=CARTESIAN_POINT('Ctrl Pts',(4.51711887209743,0.517089928133967,6.63080178982329));
#33916=CARTESIAN_POINT('Ctrl Pts',(4.51756917096255,-0.000106270599391639,
6.61258330249198));
#33917=CARTESIAN_POINT('Origin',(0.,0.,20.5));
#33918=CARTESIAN_POINT('',(4.51761916309611,0.000112359330087797,5.61258330249198));
#33919=CARTESIAN_POINT('',(4.51777856404949,-0.00011613542669066,5.88741669750807));
#33920=CARTESIAN_POINT('',(4.51775,5.53264807684796E-16,20.5));
#33921=CARTESIAN_POINT('Ctrl Pts',(4.51777856404949,-0.00011613542669066,
5.88741669750807));
#33922=CARTESIAN_POINT('Ctrl Pts',(4.51717292408202,0.586903980160037,5.90809752070199));
#33923=CARTESIAN_POINT('Ctrl Pts',(4.40219918284471,1.17415437942607,5.92877834389592));
#33924=CARTESIAN_POINT('Ctrl Pts',(4.17916749942524,1.71700921836349,5.94945916708984));
#33925=CARTESIAN_POINT('Ctrl Pts',(3.89383962040738,2.41149180233464,5.97591646377431));
#33926=CARTESIAN_POINT('Ctrl Pts',(3.43165892348727,3.03331448007484,6.00237376045877));
#33927=CARTESIAN_POINT('Ctrl Pts',(2.84891850603996,3.50673993762589,6.02883105714324));
#33928=CARTESIAN_POINT('Ctrl Pts',(2.26617808859264,3.98016539517695,6.05528835382771));
#33929=CARTESIAN_POINT('Ctrl Pts',(1.56287795061812,4.30519363253886,6.08174565051218));
#33930=CARTESIAN_POINT('Ctrl Pts',(0.82467927055748,4.44223657011985,6.10820294719664));
#33931=CARTESIAN_POINT('Ctrl Pts',(0.086480590496836,4.57927950770083,6.13466024388111));
#33932=CARTESIAN_POINT('Ctrl Pts',(-0.686616631649936,4.5283371455009,6.16111754056558));
#33933=CARTESIAN_POINT('Ctrl Pts',(-1.4004500098362,4.29561420685648,6.18757483725005));
#33934=CARTESIAN_POINT('Ctrl Pts',(-2.11428338802246,4.06289126821206,6.21403213393451));
#33935=CARTESIAN_POINT('Ctrl Pts',(-2.76885292224821,3.64838775312316,6.24048943061899));
#33936=CARTESIAN_POINT('Ctrl Pts',(-3.28443276767729,3.10258973098363,6.26694672730345));
#33937=CARTESIAN_POINT('Ctrl Pts',(-3.80001261310638,2.5567917088441,6.29340402398792));
#33938=CARTESIAN_POINT('Ctrl Pts',(-4.1766027697388,1.87969917965394,6.31986132067238));
#33939=CARTESIAN_POINT('Ctrl Pts',(-4.36833497328082,1.15378126410905,6.34631861735685));
#33940=CARTESIAN_POINT('Ctrl Pts',(-4.56006717682283,0.427863348564182,
6.37277591404132));
#33941=CARTESIAN_POINT('Ctrl Pts',(-4.56694142727444,-0.346879953335408,
6.39923321072579));
#33942=CARTESIAN_POINT('Ctrl Pts',(-4.38812044853859,-1.07608576485095,
6.42569050741026));
#33943=CARTESIAN_POINT('Ctrl Pts',(-4.20929946980274,-1.80529157636651,
6.45214780409473));
#33944=CARTESIAN_POINT('Ctrl Pts',(-3.84478326187941,-2.48895989749803,
6.4786051007792));
#33945=CARTESIAN_POINT('Ctrl Pts',(-3.33896949547221,-3.04382068336875,
6.50506239746367));
#33946=CARTESIAN_POINT('Ctrl Pts',(-2.83315572906502,-3.59868146923946,
6.53151969414813));
#33947=CARTESIAN_POINT('Ctrl Pts',(-2.18604440417397,-4.02473471984939,
6.55797699083259));
#33948=CARTESIAN_POINT('Ctrl Pts',(-1.47645296399246,-4.27008762080069,
6.58443428751706));
#33949=CARTESIAN_POINT('Ctrl Pts',(-0.766861523810935,-4.51544052175199,
6.61089158420153));
#33950=CARTESIAN_POINT('Ctrl Pts',(0.00521003166104095,-4.58009307304465,
6.637348880886));
#33951=CARTESIAN_POINT('Ctrl Pts',(0.745724241442684,-4.45617066548422,
6.66380617757047));
#33952=CARTESIAN_POINT('Ctrl Pts',(1.48623845122433,-4.3322482579238,6.69026347425494));
#33953=CARTESIAN_POINT('Ctrl Pts',(2.19519531531564,-4.01975089151029,6.7167207709394));
#33954=CARTESIAN_POINT('Ctrl Pts',(2.78624467229499,-3.55674039962227,6.74317806762387));
#33955=CARTESIAN_POINT('Ctrl Pts',(3.37729402927435,-3.09372990773424,6.76963536430834));
#33956=CARTESIAN_POINT('Ctrl Pts',(3.85043587914176,-2.4802062903717,6.79609266099281));
#33957=CARTESIAN_POINT('Ctrl Pts',(4.14804206822422,-1.79089604512366,6.82254995767728));
#33958=CARTESIAN_POINT('Ctrl Pts',(4.39126096128897,-1.22755670280584,6.84417220428754));
#33959=CARTESIAN_POINT('Ctrl Pts',(4.51723978779142,-0.613599558623174,
6.86579445089781));
#33960=CARTESIAN_POINT('Ctrl Pts',(4.5178629555887,0.000109594847417262,
6.88741669750807));
#33961=CARTESIAN_POINT('Ctrl Pts',(4.51756917096255,-0.000106270599391639,
6.61258330249198));
#33962=CARTESIAN_POINT('Ctrl Pts',(4.51777280622788,-0.233994013420898,
6.60434449313882));
#33963=CARTESIAN_POINT('Ctrl Pts',(4.49992676845961,-0.467850975545092,
6.59610568378566));
#33964=CARTESIAN_POINT('Ctrl Pts',(4.46376343532316,-0.698840208967197,
6.5878668744325));
#33965=CARTESIAN_POINT('Ctrl Pts',(4.34763208759105,-1.44061616439985,6.56140957774804));
#33966=CARTESIAN_POINT('Ctrl Pts',(4.04260447233807,-2.15281879925221,6.53495228106357));
#33967=CARTESIAN_POINT('Ctrl Pts',(3.58583261551844,-2.74870262081615,6.5084949843791));
#33968=CARTESIAN_POINT('Ctrl Pts',(3.1290607586988,-3.3445864423801,6.48203768769463));
#33969=CARTESIAN_POINT('Ctrl Pts',(2.52054466031253,-3.82415145065562,6.45558039101016));
#33970=CARTESIAN_POINT('Ctrl Pts',(1.83440090767928,-4.12898715838434,6.42912309432569));
#33971=CARTESIAN_POINT('Ctrl Pts',(1.14825715504604,-4.43382286611306,6.40266579764122));
#33972=CARTESIAN_POINT('Ctrl Pts',(0.384485748165844,-4.56392927329498,
6.37620850095676));
#33973=CARTESIAN_POINT('Ctrl Pts',(-0.363886800892981,-4.50345956352816,
6.34975120427229));
#33974=CARTESIAN_POINT('Ctrl Pts',(-1.11225934995183,-4.44298985376135,
6.32329390758782));
#33975=CARTESIAN_POINT('Ctrl Pts',(-1.84523304118933,-4.19194402704577,
6.29683661090335));
#33976=CARTESIAN_POINT('Ctrl Pts',(-2.47353249021757,-3.78089918723516,
6.27037931421889));
#33977=CARTESIAN_POINT('Ctrl Pts',(-3.10183193924579,-3.36985434742456,
6.24392201753442));
#33978=CARTESIAN_POINT('Ctrl Pts',(-3.62545714606476,-2.79881049451895,
6.21746472084996));
#33979=CARTESIAN_POINT('Ctrl Pts',(-3.98063113999636,-2.13732013781012,
6.19100742416549));
#33980=CARTESIAN_POINT('Ctrl Pts',(-4.33580513392796,-1.47582978110128,
6.16455012748102));
#33981=CARTESIAN_POINT('Ctrl Pts',(-4.52252791497214,-0.723892920589236,
6.13809283079655));
#33982=CARTESIAN_POINT('Ctrl Pts',(-4.51805685504966,0.0269053663076428,
6.11163553411208));
#33983=CARTESIAN_POINT('Ctrl Pts',(-4.51358579512718,0.777703653204501,
6.08517823742761));
#33984=CARTESIAN_POINT('Ctrl Pts',(-4.31792089423804,1.52736336648619,6.05872094074314));
#33985=CARTESIAN_POINT('Ctrl Pts',(-3.95489392076209,2.18457678274683,6.03226364405868));
#33986=CARTESIAN_POINT('Ctrl Pts',(-3.59186694728612,2.84179019900748,6.00580634737421));
#33987=CARTESIAN_POINT('Ctrl Pts',(-3.06147790122333,3.40655731824708,5.97934905068974));
#33988=CARTESIAN_POINT('Ctrl Pts',(-2.42832758138604,3.81009013038763,5.95289175400527));
#33989=CARTESIAN_POINT('Ctrl Pts',(-1.79517726154877,4.21362294252816,5.9264344573208));
#33990=CARTESIAN_POINT('Ctrl Pts',(-1.05926566793702,4.45592144756967,5.89997716063634));
#33991=CARTESIAN_POINT('Ctrl Pts',(-0.310226018196338,4.50747395575742,
5.87351986395187));
#33992=CARTESIAN_POINT('Ctrl Pts',(0.438813631544363,4.55902646394516,5.8470625672674));
#33993=CARTESIAN_POINT('Ctrl Pts',(1.20098133741399,4.41983297527914,5.82060527058293));
#33994=CARTESIAN_POINT('Ctrl Pts',(1.88344591635241,4.10684710262907,5.79414797389846));
#33995=CARTESIAN_POINT('Ctrl Pts',(2.56591049529081,3.79386122997902,5.767690677214));
#33996=CARTESIAN_POINT('Ctrl Pts',(3.16867194729802,3.30708297334494,5.74123338052953));
#33997=CARTESIAN_POINT('Ctrl Pts',(3.61831459461448,2.70580138565218,5.71477608384506));
#33998=CARTESIAN_POINT('Ctrl Pts',(4.06795724193093,2.10451979795941,5.68831878716059));
#33999=CARTESIAN_POINT('Ctrl Pts',(4.36448108455665,1.38873487920795,5.66186149047613));
#34000=CARTESIAN_POINT('Ctrl Pts',(4.47176984663199,0.645628440320207,5.63540419379166));
#34001=CARTESIAN_POINT('Ctrl Pts',(4.50261735669319,0.431971549265432,5.6277972300251));
#34002=CARTESIAN_POINT('Ctrl Pts',(4.51782138536506,0.216056072273327,5.62019026625854));
#34003=CARTESIAN_POINT('Ctrl Pts',(4.51761916309611,0.000112359330087797,
5.61258330249198));
#34004=CARTESIAN_POINT('Origin',(0.,0.,20.5));
#34005=CARTESIAN_POINT('',(4.51801297056466,-8.08487039419617E-5,4.61258330249197));
#34006=CARTESIAN_POINT('',(4.51744953111884,7.68816669171638E-5,4.88741669750807));
#34007=CARTESIAN_POINT('',(4.51775,5.53264807684796E-16,20.5));
#34008=CARTESIAN_POINT('Ctrl Pts',(4.51744953111884,7.68816669171638E-5,
4.88741669750807));
#34009=CARTESIAN_POINT('Ctrl Pts',(4.51762304095457,0.28595126409645,4.89748599713724));
#34010=CARTESIAN_POINT('Ctrl Pts',(4.49090928481679,0.571793625338861,4.90755529676642));
#34011=CARTESIAN_POINT('Ctrl Pts',(4.43699864797727,0.852411075740623,4.91762459639559));
#34012=CARTESIAN_POINT('Ctrl Pts',(4.2953473151299,1.58973933227679,4.94408189308006));
#34013=CARTESIAN_POINT('Ctrl Pts',(3.96593233939643,2.29099550010712,4.97053918976452));
#34014=CARTESIAN_POINT('Ctrl Pts',(3.48887610024735,2.87076735409198,4.99699648644899));
#34015=CARTESIAN_POINT('Ctrl Pts',(3.01181986109827,3.45053920807684,5.02345378313346));
#34016=CARTESIAN_POINT('Ctrl Pts',(2.38712235853358,3.90882674821622,5.04991107981793));
#34017=CARTESIAN_POINT('Ctrl Pts',(1.69087105699343,4.18981105932229,5.0763683765024));
#34018=CARTESIAN_POINT('Ctrl Pts',(0.994619755453274,4.47079537042835,5.10282567318686));
#34019=CARTESIAN_POINT('Ctrl Pts',(0.226814654937662,4.57447645250109,5.12928296987133));
#34020=CARTESIAN_POINT('Ctrl Pts',(-0.519026433064492,4.48822606449115,
5.1557402665558));
#34021=CARTESIAN_POINT('Ctrl Pts',(-1.26486752106665,4.40197567648121,5.18219756324027));
#34022=CARTESIAN_POINT('Ctrl Pts',(-1.98874459655534,4.12579381838858,5.20865485992474));
#34023=CARTESIAN_POINT('Ctrl Pts',(-2.60249023287342,3.69331913486986,5.2351121566092));
#34024=CARTESIAN_POINT('Ctrl Pts',(-3.21623586919149,3.26084445135114,5.26156945329367));
#34025=CARTESIAN_POINT('Ctrl Pts',(-3.71985006633895,2.67207694240634,5.28802674997814));
#34026=CARTESIAN_POINT('Ctrl Pts',(-4.05199317246879,1.99872783901753,5.31448404666261));
#34027=CARTESIAN_POINT('Ctrl Pts',(-4.38413627859864,1.32537873562872,5.34094134334707));
#34028=CARTESIAN_POINT('Ctrl Pts',(-4.54480829371086,0.567448037795898,
5.36739864003154));
#34029=CARTESIAN_POINT('Ctrl Pts',(-4.51443954418554,-0.182749134310455,
5.39385593671601));
#34030=CARTESIAN_POINT('Ctrl Pts',(-4.48407079466022,-0.932946306416809,
5.42031323340048));
#34031=CARTESIAN_POINT('Ctrl Pts',(-4.26266128049735,-1.6754099527967,5.44677053008495));
#34032=CARTESIAN_POINT('Ctrl Pts',(-3.87717843548113,-2.31970882302876,
5.47322782676942));
#34033=CARTESIAN_POINT('Ctrl Pts',(-3.49169559046492,-2.96400769326083,
5.49968512345388));
#34034=CARTESIAN_POINT('Ctrl Pts',(-2.94213941459537,-3.51014178734505,
5.52614242013835));
#34035=CARTESIAN_POINT('Ctrl Pts',(-2.29544524188241,-3.89159257704565,
5.55259971682282));
#34036=CARTESIAN_POINT('Ctrl Pts',(-1.64875106916946,-4.27304336674624,
5.57905701350729));
#34037=CARTESIAN_POINT('Ctrl Pts',(-0.904918899613081,-4.48981085206321,
5.60551431019175));
#34038=CARTESIAN_POINT('Ctrl Pts',(-0.154546668242997,-4.51549299318827,
5.63197160687622));
#34039=CARTESIAN_POINT('Ctrl Pts',(0.595825563127097,-4.54117513431334,
5.65842890356069));
#34040=CARTESIAN_POINT('Ctrl Pts',(1.35273785631093,-4.37577193124651,5.68488620024516));
#34041=CARTESIAN_POINT('Ctrl Pts',(2.02399913169717,-4.03942931106444,5.71134349692963));
#34042=CARTESIAN_POINT('Ctrl Pts',(2.69526040708341,-3.70308669088236,5.73780079361409));
#34043=CARTESIAN_POINT('Ctrl Pts',(3.28087066467206,-3.19580465358505,5.76425809029856));
#34044=CARTESIAN_POINT('Ctrl Pts',(3.70950322320198,-2.57936958989042,5.79071538698303));
#34045=CARTESIAN_POINT('Ctrl Pts',(4.13813578173191,-1.9629345261958,5.8171726836675));
#34046=CARTESIAN_POINT('Ctrl Pts',(4.40979064120311,-1.23734643610387,5.84362998035196));
#34047=CARTESIAN_POINT('Ctrl Pts',(4.49138054038091,-0.490981145956846,
5.87008727703643));
#34048=CARTESIAN_POINT('Ctrl Pts',(4.50919422313609,-0.328025747897277,
5.87586375052698));
#34049=CARTESIAN_POINT('Ctrl Pts',(4.51794772865112,-0.164079924696943,
5.88164022401752));
#34050=CARTESIAN_POINT('Ctrl Pts',(4.51777856404949,-0.00011613542669066,
5.88741669750807));
#34051=CARTESIAN_POINT('Ctrl Pts',(4.51761916309611,0.000112359330087797,
5.61258330249198));
#34052=CARTESIAN_POINT('Ctrl Pts',(4.51711804895781,-0.535004016325972,
5.59373296957407));
#34053=CARTESIAN_POINT('Ctrl Pts',(4.42201232003226,-1.07029377947848,5.57488263665616));
#34054=CARTESIAN_POINT('Ctrl Pts',(4.23591186210463,-1.57181816399948,5.55603230373826));
#34055=CARTESIAN_POINT('Ctrl Pts',(3.97471143397694,-2.27573037040736,5.52957500705379));
#34056=CARTESIAN_POINT('Ctrl Pts',(3.5342568961966,-2.91312682419909,5.50311771036932));
#34057=CARTESIAN_POINT('Ctrl Pts',(2.96819512400045,-3.40637334272939,5.47666041368485));
#34058=CARTESIAN_POINT('Ctrl Pts',(2.4021333518043,-3.89961986125968,5.45020311700038));
#34059=CARTESIAN_POINT('Ctrl Pts',(1.71046434519234,-4.24871644452854,5.42374582031592));
#34060=CARTESIAN_POINT('Ctrl Pts',(0.977432623678222,-4.41114351504991,
5.39728852363145));
#34061=CARTESIAN_POINT('Ctrl Pts',(0.244400902164107,-4.57357058557128,
5.37083122694698));
#34062=CARTESIAN_POINT('Ctrl Pts',(-0.529993534252169,-4.54932814334517,
5.34437393026251));
#34063=CARTESIAN_POINT('Ctrl Pts',(-1.2514303002616,-4.34136889100483,5.31791663357804));
#34064=CARTESIAN_POINT('Ctrl Pts',(-1.97286706627105,-4.1334096386645,5.29145933689358));
#34065=CARTESIAN_POINT('Ctrl Pts',(-2.64134616187366,-3.74173357620994,
5.2650020402091));
#34066=CARTESIAN_POINT('Ctrl Pts',(-3.17544757305171,-3.214046414568,5.23854474352464));
#34067=CARTESIAN_POINT('Ctrl Pts',(-3.70954898422975,-2.68635925292607,
5.21208744684017));
#34068=CARTESIAN_POINT('Ctrl Pts',(-4.10927271098324,-2.02266099209677,
5.1856301501557));
#34069=CARTESIAN_POINT('Ctrl Pts',(-4.32593284578035,-1.3037893457135,5.15917285347124));
#34070=CARTESIAN_POINT('Ctrl Pts',(-4.54259298057747,-0.584917699330228,
5.13271555678677));
#34071=CARTESIAN_POINT('Ctrl Pts',(-4.57618952341819,0.189127332607011,
5.1062582601023));
#34072=CARTESIAN_POINT('Ctrl Pts',(-4.42263045256687,0.924067921868061,
5.07980096341783));
#34073=CARTESIAN_POINT('Ctrl Pts',(-4.26907138171554,1.65900851112912,5.05334366673336));
#34074=CARTESIAN_POINT('Ctrl Pts',(-3.92835669717217,2.35484465771397,5.0268863700489));
#34075=CARTESIAN_POINT('Ctrl Pts',(-3.44198507043455,2.92682428907221,5.00042907336443));
#34076=CARTESIAN_POINT('Ctrl Pts',(-2.95561344369694,3.49880392043043,4.97397177667996));
#34077=CARTESIAN_POINT('Ctrl Pts',(-2.3235848747651,3.94692703656203,4.9475144799955));
#34078=CARTESIAN_POINT('Ctrl Pts',(-1.62287974384915,4.21661273787403,4.92105718331103));
#34079=CARTESIAN_POINT('Ctrl Pts',(-0.922174612933183,4.48629843918604,
4.89459988662656));
#34080=CARTESIAN_POINT('Ctrl Pts',(-0.152792920033106,4.57754672567842,
4.86814258994209));
#34081=CARTESIAN_POINT('Ctrl Pts',(0.591555496154586,4.47924365704375,4.84168529325762));
#34082=CARTESIAN_POINT('Ctrl Pts',(1.33590391234227,4.38094058840908,4.81522799657315));
#34083=CARTESIAN_POINT('Ctrl Pts',(2.05521905181757,4.09308616464735,4.78877069988869));
#34084=CARTESIAN_POINT('Ctrl Pts',(2.66188912668092,3.65074073599527,4.76231340320422));
#34085=CARTESIAN_POINT('Ctrl Pts',(3.26855920154427,3.20839530734318,4.73585610651975));
#34086=CARTESIAN_POINT('Ctrl Pts',(3.76258421179568,2.61155887380074,4.70939880983528));
#34087=CARTESIAN_POINT('Ctrl Pts',(4.08379245793942,1.93292545243589,4.68294151315081));
#34088=CARTESIAN_POINT('Ctrl Pts',(4.36852345568096,1.33135941704992,4.65948877626453));
#34089=CARTESIAN_POINT('Ctrl Pts',(4.51746001083452,0.665519661321642,4.63603603937825));
#34090=CARTESIAN_POINT('Ctrl Pts',(4.51801297056466,-8.08487039419617E-5,
4.61258330249197));
#34091=CARTESIAN_POINT('Origin',(0.,0.,20.5));
#34092=CARTESIAN_POINT('',(4.51736370604735,1.02551535238581E-5,3.61258330249198));
#34093=CARTESIAN_POINT('',(4.51813206731963,-1.62797693238861E-5,3.88741669750807));
#34094=CARTESIAN_POINT('',(4.51775,5.53264807684796E-16,20.5));
#34095=CARTESIAN_POINT('Ctrl Pts',(4.51813206731963,-1.62797693238861E-5,
3.88741669750807));
#34096=CARTESIAN_POINT('Ctrl Pts',(4.51798177204935,0.735410282480124,3.91333177025696));
#34097=CARTESIAN_POINT('Ctrl Pts',(4.33483992986086,1.47090898249386,3.93924684300585));
#34098=CARTESIAN_POINT('Ctrl Pts',(3.98971201192936,2.12032066114161,3.96516191575474));
#34099=CARTESIAN_POINT('Ctrl Pts',(3.63736294436994,2.78332005222287,3.99161921243921));
#34100=CARTESIAN_POINT('Ctrl Pts',(3.11617838217547,3.35659231850456,4.01807650912368));
#34101=CARTESIAN_POINT('Ctrl Pts',(2.48963802820999,3.77031353241187,4.04453380580815));
#34102=CARTESIAN_POINT('Ctrl Pts',(1.86309767424454,4.18403474631916,4.07099110249262));
#34103=CARTESIAN_POINT('Ctrl Pts',(1.13120152850809,4.4382049078521,4.09744839917709));
#34104=CARTESIAN_POINT('Ctrl Pts',(0.383093731539025,4.50186637263401,4.12390569586155));
#34105=CARTESIAN_POINT('Ctrl Pts',(-0.365014065430051,4.56552783741592,
4.15036299254602));
#34106=CARTESIAN_POINT('Ctrl Pts',(-1.12933351363175,4.43868060544681,4.17682028923049));
#34107=CARTESIAN_POINT('Ctrl Pts',(-1.81677135017129,4.13677452919472,4.20327758591496));
#34108=CARTESIAN_POINT('Ctrl Pts',(-2.50420918671083,3.83486845294263,4.22973488259942));
#34109=CARTESIAN_POINT('Ctrl Pts',(-3.11476541158823,3.35790353240755,4.25619217928389));
#34110=CARTESIAN_POINT('Ctrl Pts',(-3.57407495233505,2.7639735670387,4.28264947596836));
#34111=CARTESIAN_POINT('Ctrl Pts',(-4.03338449308186,2.17004360166985,4.30910677265283));
#34112=CARTESIAN_POINT('Ctrl Pts',(-4.3414473496981,1.45914859146723,4.3355640693373));
#34113=CARTESIAN_POINT('Ctrl Pts',(-4.4607418071907,0.717874761903797,4.36202136602176));
#34114=CARTESIAN_POINT('Ctrl Pts',(-4.5800362646833,-0.0233990676596439,
4.38847866270623));
#34115=CARTESIAN_POINT('Ctrl Pts',(-4.51056232305225,-0.795051716583895,
4.4149359593907));
#34116=CARTESIAN_POINT('Ctrl Pts',(-4.26078183149923,-1.50309674624206,
4.44139325607517));
#34117=CARTESIAN_POINT('Ctrl Pts',(-4.01100133994621,-2.21114177590023,
4.46785055275963));
#34118=CARTESIAN_POINT('Ctrl Pts',(-3.58091429847122,-2.85557918629231,
4.4943078494441));
#34119=CARTESIAN_POINT('Ctrl Pts',(-3.02290483273516,-3.35791721405156,
4.52076514612857));
#34120=CARTESIAN_POINT('Ctrl Pts',(-2.4648953669991,-3.86025524181081,4.54722244281304));
#34121=CARTESIAN_POINT('Ctrl Pts',(-1.77896347700197,-4.22049388693723,
4.57367973949751));
#34122=CARTESIAN_POINT('Ctrl Pts',(-1.04865490780318,-4.39475648114178,
4.60013703618198));
#34123=CARTESIAN_POINT('Ctrl Pts',(-0.318346338604368,-4.56901907534634,
4.62659433286644));
#34124=CARTESIAN_POINT('Ctrl Pts',(0.456338909796113,-4.55730561862902,
4.65305162955091));
#34125=CARTESIAN_POINT('Ctrl Pts',(1.18104503151144,-4.36104279705434,4.67950892623538));
#34126=CARTESIAN_POINT('Ctrl Pts',(1.90575115322676,-4.16477997547966,4.70596622291985));
#34127=CARTESIAN_POINT('Ctrl Pts',(2.58047814825693,-3.78396778904763,4.73242351960431));
#34128=CARTESIAN_POINT('Ctrl Pts',(3.1230450153487,-3.26498874060892,4.75888081628878));
#34129=CARTESIAN_POINT('Ctrl Pts',(3.66561188244045,-2.74600969217023,4.78533811297325));
#34130=CARTESIAN_POINT('Ctrl Pts',(4.07601862159381,-2.08886378172488,4.81179540965772));
#34131=CARTESIAN_POINT('Ctrl Pts',(4.30427814618986,-1.37359065388121,4.83825270634219));
#34132=CARTESIAN_POINT('Ctrl Pts',(4.4456650936749,-0.930541084129997,4.85464070339748));
#34133=CARTESIAN_POINT('Ctrl Pts',(4.51716714020965,-0.465189691975021,
4.87102870045278));
#34134=CARTESIAN_POINT('Ctrl Pts',(4.51744953111884,7.68816669171638E-5,
4.88741669750807));
#34135=CARTESIAN_POINT('Ctrl Pts',(4.51801297056466,-8.08487039419617E-5,
4.61258330249197));
#34136=CARTESIAN_POINT('Ctrl Pts',(4.51808381093537,-0.0853517722542952,
4.60957874269379));
#34137=CARTESIAN_POINT('Ctrl Pts',(4.51571930609417,-0.170618769185437,
4.6065741828956));
#34138=CARTESIAN_POINT('Ctrl Pts',(4.51089298576516,-0.255746192878958,
4.60356962309741));
#34139=CARTESIAN_POINT('Ctrl Pts',(4.46839378541107,-1.00535400764169,4.57711232641294));
#34140=CARTESIAN_POINT('Ctrl Pts',(4.23500390266681,-1.74413922797991,4.55065502972848));
#34141=CARTESIAN_POINT('Ctrl Pts',(3.83914996695076,-2.38211863169309,4.52419773304401));
#34142=CARTESIAN_POINT('Ctrl Pts',(3.44329603123471,-3.02009803540626,4.49774043635954));
#34143=CARTESIAN_POINT('Ctrl Pts',(2.88497804254688,-3.55727162249439,4.47128313967507));
#34144=CARTESIAN_POINT('Ctrl Pts',(2.23219851400147,-3.92821224455693,4.4448258429906));
#34145=CARTESIAN_POINT('Ctrl Pts',(1.57941898545608,-4.29915286661947,4.41836854630613));
#34146=CARTESIAN_POINT('Ctrl Pts',(0.832177917053118,-4.50386052365641,
4.39191124962167));
#34147=CARTESIAN_POINT('Ctrl Pts',(0.0814884439290546,-4.51740204959703,
4.3654539529372));
#34148=CARTESIAN_POINT('Ctrl Pts',(-0.66920102919502,-4.53094357553764,
4.33899665625273));
#34149=CARTESIAN_POINT('Ctrl Pts',(-1.42333890704021,-4.35331897038192,
4.31253935956826));
#34150=CARTESIAN_POINT('Ctrl Pts',(-2.08907203071289,-4.00616271445513,
4.28608206288379));
#34151=CARTESIAN_POINT('Ctrl Pts',(-2.75480515438558,-3.65900645852834,
4.25962476619933));
#34152=CARTESIAN_POINT('Ctrl Pts',(-3.33213352388578,-3.14231855183048,
4.23316746951486));
#34153=CARTESIAN_POINT('Ctrl Pts',(-3.75073918275569,-2.51903100956272,
4.20671017283039));
#34154=CARTESIAN_POINT('Ctrl Pts',(-4.1693448416256,-1.89574346729495,4.18025287614593));
#34155=CARTESIAN_POINT('Ctrl Pts',(-4.42922778986523,-1.16585628945725,
4.15379557946146));
#34156=CARTESIAN_POINT('Ctrl Pts',(-4.49873457199956,-0.418268926521358,
4.12733828277699));
#34157=CARTESIAN_POINT('Ctrl Pts',(-4.56824135413388,0.329318436414523,
4.10088098609252));
#34158=CARTESIAN_POINT('Ctrl Pts',(-4.44737197016292,1.0946059844486,4.07442368940805));
#34159=CARTESIAN_POINT('Ctrl Pts',(-4.1508481772844,1.78438254119798,4.04796639272359));
#34160=CARTESIAN_POINT('Ctrl Pts',(-3.85432438440588,2.47415909794737,4.02150909603912));
#34161=CARTESIAN_POINT('Ctrl Pts',(-3.3821461826198,3.08842466341204,3.99505179935465));
#34162=CARTESIAN_POINT('Ctrl Pts',(-2.79182435432936,3.55236237154529,3.96859450267018));
#34163=CARTESIAN_POINT('Ctrl Pts',(-2.20150252603891,4.01630007967853,3.94213720598571));
#34164=CARTESIAN_POINT('Ctrl Pts',(-1.49303707124409,4.32990993048035,3.91567990930125));
#34165=CARTESIAN_POINT('Ctrl Pts',(-0.752718298258071,4.45499459120489,
3.88922261261678));
#34166=CARTESIAN_POINT('Ctrl Pts',(-0.0123995252720613,4.58007925192944,
3.86276531593231));
#34167=CARTESIAN_POINT('Ctrl Pts',(0.759772565905157,4.51663872257671,3.83630801924784));
#34168=CARTESIAN_POINT('Ctrl Pts',(1.46974826915516,4.27239998941026,3.80985072256337));
#34169=CARTESIAN_POINT('Ctrl Pts',(2.17972397240517,4.02816125624381,3.78339342587891));
#34170=CARTESIAN_POINT('Ctrl Pts',(2.82750328772796,3.60312431926363,3.75693612919444));
#34171=CARTESIAN_POINT('Ctrl Pts',(3.33418741143483,3.04905820699226,3.73047883250997));
#34172=CARTESIAN_POINT('Ctrl Pts',(3.84087153514169,2.49499209472089,3.7040215358255));
#34173=CARTESIAN_POINT('Ctrl Pts',(4.20646046723263,1.81189680715833,3.67756423914103));
#34174=CARTESIAN_POINT('Ctrl Pts',(4.38642588038764,1.08297259432681,3.65110694245657));
#34175=CARTESIAN_POINT('Ctrl Pts',(4.47377321176399,0.729184698918257,3.63826572913504));
#34176=CARTESIAN_POINT('Ctrl Pts',(4.51739308950363,0.364600853640814,3.62542451581351));
#34177=CARTESIAN_POINT('Ctrl Pts',(4.51736430815743,1.02391689833781E-5,
3.61258330249198));
#34178=CARTESIAN_POINT('Origin',(0.,0.,20.5));
#34179=CARTESIAN_POINT('',(4.51806423128285,6.30519293007281E-5,2.61258330249198));
#34180=CARTESIAN_POINT('',(4.5174009456275,-5.29814202112051E-5,2.88741669750807));
#34181=CARTESIAN_POINT('',(4.51775,5.53264807684796E-16,20.5));
#34182=CARTESIAN_POINT('Ctrl Pts',(4.5174009456275,-5.29814202112051E-5,
2.88741669750807));
#34183=CARTESIAN_POINT('Ctrl Pts',(4.5172216944486,0.434438744202657,2.90272024669221));
#34184=CARTESIAN_POINT('Ctrl Pts',(4.45500169120217,0.868980727030553,2.91802379587635));
#34185=CARTESIAN_POINT('Ctrl Pts',(4.33145501462215,1.28532451174868,2.9333273450605));
#34186=CARTESIAN_POINT('Ctrl Pts',(4.11786331525058,2.00511381699269,2.95978464174497));
#34187=CARTESIAN_POINT('Ctrl Pts',(3.72097433835707,2.67051112625836,2.98624193842943));
#34188=CARTESIAN_POINT('Ctrl Pts',(3.18912872207782,3.2004717836931,3.0126992351139));
#34189=CARTESIAN_POINT('Ctrl Pts',(2.65728310579859,3.73043244112782,3.03915653179837));
#34190=CARTESIAN_POINT('Ctrl Pts',(1.99048085013363,4.12495644673162,3.06561382848284));
#34191=CARTESIAN_POINT('Ctrl Pts',(1.26993773185205,4.33599121325399,3.0920711251673));
#34192=CARTESIAN_POINT('Ctrl Pts',(0.54939461357047,4.54702597977637,3.11852842185177));
#34193=CARTESIAN_POINT('Ctrl Pts',(-0.22488936732773,4.57457150721731,3.14498571853624));
#34194=CARTESIAN_POINT('Ctrl Pts',(-0.958607278893408,4.41527278082,3.17144301522071));
#34195=CARTESIAN_POINT('Ctrl Pts',(-1.69232519045908,4.25597405442269,3.19790031190518));
#34196=CARTESIAN_POINT('Ctrl Pts',(-2.38547703269224,3.90983107418713,3.22435760858964));
#34197=CARTESIAN_POINT('Ctrl Pts',(-2.95363767834166,3.41900367201878,3.25081490527411));
#34198=CARTESIAN_POINT('Ctrl Pts',(-3.52179832399109,2.92817626985041,3.27727220195858));
#34199=CARTESIAN_POINT('Ctrl Pts',(-3.96496777305678,2.29266444574925,3.30372949864305));
#34200=CARTESIAN_POINT('Ctrl Pts',(-4.229168477112,1.58987283655001,3.33018679532752));
#34201=CARTESIAN_POINT('Ctrl Pts',(-4.49336918116721,0.887081227350804,
3.35664409201199));
#34202=CARTESIAN_POINT('Ctrl Pts',(-4.57860114021196,0.117009833053533,
3.38310138869645));
#34203=CARTESIAN_POINT('Ctrl Pts',(-4.47448319596347,-0.62654750277845,
3.40955868538092));
#34204=CARTESIAN_POINT('Ctrl Pts',(-4.37036525171498,-1.37010483861044,
3.43601598206539));
#34205=CARTESIAN_POINT('Ctrl Pts',(-4.07689740417324,-2.08714811597715,
3.46247327874986));
#34206=CARTESIAN_POINT('Ctrl Pts',(-3.62982371237881,-2.69034225726949,
3.48893057543432));
#34207=CARTESIAN_POINT('Ctrl Pts',(-3.18275002058438,-3.29353639856183,
3.51538787211879));
#34208=CARTESIAN_POINT('Ctrl Pts',(-2.58207048453726,-3.7828814037798,3.54184516880326));
#34209=CARTESIAN_POINT('Ctrl Pts',(-1.90094720693718,-4.09877559286125,
3.56830246548773));
#34210=CARTESIAN_POINT('Ctrl Pts',(-1.2198239293371,-4.41466978194271,3.59475976217219));
#34211=CARTESIAN_POINT('Ctrl Pts',(-0.45825691018407,-4.55711315488765,
3.62121705885666));
#34212=CARTESIAN_POINT('Ctrl Pts',(0.290995830439079,-4.5087562665179,3.64767435554113));
#34213=CARTESIAN_POINT('Ctrl Pts',(1.04024857106223,-4.46039937814816,3.6741316522256));
#34214=CARTESIAN_POINT('Ctrl Pts',(1.77718703315549,-4.22124222846373,3.70058894891007));
#34215=CARTESIAN_POINT('Ctrl Pts',(2.41205292762872,-3.8204138936135,3.72704624559453));
#34216=CARTESIAN_POINT('Ctrl Pts',(3.04691882210195,-3.41958555876328,3.753503542279));
#34217=CARTESIAN_POINT('Ctrl Pts',(3.57971214895514,-2.85708603874726,3.77996083896347));
#34218=CARTESIAN_POINT('Ctrl Pts',(3.94553927063659,-2.2014271525676,3.80641813564794));
#34219=CARTESIAN_POINT('Ctrl Pts',(4.31136639231804,-1.54576826638794,3.83287543233241));
#34220=CARTESIAN_POINT('Ctrl Pts',(4.51022730882776,-0.796950014044647,
3.85933272901687));
#34221=CARTESIAN_POINT('Ctrl Pts',(4.51790098062045,-0.0461776299325883,
3.88579002570134));
#34222=CARTESIAN_POINT('Ctrl Pts',(4.51805824719871,-0.0307910709167367,
3.88633224963692));
#34223=CARTESIAN_POINT('Ctrl Pts',(4.5181352119642,-0.0154036911331415,
3.88687447357249));
#34224=CARTESIAN_POINT('Ctrl Pts',(4.51813206731963,-1.62797693238861E-5,
3.88741669750807));
#34225=CARTESIAN_POINT('Ctrl Pts',(4.51736430815743,1.02391689833781E-5,
3.61258330249198));
#34226=CARTESIAN_POINT('Ctrl Pts',(4.51733379007481,-0.386580659657543,
3.59896721912904));
#34227=CARTESIAN_POINT('Ctrl Pts',(4.46822794652789,-0.773179169265813,
3.5853511357661));
#34228=CARTESIAN_POINT('Ctrl Pts',(4.370140714067,-1.14692274519747,3.57173505240317));
#34229=CARTESIAN_POINT('Ctrl Pts',(4.17954824037228,-1.87314073378976,3.5452777557187));
#34230=CARTESIAN_POINT('Ctrl Pts',(3.80402139876375,-2.55082357287386,3.51882045903423));
#34231=CARTESIAN_POINT('Ctrl Pts',(3.28929894294204,-3.09743024266209,3.49236316234976));
#34232=CARTESIAN_POINT('Ctrl Pts',(2.77457648712035,-3.64403691245031,3.46590586566529));
#34233=CARTESIAN_POINT('Ctrl Pts',(2.12065841708548,-4.05956741294266,3.43944856898082));
#34234=CARTESIAN_POINT('Ctrl Pts',(1.40719123005614,-4.29341058905976,3.41299127229636));
#34235=CARTESIAN_POINT('Ctrl Pts',(0.693724043026795,-4.52725376517686,
3.38653397561189));
#34236=CARTESIAN_POINT('Ctrl Pts',(-0.0792922609970231,-4.5794096169187,
3.36007667892742));
#34237=CARTESIAN_POINT('Ctrl Pts',(-0.8177051517065,-4.44352561926563,3.33361938224295));
#34238=CARTESIAN_POINT('Ctrl Pts',(-1.55611804241598,-4.30764162161257,
3.30716208555848));
#34239=CARTESIAN_POINT('Ctrl Pts',(-2.2599275198111,-3.9837177745646,3.28070478887401));
#34240=CARTESIAN_POINT('Ctrl Pts',(-2.84341036847309,-3.51120764419552,
3.25424749218955));
#34241=CARTESIAN_POINT('Ctrl Pts',(-3.42689321713508,-3.03869751382645,
3.22779019550508));
#34242=CARTESIAN_POINT('Ctrl Pts',(-3.89004943706392,-2.41760110013629,
3.20133289882062));
#34243=CARTESIAN_POINT('Ctrl Pts',(-4.17646711326174,-1.72356725892568,
3.17487560213615));
#34244=CARTESIAN_POINT('Ctrl Pts',(-4.46288478945955,-1.02953341771508,
3.14841830545168));
#34245=CARTESIAN_POINT('Ctrl Pts',(-4.57256392192634,-0.262562148984027,
3.12196100876721));
#34246=CARTESIAN_POINT('Ctrl Pts',(-4.49214571371297,0.483930295567052,
3.09550371208274));
#34247=CARTESIAN_POINT('Ctrl Pts',(-4.41172750549959,1.23042274011814,3.06904641539827));
#34248=CARTESIAN_POINT('Ctrl Pts',(-4.14121195660606,1.95643636048925,3.04258911871381));
#34249=CARTESIAN_POINT('Ctrl Pts',(-3.71354756149959,2.57354350122118,3.01613182202934));
#34250=CARTESIAN_POINT('Ctrl Pts',(-3.28588316639313,3.1906506419531,2.98967452534487));
#34251=CARTESIAN_POINT('Ctrl Pts',(-2.70106992507374,3.69885130304582,2.9632172286604));
#34252=CARTESIAN_POINT('Ctrl Pts',(-2.03033744310303,4.03624720641976,2.93675993197593));
#34253=CARTESIAN_POINT('Ctrl Pts',(-1.35960496113232,4.3736431097937,2.91030263529147));
#34254=CARTESIAN_POINT('Ctrl Pts',(-0.602953238510295,4.54023425544885,
2.883845338607));
#34255=CARTESIAN_POINT('Ctrl Pts',(0.147458382357749,4.5157300262161,2.85738804192253));
#34256=CARTESIAN_POINT('Ctrl Pts',(0.897870003225787,4.49122579698336,2.83093074523806));
#34257=CARTESIAN_POINT('Ctrl Pts',(1.64204152233985,4.27562619286271,2.80447344855359));
#34258=CARTESIAN_POINT('Ctrl Pts',(2.28933367226974,3.89519100702514,2.77801615186913));
#34259=CARTESIAN_POINT('Ctrl Pts',(2.93662582219963,3.51475582118756,2.75155885518466));
#34260=CARTESIAN_POINT('Ctrl Pts',(3.48703860294536,2.96948505363305,2.72510155850019));
#34261=CARTESIAN_POINT('Ctrl Pts',(3.873532346971,2.32579208038178,2.69864426181572));
#34262=CARTESIAN_POINT('Ctrl Pts',(4.26002609099665,1.68209910713051,2.67218696513126));
#34263=CARTESIAN_POINT('Ctrl Pts',(4.48260079830222,0.939983928182504,2.64572966844679));
#34264=CARTESIAN_POINT('Ctrl Pts',(4.51414711586846,0.189835351011121,2.61927237176232));
#34265=CARTESIAN_POINT('Ctrl Pts',(4.51680568306753,0.126616549085492,2.61704268200554));
#34266=CARTESIAN_POINT('Ctrl Pts',(4.51810751267774,0.063340691696271,2.61481299224876));
#34267=CARTESIAN_POINT('Ctrl Pts',(4.51806423128285,6.30519293007281E-5,
2.61258330249198));
#34268=CARTESIAN_POINT('Origin',(0.,0.,20.5));
#34269=CARTESIAN_POINT('',(4.51755838390264,-0.00010457874560596,1.61258330249198));
#34270=CARTESIAN_POINT('',(4.51787557461174,0.000108094638884985,1.88741669750807));
#34271=CARTESIAN_POINT('',(4.51775,5.53264807684796E-16,20.5));
#34272=CARTESIAN_POINT('Ctrl Pts',(4.51787557461174,0.000108094638884985,
1.88741669750807));
#34273=CARTESIAN_POINT('Ctrl Pts',(4.51800988663209,0.133281854142107,1.89210872312746));
#34274=CARTESIAN_POINT('Ctrl Pts',(4.5122387502371,0.266444013117212,1.89680074874686));
#34275=CARTESIAN_POINT('Ctrl Pts',(4.50047783691867,0.399075035061228,1.90149277436625));
#34276=CARTESIAN_POINT('Ctrl Pts',(4.43416064298431,1.14695208897868,1.92795007105072));
#34277=CARTESIAN_POINT('Ctrl Pts',(4.17739351195545,1.87794119941301,1.95440736773518));
#34278=CARTESIAN_POINT('Ctrl Pts',(3.76145039622174,2.50300870173296,1.98086466441965));
#34279=CARTESIAN_POINT('Ctrl Pts',(3.34550728048802,3.1280762040529,2.00732196110412));
#34280=CARTESIAN_POINT('Ctrl Pts',(2.77038818004944,3.64722209825845,2.03377925778859));
#34281=CARTESIAN_POINT('Ctrl Pts',(2.10614196483581,3.99721498898444,2.06023655447306));
#34282=CARTESIAN_POINT('Ctrl Pts',(1.44189574962217,4.34720787971043,2.08669385115753));
#34283=CARTESIAN_POINT('Ctrl Pts',(0.688522419633492,4.52804776695686,2.11315114784199));
#34284=CARTESIAN_POINT('Ctrl Pts',(-0.0622179873186998,4.51770855260139,
2.13960844452646));
#34285=CARTESIAN_POINT('Ctrl Pts',(-0.812958394270891,4.50736933824591,
2.16606574121093));
#34286=CARTESIAN_POINT('Ctrl Pts',(-1.56106587818659,4.30585102228854,2.1925230378954));
#34287=CARTESIAN_POINT('Ctrl Pts',(-2.21542177547916,3.9376983125846,2.21898033457986));
#34288=CARTESIAN_POINT('Ctrl Pts',(-2.86977767277172,3.56954560288067,2.24543763126433));
#34289=CARTESIAN_POINT('Ctrl Pts',(-3.43038198344116,3.03475849943017,2.2718949279488));
#34290=CARTESIAN_POINT('Ctrl Pts',(-3.82895372288602,2.39847347956868,2.29835222463327));
#34291=CARTESIAN_POINT('Ctrl Pts',(-4.22752546233088,1.76218845970719,2.32480952131774));
#34292=CARTESIAN_POINT('Ctrl Pts',(-4.46406463055117,1.0244055234347,2.35126681800221));
#34293=CARTESIAN_POINT('Ctrl Pts',(-4.50976101864305,0.274985815861316,
2.37772411468667));
#34294=CARTESIAN_POINT('Ctrl Pts',(-4.55545740673492,-0.474433891712066,
2.40418141137114));
#34295=CARTESIAN_POINT('Ctrl Pts',(-4.41031101469838,-1.23549037058635,
2.43063870805561));
#34296=CARTESIAN_POINT('Ctrl Pts',(-4.09200051244538,-1.91548778391935,
2.45709600474008));
#34297=CARTESIAN_POINT('Ctrl Pts',(-3.77369001019238,-2.59548519725235,
2.48355330142454));
#34298=CARTESIAN_POINT('Ctrl Pts',(-3.28221539772292,-3.19442354504408,
2.51001059810901));
#34299=CARTESIAN_POINT('Ctrl Pts',(-2.67743773890551,-3.63935279939741,
2.53646789479348));
#34300=CARTESIAN_POINT('Ctrl Pts',(-2.07266008008808,-4.08428205375076,
2.56292519147795));
#34301=CARTESIAN_POINT('Ctrl Pts',(-1.35457937492269,-4.37520221466569,
2.58938248816241));
#34302=CARTESIAN_POINT('Ctrl Pts',(-0.610657058576137,-4.47667952851314,
2.61583978484688));
#34303=CARTESIAN_POINT('Ctrl Pts',(0.133265257770398,-4.57815684236058,
2.64229708153135));
#34304=CARTESIAN_POINT('Ctrl Pts',(0.9030291852981,-4.49019130914055,2.66875437821582));
#34305=CARTESIAN_POINT('Ctrl Pts',(1.60487832955586,-4.22349703344507,2.69521167490029));
#34306=CARTESIAN_POINT('Ctrl Pts',(2.30672747381364,-3.95680275774959,2.72166897158476));
#34307=CARTESIAN_POINT('Ctrl Pts',(2.94066183480147,-3.51137973957866,2.74812626826922));
#34308=CARTESIAN_POINT('Ctrl Pts',(3.42946890894601,-2.94148000958192,2.77458356495369));
#34309=CARTESIAN_POINT('Ctrl Pts',(3.91827598309054,-2.37158027958518,2.80104086163816));
#34310=CARTESIAN_POINT('Ctrl Pts',(4.26195577039178,-1.67720383776263,2.82749815832263));
#34311=CARTESIAN_POINT('Ctrl Pts',(4.41864845311758,-0.94292496624017,2.85395545500709));
#34312=CARTESIAN_POINT('Ctrl Pts',(4.4847062457604,-0.633370999882247,2.86510920250742));
#34313=CARTESIAN_POINT('Ctrl Pts',(4.51753158998749,-0.316725338941023,
2.87626295000774));
#34314=CARTESIAN_POINT('Ctrl Pts',(4.5174009456275,-5.29814202112051E-5,
2.88741669750807));
#34315=CARTESIAN_POINT('Ctrl Pts',(4.51806423128285,6.30519293007281E-5,
2.61258330249198));
#34316=CARTESIAN_POINT('Ctrl Pts',(4.51759393956657,-0.687506049970836,
2.58835569556429));
#34317=CARTESIAN_POINT('Ctrl Pts',(4.35830909853907,-1.37528559362468,2.5641280886366));
#34318=CARTESIAN_POINT('Ctrl Pts',(4.0551256392357,-1.9923648496729,2.53990048170891));
#34319=CARTESIAN_POINT('Ctrl Pts',(3.72403991720982,-2.66623449779077,2.51344318502445));
#34320=CARTESIAN_POINT('Ctrl Pts',(3.22135054533116,-3.25579181863177,2.48698588833998));
#34321=CARTESIAN_POINT('Ctrl Pts',(2.60828453275314,-3.68922938300052,2.46052859165551));
#34322=CARTESIAN_POINT('Ctrl Pts',(1.99521852017512,-4.12266694736928,2.43407129497105));
#34323=CARTESIAN_POINT('Ctrl Pts',(1.27177586689775,-4.3999847552658,2.40761399828658));
#34324=CARTESIAN_POINT('Ctrl Pts',(0.526071087432441,-4.48740580460158,
2.38115670160211));
#34325=CARTESIAN_POINT('Ctrl Pts',(-0.219633692032863,-4.57482685393736,
2.35469940491764));
#34326=CARTESIAN_POINT('Ctrl Pts',(-0.987600597686097,-4.47235114471241,
2.32824210823317));
#34327=CARTESIAN_POINT('Ctrl Pts',(-1.68429211034942,-4.19246010490287,
2.3017848115487));
#34328=CARTESIAN_POINT('Ctrl Pts',(-2.38098362301274,-3.91256906509334,
2.27532751486424));
#34329=CARTESIAN_POINT('Ctrl Pts',(-3.00639974268614,-3.45526269469925,
2.24887021817977));
#34330=CARTESIAN_POINT('Ctrl Pts',(-3.48436547816518,-2.87624040350871,
2.2224129214953));
#34331=CARTESIAN_POINT('Ctrl Pts',(-3.96233121364423,-2.29721811231817,
2.19595562481083));
#34332=CARTESIAN_POINT('Ctrl Pts',(-4.29284656492891,-1.59647990033118,
2.16949832812637));
#34333=CARTESIAN_POINT('Ctrl Pts',(-4.43565512801646,-0.859374906258969,
2.1430410314419));
#34334=CARTESIAN_POINT('Ctrl Pts',(-4.578463691104,-0.122269912186753,2.11658373475743));
#34335=CARTESIAN_POINT('Ctrl Pts',(-4.53356546599441,0.651201863970698,
2.09012643807296));
#34336=CARTESIAN_POINT('Ctrl Pts',(-4.30642900683079,1.36683241594063,2.06366914138849));
#34337=CARTESIAN_POINT('Ctrl Pts',(-4.07929254766716,2.08246296791056,2.03721184470403));
#34338=CARTESIAN_POINT('Ctrl Pts',(-3.66991785444949,2.74025229569297,2.01075454801956));
#34339=CARTESIAN_POINT('Ctrl Pts',(-3.12816631171559,3.26008238708848,1.98429725133509));
#34340=CARTESIAN_POINT('Ctrl Pts',(-2.58641476898168,3.77991247848399,1.95783995465062));
#34341=CARTESIAN_POINT('Ctrl Pts',(-1.91228637673154,4.16178333349259,1.93138265796616));
#34342=CARTESIAN_POINT('Ctrl Pts',(-1.18788922711582,4.3591835047376,1.90492536128169));
#34343=CARTESIAN_POINT('Ctrl Pts',(-0.463492077500105,4.55658367598262,
1.87846806459722));
#34344=CARTESIAN_POINT('Ctrl Pts',(0.311173829481187,4.56951316346406,1.85201076791275));
#34345=CARTESIAN_POINT('Ctrl Pts',(1.04175504380577,4.39639716966128,1.82555347122828));
#34346=CARTESIAN_POINT('Ctrl Pts',(1.77233625813035,4.2232811758585,1.79909617454381));
#34347=CARTESIAN_POINT('Ctrl Pts',(2.45883277979823,3.86411970077152,1.77263887785935));
#34348=CARTESIAN_POINT('Ctrl Pts',(3.01763009204651,3.36265821505193,1.74618158117488));
#34349=CARTESIAN_POINT('Ctrl Pts',(3.57642740429479,2.86119672933234,1.71972428449041));
#34350=CARTESIAN_POINT('Ctrl Pts',(4.00752550712348,2.21743523298015,1.69326698780594));
#34351=CARTESIAN_POINT('Ctrl Pts',(4.2584171290782,1.50978316287142,1.66680969112148));
#34352=CARTESIAN_POINT('Ctrl Pts',(4.42982474689917,1.02631960741915,1.64873422824498));
#34353=CARTESIAN_POINT('Ctrl Pts',(4.51712029378003,0.513034879908299,1.63065876536848));
#34354=CARTESIAN_POINT('Ctrl Pts',(4.51755838390264,-0.00010457874560596,
1.61258330249198));
#34355=CARTESIAN_POINT('Origin',(0.,0.,20.5));
#34356=CARTESIAN_POINT('',(4.51763087883895,0.00011359767064345,0.612583302491977));
#34357=CARTESIAN_POINT('',(4.5177656910975,-0.000116631996953637,0.887416697508071));
#34358=CARTESIAN_POINT('',(4.51775,5.53264807684796E-16,20.5));
#34359=CARTESIAN_POINT('',(-3.4337878873619,2.93584158412996,0.));
#34360=CARTESIAN_POINT('Ctrl Pts',(4.51763087883895,0.00011359767064345,
0.612583302491977));
#34361=CARTESIAN_POINT('Ctrl Pts',(4.51711863846112,-0.539057740350668,
0.59358994511926));
#34362=CARTESIAN_POINT('Ctrl Pts',(4.42053200733307,-1.07840729234144,0.574596587746541));
#34363=CARTESIAN_POINT('Ctrl Pts',(4.23165828048039,-1.58323058504537,0.555603230373824));
#34364=CARTESIAN_POINT('Ctrl Pts',(3.96856165521391,-2.28643746765176,0.529145933689356));
#34365=CARTESIAN_POINT('Ctrl Pts',(3.52639272074203,-2.92265018460396,0.502688637004889));
#34366=CARTESIAN_POINT('Ctrl Pts',(2.95900217961999,-3.41436616507663,0.476231340320421));
#34367=CARTESIAN_POINT('Ctrl Pts',(2.39161163849795,-3.90608214554931,0.449774043635953));
#34368=CARTESIAN_POINT('Ctrl Pts',(1.69899949072575,-4.25330138954245,0.423316746951485));
#34369=CARTESIAN_POINT('Ctrl Pts',(0.965534545329656,-4.41375671437595,
0.396859450267017));
#34370=CARTESIAN_POINT('Ctrl Pts',(0.232069599933564,-4.57421203920944,
0.370402153582549));
#34371=CARTESIAN_POINT('Ctrl Pts',(-0.542248143086422,-4.54790344488329,
0.343944856898081));
#34372=CARTESIAN_POINT('Ctrl Pts',(-1.26312545635881,-4.33799038903376,
0.317487560213613));
#34373=CARTESIAN_POINT('Ctrl Pts',(-1.9840027696312,-4.12807733318424,0.291030263529145));
#34374=CARTESIAN_POINT('Ctrl Pts',(-2.651439653156,-3.73455981581135,0.264572966844678));
#34375=CARTESIAN_POINT('Ctrl Pts',(-3.18410908512135,-3.20545326780586,
0.23811567016021));
#34376=CARTESIAN_POINT('Ctrl Pts',(-3.71677851708671,-2.67634671980037,
0.211658373475742));
#34377=CARTESIAN_POINT('Ctrl Pts',(-4.11468049749262,-2.01165114116227,
0.185201076791274));
#34378=CARTESIAN_POINT('Ctrl Pts',(-4.32941757999959,-1.29215909736801,
0.158743780106806));
#34379=CARTESIAN_POINT('Ctrl Pts',(-4.54415466250656,-0.572667053573755,
0.132286483422338));
#34380=CARTESIAN_POINT('Ctrl Pts',(-4.57572684711458,0.201621455376676,
0.10582918673787));
#34381=CARTESIAN_POINT('Ctrl Pts',(-4.42014586550132,0.936043740039453,
0.0793718900534021));
#34382=CARTESIAN_POINT('Ctrl Pts',(-4.26456488388806,1.67046602470223,0.0529145933689342));
#34383=CARTESIAN_POINT('Ctrl Pts',(-3.92183073605352,2.36502208507736,0.0264572966844666));
#34384=CARTESIAN_POINT('Ctrl Pts',(-3.43378788736187,2.93584158412999,-1.38777878078145E-15));
#34385=CARTESIAN_POINT('',(3.43409108914489,2.93606647242259,-1.66533453693773E-15));
#34386=CARTESIAN_POINT('Origin',(0.,0.,0.));
#34387=CARTESIAN_POINT('Ctrl Pts',(3.43409108914489,2.93606647242259,-1.66533453693773E-15));
#34388=CARTESIAN_POINT('Ctrl Pts',(2.96705577784701,3.48188002612677,0.0253131010459874));
#34389=CARTESIAN_POINT('Ctrl Pts',(2.36757358452891,3.91460873741651,0.0506262020919764));
#34390=CARTESIAN_POINT('Ctrl Pts',(1.70215900486043,4.18523117809474,0.0759393031379656));
#34391=CARTESIAN_POINT('Ctrl Pts',(1.00666654344788,4.46808621784236,0.102396599822434));
#34392=CARTESIAN_POINT('Ctrl Pts',(0.23914646876357,4.57384880856985,0.128853896506902));
#34393=CARTESIAN_POINT('Ctrl Pts',(-0.506923795872801,4.48961228541997,
0.15531119319137));
#34394=CARTESIAN_POINT('Ctrl Pts',(-1.25299406050917,4.40537576227008,0.181768489875837));
#34395=CARTESIAN_POINT('Ctrl Pts',(-1.9776145150976,4.13114012524282,0.208225786560305));
#34396=CARTESIAN_POINT('Ctrl Pts',(-2.59252418705973,3.70032015205329,0.234683083244772));
#34397=CARTESIAN_POINT('Ctrl Pts',(-3.20743385902187,3.26950017886376,0.26114037992924));
#34398=CARTESIAN_POINT('Ctrl Pts',(-3.71263274835771,2.68209586951196,0.287597676613709));
#34399=CARTESIAN_POINT('Ctrl Pts',(-4.04658977984313,2.00964543895375,0.314054973298177));
#34400=CARTESIAN_POINT('Ctrl Pts',(-4.38054681132855,1.33719500839555,0.340512269982645));
#34401=CARTESIAN_POINT('Ctrl Pts',(-4.54326198496355,0.579698456630952,
0.366969566667112));
#34402=CARTESIAN_POINT('Ctrl Pts',(-4.51491593042486,-0.170578278221808,
0.39342686335158));
#34403=CARTESIAN_POINT('Ctrl Pts',(-4.48656987588618,-0.920855013074566,
0.419884160036048));
#34404=CARTESIAN_POINT('Ctrl Pts',(-4.26716259317382,-1.66391193101549,
0.446341456720516));
#34405=CARTESIAN_POINT('Ctrl Pts',(-3.88341809255795,-2.30924747945238,
0.472798753404984));
#34406=CARTESIAN_POINT('Ctrl Pts',(-3.49967359194208,-2.95458302788927,
0.499256050089452));
#34407=CARTESIAN_POINT('Ctrl Pts',(-2.95159187342268,-3.50219720682213,
0.52571334677392));
#34408=CARTESIAN_POINT('Ctrl Pts',(-2.30592844750098,-3.88539017854139,
0.552170643458388));
#34409=CARTESIAN_POINT('Ctrl Pts',(-1.66026502157927,-4.26858315026064,
0.578627940142856));
#34410=CARTESIAN_POINT('Ctrl Pts',(-0.91701988825525,-4.48735491476628,
0.605085236827324));
#34411=CARTESIAN_POINT('Ctrl Pts',(-0.166719607306316,-4.51505986234428,
0.631542533511792));
#34412=CARTESIAN_POINT('Ctrl Pts',(0.583580673642613,-4.54276480992227,
0.65799983019626));
#34413=CARTESIAN_POINT('Ctrl Pts',(1.34093610221646,-4.37940294057262,0.684457126880727));
#34414=CARTESIAN_POINT('Ctrl Pts',(2.01310169166318,-4.04487125838886,0.710914423565195));
#34415=CARTESIAN_POINT('Ctrl Pts',(2.68526728110991,-3.7103395762051,0.737371720249663));
#34416=CARTESIAN_POINT('Ctrl Pts',(3.27224303142951,-3.20463808118722,0.763829016934131));
#34417=CARTESIAN_POINT('Ctrl Pts',(3.70253591076623,-2.58936080975925,0.790286313618599));
#34418=CARTESIAN_POINT('Ctrl Pts',(4.13282879010294,-1.9740835383313,0.816743610303067));
#34419=CARTESIAN_POINT('Ctrl Pts',(4.40643879845678,-1.24923049049327,0.843200906987535));
#34420=CARTESIAN_POINT('Ctrl Pts',(4.49004055820744,-0.503087883691874,
0.869658203672002));
#34421=CARTESIAN_POINT('Ctrl Pts',(4.50874543387838,-0.336147561686243,
0.875577701617358));
#34422=CARTESIAN_POINT('Ctrl Pts',(4.51793876013751,-0.168141513884366,
0.881497199562714));
#34423=CARTESIAN_POINT('Ctrl Pts',(4.5177656910975,-0.000116631996953637,
0.887416697508071));
#34424=CARTESIAN_POINT('Origin',(0.,0.,-2.20833684463713));
#34425=CARTESIAN_POINT('',(5.07403060246553,1.54698778687123E-5,39.208336844637));
#34426=CARTESIAN_POINT('',(5.07396752856948,-6.48011021279027E-5,39.2916631553629));
#34427=CARTESIAN_POINT('',(5.0736,-1.85409460923845E-12,-2.20833684463713));
#34428=CARTESIAN_POINT('',(-1.31303618635666,-4.90075024188317,40.));
#34429=CARTESIAN_POINT('Ctrl Pts',(5.07396752856948,-6.48011021277175E-5,
39.2916631553629));
#34430=CARTESIAN_POINT('Ctrl Pts',(5.07347424400433,0.779307331517198,39.3161170634328));
#34431=CARTESIAN_POINT('Ctrl Pts',(4.69381943413572,2.40236770827343,39.3670282681872));
#34432=CARTESIAN_POINT('Ctrl Pts',(3.03470961035893,4.33144609848054,39.4443967696262));
#34433=CARTESIAN_POINT('Ctrl Pts',(0.593383061700927,5.25537632570972,39.5237686596795));
#34434=CARTESIAN_POINT('Ctrl Pts',(-1.99247705733066,4.8990504464678,39.603140549733));
#34435=CARTESIAN_POINT('Ctrl Pts',(-4.09299916691649,3.34943642687039,39.6825124397864));
#34436=CARTESIAN_POINT('Ctrl Pts',(-5.19642846461573,0.983699440459269,
39.7618843298398));
#34437=CARTESIAN_POINT('Ctrl Pts',(-5.03410925482033,-1.62126816458454,
39.8412562198932));
#34438=CARTESIAN_POINT('Ctrl Pts',(-3.6453165085118,-3.83208153227987,39.9206281099466));
#34439=CARTESIAN_POINT('Ctrl Pts',(-2.12771778283764,-4.68247622999901,
39.9735427033155));
#34440=CARTESIAN_POINT('Ctrl Pts',(-1.31303618635638,-4.90075024188325,
40.));
#34441=CARTESIAN_POINT('',(1.31317395760221,-4.90115117757563,40.));
#34442=CARTESIAN_POINT('Origin',(0.,0.,40.));
#34443=CARTESIAN_POINT('Ctrl Pts',(5.07403060246553,1.54698778688793E-5,
39.208336844637));
#34444=CARTESIAN_POINT('Ctrl Pts',(5.07403315687698,0.0146420671929676,
39.2087957918851));
#34445=CARTESIAN_POINT('Ctrl Pts',(5.07040151797183,0.872458469457581,39.2357120358177));
#34446=CARTESIAN_POINT('Ctrl Pts',(4.62253485344793,2.56965255248844,39.2890855764349));
#34447=CARTESIAN_POINT('Ctrl Pts',(2.83047200092405,4.46759066254981,39.3684574664882));
#34448=CARTESIAN_POINT('Ctrl Pts',(0.34891291852996,5.27723479734496,39.4478293565417));
#34449=CARTESIAN_POINT('Ctrl Pts',(-2.21764149317963,4.80135391043001,39.527201246595));
#34450=CARTESIAN_POINT('Ctrl Pts',(-4.24398161873814,3.15587819282133,39.6065731366485));
#34451=CARTESIAN_POINT('Ctrl Pts',(-5.23650047694821,0.74162931109825,39.6859450267018));
#34452=CARTESIAN_POINT('Ctrl Pts',(-4.9534132521342,-1.85326330477585,39.7653169167553));
#34453=CARTESIAN_POINT('Ctrl Pts',(-3.46369715057683,-3.99673439595749,
39.8446888068086));
#34454=CARTESIAN_POINT('Ctrl Pts',(-1.1638488125998,-5.14969078544563,39.9229165012236));
#34455=CARTESIAN_POINT('Ctrl Pts',(0.533836595431815,-5.10962665469158,
39.974686898954));
#34456=CARTESIAN_POINT('Ctrl Pts',(1.31317395760221,-4.90115117757563,40.));
#34457=CARTESIAN_POINT('Origin',(0.,0.,-2.20833684463713));
#34458=CARTESIAN_POINT('',(5.07325764975804,-8.44407784307555E-5,38.208336844637));
#34459=CARTESIAN_POINT('',(5.07316912366228,-1.81818814078922E-5,38.2916631553629));
#34460=CARTESIAN_POINT('',(5.0736,-1.85409460923845E-12,-2.20833684463713));
#34461=CARTESIAN_POINT('Ctrl Pts',(5.07316912366228,-1.81818814076751E-5,
38.2916631553629));
#34462=CARTESIAN_POINT('Ctrl Pts',(5.07311400239361,0.441352830351579,38.3055055398681));
#34463=CARTESIAN_POINT('Ctrl Pts',(4.90711571561459,1.72636801461904,38.3458052210578));
#34464=CARTESIAN_POINT('Ctrl Pts',(3.83482475204887,3.64212307300276,38.4125621989319));
#34465=CARTESIAN_POINT('Ctrl Pts',(1.62575061805696,5.03268082057242,38.4919340889853));
#34466=CARTESIAN_POINT('Ctrl Pts',(-0.979352771366501,5.19728867487039,
38.5713059790387));
#34467=CARTESIAN_POINT('Ctrl Pts',(-3.3458879870052,4.09584848370752,38.6506778690921));
#34468=CARTESIAN_POINT('Ctrl Pts',(-4.89737230716795,1.99666872129193,38.7300497591456));
#34469=CARTESIAN_POINT('Ctrl Pts',(-5.2558675504918,-0.588895222855594,
38.809421649199));
#34470=CARTESIAN_POINT('Ctrl Pts',(-4.33404513553914,-3.03100540392653,
38.8887935392523));
#34471=CARTESIAN_POINT('Ctrl Pts',(-2.35645883694701,-4.73476973691708,
38.9681654293058));
#34472=CARTESIAN_POINT('Ctrl Pts',(0.195155463808245,-5.28515396379923,
39.0475373193592));
#34473=CARTESIAN_POINT('Ctrl Pts',(2.69923061743519,-4.54808766460433,39.1269092094126));
#34474=CARTESIAN_POINT('Ctrl Pts',(4.5457786161602,-2.70311485851688,39.2062810994659));
#34475=CARTESIAN_POINT('Ctrl Pts',(5.05724155748156,-0.970965988519946,
39.2611990814494));
#34476=CARTESIAN_POINT('Ctrl Pts',(5.07400794095178,-0.063914933051532,
39.2896597667484));
#34477=CARTESIAN_POINT('Ctrl Pts',(5.07396752856948,-6.48011021277175E-5,
39.2916631553629));
#34478=CARTESIAN_POINT('Ctrl Pts',(5.07325764975804,-8.44407784305126E-5,
38.208336844637));
#34479=CARTESIAN_POINT('Ctrl Pts',(5.07294945930103,0.51977335908998,38.2246415650049));
#34480=CARTESIAN_POINT('Ctrl Pts',(4.86451980067584,1.88343404898941,38.2674035820572));
#34481=CARTESIAN_POINT('Ctrl Pts',(3.66171031660113,3.81612616476472,38.336622895794));
#34482=CARTESIAN_POINT('Ctrl Pts',(1.39049711694169,5.10269135980963,38.4159947858473));
#34483=CARTESIAN_POINT('Ctrl Pts',(-1.21943810235573,5.14625223481529,38.4953666759008));
#34484=CARTESIAN_POINT('Ctrl Pts',(-3.53232089954511,3.93619745533324,38.5747385659542));
#34485=CARTESIAN_POINT('Ctrl Pts',(-4.98473814342406,1.76729369047725,38.6541104560076));
#34486=CARTESIAN_POINT('Ctrl Pts',(-5.22288421068334,-0.832118909543577,
38.733482346061));
#34487=CARTESIAN_POINT('Ctrl Pts',(-4.18874724188046,-3.22882917750522,
38.8128542361144));
#34488=CARTESIAN_POINT('Ctrl Pts',(-2.13424072225093,-4.83900381899058,
38.8922261261678));
#34489=CARTESIAN_POINT('Ctrl Pts',(0.440162123945958,-5.27040781417516,
38.9715980162212));
#34490=CARTESIAN_POINT('Ctrl Pts',(2.90734243084964,-4.41795218255951,39.0509699062746));
#34491=CARTESIAN_POINT('Ctrl Pts',(4.65612987828293,-2.500445050276,39.1298828490799));
#34492=CARTESIAN_POINT('Ctrl Pts',(5.07388590069044,-0.828549010266373,
39.1823384952007));
#34493=CARTESIAN_POINT('Ctrl Pts',(5.07403060246553,1.54698778688793E-5,
39.208336844637));
#34494=CARTESIAN_POINT('Origin',(0.,0.,-2.20833684463713));
#34495=CARTESIAN_POINT('',(5.07364050160013,0.000130038443658109,37.208336844637));
#34496=CARTESIAN_POINT('',(5.07387656802193,9.59844669708175E-5,37.2916631553629));
#34497=CARTESIAN_POINT('',(5.0736,-1.85409460923845E-12,-2.20833684463713));
#34498=CARTESIAN_POINT('Ctrl Pts',(5.07387656802193,9.59844669710073E-5,
37.2916631553629));
#34499=CARTESIAN_POINT('Ctrl Pts',(5.07396569861154,0.103072231247123,37.2948940163033));
#34500=CARTESIAN_POINT('Ctrl Pts',(5.04574853055582,1.04926503651591,37.3245821739283));
#34501=CARTESIAN_POINT('Ctrl Pts',(4.48202491545551,2.80756015154514,37.3807276282377));
#34502=CARTESIAN_POINT('Ctrl Pts',(2.59328691715162,4.6093171199916,37.4600995182911));
#34503=CARTESIAN_POINT('Ctrl Pts',(0.0728299659736646,5.28825464055466,
37.5394714083445));
#34504=CARTESIAN_POINT('Ctrl Pts',(-2.46536820371075,4.67898503603898,37.6188432983979));
#34505=CARTESIAN_POINT('Ctrl Pts',(-4.40300813596802,2.92992503348812,37.6982151884513));
#34506=CARTESIAN_POINT('Ctrl Pts',(-5.26808503220261,0.467141778084607,
37.7775870785047));
#34507=CARTESIAN_POINT('Ctrl Pts',(-4.84986807528987,-2.10943618050861,
37.8569589685581));
#34508=CARTESIAN_POINT('Ctrl Pts',(-3.2502339902585,-4.17216015459505,37.9363308586115));
#34509=CARTESIAN_POINT('Ctrl Pts',(-0.858850099431265,-5.21855515011692,
38.0157027486649));
#34510=CARTESIAN_POINT('Ctrl Pts',(1.74174777450972,-4.99372166181591,38.0950746387183));
#34511=CARTESIAN_POINT('Ctrl Pts',(3.91805974601555,-3.55242863073569,38.1744465287717));
#34512=CARTESIAN_POINT('Ctrl Pts',(4.92684606433671,-1.64805066527608,38.2399760343199));
#34513=CARTESIAN_POINT('Ctrl Pts',(5.0732193570569,-0.402250655317197,38.2790482431836));
#34514=CARTESIAN_POINT('Ctrl Pts',(5.07316912366228,-1.81818814076751E-5,
38.2916631553629));
#34515=CARTESIAN_POINT('Ctrl Pts',(5.07364050160013,0.000130038443658265,
37.208336844637));
#34516=CARTESIAN_POINT('Ctrl Pts',(5.07382783063862,0.181611936494348,37.2140300414401));
#34517=CARTESIAN_POINT('Ctrl Pts',(5.01990561118457,1.20636170521342,37.2461805349277));
#34518=CARTESIAN_POINT('Ctrl Pts',(4.34693493313475,3.01249033764469,37.3047883250998));
#34519=CARTESIAN_POINT('Ctrl Pts',(2.37663436681862,4.72467463787371,37.3841602151531));
#34520=CARTESIAN_POINT('Ctrl Pts',(-0.17260907066365,5.28593865420645,37.4635321052065));
#34521=CARTESIAN_POINT('Ctrl Pts',(-2.67980532059584,4.55955971460153,37.54290399526));
#34522=CARTESIAN_POINT('Ctrl Pts',(-4.53420692607955,2.72248212093334,37.6222758853133));
#34523=CARTESIAN_POINT('Ctrl Pts',(-5.28408576066665,0.222213908718847,
37.7016477753668));
#34524=CARTESIAN_POINT('Ctrl Pts',(-4.74677300008161,-2.33218511979937,
37.7810196654201));
#34525=CARTESIAN_POINT('Ctrl Pts',(-3.05315684347904,-4.31846901533503,
37.8603915554736));
#34526=CARTESIAN_POINT('Ctrl Pts',(-0.615798437855754,-5.25278341751105,
37.9397634455269));
#34527=CARTESIAN_POINT('Ctrl Pts',(1.97156710418767,-4.90753140600709,38.0191353355804));
#34528=CARTESIAN_POINT('Ctrl Pts',(4.07866326363087,-3.36681560666115,38.0985072256337));
#34529=CARTESIAN_POINT('Ctrl Pts',(4.96346005639167,-1.49092415374923,38.1615743953193));
#34530=CARTESIAN_POINT('Ctrl Pts',(5.07344955290414,-0.323787998268402,
38.1981842683204));
#34531=CARTESIAN_POINT('Ctrl Pts',(5.07325764975804,-8.44407784305126E-5,
38.208336844637));
#34532=CARTESIAN_POINT('Origin',(0.,0.,-2.20833684463713));
#34533=CARTESIAN_POINT('',(5.07371855919287,-0.000123991516001801,36.208336844637));
#34534=CARTESIAN_POINT('',(5.07347409402005,-0.000127990615926579,36.2916631553629));
#34535=CARTESIAN_POINT('',(5.0736,-1.85409460923845E-12,-2.20833684463713));
#34536=CARTESIAN_POINT('Ctrl Pts',(5.07347409402005,-0.00012799061592652,
36.2916631553629));
#34537=CARTESIAN_POINT('Ctrl Pts',(5.07289252391416,0.608034774450749,36.3107397894231));
#34538=CARTESIAN_POINT('Ctrl Pts',(4.81166108430775,2.06014185956918,36.3562737201677));
#34539=CARTESIAN_POINT('Ctrl Pts',(3.45741385862894,4.002153265115,36.4282649475969));
#34540=CARTESIAN_POINT('Ctrl Pts',(1.12210854951209,5.16834729390565,36.5076368376502));
#34541=CARTESIAN_POINT('Ctrl Pts',(-1.4865399185207,5.07554336184357,36.5870087277037));
#34542=CARTESIAN_POINT('Ctrl Pts',(-3.73307055280216,3.74634830136112,36.666380617757));
#34543=CARTESIAN_POINT('Ctrl Pts',(-5.07023346343257,1.50455108706837,36.7457525078105));
#34544=CARTESIAN_POINT('Ctrl Pts',(-5.17229872514219,-1.10375144176689,
36.8251243978638));
#34545=CARTESIAN_POINT('Ctrl Pts',(-4.01440346609619,-3.44318256250012,
36.9044962879173));
#34546=CARTESIAN_POINT('Ctrl Pts',(-1.87860840844056,-4.94386203236358,
36.9838681779707));
#34547=CARTESIAN_POINT('Ctrl Pts',(0.71481149928202,-5.24022765419639,37.0632400680241));
#34548=CARTESIAN_POINT('Ctrl Pts',(3.13410490798792,-4.26008541851396,37.1426119580775));
#34549=CARTESIAN_POINT('Ctrl Pts',(4.72253605350391,-2.32433471697507,37.2187529871904));
#34550=CARTESIAN_POINT('Ctrl Pts',(5.07323581438062,-0.740193128270358,
37.2684367196189));
#34551=CARTESIAN_POINT('Ctrl Pts',(5.07387656802193,9.59844669710073E-5,
37.2916631553629));
#34552=CARTESIAN_POINT('Ctrl Pts',(5.07371855919287,-0.000123991516001801,
36.208336844637));
#34553=CARTESIAN_POINT('Ctrl Pts',(5.07301904482133,0.686442797877024,36.2298758145598));
#34554=CARTESIAN_POINT('Ctrl Pts',(4.76024594010631,2.21696867292356,36.2778720811671));
#34555=CARTESIAN_POINT('Ctrl Pts',(3.26800144929601,4.15825779320007,36.3523256444589));
#34556=CARTESIAN_POINT('Ctrl Pts',(0.881102883784141,5.2148441065383,36.4316975345123));
#34557=CARTESIAN_POINT('Ctrl Pts',(-1.72043039392939,5.00110593838543,36.5110694245656));
#34558=CARTESIAN_POINT('Ctrl Pts',(-3.90287063578981,3.56910943340206,36.5904413146191));
#34559=CARTESIAN_POINT('Ctrl Pts',(-5.13458022962944,1.26768577053169,36.6698132046725));
#34560=CARTESIAN_POINT('Ctrl Pts',(-5.11551744473188,-1.34254334006536,
36.7491850947259));
#34561=CARTESIAN_POINT('Ctrl Pts',(-3.85032593330342,-3.62573186469175,
36.8285569847793));
#34562=CARTESIAN_POINT('Ctrl Pts',(-1.64720354707418,-5.02570013250056,
36.9079288748327));
#34563=CARTESIAN_POINT('Ctrl Pts',(0.957173977199105,-5.20141897223083,
36.9873007648861));
#34564=CARTESIAN_POINT('Ctrl Pts',(3.32838603929536,-4.11008366347129,37.0666726549395));
#34565=CARTESIAN_POINT('Ctrl Pts',(4.77688430036561,-2.16763522711972,37.1403513481898));
#34566=CARTESIAN_POINT('Ctrl Pts',(5.07295727932621,-0.661766675847902,
37.1875727447556));
#34567=CARTESIAN_POINT('Ctrl Pts',(5.07364050160013,0.000130038443658265,
37.208336844637));
#34568=CARTESIAN_POINT('Origin',(0.,0.,-2.20833684463713));
#34569=CARTESIAN_POINT('',(5.07321765521711,6.54440514302745E-5,35.208336844637));
#34570=CARTESIAN_POINT('',(5.07337786466077,0.000116280867786642,35.2916631553629));
#34571=CARTESIAN_POINT('',(5.0736,-1.85409460923845E-12,-2.20833684463713));
#34572=CARTESIAN_POINT('Ctrl Pts',(5.07337786466077,0.000116280867786742,
35.2916631553629));
#34573=CARTESIAN_POINT('Ctrl Pts',(5.07360553071623,0.269998548266127,35.3001282658583));
#34574=CARTESIAN_POINT('Ctrl Pts',(4.98629871182508,1.38323904612086,35.3350506730382));
#34575=CARTESIAN_POINT('Ctrl Pts',(4.18367369924664,3.23540039647985,35.3964303769026));
#34576=CARTESIAN_POINT('Ctrl Pts',(2.12664217080567,4.8423480280398,35.4758022669559));
#34577=CARTESIAN_POINT('Ctrl Pts',(-0.448434683200953,5.2697103983248,35.5551741570095));
#34578=CARTESIAN_POINT('Ctrl Pts',(-2.91427384097317,4.41338297988397,35.6345460470627));
#34579=CARTESIAN_POINT('Ctrl Pts',(-4.67020234172003,2.48196523640092,35.7139179371163));
#34580=CARTESIAN_POINT('Ctrl Pts',(-5.28847988934142,-0.0540537449324728,
35.7932898271696));
#34581=CARTESIAN_POINT('Ctrl Pts',(-4.61849544177097,-2.57690535364626,
35.872661717223));
#34582=CARTESIAN_POINT('Ctrl Pts',(-2.82345572745135,-4.47202852209511,
35.9520336072764));
#34583=CARTESIAN_POINT('Ctrl Pts',(-0.340628447537815,-5.27777544122882,
36.0314054973298));
#34584=CARTESIAN_POINT('Ctrl Pts',(2.22517516822766,-4.79786794503694,36.1107773873833));
#34585=CARTESIAN_POINT('Ctrl Pts',(4.2489310383545,-3.14921043733466,36.1901492774366));
#34586=CARTESIAN_POINT('Ctrl Pts',(5.00002147582269,-1.31403716914749,36.2504445334299));
#34587=CARTESIAN_POINT('Ctrl Pts',(5.07369910083888,-0.235423387877496,
36.2842824927386));
#34588=CARTESIAN_POINT('Ctrl Pts',(5.07347409402005,-0.00012799061592652,
36.2916631553629));
#34589=CARTESIAN_POINT('Ctrl Pts',(5.07321765521711,6.54440514305868E-5,
35.208336844637));
#34590=CARTESIAN_POINT('Ctrl Pts',(5.07337613287412,0.348482730653562,35.2192642909951));
#34591=CARTESIAN_POINT('Ctrl Pts',(4.95236148577976,1.54037186125541,35.2566490340376));
#34592=CARTESIAN_POINT('Ctrl Pts',(4.02905439992751,3.42602714375337,35.3204910737646));
#34593=CARTESIAN_POINT('Ctrl Pts',(1.8996801667365,4.93580354262787,35.3998629638181));
#34594=CARTESIAN_POINT('Ctrl Pts',(-0.69245195020073,5.24322912373406,35.4792348538714));
#34595=CARTESIAN_POINT('Ctrl Pts',(-3.11590430478548,4.27341569598948,35.5586067439249));
#34596=CARTESIAN_POINT('Ctrl Pts',(-4.78032926766171,2.26260766374704,35.6379786339782));
#34597=CARTESIAN_POINT('Ctrl Pts',(-5.28027660201491,-0.299366587187078,
35.7173505240316));
#34598=CARTESIAN_POINT('Ctrl Pts',(-4.49396024381123,-2.78841580011912,
35.7967224140851));
#34599=CARTESIAN_POINT('Ctrl Pts',(-2.61292511742748,-4.59821309619579,
35.8760943041384));
#34600=CARTESIAN_POINT('Ctrl Pts',(-0.0953872160500441,-5.28789586001125,
35.9554661941919));
#34601=CARTESIAN_POINT('Ctrl Pts',(2.4453868000212,-4.68945889688694,36.0348380842453));
#34602=CARTESIAN_POINT('Ctrl Pts',(4.39047000437915,-2.94868012642215,36.1142099742987));
#34603=CARTESIAN_POINT('Ctrl Pts',(5.02844178521537,-1.15692185290368,36.1720428944293));
#34604=CARTESIAN_POINT('Ctrl Pts',(5.07387829014872,-0.156898425299628,
36.2034185178754));
#34605=CARTESIAN_POINT('Ctrl Pts',(5.07371855919287,-0.000123991516001801,
36.208336844637));
#34606=CARTESIAN_POINT('Origin',(0.,0.,-2.20833684463713));
#34607=CARTESIAN_POINT('',(5.07403267809782,1.0680673442065E-5,34.208336844637));
#34608=CARTESIAN_POINT('',(5.07395837593185,-6.84743504405761E-5,34.2916631553629));
#34609=CARTESIAN_POINT('',(5.0736,-1.85409460923845E-12,-2.20833684463713));
#34610=CARTESIAN_POINT('Ctrl Pts',(5.07395837593184,-6.84743504405106E-5,
34.2916631553629));
#34611=CARTESIAN_POINT('Ctrl Pts',(5.07344266957576,0.774748712740892,34.315974038978));
#34612=CARTESIAN_POINT('Ctrl Pts',(4.69722240792898,2.39327548011594,34.3667422192777));
#34613=CARTESIAN_POINT('Ctrl Pts',(3.04637426047967,4.32325632045994,34.4439676962618));
#34614=CARTESIAN_POINT('Ctrl Pts',(0.607552238322964,5.25374358196314,34.5233395863151));
#34615=CARTESIAN_POINT('Ctrl Pts',(-1.97926816429518,4.90443053586424,34.6027114763686));
#34616=CARTESIAN_POINT('Ctrl Pts',(-4.08394322312674,3.36040906700167,34.6820833664219));
#34617=CARTESIAN_POINT('Ctrl Pts',(-5.19377875245966,0.997799387556786,
34.7614552564754));
#34618=CARTESIAN_POINT('Ctrl Pts',(-5.03842127392763,-1.60787201410546,
34.8408271465287));
#34619=CARTESIAN_POINT('Ctrl Pts',(-3.65571552542313,-3.82186935209593,
34.9201990365822));
#34620=CARTESIAN_POINT('Ctrl Pts',(-1.38248556671468,-5.10486777548014,
34.9995709266355));
#34621=CARTESIAN_POINT('Ctrl Pts',(1.22751481596557,-5.14433170819057,35.078942816689));
#34622=CARTESIAN_POINT('Ctrl Pts',(3.53849530653457,-3.93064782357091,35.1583147067423));
#34623=CARTESIAN_POINT('Ctrl Pts',(4.83296736710027,-1.99102597475866,35.2292214863004));
#34624=CARTESIAN_POINT('Ctrl Pts',(5.07289397138366,-0.573505529121166,
35.2736709691739));
#34625=CARTESIAN_POINT('Ctrl Pts',(5.07337786466077,0.000116280867786742,
35.2916631553629));
#34626=CARTESIAN_POINT('Ctrl Pts',(5.07403267809783,1.06806734422689E-5,
34.208336844637));
#34627=CARTESIAN_POINT('Ctrl Pts',(5.07403390825189,0.0100790925016438,
34.2086527674304));
#34628=CARTESIAN_POINT('Ctrl Pts',(5.07154731505229,0.863336953552071,34.2354259869081));
#34629=CARTESIAN_POINT('Ctrl Pts',(4.62944563286023,2.55718096342464,34.2886565030704));
#34630=CARTESIAN_POINT('Ctrl Pts',(2.84250620674923,4.45994392474861,34.3680283931238));
#34631=CARTESIAN_POINT('Ctrl Pts',(0.363138560454883,5.27627441792225,34.4474002831772));
#34632=CARTESIAN_POINT('Ctrl Pts',(-2.20468883537271,4.80731614172534,34.5267721732306));
#34633=CARTESIAN_POINT('Ctrl Pts',(-4.23545891089946,3.1673062942179,34.606144063284));
#34634=CARTESIAN_POINT('Ctrl Pts',(-5.23448057076036,0.755747644152594,
34.6855159533374));
#34635=CARTESIAN_POINT('Ctrl Pts',(-4.95839434991029,-1.83990945920924,
34.7648878433908));
#34636=CARTESIAN_POINT('Ctrl Pts',(-3.47445424064183,-3.98736869087822,
34.8442597334442));
#34637=CARTESIAN_POINT('Ctrl Pts',(-1.14414476892706,-5.16351373534018,
34.9236316234976));
#34638=CARTESIAN_POINT('Ctrl Pts',(1.4648758359769,-5.0818382631171,35.003003513551));
#34639=CARTESIAN_POINT('Ctrl Pts',(3.71705592968454,-3.76223823845686,35.0823754036044));
#34640=CARTESIAN_POINT('Ctrl Pts',(4.87836197951498,-1.83401443292226,35.1508198472998));
#34641=CARTESIAN_POINT('Ctrl Pts',(5.07299243019996,-0.495097664945923,
35.1928069943106));
#34642=CARTESIAN_POINT('Ctrl Pts',(5.07321765521711,6.54440514305868E-5,
35.208336844637));
#34643=CARTESIAN_POINT('Origin',(0.,0.,-2.20833684463713));
#34644=CARTESIAN_POINT('',(5.07324948390142,-8.11089730112791E-5,33.208336844637));
#34645=CARTESIAN_POINT('',(5.07316757009266,-1.39624117367057E-5,33.2916631553629));
#34646=CARTESIAN_POINT('',(5.0736,-1.85409460923845E-12,-2.20833684463713));
#34647=CARTESIAN_POINT('Ctrl Pts',(5.07316757009266,-1.39624117367898E-5,
33.2916631553629));
#34648=CARTESIAN_POINT('Ctrl Pts',(5.07312569317602,0.436797029802116,33.3053625154133));
#34649=CARTESIAN_POINT('Ctrl Pts',(4.90946580291021,1.7172430470973,33.3455191721481));
#34650=CARTESIAN_POINT('Ctrl Pts',(3.84462977702742,3.63177136187071,33.4121331255675));
#34651=CARTESIAN_POINT('Ctrl Pts',(1.63931253580255,5.02827960213734,33.4915050156209));
#34652=CARTESIAN_POINT('Ctrl Pts',(-0.965337610587002,5.19991006123145,
33.5708769056743));
#34653=CARTESIAN_POINT('Ctrl Pts',(-3.33483365177614,4.1048539392153,33.6502487957277));
#34654=CARTESIAN_POINT('Ctrl Pts',(-4.89197159692173,2.00986448354636,33.7296206857811));
#34655=CARTESIAN_POINT('Ctrl Pts',(-5.25743608925264,-0.574723511554913,
33.8089925758345));
#34656=CARTESIAN_POINT('Ctrl Pts',(-4.34220078737896,-3.01931013137032,
33.888364465888));
#34657=CARTESIAN_POINT('Ctrl Pts',(-2.36921498499824,-4.72839948631349,
33.9677363559413));
#34658=CARTESIAN_POINT('Ctrl Pts',(0.18090634355963,-5.28566119252548,34.0471082459947));
#34659=CARTESIAN_POINT('Ctrl Pts',(2.68695928725581,-4.55534753185087,34.1264801360481));
#34660=CARTESIAN_POINT('Ctrl Pts',(4.53847489605999,-2.71536129550809,34.2058520261016));
#34661=CARTESIAN_POINT('Ctrl Pts',(5.05594943598948,-0.980087925357289,
34.2609130325398));
#34662=CARTESIAN_POINT('Ctrl Pts',(5.07400390775537,-0.0684772480926434,
34.2895167422936));
#34663=CARTESIAN_POINT('Ctrl Pts',(5.07395837593184,-6.84743504405106E-5,
34.2916631553629));
#34664=CARTESIAN_POINT('Ctrl Pts',(5.07324948390142,-8.1108973011175E-5,
33.208336844637));
#34665=CARTESIAN_POINT('Ctrl Pts',(5.07295666213735,0.515218890813949,33.22449854055));
#34666=CARTESIAN_POINT('Ctrl Pts',(4.86710522495599,1.87431284273704,33.2671175331475));
#34667=CARTESIAN_POINT('Ctrl Pts',(3.67198507285579,3.80624052997629,33.3361938224296));
#34668=CARTESIAN_POINT('Ctrl Pts',(1.40424863498483,5.09892411381589,33.4155657124829));
#34669=CARTESIAN_POINT('Ctrl Pts',(-1.20555966211678,5.14952106980705,33.4949376025364));
#34670=CARTESIAN_POINT('Ctrl Pts',(-3.52169629398785,3.94570609146478,33.5743094925897));
#34671=CARTESIAN_POINT('Ctrl Pts',(-4.979955503786,1.78072584291395,33.6536813826432));
#34672=CARTESIAN_POINT('Ctrl Pts',(-5.22510857580638,-0.818035279400921,
33.7330532726965));
#34673=CARTESIAN_POINT('Ctrl Pts',(-4.19743676434199,-3.2175248183441,33.81242516275));
#34674=CARTESIAN_POINT('Ctrl Pts',(-2.14727864795256,-4.83323243340904,
33.8917970528034));
#34675=CARTESIAN_POINT('Ctrl Pts',(0.425951794157462,-5.27157532587404,
33.9711689428568));
#34676=CARTESIAN_POINT('Ctrl Pts',(2.89542132203897,-4.4257741373902,34.0505408329101));
#34677=CARTESIAN_POINT('Ctrl Pts',(4.6525507987008,-2.50952187653605,34.1295968001703));
#34678=CARTESIAN_POINT('Ctrl Pts',(5.07393088766675,-0.833110966960862,
34.1821954707459));
#34679=CARTESIAN_POINT('Ctrl Pts',(5.07403267809783,1.06806734422689E-5,
34.208336844637));
#34680=CARTESIAN_POINT('Origin',(0.,0.,-2.20833684463713));
#34681=CARTESIAN_POINT('',(5.07365497060222,0.000129255909634973,32.208336844637));
#34682=CARTESIAN_POINT('',(5.0738885135215,9.2741528424134E-5,32.2916631553629));
#34683=CARTESIAN_POINT('',(5.0736,-1.85409460923845E-12,-2.20833684463713));
#34684=CARTESIAN_POINT('Ctrl Pts',(5.0738885135215,9.27415284240896E-5,
32.2916631553629));
#34685=CARTESIAN_POINT('Ctrl Pts',(5.07397157552195,0.0985097427010157,
32.2947509918485));
#34686=CARTESIAN_POINT('Ctrl Pts',(5.04713500973232,1.0401410882179,32.3242961250187));
#34687=CARTESIAN_POINT('Ctrl Pts',(4.48957765297736,2.79546665964672,32.3802985548733));
#34688=CARTESIAN_POINT('Ctrl Pts',(2.60570395470567,4.60230901263064,32.4596704449267));
#34689=CARTESIAN_POINT('Ctrl Pts',(0.0870865406955613,5.28803907717593,
32.5390423349801));
#34690=CARTESIAN_POINT('Ctrl Pts',(-2.45274496186521,4.68561452739711,32.6184142250335));
#34691=CARTESIAN_POINT('Ctrl Pts',(-4.39509322077448,2.94178465017617,32.6977861150869));
#34692=CARTESIAN_POINT('Ctrl Pts',(-5.26680649947691,0.48134254370224,32.7771580051403));
#34693=CARTESIAN_POINT('Ctrl Pts',(-4.85553737278523,-2.09635354098391,
32.8565298951937));
#34694=CARTESIAN_POINT('Ctrl Pts',(-3.26147008963279,-4.16338254328624,
32.9359017852471));
#34695=CARTESIAN_POINT('Ctrl Pts',(-0.8729159117874,-5.21622077353502,33.0152736753005));
#34696=CARTESIAN_POINT('Ctrl Pts',(1.72827865000283,-4.99839916925953,33.0946455653539));
#34697=CARTESIAN_POINT('Ctrl Pts',(3.9084683581323,-3.5629785911213,33.1740174554073));
#34698=CARTESIAN_POINT('Ctrl Pts',(4.92459807825024,-1.65717664129123,33.2396899854103));
#34699=CARTESIAN_POINT('Ctrl Pts',(5.07320656921722,-0.406807195031642,
33.2789052187288));
#34700=CARTESIAN_POINT('Ctrl Pts',(5.07316757009266,-1.39624117367898E-5,
33.2916631553629));
#34701=CARTESIAN_POINT('Ctrl Pts',(5.07365497060222,0.000129255909635077,
32.208336844637));
#34702=CARTESIAN_POINT('Ctrl Pts',(5.07383759281576,0.177050513766622,32.2138870169853));
#34703=CARTESIAN_POINT('Ctrl Pts',(5.02150924629178,1.19723596214486,32.2458944860181));
#34704=CARTESIAN_POINT('Ctrl Pts',(4.35504064192764,3.00076029606972,32.3043592517354));
#34705=CARTESIAN_POINT('Ctrl Pts',(2.3893631891323,4.71825019448202,32.3837311417886));
#34706=CARTESIAN_POINT('Ctrl Pts',(-0.158357847769981,5.28638478918814,
32.4631030318421));
#34707=CARTESIAN_POINT('Ctrl Pts',(-2.66750326347463,4.56676775046226,32.5424749218955));
#34708=CARTESIAN_POINT('Ctrl Pts',(-4.52685078861515,2.73469619609277,32.6218468119489));
#34709=CARTESIAN_POINT('Ctrl Pts',(-5.28346748166331,0.23645870150246,32.7012187020024));
#34710=CARTESIAN_POINT('Ctrl Pts',(-4.75304319093522,-2.31937960938145,
32.7805905920557));
#34711=CARTESIAN_POINT('Ctrl Pts',(-3.06478809957792,-4.3102221812797,32.8599624821091));
#34712=CARTESIAN_POINT('Ctrl Pts',(-0.629957410956834,-5.25110417033318,
32.9393343721625));
#34713=CARTESIAN_POINT('Ctrl Pts',(1.95832950858626,-4.91282880661543,33.0187062622159));
#34714=CARTESIAN_POINT('Ctrl Pts',(4.06957169452659,-3.37779921996823,33.0980781522693));
#34715=CARTESIAN_POINT('Ctrl Pts',(4.96144058461863,-1.50005120370765,33.1612883464097));
#34716=CARTESIAN_POINT('Ctrl Pts',(5.07343602224469,-0.328346354394994,
33.1980412438656));
#34717=CARTESIAN_POINT('Ctrl Pts',(5.07324948390142,-8.1108973011175E-5,
33.208336844637));
#34718=CARTESIAN_POINT('Origin',(0.,0.,-2.20833684463713));
#34719=CARTESIAN_POINT('',(5.073704252564,-0.000125440355911652,31.2083368446371));
#34720=CARTESIAN_POINT('',(5.07346075270687,-0.000126888963244813,31.2916631553629));
#34721=CARTESIAN_POINT('',(5.0736,-1.85409460923845E-12,-2.20833684463713));
#34722=CARTESIAN_POINT('Ctrl Pts',(5.07346075270687,-0.000126888963244594,
31.2916631553629));
#34723=CARTESIAN_POINT('Ctrl Pts',(5.07289095298355,0.60348081698673,31.3105967649683));
#34724=CARTESIAN_POINT('Ctrl Pts',(4.81451756387892,2.05102782258644,31.3559876712581));
#34725=CARTESIAN_POINT('Ctrl Pts',(3.46819087602115,3.99281772621712,31.4278358742324));
#34726=CARTESIAN_POINT('Ctrl Pts',(1.13603804757386,5.16530336977167,31.5072077642858));
#34727=CARTESIAN_POINT('Ctrl Pts',(-1.47285113468488,5.07953254565492,31.5865796543392));
#34728=CARTESIAN_POINT('Ctrl Pts',(-3.72295704063504,3.75639883677117,31.6659515443926));
#34729=CARTESIAN_POINT('Ctrl Pts',(-5.06615885211213,1.51821468589782,31.745323434446));
#34730=CARTESIAN_POINT('Ctrl Pts',(-5.17525558096714,-1.08980320194903,
31.8246953244994));
#34731=CARTESIAN_POINT('Ctrl Pts',(-4.02367150553249,-3.43234744203962,
31.9040672145529));
#34732=CARTESIAN_POINT('Ctrl Pts',(-1.89192995759591,-4.93877944262154,
31.9834391046062));
#34733=CARTESIAN_POINT('Ctrl Pts',(0.70068154029511,-5.24213570278371,32.0628109946597));
#34734=CARTESIAN_POINT('Ctrl Pts',(3.12260856590247,-4.26851930901834,32.142182884713));
#34735=CARTESIAN_POINT('Ctrl Pts',(4.71924613978307,-2.33342987779042,32.2184669382808));
#34736=CARTESIAN_POINT('Ctrl Pts',(5.07325988110442,-0.74474986994901,32.2682936951641));
#34737=CARTESIAN_POINT('Ctrl Pts',(5.0738885135215,9.27415284240896E-5,
32.2916631553629));
#34738=CARTESIAN_POINT('Ctrl Pts',(5.073704252564,-0.000125440355911652,
31.2083368446371));
#34739=CARTESIAN_POINT('Ctrl Pts',(5.0730059773177,0.681887909050636,31.2297327901051));
#34740=CARTESIAN_POINT('Ctrl Pts',(4.76334894417968,2.20786416800771,31.2775860322575));
#34741=CARTESIAN_POINT('Ctrl Pts',(3.27920000412114,4.14943233229341,31.3518965710945));
#34742=CARTESIAN_POINT('Ctrl Pts',(0.895158610487983,5.21244975125701,31.4312684611478));
#34743=CARTESIAN_POINT('Ctrl Pts',(-1.70694143926006,5.00572594837619,31.5106403512013));
#34744=CARTESIAN_POINT('Ctrl Pts',(-3.89323433265515,3.57961838445739,31.5900122412546));
#34745=CARTESIAN_POINT('Ctrl Pts',(-5.13114396014345,1.28152370543563,31.6693841313081));
#34746=CARTESIAN_POINT('Ctrl Pts',(-5.11911827653528,-1.32874731162563,
31.7487560213615));
#34747=CARTESIAN_POINT('Ctrl Pts',(-3.86008671173927,-3.61533842470713,
31.8281279114149));
#34748=CARTESIAN_POINT('Ctrl Pts',(-1.6607465681206,-5.02124109994587,31.9074998014683));
#34749=CARTESIAN_POINT('Ctrl Pts',(0.943147763492109,-5.20398055756647,
31.9868716915216));
#34750=CARTESIAN_POINT('Ctrl Pts',(3.31729338754031,-4.11904187017945,32.0662435815751));
#34751=CARTESIAN_POINT('Ctrl Pts',(4.77384508508688,-2.17674249303873,32.1400652992802));
#34752=CARTESIAN_POINT('Ctrl Pts',(5.07296704505946,-0.666321171863868,
32.1874297203008));
#34753=CARTESIAN_POINT('Ctrl Pts',(5.07365497060222,0.000129255909635077,
32.208336844637));
#34754=CARTESIAN_POINT('Origin',(0.,0.,-2.20833684463713));
#34755=CARTESIAN_POINT('',(5.0732242396654,6.91156314036601E-5,30.208336844637));
#34756=CARTESIAN_POINT('',(5.07338983982448,0.000118254562807938,30.2916631553629));
#34757=CARTESIAN_POINT('',(5.0736,-1.85409460923845E-12,-2.20833684463713));
#34758=CARTESIAN_POINT('Ctrl Pts',(5.07338983982448,0.000118254562808118,
30.2916631553629));
#34759=CARTESIAN_POINT('Ctrl Pts',(5.07361825292341,0.265438860321299,30.2999852414035));
#34760=CARTESIAN_POINT('Ctrl Pts',(4.98815112489718,1.37411209267241,30.3347646241286));
#34761=CARTESIAN_POINT('Ctrl Pts',(4.19238095442003,3.22410968801099,30.3960013035382));
#34762=CARTESIAN_POINT('Ctrl Pts',(2.13968914249988,4.83659712202475,30.4753731935916));
#34763=CARTESIAN_POINT('Ctrl Pts',(-0.434226208411599,5.27090020273941,
30.554745083645));
#34764=CARTESIAN_POINT('Ctrl Pts',(-2.90236501609743,4.4212236610065,30.6341169736984));
#34765=CARTESIAN_POINT('Ctrl Pts',(-4.66349413013793,2.49454682166501,30.7134888637518));
#34766=CARTESIAN_POINT('Ctrl Pts',(-5.28860639654603,-0.0397961018483339,
30.7928607538052));
#34767=CARTESIAN_POINT('Ctrl Pts',(-4.62542585088724,-2.56444478303865,
30.8722326438586));
#34768=CARTESIAN_POINT('Ctrl Pts',(-2.83550180615875,-4.46440039138299,
30.951604533912));
#34769=CARTESIAN_POINT('Ctrl Pts',(-0.354855797726762,-5.27683794616905,
31.0309764239654));
#34770=CARTESIAN_POINT('Ctrl Pts',(2.21223229757146,-4.80384945735102,31.1103483140188));
#34771=CARTESIAN_POINT('Ctrl Pts',(4.24042550187443,-3.16065387386267,31.1897202040722));
#34772=CARTESIAN_POINT('Ctrl Pts',(4.99825410162456,-1.32316383571886,31.2501584845202));
#34773=CARTESIAN_POINT('Ctrl Pts',(5.07368717518548,-0.239983714616348,
31.2841394682838));
#34774=CARTESIAN_POINT('Ctrl Pts',(5.07346075270687,-0.000126888963244594,
31.2916631553629));
#34775=CARTESIAN_POINT('Ctrl Pts',(5.0732242396654,6.91156314035213E-5,
30.208336844637));
#34776=CARTESIAN_POINT('Ctrl Pts',(5.07338968774506,0.343924846945636,30.2191212665403));
#34777=CARTESIAN_POINT('Ctrl Pts',(4.95443916911164,1.53124494231641,30.256362985128));
#34778=CARTESIAN_POINT('Ctrl Pts',(4.0382761360698,3.41515258753676,30.3200620004003));
#34779=CARTESIAN_POINT('Ctrl Pts',(1.91297991407722,4.93066417388641,30.3994338904535));
#34780=CARTESIAN_POINT('Ctrl Pts',(-0.678313980675348,5.24507688131741,
30.4788057805071));
#34781=CARTESIAN_POINT('Ctrl Pts',(-3.10437209115798,4.28180047024023,30.5581776705604));
#34782=CARTESIAN_POINT('Ctrl Pts',(-4.77421203164559,2.2754869422171,30.6375495606138));
#34783=CARTESIAN_POINT('Ctrl Pts',(-5.28106448876339,-0.285130168225216,
30.7169214506672));
#34784=CARTESIAN_POINT('Ctrl Pts',(-4.50146132585641,-2.77629020081278,
30.7962933407206));
#34785=CARTESIAN_POINT('Ctrl Pts',(-2.62531214778642,-4.59115208569648,
30.8756652307741));
#34786=CARTESIAN_POINT('Ctrl Pts',(-0.109642741545517,-5.28761948484725,
30.9550371208274));
#34787=CARTESIAN_POINT('Ctrl Pts',(2.43273539384572,-4.69603448143646,31.0344090108809));
#34788=CARTESIAN_POINT('Ctrl Pts',(4.38250457206463,-2.96050587284378,31.1137809009342));
#34789=CARTESIAN_POINT('Ctrl Pts',(5.02689419953704,-1.16604718553494,31.1717568455196));
#34790=CARTESIAN_POINT('Ctrl Pts',(5.07386943415284,-0.161460170846308,
31.2032754934206));
#34791=CARTESIAN_POINT('Ctrl Pts',(5.073704252564,-0.000125440355911652,
31.2083368446371));
#34792=CARTESIAN_POINT('Origin',(0.,0.,-2.20833684463713));
#34793=CARTESIAN_POINT('',(5.07403430731529,5.85510781675173E-6,29.2083368446371));
#34794=CARTESIAN_POINT('',(5.07394886825829,-7.2464216758803E-5,29.2916631553629));
#34795=CARTESIAN_POINT('',(5.0736,-1.85409460923845E-12,-2.20833684463713));
#34796=CARTESIAN_POINT('Ctrl Pts',(5.07394886825829,-7.24642167588933E-5,
29.2916631553629));
#34797=CARTESIAN_POINT('Ctrl Pts',(5.07341208948874,0.770190548650157,29.3158310145232));
#34798=CARTESIAN_POINT('Ctrl Pts',(4.70060969038705,2.3841859592787,29.3664561703681));
#34799=CARTESIAN_POINT('Ctrl Pts',(3.05801844753361,4.31502775447088,29.4435386228973));
#34800=CARTESIAN_POINT('Ctrl Pts',(0.621713829942241,5.25208656259286,29.5229105129507));
#34801=CARTESIAN_POINT('Ctrl Pts',(-1.96603890048284,4.90974870936366,29.6022824030042));
#34802=CARTESIAN_POINT('Ctrl Pts',(-4.07486890650364,3.37140693807791,29.6816542930575));
#34803=CARTESIAN_POINT('Ctrl Pts',(-5.19106986646947,1.01179789915904,29.7610261831109));
#34804=CARTESIAN_POINT('Ctrl Pts',(-5.04273769720158,-1.59428286841832,
29.8403980731643));
#34805=CARTESIAN_POINT('Ctrl Pts',(-3.66600578680595,-3.81199985813419,
29.9197699632177));
#34806=CARTESIAN_POINT('Ctrl Pts',(-1.39624298131062,-5.10112212012718,
29.9991418532712));
#34807=CARTESIAN_POINT('Ctrl Pts',(1.21364152390063,-5.1476223247995,30.0785137433246));
#34808=CARTESIAN_POINT('Ctrl Pts',(3.52788564023963,-3.94017312521939,30.157885633378));
#34809=CARTESIAN_POINT('Ctrl Pts',(4.83020369710336,-2.00014283583164,30.2289354373907));
#34810=CARTESIAN_POINT('Ctrl Pts',(5.07289208966392,-0.578059506409542,
30.2735279447191));
#34811=CARTESIAN_POINT('Ctrl Pts',(5.07338983982448,0.000118254562808118,
30.2916631553629));
#34812=CARTESIAN_POINT('Ctrl Pts',(5.07403400238361,5.85099688312179E-6,
29.2083368446371));
#34813=CARTESIAN_POINT('Ctrl Pts',(5.07403437680669,0.00551609080175396,
29.2085097429756));
#34814=CARTESIAN_POINT('Ctrl Pts',(5.07268078911905,0.854215563279166,29.2351399379985));
#34815=CARTESIAN_POINT('Ctrl Pts',(4.6363228263275,2.54469094339263,29.2882274297059));
#34816=CARTESIAN_POINT('Ctrl Pts',(2.85451963682592,4.45226447892365,29.3675993197594));
#34817=CARTESIAN_POINT('Ctrl Pts',(0.377361782165573,5.2752762423091,29.4469712098127));
#34818=CARTESIAN_POINT('Ctrl Pts',(-2.19172056735417,4.81324238969394,29.5263430998662));
#34819=CARTESIAN_POINT('Ctrl Pts',(-4.22690463795758,3.17871334488069,29.6057149899195));
#34820=CARTESIAN_POINT('Ctrl Pts',(-5.23242409484928,0.769856765217166,
29.6850868799731));
#34821=CARTESIAN_POINT('Ctrl Pts',(-4.96333662400999,-1.82653521840426,
29.7644587700263));
#34822=CARTESIAN_POINT('Ctrl Pts',(-3.48519133772112,-3.97798726578954,
29.8438306600798));
#34823=CARTESIAN_POINT('Ctrl Pts',(-1.15806115590354,-5.16041042035391,
29.9232025501331));
#34824=CARTESIAN_POINT('Ctrl Pts',(1.45117016016719,-5.08576901889481,30.0025744401866));
#34825=CARTESIAN_POINT('Ctrl Pts',(3.70689963733188,-3.77224554159173,30.08194633024));
#34826=CARTESIAN_POINT('Ctrl Pts',(4.87583741971579,-1.84313681714053,30.1505337983901));
#34827=CARTESIAN_POINT('Ctrl Pts',(5.07298379589765,-0.499652414928338,
30.1926639698558));
#34828=CARTESIAN_POINT('Ctrl Pts',(5.0732242396654,6.91156314035213E-5,
30.208336844637));
#34829=CARTESIAN_POINT('Origin',(0.,0.,-2.20833684463713));
#34830=CARTESIAN_POINT('',(5.07324166632265,-7.76939179139569E-5,28.2083368446371));
#34831=CARTESIAN_POINT('',(5.07316594158954,-9.7399319174236E-6,28.2916631553629));
#34832=CARTESIAN_POINT('',(5.0736,-1.85409460923845E-12,-2.20833684463713));
#34833=CARTESIAN_POINT('Ctrl Pts',(5.0731664254358,-9.72907478691276E-6,
28.2916631553629));
#34834=CARTESIAN_POINT('Ctrl Pts',(5.07313755787372,0.432241135355033,28.3052194909585));
#34835=CARTESIAN_POINT('Ctrl Pts',(4.91180237168408,1.70811792520993,28.3452331232385));
#34836=CARTESIAN_POINT('Ctrl Pts',(3.85440685831077,3.62139325645763,28.4117040522031));
#34837=CARTESIAN_POINT('Ctrl Pts',(1.6528625396316,5.02384183393471,28.4910759422564));
#34838=CARTESIAN_POINT('Ctrl Pts',(-0.951315435152638,5.20249366075061,
28.5704478323099));
#34839=CARTESIAN_POINT('Ctrl Pts',(-3.32375507563475,4.11382954733206,28.6498197223633));
#34840=CARTESIAN_POINT('Ctrl Pts',(-4.8865353366993,2.02304566199065,28.7291916124167));
#34841=CARTESIAN_POINT('Ctrl Pts',(-5.25896640590637,-0.560547668676075,
28.8085635024701));
#34842=CARTESIAN_POINT('Ctrl Pts',(-4.35032489915935,-3.00759282800452,
28.8879353925235));
#34843=CARTESIAN_POINT('Ctrl Pts',(-2.38195387625792,-4.72199503162487,
28.9673072825769));
#34844=CARTESIAN_POINT('Ctrl Pts',(0.166655838534471,-5.28612969750008,
29.0466791726303));
#34845=CARTESIAN_POINT('Ctrl Pts',(2.67466855994625,-4.56257486971391,29.1260510626837));
#34846=CARTESIAN_POINT('Ctrl Pts',(4.53113794043359,-2.72758690275364,29.2054229527372));
#34847=CARTESIAN_POINT('Ctrl Pts',(5.05464511995301,-0.989211078787786,
29.2606269836302));
#34848=CARTESIAN_POINT('Ctrl Pts',(5.07399971767151,-0.0730399965665694,
29.2893737178388));
#34849=CARTESIAN_POINT('Ctrl Pts',(5.07394886825829,-7.24642167588933E-5,
29.2916631553629));
#34850=CARTESIAN_POINT('Ctrl Pts',(5.07324166632265,-7.76939179139916E-5,
28.2083368446371));
#34851=CARTESIAN_POINT('Ctrl Pts',(5.07296420662618,0.510664363139913,28.2243555160953));
#34852=CARTESIAN_POINT('Ctrl Pts',(4.86967684263928,1.86519135610718,28.266831484238));
#34853=CARTESIAN_POINT('Ctrl Pts',(3.68223314068176,3.79632723101881,28.3357647490651));
#34854=CARTESIAN_POINT('Ctrl Pts',(1.41798994671214,5.09511980804509,28.4151366391186));
#34855=CARTESIAN_POINT('Ctrl Pts',(-1.19167245960906,5.15275247768794,28.4945085291719));
#34856=CARTESIAN_POINT('Ctrl Pts',(-3.51104609249168,3.9551860491902,28.5738804192253));
#34857=CARTESIAN_POINT('Ctrl Pts',(-4.97513666881207,1.79414505376557,28.6532523092787));
#34858=CARTESIAN_POINT('Ctrl Pts',(-5.22729496488809,-0.803945705483672,
28.7326241993322));
#34859=CARTESIAN_POINT('Ctrl Pts',(-4.2060957779385,-3.20619707038074,28.8119960893855));
#34860=CARTESIAN_POINT('Ctrl Pts',(-2.16030096951815,-4.82742592572986,
28.891367979439));
#34861=CARTESIAN_POINT('Ctrl Pts',(0.41173837333167,-5.27270451089724,28.9707398694923));
#34862=CARTESIAN_POINT('Ctrl Pts',(2.88347915980534,-4.43356394814356,29.0501117595458));
#34863=CARTESIAN_POINT('Ctrl Pts',(4.64895661344711,-2.51859756056696,29.1293107512606));
#34864=CARTESIAN_POINT('Ctrl Pts',(5.07397708173548,-0.837673326665985,
29.1820524462911));
#34865=CARTESIAN_POINT('Ctrl Pts',(5.07403400238361,5.85099688312179E-6,
29.2083368446371));
#34866=CARTESIAN_POINT('Origin',(0.,0.,-2.20833684463713));
#34867=CARTESIAN_POINT('',(5.07366942975965,0.000128322057781627,27.2083368446371));
#34868=CARTESIAN_POINT('',(5.07390014538872,8.93747992460227E-5,27.2916631553629));
#34869=CARTESIAN_POINT('',(5.0736,-1.85409460923845E-12,-2.20833684463713));
#34870=CARTESIAN_POINT('Ctrl Pts',(5.07390014538872,8.93747992459192E-5,
27.2916631553629));
#34871=CARTESIAN_POINT('Ctrl Pts',(5.07397720165276,0.0939472090868575,
27.2946079673937));
#34872=CARTESIAN_POINT('Ctrl Pts',(5.04850897709501,1.03101725778952,27.324010076109));
#34873=CARTESIAN_POINT('Ctrl Pts',(4.49709775967288,2.7833528499375,27.3798694815089));
#34874=CARTESIAN_POINT('Ctrl Pts',(2.61810205366886,4.59526745509821,27.4592413715622));
#34875=CARTESIAN_POINT('Ctrl Pts',(0.101342482461748,5.28778507964899,27.5386132616156));
#34876=CARTESIAN_POINT('Ctrl Pts',(-2.44010389315526,4.69220996311103,27.617985151669));
#34877=CARTESIAN_POINT('Ctrl Pts',(-4.38714636147802,2.95362288558985,27.6973570417224));
#34878=CARTESIAN_POINT('Ctrl Pts',(-5.26548968692851,0.495539810872365,
27.7767289317758));
#34879=CARTESIAN_POINT('Ctrl Pts',(-4.86117137960698,-2.08325566491491,
27.8561008218293));
#34880=CARTESIAN_POINT('Ctrl Pts',(-3.27268248423349,-4.15457467193712,
27.9354727118826));
#34881=CARTESIAN_POINT('Ctrl Pts',(-0.886975379660524,-5.21384848487045,
28.0148446019361));
#34882=CARTESIAN_POINT('Ctrl Pts',(1.71479696411104,-5.00304034754724,28.0942164919895));
#34883=CARTESIAN_POINT('Ctrl Pts',(3.89884856306386,-3.57350265560346,28.1735883820429));
#34884=CARTESIAN_POINT('Ctrl Pts',(4.92233667869786,-1.66630250443567,28.2394039365007));
#34885=CARTESIAN_POINT('Ctrl Pts',(5.07319389740952,-0.411363633920409,
28.278762194274));
#34886=CARTESIAN_POINT('Ctrl Pts',(5.0731664254358,-9.72907478691276E-6,
28.2916631553629));
#34887=CARTESIAN_POINT('Ctrl Pts',(5.07366942975965,0.000128322057781714,
27.2083368446371));
#34888=CARTESIAN_POINT('Ctrl Pts',(5.07384715626772,0.172489015223486,27.2137439925305));
#34889=CARTESIAN_POINT('Ctrl Pts',(5.02310017357893,1.18811030837938,27.2456084371085));
#34890=CARTESIAN_POINT('Ctrl Pts',(4.36311469772634,2.98900844458398,27.3039301783709));
#34891=CARTESIAN_POINT('Ctrl Pts',(2.40207464524773,4.7117914582426,27.3833020684242));
#34892=CARTESIAN_POINT('Ctrl Pts',(-0.144105473911181,5.28679250204684,
27.4626739584777));
#34893=CARTESIAN_POINT('Ctrl Pts',(-2.65518181859737,4.57394259446923,27.542045848531));
#34894=CARTESIAN_POINT('Ctrl Pts',(-4.51946174941854,2.74689039512913,27.6214177385845));
#34895=CARTESIAN_POINT('Ctrl Pts',(-5.28281080174027,0.25070177567431,27.7007896286378));
#34896=CARTESIAN_POINT('Ctrl Pts',(-4.75927883606144,-2.30655724141581,
27.7801615186913));
#34897=CARTESIAN_POINT('Ctrl Pts',(-3.07639708040302,-4.30194401997489,
27.8595334087447));
#34898=CARTESIAN_POINT('Ctrl Pts',(-0.644111805447875,-5.24938675745965,
27.9389052987981));
#34899=CARTESIAN_POINT('Ctrl Pts',(1.94507767959709,-4.91809050014772,28.0182771888515));
#34900=CARTESIAN_POINT('Ctrl Pts',(4.06045054724861,-3.38875828300845,28.0976490789049));
#34901=CARTESIAN_POINT('Ctrl Pts',(4.95940796121397,-1.50917823199387,28.1610022975001));
#34902=CARTESIAN_POINT('Ctrl Pts',(5.07342247393797,-0.332904603741066,
28.1978982194108));
#34903=CARTESIAN_POINT('Ctrl Pts',(5.07324166632265,-7.76939179139916E-5,
28.2083368446371));
#34904=CARTESIAN_POINT('Origin',(0.,0.,-2.20833684463713));
#34905=CARTESIAN_POINT('',(5.07368988190431,-0.000126739092140837,26.2083368446371));
#34906=CARTESIAN_POINT('',(5.07344758812249,-0.000125648970980255,26.2916631553629));
#34907=CARTESIAN_POINT('',(5.0736,-1.85409460923845E-12,-2.20833684463713));
#34908=CARTESIAN_POINT('Ctrl Pts',(5.07344758812249,-0.000125648970980205,
26.2916631553629));
#34909=CARTESIAN_POINT('Ctrl Pts',(5.0728899391017,0.598926868258771,26.3104537405135));
#34910=CARTESIAN_POINT('Ctrl Pts',(4.81735989282913,2.0419133290656,26.3557016223485));
#34911=CARTESIAN_POINT('Ctrl Pts',(3.47894268615705,3.98345316700778,26.427406800868));
#34912=CARTESIAN_POINT('Ctrl Pts',(1.14995928876529,5.16222190355009,26.5067786909214));
#34913=CARTESIAN_POINT('Ctrl Pts',(-1.45915164597797,5.08348481077201,26.5861505809748));
#34914=CARTESIAN_POINT('Ctrl Pts',(-3.71281646953845,3.76642207019263,26.6655224710282));
#34915=CARTESIAN_POINT('Ctrl Pts',(-5.06204741929919,1.53186725014815,26.7448943610816));
#34916=CARTESIAN_POINT('Ctrl Pts',(-5.17817482237054,-1.07584704130177,
26.824266251135));
#34917=CARTESIAN_POINT('Ctrl Pts',(-4.032910300408,-3.42148737483758,26.9036381411884));
#34918=CARTESIAN_POINT('Ctrl Pts',(-1.90523775596165,-4.93366095719681,
26.9830100312419));
#34919=CARTESIAN_POINT('Ctrl Pts',(0.686546488664775,-5.24400565085624,
27.0623819212952));
#34920=CARTESIAN_POINT('Ctrl Pts',(3.11108952829732,-4.27692217537667,27.1417538113486));
#34921=CARTESIAN_POINT('Ctrl Pts',(4.71594148821095,-2.34252421969056,27.2181808893712));
#34922=CARTESIAN_POINT('Ctrl Pts',(5.07328489925194,-0.749306805737992,
27.2681506707093));
#34923=CARTESIAN_POINT('Ctrl Pts',(5.07390014538872,8.93747992459192E-5,
27.2916631553629));
#34924=CARTESIAN_POINT('Ctrl Pts',(5.07368988190431,-0.000126739092140768,
26.2083368446371));
#34925=CARTESIAN_POINT('Ctrl Pts',(5.07299367900981,0.677333119387493,26.2295897656503));
#34926=CARTESIAN_POINT('Ctrl Pts',(4.76643747661854,2.19875901809265,26.2772999833479));
#34927=CARTESIAN_POINT('Ctrl Pts',(3.29037472529985,4.14057671278022,26.35146749773));
#34928=CARTESIAN_POINT('Ctrl Pts',(0.909207831064193,5.21001751122215,26.4308393877834));
#34929=CARTESIAN_POINT('Ctrl Pts',(-1.69344007832135,5.01030957610855,26.5102112778369));
#34930=CARTESIAN_POINT('Ctrl Pts',(-3.88356973299385,3.59010131838702,26.5895831678902));
#34931=CARTESIAN_POINT('Ctrl Pts',(-5.12767039684481,1.29535232606086,26.6689550579437));
#34932=CARTESIAN_POINT('Ctrl Pts',(-5.12268190193029,-1.31494162567991,
26.748326947997));
#34933=CARTESIAN_POINT('Ctrl Pts',(-3.86981943456965,-3.604918707979,26.8276988380504));
#34934=CARTESIAN_POINT('Ctrl Pts',(-1.67427751864785,-5.01674557236666,
26.9070707281038));
#34935=CARTESIAN_POINT('Ctrl Pts',(0.929114694866165,-5.20650431970375,
26.9864426181573));
#34936=CARTESIAN_POINT('Ctrl Pts',(3.30617662527125,-4.12797013916282,27.0658145082107));
#34937=CARTESIAN_POINT('Ctrl Pts',(4.77079146294434,-2.18584915384965,27.1397792503706));
#34938=CARTESIAN_POINT('Ctrl Pts',(5.07297753645236,-0.6708757466937,27.1872866958461));
#34939=CARTESIAN_POINT('Ctrl Pts',(5.07366942975965,0.000128322057781714,
27.2083368446371));
#34940=CARTESIAN_POINT('Origin',(0.,0.,-2.20833684463713));
#34941=CARTESIAN_POINT('',(5.07323119136609,7.27167192501876E-5,25.2083368446371));
#34942=CARTESIAN_POINT('',(5.07340205215522,0.00012010210694157,25.2916631553629));
#34943=CARTESIAN_POINT('',(5.0736,-1.85409460923845E-12,-2.20833684463713));
#34944=CARTESIAN_POINT('Ctrl Pts',(5.07340205215522,0.000120102106941772,
25.2916631553629));
#34945=CARTESIAN_POINT('Ctrl Pts',(5.07363086957761,0.260879072720769,25.2998422169487));
#34946=CARTESIAN_POINT('Ctrl Pts',(4.98999058102238,1.36498517337352,25.334478575219));
#34947=CARTESIAN_POINT('Ctrl Pts',(4.20105773883081,3.21279554629917,25.3955722301737));
#34948=CARTESIAN_POINT('Ctrl Pts',(2.15272056265901,4.83081106300121,25.4749441202272));
#34949=CARTESIAN_POINT('Ctrl Pts',(-0.420014577610356,5.27205169757513,
25.5543160102805));
#34950=CARTESIAN_POINT('Ctrl Pts',(-2.89043509646038,4.42903220810823,25.6336879003339));
#34951=CARTESIAN_POINT('Ctrl Pts',(-4.65675202368223,2.50711027624266,25.7130597903873));
#34952=CARTESIAN_POINT('Ctrl Pts',(-5.28869446548081,-0.0255381695211706,
25.7924316804408));
#34953=CARTESIAN_POINT('Ctrl Pts',(-4.63232264181493,-2.55196557371741,
25.8718035704942));
#34954=CARTESIAN_POINT('Ctrl Pts',(-2.84752727607513,-4.45673981283608,
25.9511754605475));
#34955=CARTESIAN_POINT('Ctrl Pts',(-0.369080568778156,-5.27586209837409,
26.030547350601));
#34956=CARTESIAN_POINT('Ctrl Pts',(2.19927334812716,-4.80979605467087,26.1099192406543));
#34957=CARTESIAN_POINT('Ctrl Pts',(4.23188914543768,-3.17207433835284,26.1892911307078));
#34958=CARTESIAN_POINT('Ctrl Pts',(4.99647384522203,-1.33229055500106,26.2498724356106));
#34959=CARTESIAN_POINT('Ctrl Pts',(5.0736751134574,-0.244543947095586,26.283996443829));
#34960=CARTESIAN_POINT('Ctrl Pts',(5.07344758812249,-0.000125648970980205,
26.2916631553629));
#34961=CARTESIAN_POINT('Ctrl Pts',(5.07323119136609,7.2716719250257E-5,
25.2083368446371));
#34962=CARTESIAN_POINT('Ctrl Pts',(5.07340324942578,0.339366856221997,25.2189782420855));
#34963=CARTESIAN_POINT('Ctrl Pts',(4.95650365046512,1.52211798561692,25.2560769362184));
#34964=CARTESIAN_POINT('Ctrl Pts',(4.04746852150308,3.40425320955296,25.3196329270358));
#34965=CARTESIAN_POINT('Ctrl Pts',(1.92626575763449,4.92548896844514,25.3990048170892));
#34966=CARTESIAN_POINT('Ctrl Pts',(-0.664171081076968,5.24688651700902,
25.4783767071426));
#34967=CARTESIAN_POINT('Ctrl Pts',(-3.09281731455583,4.2901541238158,25.5577485971959));
#34968=CARTESIAN_POINT('Ctrl Pts',(-4.76806009604388,2.2883496821561,25.6371204872494));
#34969=CARTESIAN_POINT('Ctrl Pts',(-5.28181399205765,-0.2708916769007,25.7164923773028));
#34970=CARTESIAN_POINT('Ctrl Pts',(-4.50892969070311,-2.76414442307307,
25.7958642673562));
#34971=CARTESIAN_POINT('Ctrl Pts',(-2.63768009703987,-4.58405770611471,
25.8752361574096));
#34972=CARTESIAN_POINT('Ctrl Pts',(-0.123897470143628,-5.28730467858643,
25.9546080474629));
#34973=CARTESIAN_POINT('Ctrl Pts',(2.42006630623721,-4.70257593460492,26.0339799375165));
#34974=CARTESIAN_POINT('Ctrl Pts',(4.37450728714461,-2.97231010192892,26.1133518275698));
#34975=CARTESIAN_POINT('Ctrl Pts',(5.02533394688967,-1.17517261458846,26.17147079661));
#34976=CARTESIAN_POINT('Ctrl Pts',(5.07386036677103,-0.166021846101412,
26.2031324689658));
#34977=CARTESIAN_POINT('Ctrl Pts',(5.07368988190431,-0.000126739092140768,
26.2083368446371));
#34978=CARTESIAN_POINT('Origin',(0.,0.,-2.20833684463713));
#34979=CARTESIAN_POINT('',(5.07403460521456,1.01146903839872E-6,24.2083368446371));
#34980=CARTESIAN_POINT('',(5.07393893245752,-7.63518475177419E-5,24.2916631553629));
#34981=CARTESIAN_POINT('',(5.0736,-1.85409460923845E-12,-2.20833684463713));
#34982=CARTESIAN_POINT('Ctrl Pts',(5.07393893245752,-7.63518475176573E-5,
24.2916631553629));
#34983=CARTESIAN_POINT('Ctrl Pts',(5.0733825372435,0.765632623134578,24.3156879900684));
#34984=CARTESIAN_POINT('Ctrl Pts',(4.70398212533016,2.37509554318665,24.3661701214584));
#34985=CARTESIAN_POINT('Ctrl Pts',(3.0696404085172,4.30676782630642,24.4431095495329));
#34986=CARTESIAN_POINT('Ctrl Pts',(0.635870902865647,5.25039137038364,24.5224814395863));
#34987=CARTESIAN_POINT('Ctrl Pts',(-1.95279534724764,4.9150311981795,24.6018533296397));
#34988=CARTESIAN_POINT('Ctrl Pts',(-4.06576497321052,3.38238030533593,24.6812252196931));
#34989=CARTESIAN_POINT('Ctrl Pts',(-5.18832325111748,1.02578905688434,24.7605971097465));
#34990=CARTESIAN_POINT('Ctrl Pts',(-5.04701746921096,-1.58068213527875,
24.8399689997999));
#34991=CARTESIAN_POINT('Ctrl Pts',(-3.67626940318832,-3.80210265806849,
24.9193408898533));
#34992=CARTESIAN_POINT('Ctrl Pts',(-1.40999024783327,-5.09733938916421,
24.9987127799067));
#34993=CARTESIAN_POINT('Ctrl Pts',(1.19975941093347,-5.1508755278289,25.0780846699601));
#34994=CARTESIAN_POINT('Ctrl Pts',(3.51725033281924,-3.94966978918403,25.1574565600135));
#34995=CARTESIAN_POINT('Ctrl Pts',(4.82742597758186,-2.00925929492118,25.2286493884811));
#34996=CARTESIAN_POINT('Ctrl Pts',(5.07289070026022,-0.582613469337955,
25.2733849202643));
#34997=CARTESIAN_POINT('Ctrl Pts',(5.07340205215522,0.000120102106941772,
25.2916631553629));
#34998=CARTESIAN_POINT('Ctrl Pts',(5.07403455984306,1.01136344364921E-6,
24.2083368446371));
#34999=CARTESIAN_POINT('Ctrl Pts',(5.07403457120051,0.000953086505682821,
24.2083667185208));
#35000=CARTESIAN_POINT('Ctrl Pts',(5.07380195086792,0.845094303182403,24.2348538890889));
#35001=CARTESIAN_POINT('Ctrl Pts',(4.64316632240633,2.53218242822061,24.2877983563415));
#35002=CARTESIAN_POINT('Ctrl Pts',(2.86651231988729,4.4445526734691,24.3671702463949));
#35003=CARTESIAN_POINT('Ctrl Pts',(0.391582261162602,5.27423972531146,24.4465421364484));
#35004=CARTESIAN_POINT('Ctrl Pts',(-2.1787363696294,4.81913365439931,24.5259140265017));
#35005=CARTESIAN_POINT('Ctrl Pts',(-4.21831964333045,3.19009729224708,24.6052859165552));
#35006=CARTESIAN_POINT('Ctrl Pts',(-5.23032958900859,0.783960290863936,
24.6846578066085));
#35007=CARTESIAN_POINT('Ctrl Pts',(-4.9682428239423,-1.81314770210696,24.764029696662));
#35008=CARTESIAN_POINT('Ctrl Pts',(-3.49590310398264,-3.96857692817898,
24.8434015867153));
#35009=CARTESIAN_POINT('Ctrl Pts',(-1.17196912594307,-5.15726959884261,
24.9227734767688));
#35010=CARTESIAN_POINT('Ctrl Pts',(1.43745393706658,-5.08966281065081,25.0021453668222));
#35011=CARTESIAN_POINT('Ctrl Pts',(3.69671640275713,-3.78222542756197,25.0815172568756));
#35012=CARTESIAN_POINT('Ctrl Pts',(4.87329911188321,-1.85225894830422,25.1502477494805));
#35013=CARTESIAN_POINT('Ctrl Pts',(5.07297546809779,-0.504207096881882,
25.192520945401));
#35014=CARTESIAN_POINT('Ctrl Pts',(5.07323119136609,7.2716719250257E-5,
25.2083368446371));
#35015=CARTESIAN_POINT('Origin',(0.,0.,-2.20833684463713));
#35016=CARTESIAN_POINT('',(5.07323420419449,-7.41988534934401E-5,23.2083368446371));
#35017=CARTESIAN_POINT('',(5.07316553675605,-5.48786176412603E-6,23.2916631553629));
#35018=CARTESIAN_POINT('',(5.0736,-1.85409460923845E-12,-2.20833684463713));
#35019=CARTESIAN_POINT('Ctrl Pts',(5.07316569050492,-5.48591970746248E-6,
23.2916631553629));
#35020=CARTESIAN_POINT('Ctrl Pts',(5.07314958741115,0.42768514602335,23.3050764665037));
#35021=CARTESIAN_POINT('Ctrl Pts',(4.91412543793041,1.69899265595715,23.344947074329));
#35022=CARTESIAN_POINT('Ctrl Pts',(3.86415592530766,3.6109888303426,23.4112749788386));
#35023=CARTESIAN_POINT('Ctrl Pts',(1.66640053022393,5.01936755177924,23.4906468688921));
#35024=CARTESIAN_POINT('Ctrl Pts',(-0.937286345425383,5.20503944789203,
23.5700187589454));
#35025=CARTESIAN_POINT('Ctrl Pts',(-3.31265234202061,4.12277525560054,23.6493906489989));
#35026=CARTESIAN_POINT('Ctrl Pts',(-4.88106356050821,2.03621213668325,23.7287625390522));
#35027=CARTESIAN_POINT('Ctrl Pts',(-5.26045849971908,-0.546367751667005,
23.8081344291057));
#35028=CARTESIAN_POINT('Ctrl Pts',(-4.35841739221935,-2.99585366506712,
23.887506319159));
#35029=CARTESIAN_POINT('Ctrl Pts',(-2.3946754551717,-4.71555625687105,23.9668782092125));
#35030=CARTESIAN_POINT('Ctrl Pts',(0.152404122233421,-5.28655978220554,
24.0462500992659));
#35031=CARTESIAN_POINT('Ctrl Pts',(2.66235839280233,-4.56976904619763,24.1256219893193));
#35032=CARTESIAN_POINT('Ctrl Pts',(4.52376805191542,-2.73979268554746,24.2049938793727));
#35033=CARTESIAN_POINT('Ctrl Pts',(5.05332835032277,-0.998334355631039,
24.2603409347206));
#35034=CARTESIAN_POINT('Ctrl Pts',(5.07399526625627,-0.0776027111923523,
24.289230693384));
#35035=CARTESIAN_POINT('Ctrl Pts',(5.07393893245752,-7.63518475176573E-5,
24.2916631553629));
#35036=CARTESIAN_POINT('Ctrl Pts',(5.07323420419449,-7.41988534933707E-5,
23.2083368446371));
#35037=CARTESIAN_POINT('Ctrl Pts',(5.07297208311489,0.506109773689648,23.2242124916405));
#35038=CARTESIAN_POINT('Ctrl Pts',(4.87223466883649,1.85606959653113,23.2665454353283));
#35039=CARTESIAN_POINT('Ctrl Pts',(3.69245444696201,3.78638634033052,23.3353356757007));
#35040=CARTESIAN_POINT('Ctrl Pts',(1.43172095156667,5.09127847004479,23.4147075657541));
#35041=CARTESIAN_POINT('Ctrl Pts',(-1.17777659548102,5.1559464348325,23.4940794558075));
#35042=CARTESIAN_POINT('Ctrl Pts',(-3.50037037246962,3.96463726004727,23.5734513458609));
#35043=CARTESIAN_POINT('Ctrl Pts',(-4.97028167379665,1.80755122457705,23.6528232359143));
#35044=CARTESIAN_POINT('Ctrl Pts',(-5.22944336137752,-0.789850288405212,
23.7321951259677));
#35045=CARTESIAN_POINT('Ctrl Pts',(-4.21472422106041,-3.19484601935549,
23.8115670160211));
#35046=CARTESIAN_POINT('Ctrl Pts',(-2.17330758975551,-4.82158433170509,
23.8909389060745));
#35047=CARTESIAN_POINT('Ctrl Pts',(0.397521959947206,-5.27379537322471,
23.9703107961279));
#35048=CARTESIAN_POINT('Ctrl Pts',(2.87151604007067,-4.4413215351868,24.0496826861813));
#35049=CARTESIAN_POINT('Ctrl Pts',(4.64534728528402,-2.52767212981305,24.129024702351));
#35050=CARTESIAN_POINT('Ctrl Pts',(5.07402451266825,-0.842236060605585,
24.1819094218363));
#35051=CARTESIAN_POINT('Ctrl Pts',(5.07403455984306,1.01136344364921E-6,
24.2083368446371));
#35052=CARTESIAN_POINT('Origin',(0.,0.,-2.20833684463713));
#35053=CARTESIAN_POINT('',(5.07368445537635,0.000127432987209741,22.2083368446371));
#35054=CARTESIAN_POINT('',(5.0739114897015,8.59482686052055E-5,22.2916631553629));
#35055=CARTESIAN_POINT('',(5.0736,-1.85409460923845E-12,-2.20833684463713));
#35056=CARTESIAN_POINT('Ctrl Pts',(5.0739114897015,8.59482686050433E-5,
22.2916631553629));
#35057=CARTESIAN_POINT('Ctrl Pts',(5.07398263122595,0.0893847065795861,
22.2944649429389));
#35058=CARTESIAN_POINT('Ctrl Pts',(5.04987059102411,1.02189374093949,22.3237240271994));
#35059=CARTESIAN_POINT('Ctrl Pts',(4.50458503707303,2.77121862106756,22.3794404081444));
#35060=CARTESIAN_POINT('Ctrl Pts',(2.63048120009391,4.58819259887664,22.4588122981978));
#35061=CARTESIAN_POINT('Ctrl Pts',(0.115597647321455,5.28749259670008,22.5381841882512));
#35062=CARTESIAN_POINT('Ctrl Pts',(-2.42744506809483,4.69877132337436,22.6175560783046));
#35063=CARTESIAN_POINT('Ctrl Pts',(-4.37916762715256,2.96543963879382,22.696927968358));
#35064=CARTESIAN_POINT('Ctrl Pts',(-5.26413459813381,0.509733484286287,
22.7762998584114));
#35065=CARTESIAN_POINT('Ctrl Pts',(-4.86677005798463,-2.07014265165558,
22.8556717484648));
#35066=CARTESIAN_POINT('Ctrl Pts',(-3.28387109087741,-4.14573660239302,
22.9350436385182));
#35067=CARTESIAN_POINT('Ctrl Pts',(-0.901028401772815,-5.21143830245831,
23.0144155285717));
#35068=CARTESIAN_POINT('Ctrl Pts',(1.70130281532621,-5.00764516247504,23.093787418625));
#35069=CARTESIAN_POINT('Ctrl Pts',(3.88920043041414,-3.58400074773866,23.1731593086785));
#35070=CARTESIAN_POINT('Ctrl Pts',(4.92006185002291,-1.67542824897262,23.239117887591));
#35071=CARTESIAN_POINT('Ctrl Pts',(5.07318135021192,-0.415919972782139,
23.2786191698192));
#35072=CARTESIAN_POINT('Ctrl Pts',(5.07316569050492,-5.48591970746248E-6,
23.2916631553629));
#35073=CARTESIAN_POINT('Ctrl Pts',(5.07368445537635,0.000127432987209863,
22.2083368446371));
#35074=CARTESIAN_POINT('Ctrl Pts',(5.07385799503573,0.167927931732477,22.2136009680757));
#35075=CARTESIAN_POINT('Ctrl Pts',(5.02468445773871,1.17898674996513,22.2453223881989));
#35076=CARTESIAN_POINT('Ctrl Pts',(4.37115162329097,2.97723307464397,22.3035011050064));
#35077=CARTESIAN_POINT('Ctrl Pts',(2.4147715124657,4.70529942618521,22.3828729950599));
#35078=CARTESIAN_POINT('Ctrl Pts',(-0.129853572474074,5.28716128664959,
22.4622448851132));
#35079=CARTESIAN_POINT('Ctrl Pts',(-2.64284027062663,4.58108446095525,22.5416167751666));
#35080=CARTESIAN_POINT('Ctrl Pts',(-4.51204028846786,2.7590644882843,22.62098866522));
#35081=CARTESIAN_POINT('Ctrl Pts',(-5.28211549991429,0.264943102456049,
22.7003605552734));
#35082=CARTESIAN_POINT('Ctrl Pts',(-4.76548000969985,-2.2937181486802,22.7797324453269));
#35083=CARTESIAN_POINT('Ctrl Pts',(-3.08798363825926,-4.29363457062517,
22.8591043353802));
#35084=CARTESIAN_POINT('Ctrl Pts',(-0.658261551986295,-5.24763120247219,
22.9384762254337));
#35085=CARTESIAN_POINT('Ctrl Pts',(1.93181173129385,-4.92331644248731,23.017848115487));
#35086=CARTESIAN_POINT('Ctrl Pts',(4.05129987868926,-3.39969271923279,23.0972200055405));
#35087=CARTESIAN_POINT('Ctrl Pts',(4.95736217363157,-1.51830523331034,23.1607162485905));
#35088=CARTESIAN_POINT('Ctrl Pts',(5.07340891666056,-0.3374627456306,23.197755194956));
#35089=CARTESIAN_POINT('Ctrl Pts',(5.07323420419449,-7.41988534933707E-5,
23.2083368446371));
#35090=CARTESIAN_POINT('Origin',(0.,0.,-2.20833684463713));
#35091=CARTESIAN_POINT('',(5.0647135783285,-0.000493560823505712,21.2083368446371));
#35092=CARTESIAN_POINT('',(5.07311795825563,-0.000541267147824199,21.2916631553629));
#35093=CARTESIAN_POINT('',(5.0736,-1.85409460923845E-12,-2.20833684463713));
#35094=CARTESIAN_POINT('Ctrl Pts',(5.07311795825563,-0.000541267147824084,
21.2916631553629));
#35095=CARTESIAN_POINT('Ctrl Pts',(5.07265472641037,0.594063927299599,21.3103107160587));
#35096=CARTESIAN_POINT('Ctrl Pts',(4.82066183061084,2.03342224951305,21.3554155734389));
#35097=CARTESIAN_POINT('Ctrl Pts',(3.48937383888172,3.97367066688458,21.4269777275036));
#35098=CARTESIAN_POINT('Ctrl Pts',(1.16402860508423,5.15930893371516,21.5063496175569));
#35099=CARTESIAN_POINT('Ctrl Pts',(-1.44552439996815,5.08729102078623,21.5857215076104));
#35100=CARTESIAN_POINT('Ctrl Pts',(-3.70260503654192,3.77647571272897,21.6650933976637));
#35101=CARTESIAN_POINT('Ctrl Pts',(-5.057922432142,1.54547807796832,21.7444652877172));
#35102=CARTESIAN_POINT('Ctrl Pts',(-5.18104412158608,-1.06186685398839,
21.8238371777705));
#35103=CARTESIAN_POINT('Ctrl Pts',(-4.04212630117128,-3.41061102326193,
21.903209067824));
#35104=CARTESIAN_POINT('Ctrl Pts',(-1.91852825506946,-4.92850206746972,
21.9825809578774));
#35105=CARTESIAN_POINT('Ctrl Pts',(0.672404619068471,-5.245839892308,22.0619528479308));
#35106=CARTESIAN_POINT('Ctrl Pts',(3.09954884704109,-4.28529268150223,22.1413247379842));
#35107=CARTESIAN_POINT('Ctrl Pts',(4.71262161876037,-2.35161833566565,22.2178948404616));
#35108=CARTESIAN_POINT('Ctrl Pts',(5.07331084138903,-0.753863997357442,
22.2680076462545));
#35109=CARTESIAN_POINT('Ctrl Pts',(5.0739114897015,8.59482686050433E-5,
22.2916631553629));
#35110=CARTESIAN_POINT('Ctrl Pts',(5.0647135783285,-0.000493560823505643,
21.2083368446371));
#35111=CARTESIAN_POINT('Ctrl Pts',(5.06741194864459,0.674127865172368,21.2294467411954));
#35112=CARTESIAN_POINT('Ctrl Pts',(4.7845254230904,2.19368980981962,21.2770139344383));
#35113=CARTESIAN_POINT('Ctrl Pts',(3.29092685490723,4.12830747359771,21.3510384243656));
#35114=CARTESIAN_POINT('Ctrl Pts',(0.929079443196039,5.20946188754723,21.430410314419));
#35115=CARTESIAN_POINT('Ctrl Pts',(-1.68303999757346,5.01382783115869,21.5097822044724));
#35116=CARTESIAN_POINT('Ctrl Pts',(-3.8722246926078,3.60110493868854,21.5891540945258));
#35117=CARTESIAN_POINT('Ctrl Pts',(-5.12503498129818,1.30888173016128,21.6685259845792));
#35118=CARTESIAN_POINT('Ctrl Pts',(-5.12574462250326,-1.300972874894,21.7478978746326));
#35119=CARTESIAN_POINT('Ctrl Pts',(-3.87976959979778,-3.59455409188016,
21.827269764686));
#35120=CARTESIAN_POINT('Ctrl Pts',(-1.68766624540451,-5.01217052435348,
21.9066416547394));
#35121=CARTESIAN_POINT('Ctrl Pts',(0.915005995631755,-5.2090130440819,21.9860135447928));
#35122=CARTESIAN_POINT('Ctrl Pts',(3.29507231119182,-4.13685632854986,22.0653854348462));
#35123=CARTESIAN_POINT('Ctrl Pts',(4.76770779675958,-2.19496036885575,22.139493201461));
#35124=CARTESIAN_POINT('Ctrl Pts',(5.07298579089609,-0.675431391209716,
22.1871436713913));
#35125=CARTESIAN_POINT('Ctrl Pts',(5.07368445537635,0.000127432987209863,
22.2083368446371));
#35126=CARTESIAN_POINT('Origin',(0.,0.,-2.20833684463713));
#35127=CARTESIAN_POINT('',(5.07022284182504,-0.00437131830465176,20.2083368446371));
#35128=CARTESIAN_POINT('',(5.07763086250027,0.00422747191343611,20.2916631553629));
#35129=CARTESIAN_POINT('',(5.0736,-1.85409460923845E-12,-2.20833684463713));
#35130=CARTESIAN_POINT('Ctrl Pts',(5.07763086250027,0.00422747191343598,
20.2916631553629));
#35131=CARTESIAN_POINT('Ctrl Pts',(5.07981016603818,0.259793667372929,20.2996991924939));
#35132=CARTESIAN_POINT('Ctrl Pts',(4.94610737387947,2.19579442888697,20.3606498229938));
#35133=CARTESIAN_POINT('Ctrl Pts',(2.45559119020176,5.46873373673919,20.4745150468627));
#35134=CARTESIAN_POINT('Ctrl Pts',(-3.26379011618977,5.03400372054189,20.6332588269695));
#35135=CARTESIAN_POINT('Ctrl Pts',(-5.99600976813329,-0.0197068834827358,
20.7920026070763));
#35136=CARTESIAN_POINT('Ctrl Pts',(-3.70230252414087,-4.19446206534972,
20.9242890904987));
#35137=CARTESIAN_POINT('Ctrl Pts',(-0.376480053418488,-5.26605971579228,
21.0301182772365));
#35138=CARTESIAN_POINT('Ctrl Pts',(2.18257651229242,-4.8205851862161,21.10949016729));
#35139=CARTESIAN_POINT('Ctrl Pts',(4.22530652207796,-3.18086119603153,21.1888620573433));
#35140=CARTESIAN_POINT('Ctrl Pts',(4.99434160286696,-1.34186431057878,21.249586386701));
#35141=CARTESIAN_POINT('Ctrl Pts',(5.07331196316984,-0.249566309185764,
21.2838534193742));
#35142=CARTESIAN_POINT('Ctrl Pts',(5.07311795825563,-0.000541267147824084,
21.2916631553629));
#35143=CARTESIAN_POINT('Ctrl Pts',(5.07022284182504,-0.00437131830465176,
20.2083368446371));
#35144=CARTESIAN_POINT('Ctrl Pts',(5.06064558604025,1.17531423721709,20.2452925143152));
#35145=CARTESIAN_POINT('Ctrl Pts',(4.06283412548092,4.05874270439873,20.3351627773622));
#35146=CARTESIAN_POINT('Ctrl Pts',(-0.73672307947618,5.95134306184733,20.4779476337782));
#35147=CARTESIAN_POINT('Ctrl Pts',(-5.3995463563661,2.60828838171381,20.6366914138849));
#35148=CARTESIAN_POINT('Ctrl Pts',(-5.1196790448508,-3.11863163173554,20.7954351939918));
#35149=CARTESIAN_POINT('Ctrl Pts',(-0.158509478954971,-5.99736559883163,
20.9541789740985));
#35150=CARTESIAN_POINT('Ctrl Pts',(4.27441519030586,-3.72585141387614,21.091812857647));
#35151=CARTESIAN_POINT('Ctrl Pts',(5.06064814629056,-1.01689503187705,21.1765321478265));
#35152=CARTESIAN_POINT('Ctrl Pts',(5.0647135783285,-0.000493560823505643,
21.2083368446371));
#35153=CARTESIAN_POINT('Origin',(0.,0.,-2.20833684463713));
#35154=CARTESIAN_POINT('',(5.08190747034449,-0.0016131106486481,19.2083368446371));
#35155=CARTESIAN_POINT('',(5.0654395261759,0.00158764291868628,19.2916631553629));
#35156=CARTESIAN_POINT('',(5.0736,-1.85409460923845E-12,-2.20833684463713));
#35157=CARTESIAN_POINT('Ctrl Pts',(5.0654395261759,0.00158764291868674,
19.2916631553629));
#35158=CARTESIAN_POINT('Ctrl Pts',(5.06734596007678,0.765537039397172,19.3155449656136));
#35159=CARTESIAN_POINT('Ctrl Pts',(4.5467586954857,3.21970245674355,19.3923413692333));
#35160=CARTESIAN_POINT('Ctrl Pts',(0.736723079475925,5.95134306184737,19.5220523662219));
#35161=CARTESIAN_POINT('Ctrl Pts',(-4.59927593805429,3.84720861430001,19.6807961463287));
#35162=CARTESIAN_POINT('Ctrl Pts',(-5.72720375155086,-1.77677009197966,
19.8395399264355));
#35163=CARTESIAN_POINT('Ctrl Pts',(-1.61419617037545,-5.77483540889735,
19.9982837065423));
#35164=CARTESIAN_POINT('Ctrl Pts',(3.69280075007907,-4.55444079317796,20.1489914495181));
#35165=CARTESIAN_POINT('Ctrl Pts',(5.0654601874783,-1.42302350869954,20.246784599125));
#35166=CARTESIAN_POINT('Ctrl Pts',(5.07763086250027,0.00422747191343598,
20.2916631553629));
#35167=CARTESIAN_POINT('Ctrl Pts',(5.08190747034449,-0.00161311064864815,
19.2083368446371));
#35168=CARTESIAN_POINT('Ctrl Pts',(5.08137262398886,1.67206424053112,19.2611382874349));
#35169=CARTESIAN_POINT('Ctrl Pts',(3.25971341308398,5.0343135906333,19.3668543236016));
#35170=CARTESIAN_POINT('Ctrl Pts',(-2.45559119020206,5.46873373673905,19.5254849531373));
#35171=CARTESIAN_POINT('Ctrl Pts',(-5.92771323046149,0.905806267444168,
19.6842287332441));
#35172=CARTESIAN_POINT('Ctrl Pts',(-3.97578039972873,-4.48936692070992,
19.8429725133509));
#35173=CARTESIAN_POINT('Ctrl Pts',(1.61419617037569,-5.77483540889728,20.0017162934577));
#35174=CARTESIAN_POINT('Ctrl Pts',(4.76969253787625,-2.70752266133374,20.1235044038864));
#35175=CARTESIAN_POINT('Ctrl Pts',(5.0743586806711,-0.513806323102652,20.1923779209462));
#35176=CARTESIAN_POINT('Ctrl Pts',(5.07022284182504,-0.00437131830465176,
20.2083368446371));
#35177=CARTESIAN_POINT('Origin',(0.,0.,-2.20833684463713));
#35178=CARTESIAN_POINT('',(5.07322996641872,-7.44046081432859E-5,18.2083368446371));
#35179=CARTESIAN_POINT('',(5.0733324096026,-5.65345686568016E-5,18.2916631553629));
#35180=CARTESIAN_POINT('',(5.0736,-1.85409460923845E-12,-2.20833684463713));
#35181=CARTESIAN_POINT('Ctrl Pts',(5.0733324096026,-5.65345686565077E-5,
18.2916631553629));
#35182=CARTESIAN_POINT('Ctrl Pts',(5.07342932055268,0.423040487316443,18.3049334420489));
#35183=CARTESIAN_POINT('Ctrl Pts',(4.9168904884294,1.68971643561363,18.3446610254193));
#35184=CARTESIAN_POINT('Ctrl Pts',(3.87222469260764,3.60110493868871,18.4108459054742));
#35185=CARTESIAN_POINT('Ctrl Pts',(1.68303999757325,5.01382783115876,18.4902177955276));
#35186=CARTESIAN_POINT('Ctrl Pts',(-0.929079443196312,5.2094618875472,18.569589685581));
#35187=CARTESIAN_POINT('Ctrl Pts',(-3.29092685490746,4.12830747359753,18.6489615756344));
#35188=CARTESIAN_POINT('Ctrl Pts',(-5.42625155540715,1.36247937795741,18.7547907623723));
#35189=CARTESIAN_POINT('Ctrl Pts',(-4.95432466322409,-3.37745298000962,
18.8870772457946));
#35190=CARTESIAN_POINT('Ctrl Pts',(0.158509478955228,-5.99736559883162,
19.0458210259014));
#35191=CARTESIAN_POINT('Ctrl Pts',(4.3733083201864,-3.5517155504766,19.1806829957575));
#35192=CARTESIAN_POINT('Ctrl Pts',(5.06312190111345,-0.927134966817506,
19.2626303722447));
#35193=CARTESIAN_POINT('Ctrl Pts',(5.0654395261759,0.00158764291868674,
19.2916631553629));
#35194=CARTESIAN_POINT('Ctrl Pts',(5.07322996641872,-7.44046081432165E-5,
18.2083368446371));
#35195=CARTESIAN_POINT('Ctrl Pts',(5.07298661447134,0.501546775803683,18.2240694671857));
#35196=CARTESIAN_POINT('Ctrl Pts',(4.87479289587003,1.8469289142109,18.2662593864187));
#35197=CARTESIAN_POINT('Ctrl Pts',(3.70260503654169,3.77647571272922,18.3349066023362));
#35198=CARTESIAN_POINT('Ctrl Pts',(1.44552439996779,5.08729102078633,18.4142784923897));
#35199=CARTESIAN_POINT('Ctrl Pts',(-1.16402860508455,5.15930893371508,18.4936503824431));
#35200=CARTESIAN_POINT('Ctrl Pts',(-3.48937383888192,3.97367066688439,18.5730222724965));
#35201=CARTESIAN_POINT('Ctrl Pts',(-4.96594823061187,1.82167865277138,18.6523941625499));
#35202=CARTESIAN_POINT('Ctrl Pts',(-5.23050112077116,-0.77713504302674,
18.7317660526033));
#35203=CARTESIAN_POINT('Ctrl Pts',(-4.22530652207786,-3.18086119603167,
18.8111379426567));
#35204=CARTESIAN_POINT('Ctrl Pts',(-2.18257651229225,-4.82058518621618,
18.8905098327101));
#35205=CARTESIAN_POINT('Ctrl Pts',(0.37648005341871,-5.26605971579227,18.9698817227635));
#35206=CARTESIAN_POINT('Ctrl Pts',(3.70230252414111,-4.19446206534953,19.0757109095013));
#35207=CARTESIAN_POINT('Ctrl Pts',(5.08048878136776,-1.68603810060634,19.1551959501259));
#35208=CARTESIAN_POINT('Ctrl Pts',(5.08190861649065,-0.00519970863047212,
19.2082236940659));
#35209=CARTESIAN_POINT('Ctrl Pts',(5.08190747034449,-0.00161311064864815,
19.2083368446371));
#35210=CARTESIAN_POINT('Origin',(0.,0.,-2.20833684463713));
#35211=CARTESIAN_POINT('',(5.07369825422177,0.000126003717071388,17.2083368446371));
#35212=CARTESIAN_POINT('',(5.07392231800261,8.23068815517256E-5,17.2916631553629));
#35213=CARTESIAN_POINT('',(5.0736,-1.85409460923845E-12,-2.20833684463713));
#35214=CARTESIAN_POINT('Ctrl Pts',(5.07392231800261,8.23068815519051E-5,
17.2916631553629));
#35215=CARTESIAN_POINT('Ctrl Pts',(5.07398762507078,0.0848220371273371,
17.2943219184842));
#35216=CARTESIAN_POINT('Ctrl Pts',(5.05121938853888,1.01276996498335,17.3234379782898));
#35217=CARTESIAN_POINT('Ctrl Pts',(4.51204028846775,2.7590644882845,17.3790113347799));
#35218=CARTESIAN_POINT('Ctrl Pts',(2.64284027062647,4.58108446095533,17.4583832248334));
#35219=CARTESIAN_POINT('Ctrl Pts',(0.129853572473924,5.28716128664959,17.5377551148867));
#35220=CARTESIAN_POINT('Ctrl Pts',(-2.41477151246584,4.70529942618515,17.6171270049402));
#35221=CARTESIAN_POINT('Ctrl Pts',(-4.37115162329109,2.9772330746438,17.6964988949936));
#35222=CARTESIAN_POINT('Ctrl Pts',(-5.2627514922539,0.523926824466488,17.775870785047));
#35223=CARTESIAN_POINT('Ctrl Pts',(-4.87231403886184,-2.05702097999283,
17.8552426751004));
#35224=CARTESIAN_POINT('Ctrl Pts',(-3.29507231119166,-4.13685632854999,
17.9346145651538));
#35225=CARTESIAN_POINT('Ctrl Pts',(-0.915005995631555,-5.20901304408194,
18.0139864552072));
#35226=CARTESIAN_POINT('Ctrl Pts',(1.68766624540468,-5.01217052435341,18.0933583452606));
#35227=CARTESIAN_POINT('Ctrl Pts',(3.8797695997979,-3.59455409188004,18.172730235314));
#35228=CARTESIAN_POINT('Ctrl Pts',(4.9174284825737,-1.68443961943593,18.2388318386815));
#35229=CARTESIAN_POINT('Ctrl Pts',(5.07323610680991,-0.420498442869185,
18.2784761453644));
#35230=CARTESIAN_POINT('Ctrl Pts',(5.0733324096026,-5.65345686565077E-5,
18.2916631553629));
#35231=CARTESIAN_POINT('Ctrl Pts',(5.07369825422177,0.000126003717071926,
17.2083368446371));
#35232=CARTESIAN_POINT('Ctrl Pts',(5.07386566986272,0.163365799600409,17.2134579436209));
#35233=CARTESIAN_POINT('Ctrl Pts',(5.02624395147431,1.16985927909857,17.2450363392892));
#35234=CARTESIAN_POINT('Ctrl Pts',(4.37916762715237,2.96543963879408,17.303072031642));
#35235=CARTESIAN_POINT('Ctrl Pts',(2.42744506809458,4.69877132337447,17.3824439216954));
#35236=CARTESIAN_POINT('Ctrl Pts',(-0.115597647321682,5.28749259670007,
17.4618158117488));
#35237=CARTESIAN_POINT('Ctrl Pts',(-2.63048120009413,4.58819259887652,17.5411877018022));
#35238=CARTESIAN_POINT('Ctrl Pts',(-4.5045850370732,2.7712186210673,17.6205595918556));
#35239=CARTESIAN_POINT('Ctrl Pts',(-5.28138253005218,0.27918271172893,17.699931481909));
#35240=CARTESIAN_POINT('Ctrl Pts',(-4.77164579536179,-2.28086298099153,
17.7793033719624));
#35241=CARTESIAN_POINT('Ctrl Pts',(-3.09954884704088,-4.28529268150238,
17.8586752620158));
#35242=CARTESIAN_POINT('Ctrl Pts',(-0.672404619068171,-5.24583989230806,
17.9380471520692));
#35243=CARTESIAN_POINT('Ctrl Pts',(1.91852825506979,-4.9285020674696,18.0174190421226));
#35244=CARTESIAN_POINT('Ctrl Pts',(4.04212630117149,-3.41061102326166,18.096790932176));
#35245=CARTESIAN_POINT('Ctrl Pts',(4.95529462550652,-1.52742091164643,18.1604301996809));
#35246=CARTESIAN_POINT('Ctrl Pts',(5.07339585550224,-0.342021443822988,
18.1976121705012));
#35247=CARTESIAN_POINT('Ctrl Pts',(5.07322996641872,-7.44046081432165E-5,
18.2083368446371));
#35248=CARTESIAN_POINT('Origin',(0.,0.,-2.20833684463713));
#35249=CARTESIAN_POINT('',(5.07366101292862,-0.000128884195875409,16.2083368446371));
#35250=CARTESIAN_POINT('',(5.07342183474754,-0.000122761774360241,16.2916631553629));
#35251=CARTESIAN_POINT('',(5.0736,-1.85409460923845E-12,-2.20833684463713));
#35252=CARTESIAN_POINT('Ctrl Pts',(5.07342183474754,-0.000122761774360089,
16.2916631553629));
#35253=CARTESIAN_POINT('Ctrl Pts',(5.07288953552851,0.589818979702204,16.3101676916039));
#35254=CARTESIAN_POINT('Ctrl Pts',(4.82300217163475,2.02368301235074,16.3551295245292));
#35255=CARTESIAN_POINT('Ctrl Pts',(3.50037037246945,3.9646372600474,16.4265486541391));
#35256=CARTESIAN_POINT('Ctrl Pts',(1.17777659548083,5.15594643483254,16.5059205441925));
#35257=CARTESIAN_POINT('Ctrl Pts',(-1.43172095156687,5.09127847004474,16.5852924342459));
#35258=CARTESIAN_POINT('Ctrl Pts',(-3.69245444696213,3.78638634033038,16.6646643242993));
#35259=CARTESIAN_POINT('Ctrl Pts',(-5.05371420635461,1.5591388772047,16.7440362143527));
#35260=CARTESIAN_POINT('Ctrl Pts',(-5.18390038229795,-1.04791136166686,
16.8234081044061));
#35261=CARTESIAN_POINT('Ctrl Pts',(-4.05129987868913,-3.39969271923294,
16.9027799944595));
#35262=CARTESIAN_POINT('Ctrl Pts',(-1.93181173129365,-4.9233164424874,16.9821518845129));
#35263=CARTESIAN_POINT('Ctrl Pts',(0.658261551986501,-5.24763120247215,
17.0615237745663));
#35264=CARTESIAN_POINT('Ctrl Pts',(3.08798363825942,-4.29363457062506,17.1408956646198));
#35265=CARTESIAN_POINT('Ctrl Pts',(4.70928800664519,-2.36071043051411,17.2176087915519));
#35266=CARTESIAN_POINT('Ctrl Pts',(5.0733377557896,-0.758421261304332,17.2678646217997));
#35267=CARTESIAN_POINT('Ctrl Pts',(5.07392231800261,8.23068815519051E-5,
17.2916631553629));
#35268=CARTESIAN_POINT('Ctrl Pts',(5.07366101292862,-0.000128884195875374,
16.2083368446371));
#35269=CARTESIAN_POINT('Ctrl Pts',(5.07297133880781,0.668223813333716,16.2293037167406));
#35270=CARTESIAN_POINT('Ctrl Pts',(4.77257120255655,2.18054683036438,16.2767278855287));
#35271=CARTESIAN_POINT('Ctrl Pts',(3.31265234202039,4.12277525560071,16.3506093510011));
#35272=CARTESIAN_POINT('Ctrl Pts',(0.937286345425132,5.20503944789207,16.4299812410546));
#35273=CARTESIAN_POINT('Ctrl Pts',(-1.66640053022416,5.01936755177917,16.509353131108));
#35274=CARTESIAN_POINT('Ctrl Pts',(-3.86415592530783,3.6109888303424,16.5887250211614));
#35275=CARTESIAN_POINT('Ctrl Pts',(-5.12061148999576,1.32298122241861,16.6680969112148));
#35276=CARTESIAN_POINT('Ctrl Pts',(-5.1296974302943,-1.28730168253218,16.7474688012682));
#35277=CARTESIAN_POINT('Ctrl Pts',(-3.88920043041393,-3.58400074773889,
16.8268406913216));
#35278=CARTESIAN_POINT('Ctrl Pts',(-1.70130281532588,-5.00764516247516,
16.906212581375));
#35279=CARTESIAN_POINT('Ctrl Pts',(0.90102840177319,-5.21143830245825,16.9855844714284));
#35280=CARTESIAN_POINT('Ctrl Pts',(3.28387109087768,-4.1457366023928,17.0649563614818));
#35281=CARTESIAN_POINT('Ctrl Pts',(4.76464092528408,-2.20406061763576,17.1392071525514));
#35282=CARTESIAN_POINT('Ctrl Pts',(5.07300074510805,-0.679985153784537,
17.1870006469365));
#35283=CARTESIAN_POINT('Ctrl Pts',(5.07369825422177,0.000126003717071926,
17.2083368446371));
#35284=CARTESIAN_POINT('Origin',(0.,0.,-2.20833684463713));
#35285=CARTESIAN_POINT('',(5.07324617544329,7.96922658102828E-5,15.2083368446371));
#35286=CARTESIAN_POINT('',(5.07342714732068,0.00012340910666319,15.2916631553629));
#35287=CARTESIAN_POINT('',(5.0736,-1.85409460923845E-12,-2.20833684463713));
#35288=CARTESIAN_POINT('Ctrl Pts',(5.07342714732068,0.000123409106663336,
15.2916631553629));
#35289=CARTESIAN_POINT('Ctrl Pts',(5.07365576358557,0.251759202071401,15.2995561680391));
#35290=CARTESIAN_POINT('Ctrl Pts',(4.99363067660841,1.34673145111339,15.3339064773998));
#35291=CARTESIAN_POINT('Ctrl Pts',(4.21831964333036,3.19009729224721,15.3947140834449));
#35292=CARTESIAN_POINT('Ctrl Pts',(2.17873636962922,4.81913365439941,15.4740859734983));
#35293=CARTESIAN_POINT('Ctrl Pts',(-0.391582261162836,5.27423972531144,
15.5534578635517));
#35294=CARTESIAN_POINT('Ctrl Pts',(-2.86651231988745,4.44455267346898,15.6328297536051));
#35295=CARTESIAN_POINT('Ctrl Pts',(-4.64316632240643,2.53218242822043,15.7122016436585));
#35296=CARTESIAN_POINT('Ctrl Pts',(-5.28875528625864,0.00297814834715876,
15.7915735337119));
#35297=CARTESIAN_POINT('Ctrl Pts',(-4.64601516884489,-2.52695160186966,
15.8709454237653));
#35298=CARTESIAN_POINT('Ctrl Pts',(-2.87151604007055,-4.44132153518687,
15.9503173138187));
#35299=CARTESIAN_POINT('Ctrl Pts',(-0.397521959947054,-5.27379537322474,
16.0296892038721));
#35300=CARTESIAN_POINT('Ctrl Pts',(2.1733075897557,-4.82158433170501,16.1090610939255));
#35301=CARTESIAN_POINT('Ctrl Pts',(4.21472422106055,-3.1948460193553,16.1884329839789));
#35302=CARTESIAN_POINT('Ctrl Pts',(4.99287463290549,-1.35054413899492,16.2493003377914));
#35303=CARTESIAN_POINT('Ctrl Pts',(5.07365060287866,-0.253664125066255,
16.2837103949194));
#35304=CARTESIAN_POINT('Ctrl Pts',(5.07342183474754,-0.000122761774360089,
16.2916631553629));
#35305=CARTESIAN_POINT('Ctrl Pts',(5.07324617544329,7.96922658102828E-5,
15.2083368446371));
#35306=CARTESIAN_POINT('Ctrl Pts',(5.07343036424897,0.330250553788653,15.2186921931759));
#35307=CARTESIAN_POINT('Ctrl Pts',(4.96059306642381,1.5038639780885,15.2555048383992));
#35308=CARTESIAN_POINT('Ctrl Pts',(4.06576497321036,3.38238030533612,15.3187747803069));
#35309=CARTESIAN_POINT('Ctrl Pts',(1.95279534724736,4.91503119817963,15.3981466703603));
#35310=CARTESIAN_POINT('Ctrl Pts',(-0.635870902865948,5.2503913703836,15.4775185604137));
#35311=CARTESIAN_POINT('Ctrl Pts',(-3.06964040851742,4.30676782630626,15.5568904504671));
#35312=CARTESIAN_POINT('Ctrl Pts',(-4.75565230518791,2.31402517260967,15.6362623405205));
#35313=CARTESIAN_POINT('Ctrl Pts',(-5.28319782677237,-0.24240889112691,
15.7156342305739));
#35314=CARTESIAN_POINT('Ctrl Pts',(-4.52376805191524,-2.73979268554778,
15.7950061206273));
#35315=CARTESIAN_POINT('Ctrl Pts',(-2.66235839280204,-4.56976904619777,
15.8743780106807));
#35316=CARTESIAN_POINT('Ctrl Pts',(-0.15240412223312,-5.28655978220556,
15.9537499007341));
#35317=CARTESIAN_POINT('Ctrl Pts',(2.39467545517194,-4.71555625687092,16.0331217907875));
#35318=CARTESIAN_POINT('Ctrl Pts',(4.35841739221953,-2.99585366506689,16.112493680841));
#35319=CARTESIAN_POINT('Ctrl Pts',(5.02217539318898,-1.19342375387563,16.1708986987908));
#35320=CARTESIAN_POINT('Ctrl Pts',(5.0738416122916,-0.175144979162809,16.2028464200562));
#35321=CARTESIAN_POINT('Ctrl Pts',(5.07366101292862,-0.000128884195875374,
16.2083368446371));
#35322=CARTESIAN_POINT('Origin',(0.,0.,-2.20833684463713));
#35323=CARTESIAN_POINT('',(5.07403332299931,-8.66482790312043E-6,14.2083368446371));
#35324=CARTESIAN_POINT('',(5.07391786048903,-8.38031740753252E-5,14.2916631553629));
#35325=CARTESIAN_POINT('',(5.0736,-1.85409460923845E-12,-2.20833684463713));
#35326=CARTESIAN_POINT('Ctrl Pts',(5.07391786048903,-8.38031740754523E-5,
14.2916631553629));
#35327=CARTESIAN_POINT('Ctrl Pts',(5.07332646114364,0.756517455027875,14.3154019411588));
#35328=CARTESIAN_POINT('Ctrl Pts',(4.7106825315255,2.35691208085668,14.3655980236392));
#35329=CARTESIAN_POINT('Ctrl Pts',(3.09281731455568,4.29015412381589,14.442251402804));
#35330=CARTESIAN_POINT('Ctrl Pts',(0.664171081076821,5.24688651700904,14.5216232928574));
#35331=CARTESIAN_POINT('Ctrl Pts',(-1.92626575763464,4.9254889684451,14.6009951829108));
#35332=CARTESIAN_POINT('Ctrl Pts',(-4.04746852150321,3.4042532095528,14.6803670729642));
#35333=CARTESIAN_POINT('Ctrl Pts',(-5.1827169124532,1.05374890400015,14.7597389630177));
#35334=CARTESIAN_POINT('Ctrl Pts',(-5.05546693527891,-1.55344630213332,
14.839110853071));
#35335=CARTESIAN_POINT('Ctrl Pts',(-3.69671640275692,-3.78222542756219,
14.9184827431245));
#35336=CARTESIAN_POINT('Ctrl Pts',(-1.43745393706629,-5.08966281065088,
14.9978546331779));
#35337=CARTESIAN_POINT('Ctrl Pts',(1.17196912594334,-5.15726959884254,15.0772265232312));
#35338=CARTESIAN_POINT('Ctrl Pts',(3.49590310398282,-3.96857692817882,15.1565984132847));
#35339=CARTESIAN_POINT('Ctrl Pts',(4.82182831793198,-2.02749096887971,15.2280772906619));
#35340=CARTESIAN_POINT('Ctrl Pts',(5.07288944423512,-0.591721367900843,
15.2730988713546));
#35341=CARTESIAN_POINT('Ctrl Pts',(5.07342714732068,0.000123409106663336,
15.2916631553629));
#35342=CARTESIAN_POINT('Ctrl Pts',(5.07403332299931,-8.66482790325162E-6,
14.2083368446371));
#35343=CARTESIAN_POINT('Ctrl Pts',(5.07395003551347,0.835016825572543,14.2345379662956));
#35344=CARTESIAN_POINT('Ctrl Pts',(4.65105118571099,2.51331333377907,14.2871963846386));
#35345=CARTESIAN_POINT('Ctrl Pts',(2.89043509646017,4.42903220810837,14.3663120996661));
#35346=CARTESIAN_POINT('Ctrl Pts',(0.420014577610126,5.27205169757513,14.4456839897195));
#35347=CARTESIAN_POINT('Ctrl Pts',(-2.15272056265924,4.83081106300113,14.5250558797729));
#35348=CARTESIAN_POINT('Ctrl Pts',(-4.201057738831,3.21279554629894,14.6044277698263));
#35349=CARTESIAN_POINT('Ctrl Pts',(-5.22602654870706,0.81215014592063,14.6837996598797));
#35350=CARTESIAN_POINT('Ctrl Pts',(-4.97794685893165,-1.78633323234006,
14.7631715499331));
#35351=CARTESIAN_POINT('Ctrl Pts',(-3.51725033281897,-3.94966978918425,
14.8425434399865));
#35352=CARTESIAN_POINT('Ctrl Pts',(-1.19975941093315,-5.15087552782897,
14.9219153300399));
#35353=CARTESIAN_POINT('Ctrl Pts',(1.40999024783357,-5.09733938916413,15.0012872200933));
#35354=CARTESIAN_POINT('Ctrl Pts',(3.67626940318851,-3.8021026580683,15.0806591101467));
#35355=CARTESIAN_POINT('Ctrl Pts',(4.86818118380815,-1.87050241988135,15.1496756516613));
#35356=CARTESIAN_POINT('Ctrl Pts',(5.07295977285751,-0.513316266501481,
15.1922348964914));
#35357=CARTESIAN_POINT('Ctrl Pts',(5.07324617544329,7.96922658102828E-5,
15.2083368446371));
#35358=CARTESIAN_POINT('Origin',(0.,0.,-2.20833684463713));
#35359=CARTESIAN_POINT('',(5.07322036085286,-6.69861637152269E-5,13.2083368446371));
#35360=CARTESIAN_POINT('',(5.07316540514723,3.01288341894208E-6,13.2916631553629));
#35361=CARTESIAN_POINT('',(5.0736,-1.85409460923845E-12,-2.20833684463713));
#35362=CARTESIAN_POINT('Ctrl Pts',(5.07316545149283,3.01256212205392E-6,
13.2916631553629));
#35363=CARTESIAN_POINT('Ctrl Pts',(5.07317410528241,0.418572877762161,13.3047904175941));
#35364=CARTESIAN_POINT('Ctrl Pts',(4.91873112752187,1.68074170142874,13.3443749765097));
#35365=CARTESIAN_POINT('Ctrl Pts',(3.8835697329937,3.59010131838716,13.4104168321098));
#35366=CARTESIAN_POINT('Ctrl Pts',(1.69344007832116,5.01030957610862,13.4897887221632));
#35367=CARTESIAN_POINT('Ctrl Pts',(-0.909207831064397,5.21001751122212,
13.5691606122166));
#35368=CARTESIAN_POINT('Ctrl Pts',(-3.29037472530003,4.14057671278008,13.64853250227));
#35369=CARTESIAN_POINT('Ctrl Pts',(-4.87001361957351,2.06250059211591,13.7279043923234));
#35370=CARTESIAN_POINT('Ctrl Pts',(-5.26332797571119,-0.517996107520081,
13.8072762823768));
#35371=CARTESIAN_POINT('Ctrl Pts',(-4.37450728714447,-2.97231010192914,
13.8866481724302));
#35372=CARTESIAN_POINT('Ctrl Pts',(-2.420066306237,-4.70257593460501,13.9660200624836));
#35373=CARTESIAN_POINT('Ctrl Pts',(0.123897470143854,-5.28730467858643,
14.045391952537));
#35374=CARTESIAN_POINT('Ctrl Pts',(2.63768009704007,-4.58405770611459,14.1247638425904));
#35375=CARTESIAN_POINT('Ctrl Pts',(4.50892969070322,-2.76414442307289,14.2041357326438));
#35376=CARTESIAN_POINT('Ctrl Pts',(5.05065740926092,-1.01658127603429,14.2597688369013));
#35377=CARTESIAN_POINT('Ctrl Pts',(5.07398558617533,-0.0867280307438605,
14.2889446444744));
#35378=CARTESIAN_POINT('Ctrl Pts',(5.07391786048903,-8.38031740754523E-5,
14.2916631553629));
#35379=CARTESIAN_POINT('Ctrl Pts',(5.07322036085286,-6.69861637153657E-5,
13.2083368446371));
#35380=CARTESIAN_POINT('Ctrl Pts',(5.07298878663719,0.497000397927876,13.2239264427309));
#35381=CARTESIAN_POINT('Ctrl Pts',(4.87730902789417,1.83782529464356,13.2659733375091));
#35382=CARTESIAN_POINT('Ctrl Pts',(3.71281646953824,3.76642207019282,13.3344775289718));
#35383=CARTESIAN_POINT('Ctrl Pts',(1.45915164597774,5.08348481077208,13.4138494190252));
#35384=CARTESIAN_POINT('Ctrl Pts',(-1.14995928876559,5.16222190355004,13.4932213090786));
#35385=CARTESIAN_POINT('Ctrl Pts',(-3.47894268615732,3.98345316700755,13.572593199132));
#35386=CARTESIAN_POINT('Ctrl Pts',(-4.96046334571011,1.83432405620607,13.6519650891854));
#35387=CARTESIAN_POINT('Ctrl Pts',(-5.23362611404733,-0.761642334479749,
13.7313369792388));
#35388=CARTESIAN_POINT('Ctrl Pts',(-4.23188914543755,-3.17207433835303,
13.8107088692922));
#35389=CARTESIAN_POINT('Ctrl Pts',(-2.19927334812693,-4.80979605467098,
13.8900807593456));
#35390=CARTESIAN_POINT('Ctrl Pts',(0.369080568778457,-5.27586209837409,
13.9694526493991));
#35391=CARTESIAN_POINT('Ctrl Pts',(2.84752727607539,-4.45673981283591,14.0488245394524));
#35392=CARTESIAN_POINT('Ctrl Pts',(4.63232264181505,-2.55196557371717,14.1281964295059));
#35393=CARTESIAN_POINT('Ctrl Pts',(5.07202231626624,-0.859526521495883,
14.1813671979007));
#35394=CARTESIAN_POINT('Ctrl Pts',(5.07403413732223,-0.00817292128436273,
14.2080806696111));
#35395=CARTESIAN_POINT('Ctrl Pts',(5.07403332299931,-8.66482790325162E-6,
14.2083368446371));
#35396=CARTESIAN_POINT('Origin',(0.,0.,-2.20833684463713));
#35397=CARTESIAN_POINT('',(5.07371259150425,0.000124614973235349,12.2083368446371));
#35398=CARTESIAN_POINT('',(5.07393295843892,7.85666071205126E-5,12.2916631553629));
#35399=CARTESIAN_POINT('',(5.0736,-1.85409460923845E-12,-2.20833684463713));
#35400=CARTESIAN_POINT('Ctrl Pts',(5.07393295843892,7.85666071204203E-5,
12.2916631553629));
#35401=CARTESIAN_POINT('Ctrl Pts',(5.07399255467328,0.080259357669063,12.2941788940293));
#35402=CARTESIAN_POINT('Ctrl Pts',(5.0525559141232,1.00364648464526,12.3231519293802));
#35403=CARTESIAN_POINT('Ctrl Pts',(4.51946174941847,2.74689039512926,12.3785822614155));
#35404=CARTESIAN_POINT('Ctrl Pts',(2.6551818185972,4.57394259446934,12.4579541514689));
#35405=CARTESIAN_POINT('Ctrl Pts',(0.144105473910954,5.28679250204684,12.5373260415223));
#35406=CARTESIAN_POINT('Ctrl Pts',(-2.40207464524796,4.7117914582425,12.6166979315757));
#35407=CARTESIAN_POINT('Ctrl Pts',(-4.36311469772651,2.98900844458373,12.6960698216291));
#35408=CARTESIAN_POINT('Ctrl Pts',(-5.26130966742946,0.538109589882336,
12.7754417116825));
#35409=CARTESIAN_POINT('Ctrl Pts',(-4.87786124785798,-2.043871569829,12.854813601736));
#35410=CARTESIAN_POINT('Ctrl Pts',(-3.30617662527107,-4.12797013916298,
12.9341854917893));
#35411=CARTESIAN_POINT('Ctrl Pts',(-0.929114694865931,-5.20650431970379,
13.0135573818428));
#35412=CARTESIAN_POINT('Ctrl Pts',(1.67427751864803,-5.01674557236658,13.0929292718962));
#35413=CARTESIAN_POINT('Ctrl Pts',(3.86981943456978,-3.60491870797887,13.1723011619496));
#35414=CARTESIAN_POINT('Ctrl Pts',(4.91547184132152,-1.69367935817457,13.2385457897718));
#35415=CARTESIAN_POINT('Ctrl Pts',(5.07315666403118,-0.425032354751582,
13.2783331209096));
#35416=CARTESIAN_POINT('Ctrl Pts',(5.07316545149283,3.01256212205392E-6,
13.2916631553629));
#35417=CARTESIAN_POINT('Ctrl Pts',(5.07371259150425,0.000124614973235296,
12.2083368446371));
#35418=CARTESIAN_POINT('Ctrl Pts',(5.07387461653381,0.158804080659856,12.2133149191661));
#35419=CARTESIAN_POINT('Ctrl Pts',(5.02779682862049,1.1607339041827,12.2447502903796));
#35420=CARTESIAN_POINT('Ctrl Pts',(4.38714636147788,2.95362288559007,12.3026429582776));
#35421=CARTESIAN_POINT('Ctrl Pts',(2.44010389315499,4.69220996311119,12.382014848331));
#35422=CARTESIAN_POINT('Ctrl Pts',(-0.101342482462103,5.28778507964898,
12.4613867383844));
#35423=CARTESIAN_POINT('Ctrl Pts',(-2.61810205366918,4.59526745509803,12.5407586284378));
#35424=CARTESIAN_POINT('Ctrl Pts',(-4.49709775967304,2.78335284993721,12.6201305184912));
#35425=CARTESIAN_POINT('Ctrl Pts',(-5.28061040557763,0.293419651378745,
12.6995024085446));
#35426=CARTESIAN_POINT('Ctrl Pts',(-4.7777780451164,-2.26798992478223,12.778874298598));
#35427=CARTESIAN_POINT('Ctrl Pts',(-3.11108952829712,-4.27692217537683,
12.8582461886514));
#35428=CARTESIAN_POINT('Ctrl Pts',(-0.686546488664521,-5.24400565085626,
12.9376180787048));
#35429=CARTESIAN_POINT('Ctrl Pts',(1.90523775596186,-4.93366095719673,13.0169899687582));
#35430=CARTESIAN_POINT('Ctrl Pts',(4.03291030040817,-3.42148737483739,13.0963618588116));
#35431=CARTESIAN_POINT('Ctrl Pts',(4.95323103438167,-1.53655914035534,13.1601441507712));
#35432=CARTESIAN_POINT('Ctrl Pts',(5.07338179405736,-0.346578710011678,
13.1974691460464));
#35433=CARTESIAN_POINT('Ctrl Pts',(5.07322036085286,-6.69861637153657E-5,
13.2083368446371));
#35434=CARTESIAN_POINT('Origin',(0.,0.,-2.20833684463713));
#35435=CARTESIAN_POINT('',(5.0736465461671,-0.000129729951178492,11.2083368446371));
#35436=CARTESIAN_POINT('',(5.07340926806867,-0.000121118768615341,11.2916631553629));
#35437=CARTESIAN_POINT('',(5.0736,-1.85409460923845E-12,-2.20833684463713));
#35438=CARTESIAN_POINT('Ctrl Pts',(5.07340926806867,-0.000121118768615022,
11.2916631553629));
#35439=CARTESIAN_POINT('Ctrl Pts',(5.07289012258619,0.585265031435054,11.310024667149));
#35440=CARTESIAN_POINT('Ctrl Pts',(4.82580215794652,2.01456720880964,11.3548434756196));
#35441=CARTESIAN_POINT('Ctrl Pts',(3.51104609249152,3.95518604919035,11.4261195807747));
#35442=CARTESIAN_POINT('Ctrl Pts',(1.19167245960881,5.152752477688,11.5054914708281));
#35443=CARTESIAN_POINT('Ctrl Pts',(-1.41798994671238,5.09511980804502,11.5848633608815));
#35444=CARTESIAN_POINT('Ctrl Pts',(-3.68223314068194,3.79632723101863,11.6642352509349));
#35445=CARTESIAN_POINT('Ctrl Pts',(-5.04949249206616,1.57275774354392,11.7436071409883));
#35446=CARTESIAN_POINT('Ctrl Pts',(-5.18670664924514,-1.03393204901786,
11.8229790310417));
#35447=CARTESIAN_POINT('Ctrl Pts',(-4.06045054724843,-3.38875828300867,
11.9023509210951));
#35448=CARTESIAN_POINT('Ctrl Pts',(-1.94507767959685,-4.91809050014781,
11.9817228111485));
#35449=CARTESIAN_POINT('Ctrl Pts',(0.644111805448097,-5.24938675745961,
12.0610947012019));
#35450=CARTESIAN_POINT('Ctrl Pts',(3.0763970804032,-4.30194401997477,12.1404665912553));
#35451=CARTESIAN_POINT('Ctrl Pts',(4.70593891054333,-2.36980219715329,12.2173227426423));
#35452=CARTESIAN_POINT('Ctrl Pts',(5.07336579829568,-0.762978855367823,
12.2677215973449));
#35453=CARTESIAN_POINT('Ctrl Pts',(5.07393295843892,7.85666071204203E-5,
12.2916631553629));
#35454=CARTESIAN_POINT('Ctrl Pts',(5.0736465461671,-0.000129729951178388,
11.2083368446371));
#35455=CARTESIAN_POINT('Ctrl Pts',(5.07296127147132,0.663669285094766,11.2291606922858));
#35456=CARTESIAN_POINT('Ctrl Pts',(4.77561643393883,2.17143981582611,11.276441836619));
#35457=CARTESIAN_POINT('Ctrl Pts',(3.32375507563458,4.11382954733217,11.3501802776367));
#35458=CARTESIAN_POINT('Ctrl Pts',(0.951315435152466,5.20249366075065,11.4295521676901));
#35459=CARTESIAN_POINT('Ctrl Pts',(-1.6528625396318,5.02384183393465,11.5089240577436));
#35460=CARTESIAN_POINT('Ctrl Pts',(-3.85440685831092,3.62139325645746,11.5882959477969));
#35461=CARTESIAN_POINT('Ctrl Pts',(-5.11702619789041,1.33678129752526,11.6676678378503));
#35462=CARTESIAN_POINT('Ctrl Pts',(-5.13314928200913,-1.27346762656892,
11.7470397279037));
#35463=CARTESIAN_POINT('Ctrl Pts',(-3.89884856306365,-3.57350265560368,
11.8264116179572));
#35464=CARTESIAN_POINT('Ctrl Pts',(-1.71479696411077,-5.00304034754732,
11.9057835080105));
#35465=CARTESIAN_POINT('Ctrl Pts',(0.886975379660772,-5.21384848487043,
11.985155398064));
#35466=CARTESIAN_POINT('Ctrl Pts',(3.27268248423369,-4.15457467193696,12.0645272881174));
#35467=CARTESIAN_POINT('Ctrl Pts',(4.76154396611873,-2.21316538967253,12.1389211036417));
#35468=CARTESIAN_POINT('Ctrl Pts',(5.0730134915642,-0.684540002865494,12.1868576224816));
#35469=CARTESIAN_POINT('Ctrl Pts',(5.07371259150425,0.000124614973235296,
12.2083368446371));
#35470=CARTESIAN_POINT('Origin',(0.,0.,-2.20833684463713));
#35471=CARTESIAN_POINT('',(5.07325419654647,8.30592867887003E-5,10.2083368446371));
#35472=CARTESIAN_POINT('',(5.07344000894767,0.000124864012350097,10.2916631553629));
#35473=CARTESIAN_POINT('',(5.0736,-1.85409460923845E-12,-2.20833684463713));
#35474=CARTESIAN_POINT('Ctrl Pts',(5.07344000894767,0.000124864012350061,
10.2916631553629));
#35475=CARTESIAN_POINT('Ctrl Pts',(5.07366802985413,0.247199120889535,10.2994131435843));
#35476=CARTESIAN_POINT('Ctrl Pts',(4.99543134296861,1.33760465491503,10.3336204284901));
#35477=CARTESIAN_POINT('Ctrl Pts',(4.22690463795744,3.1787133448809,10.3942850100804));
#35478=CARTESIAN_POINT('Ctrl Pts',(2.1917205673539,4.81324238969408,10.4736569001339));
#35479=CARTESIAN_POINT('Ctrl Pts',(-0.377361782165876,5.27527624230907,
10.5530287901872));
#35480=CARTESIAN_POINT('Ctrl Pts',(-2.85451963682615,4.45226447892349,10.6324006802407));
#35481=CARTESIAN_POINT('Ctrl Pts',(-4.63632282632763,2.54469094339242,10.711772570294));
#35482=CARTESIAN_POINT('Ctrl Pts',(-5.28872803766221,0.0172363266288179,
10.7911444603475));
#35483=CARTESIAN_POINT('Ctrl Pts',(-4.65281080542322,-2.5144170211496,10.8705163504009));
#35484=CARTESIAN_POINT('Ctrl Pts',(-2.88347915980519,-4.43356394814365,
10.9498882404543));
#35485=CARTESIAN_POINT('Ctrl Pts',(-0.411738373331464,-5.27270451089727,
11.0292601305077));
#35486=CARTESIAN_POINT('Ctrl Pts',(2.16030096951836,-4.82742592572977,11.1086320205611));
#35487=CARTESIAN_POINT('Ctrl Pts',(4.20609577793862,-3.20619707038057,11.1880039106145));
#35488=CARTESIAN_POINT('Ctrl Pts',(4.99105565025759,-1.3596709971465,11.2490142888818));
#35489=CARTESIAN_POINT('Ctrl Pts',(5.07363816480692,-0.25822406855438,11.2835673704646));
#35490=CARTESIAN_POINT('Ctrl Pts',(5.07340926806867,-0.000121118768615022,
11.2916631553629));
#35491=CARTESIAN_POINT('Ctrl Pts',(5.07325419654647,8.30592867889779E-5,
10.2083368446371));
#35492=CARTESIAN_POINT('Ctrl Pts',(5.07344390313192,0.32569224224827,10.2185491687211));
#35493=CARTESIAN_POINT('Ctrl Pts',(4.96261803044706,1.49473693663548,10.2552187894896));
#35494=CARTESIAN_POINT('Ctrl Pts',(4.07486890650351,3.37140693807807,10.3183457069425));
#35495=CARTESIAN_POINT('Ctrl Pts',(1.96603890048266,4.90974870936374,10.3977175969959));
#35496=CARTESIAN_POINT('Ctrl Pts',(-0.621713829942471,5.25208656259283,
10.4770894870493));
#35497=CARTESIAN_POINT('Ctrl Pts',(-3.05801844753381,4.31502775447074,10.5564613771027));
#35498=CARTESIAN_POINT('Ctrl Pts',(-4.74939654011498,2.32683773651149,10.6358332671561));
#35499=CARTESIAN_POINT('Ctrl Pts',(-5.28383214813503,-0.228164803694007,
10.7152051572095));
#35500=CARTESIAN_POINT('Ctrl Pts',(-4.53113794043347,-2.72758690275384,
10.7945770472629));
#35501=CARTESIAN_POINT('Ctrl Pts',(-2.67466855994604,-4.56257486971405,
10.8739489373163));
#35502=CARTESIAN_POINT('Ctrl Pts',(-0.166655838534166,-5.2861296975001,
10.9533208273697));
#35503=CARTESIAN_POINT('Ctrl Pts',(2.38195387625819,-4.72199503162473,11.0326927174231));
#35504=CARTESIAN_POINT('Ctrl Pts',(4.3503248991595,-3.00759282800428,11.1120646074765));
#35505=CARTESIAN_POINT('Ctrl Pts',(5.02057706818124,-1.20254945990408,11.1706126498812));
#35506=CARTESIAN_POINT('Ctrl Pts',(5.07383193265951,-0.17970643375256,11.2027033956014));
#35507=CARTESIAN_POINT('Ctrl Pts',(5.0736465461671,-0.000129729951178388,
11.2083368446371));
#35508=CARTESIAN_POINT('Origin',(0.,0.,-2.20833684463713));
#35509=CARTESIAN_POINT('',(5.07403156349013,-1.34850231131101E-5,9.20833684463708));
#35510=CARTESIAN_POINT('',(5.07390676572803,-8.73588085612467E-5,9.29166315536294));
#35511=CARTESIAN_POINT('',(5.0736,-1.85409460923845E-12,-2.20833684463713));
#35512=CARTESIAN_POINT('Ctrl Pts',(5.07390676572803,-8.73588085611478E-5,
9.29166315536294));
#35513=CARTESIAN_POINT('Ctrl Pts',(5.07329990983557,0.75196019632477,9.31525891670402));
#35514=CARTESIAN_POINT('Ctrl Pts',(4.71401054212216,2.34781906214645,9.36531197472956));
#35515=CARTESIAN_POINT('Ctrl Pts',(3.10437209115777,4.28180047024037,9.44182232943961));
#35516=CARTESIAN_POINT('Ctrl Pts',(0.67831398067512,5.24507688131743,9.52119421949299));
#35517=CARTESIAN_POINT('Ctrl Pts',(-1.91297991407746,4.93066417388633,9.6005661095464));
#35518=CARTESIAN_POINT('Ctrl Pts',(-4.03827613607002,3.41515258753654,9.6799379995998));
#35519=CARTESIAN_POINT('Ctrl Pts',(-5.1798572298885,1.06771739017486,9.75930988965322));
#35520=CARTESIAN_POINT('Ctrl Pts',(-5.05963656792565,-1.53981140008104,
9.8386817797066));
#35521=CARTESIAN_POINT('Ctrl Pts',(-3.70689963733171,-3.77224554159189,
9.91805366976003));
#35522=CARTESIAN_POINT('Ctrl Pts',(-1.45117016016697,-5.08576901889487,
9.99742555981341));
#35523=CARTESIAN_POINT('Ctrl Pts',(1.1580611559038,-5.16041042035386,10.0767974498668));
#35524=CARTESIAN_POINT('Ctrl Pts',(3.48519133772131,-3.97798726578937,10.1561693399202));
#35525=CARTESIAN_POINT('Ctrl Pts',(4.81900834166099,-2.03660616436304,10.2277912417523));
#35526=CARTESIAN_POINT('Ctrl Pts',(5.07288960070042,-0.596275311661321,
10.2729558468998));
#35527=CARTESIAN_POINT('Ctrl Pts',(5.07344000894767,0.000124864012350061,
10.2916631553629));
#35528=CARTESIAN_POINT('Ctrl Pts',(5.07403156349013,-1.34850231132098E-5,
9.20833684463708));
#35529=CARTESIAN_POINT('Ctrl Pts',(5.07390455498411,0.830454679150979,9.2343949418408));
#35530=CARTESIAN_POINT('Ctrl Pts',(4.65463656321598,2.50423700786744,9.28691033572898));
#35531=CARTESIAN_POINT('Ctrl Pts',(2.90236501609723,4.42122366100663,9.36588302630163));
#35532=CARTESIAN_POINT('Ctrl Pts',(0.434226208411351,5.27090020273944,9.44525491635504));
#35533=CARTESIAN_POINT('Ctrl Pts',(-2.13968914250016,4.83659712202464,9.52462680640844));
#35534=CARTESIAN_POINT('Ctrl Pts',(-4.1923809544202,3.22410968801074,9.60399869646184));
#35535=CARTESIAN_POINT('Ctrl Pts',(-5.22381804552131,0.826236270443201,
9.68337058651526));
#35536=CARTESIAN_POINT('Ctrl Pts',(-4.98274462345855,-1.77290647376134,
9.76274247656865));
#35537=CARTESIAN_POINT('Ctrl Pts',(-3.52788564023945,-3.94017312521954,
9.84211436662205));
#35538=CARTESIAN_POINT('Ctrl Pts',(-1.21364152390043,-5.14762232479954,
9.92148625667546));
#35539=CARTESIAN_POINT('Ctrl Pts',(1.39624298131078,-5.10112212012714,10.0008581467289));
#35540=CARTESIAN_POINT('Ctrl Pts',(3.66600578680612,-3.81199985813406,10.0802300367823));
#35541=CARTESIAN_POINT('Ctrl Pts',(4.86560152926764,-1.87962374426628,10.1493896027517));
#35542=CARTESIAN_POINT('Ctrl Pts',(5.07295242603298,-0.517870759272535,
10.1920918720366));
#35543=CARTESIAN_POINT('Ctrl Pts',(5.07325419654647,8.30592867889779E-5,
10.2083368446371));
#35544=CARTESIAN_POINT('Origin',(0.,0.,-2.20833684463713));
#35545=CARTESIAN_POINT('',(5.07321399251666,-6.32753131005193E-5,8.20833684463707));
#35546=CARTESIAN_POINT('',(5.07316567838514,7.26391603613751E-6,8.29166315536292));
#35547=CARTESIAN_POINT('',(5.0736,-1.85409460923845E-12,-2.20833684463713));
#35548=CARTESIAN_POINT('Ctrl Pts',(5.07316594763625,7.25941288019782E-6,
8.29166315536292));
#35549=CARTESIAN_POINT('Ctrl Pts',(5.07318657601694,0.414016596607197,8.30464739313926));
#35550=CARTESIAN_POINT('Ctrl Pts',(4.92101378278626,1.67161602862595,8.34408892760008));
#35551=CARTESIAN_POINT('Ctrl Pts',(3.89323433265495,3.57961838445758,8.40998775874535));
#35552=CARTESIAN_POINT('Ctrl Pts',(1.70694143925982,5.00572594837628,8.48935964879875));
#35553=CARTESIAN_POINT('Ctrl Pts',(-0.895158610488236,5.21244975125697,
8.56873153885215));
#35554=CARTESIAN_POINT('Ctrl Pts',(-3.27920000412133,4.14943233229326,8.64810342890557));
#35555=CARTESIAN_POINT('Ctrl Pts',(-4.86443553513654,2.0756223817956,8.72747531895896));
#35556=CARTESIAN_POINT('Ctrl Pts',(-5.26470533703792,-0.503804586595236,
8.80684720901237));
#35557=CARTESIAN_POINT('Ctrl Pts',(-4.38250457206448,-2.96050587284403,
8.88621909906576));
#35558=CARTESIAN_POINT('Ctrl Pts',(-2.43273539384546,-4.69603448143659,
8.96559098911917));
#35559=CARTESIAN_POINT('Ctrl Pts',(0.109642741545844,-5.28761948484726,
9.04496287917257));
#35560=CARTESIAN_POINT('Ctrl Pts',(2.62531214778668,-4.59115208569632,9.12433476922599));
#35561=CARTESIAN_POINT('Ctrl Pts',(4.50146132585655,-2.77629020081255,9.20370665927937));
#35562=CARTESIAN_POINT('Ctrl Pts',(5.04930321710503,-1.02570491769659,9.25948278799171));
#35563=CARTESIAN_POINT('Ctrl Pts',(5.07398036113186,-0.0912906316256552,
9.28880162001956));
#35564=CARTESIAN_POINT('Ctrl Pts',(5.07390676572803,-8.73588085611478E-5,
9.29166315536294));
#35565=CARTESIAN_POINT('Ctrl Pts',(5.07321399251666,-6.32753131006233E-5,
8.20833684463707));
#35566=CARTESIAN_POINT('Ctrl Pts',(5.07299759473682,0.492445607247212,8.22378341827604));
#35567=CARTESIAN_POINT('Ctrl Pts',(4.87982559067105,1.82870276667211,8.26568728859948));
#35568=CARTESIAN_POINT('Ctrl Pts',(3.72295704063487,3.75639883677136,8.33404845560738));
#35569=CARTESIAN_POINT('Ctrl Pts',(1.47285113468463,5.07953254565499,8.41342034566079));
#35570=CARTESIAN_POINT('Ctrl Pts',(-1.1360380475741,5.16530336977162,8.49279223571419));
#35571=CARTESIAN_POINT('Ctrl Pts',(-3.46819087602133,3.99281772621695,8.57216412576759));
#35572=CARTESIAN_POINT('Ctrl Pts',(-4.95550008378004,1.84769052250801,8.651536015821));
#35573=CARTESIAN_POINT('Ctrl Pts',(-5.23566043994335,-0.74753000269027,
8.7309079058744));
#35574=CARTESIAN_POINT('Ctrl Pts',(-4.24042550187429,-3.16065387386283,
8.81027979592781));
#35575=CARTESIAN_POINT('Ctrl Pts',(-2.21223229757129,-4.8038494573511,8.88965168598121));
#35576=CARTESIAN_POINT('Ctrl Pts',(0.354855797726969,-5.27683794616905,
8.96902357603462));
#35577=CARTESIAN_POINT('Ctrl Pts',(2.83550180615889,-4.46440039138287,9.04839546608801));
#35578=CARTESIAN_POINT('Ctrl Pts',(4.6254258508873,-2.56444478303851,9.12776735614143));
#35579=CARTESIAN_POINT('Ctrl Pts',(5.0708816691802,-0.868647987514843,9.18108114899111));
#35580=CARTESIAN_POINT('Ctrl Pts',(5.07403350920893,-0.0127359204844534,
9.20793764515633));
#35581=CARTESIAN_POINT('Ctrl Pts',(5.07403156349013,-1.34850231132098E-5,
9.20833684463708));
#35582=CARTESIAN_POINT('Origin',(0.,0.,-2.20833684463713));
#35583=CARTESIAN_POINT('',(5.0737268532953,0.000123079057421927,7.20833684463709));
#35584=CARTESIAN_POINT('',(5.07394313380083,7.47405269748897E-5,7.29166315536293));
#35585=CARTESIAN_POINT('',(5.0736,-1.85409460923845E-12,-2.20833684463713));
#35586=CARTESIAN_POINT('Ctrl Pts',(5.07394313380082,7.47405269749084E-5,
7.29166315536293));
#35587=CARTESIAN_POINT('Ctrl Pts',(5.07399715749136,0.0756966636928046,
7.29403586957452));
#35588=CARTESIAN_POINT('Ctrl Pts',(5.05387993962774,0.994523136339973,7.32286588047058));
#35589=CARTESIAN_POINT('Ctrl Pts',(4.52685078861501,2.73469619609302,7.37815318805109));
#35590=CARTESIAN_POINT('Ctrl Pts',(2.66750326347436,4.56676775046241,7.45752507810451));
#35591=CARTESIAN_POINT('Ctrl Pts',(0.158357847769689,5.28638478918814,7.5368969681579));
#35592=CARTESIAN_POINT('Ctrl Pts',(-2.38936318913255,4.71825019448189,7.61626885821132));
#35593=CARTESIAN_POINT('Ctrl Pts',(-4.3550406419278,3.0007602960695,7.69564074826471));
#35594=CARTESIAN_POINT('Ctrl Pts',(-5.25983983406839,0.552291831604834,
7.77501263831812));
#35595=CARTESIAN_POINT('Ctrl Pts',(-4.88335368508791,-2.03071370056153,
7.85438452837152));
#35596=CARTESIAN_POINT('Ctrl Pts',(-3.31729338754006,-4.11904187017964,
7.93375641842492));
#35597=CARTESIAN_POINT('Ctrl Pts',(-0.943147763491834,-5.20398055756651,
8.01312830847834));
#35598=CARTESIAN_POINT('Ctrl Pts',(1.66074656812082,-5.02124109994579,8.09250019853171));
#35599=CARTESIAN_POINT('Ctrl Pts',(3.86008671173945,-3.61533842470695,8.17187208858515));
#35600=CARTESIAN_POINT('Ctrl Pts',(4.91315662948087,-1.70280471015196,8.23825974086219));
#35601=CARTESIAN_POINT('Ctrl Pts',(5.07314454265331,-0.429588399925582,
8.27819009645479));
#35602=CARTESIAN_POINT('Ctrl Pts',(5.07316594763625,7.25941288019782E-6,
8.29166315536292));
#35603=CARTESIAN_POINT('Ctrl Pts',(5.0737268532953,0.000123079057421736,
7.20833684463709));
#35604=CARTESIAN_POINT('Ctrl Pts',(5.07388334783635,0.154242294956097,7.2131718947113));
#35605=CARTESIAN_POINT('Ctrl Pts',(5.02933704432274,1.15160862859258,7.24446424146999));
#35606=CARTESIAN_POINT('Ctrl Pts',(4.39509322077433,2.9417846501764,7.30221388491313));
#35607=CARTESIAN_POINT('Ctrl Pts',(2.45274496186498,4.68561452739722,7.38158577496654));
#35608=CARTESIAN_POINT('Ctrl Pts',(-0.0870865406957981,5.28803907717593,
7.46095766501995));
#35609=CARTESIAN_POINT('Ctrl Pts',(-2.60570395470586,4.60230901263053,7.54032955507335));
#35610=CARTESIAN_POINT('Ctrl Pts',(-4.48957765297745,2.79546665964655,7.61970144512676));
#35611=CARTESIAN_POINT('Ctrl Pts',(-5.27980017249532,0.307654816033177,
7.69907333518014));
#35612=CARTESIAN_POINT('Ctrl Pts',(-4.78387505663278,-2.25510105978351,
7.77844522523357));
#35613=CARTESIAN_POINT('Ctrl Pts',(-3.12260856590233,-4.26851930901846,
7.85781711528695));
#35614=CARTESIAN_POINT('Ctrl Pts',(-0.70068154029489,-5.24213570278374,
7.93718900534038));
#35615=CARTESIAN_POINT('Ctrl Pts',(1.8919299575961,-4.93877944262147,8.01656089539376));
#35616=CARTESIAN_POINT('Ctrl Pts',(4.02367150553262,-3.43234744203947,8.09593278544719));
#35617=CARTESIAN_POINT('Ctrl Pts',(4.95114565728143,-1.54568603506211,8.15985810186161));
#35618=CARTESIAN_POINT('Ctrl Pts',(5.07336824653293,-0.351136531432447,
8.19732612159157));
#35619=CARTESIAN_POINT('Ctrl Pts',(5.07321399251666,-6.32753131006233E-5,
8.20833684463707));
#35620=CARTESIAN_POINT('Origin',(0.,0.,-2.20833684463713));
#35621=CARTESIAN_POINT('',(5.07363207848188,-0.00013042437206158,6.20833684463708));
#35622=CARTESIAN_POINT('',(5.07339692231655,-0.000119345805453296,6.29166315536293));
#35623=CARTESIAN_POINT('',(5.0736,-1.85409460923845E-12,-2.20833684463713));
#35624=CARTESIAN_POINT('Ctrl Pts',(5.07339692231655,-0.000119345805453183,
6.29166315536293));
#35625=CARTESIAN_POINT('Ctrl Pts',(5.07289122007049,0.580711075066297,6.30988164269423));
#35626=CARTESIAN_POINT('Ctrl Pts',(4.82858806615863,2.00545098816607,6.35455742671001));
#35627=CARTESIAN_POINT('Ctrl Pts',(3.52169629398765,3.94570609146495,6.42569050741027));
#35628=CARTESIAN_POINT('Ctrl Pts',(1.20555966211655,5.14952106980711,6.50506239746365));
#35629=CARTESIAN_POINT('Ctrl Pts',(-1.40424863498509,5.09892411381582,6.58443428751707));
#35630=CARTESIAN_POINT('Ctrl Pts',(-3.67198507285601,3.80624052997609,6.66380617757046));
#35631=CARTESIAN_POINT('Ctrl Pts',(-5.04523407478029,1.58636517800468,6.74317806762388));
#35632=CARTESIAN_POINT('Ctrl Pts',(-5.1894752235243,-1.01994521996889,6.82254995767727));
#35633=CARTESIAN_POINT('Ctrl Pts',(-4.06957169452636,-3.37779921996849,
6.90192184773068));
#35634=CARTESIAN_POINT('Ctrl Pts',(-1.95832950858598,-4.91282880661553,
6.98129373778407));
#35635=CARTESIAN_POINT('Ctrl Pts',(0.629957410957137,-5.25110417033315,
7.06066562783749));
#35636=CARTESIAN_POINT('Ctrl Pts',(3.06478809957816,-4.31022218127953,7.14003751789089));
#35637=CARTESIAN_POINT('Ctrl Pts',(4.70257511155161,-2.37889312808664,7.2170366937327));
#35638=CARTESIAN_POINT('Ctrl Pts',(5.07339475843234,-0.767536645770191,
7.26757857289005));
#35639=CARTESIAN_POINT('Ctrl Pts',(5.07394313380082,7.47405269749084E-5,
7.29166315536293));
#35640=CARTESIAN_POINT('Ctrl Pts',(5.07363207848188,-0.000130424372061667,
6.20833684463708));
#35641=CARTESIAN_POINT('Ctrl Pts',(5.07295192244443,0.659114832324929,6.22901766783102));
#35642=CARTESIAN_POINT('Ctrl Pts',(4.77864726944019,2.16233220285461,6.27615578770943));
#35643=CARTESIAN_POINT('Ctrl Pts',(3.33483365177601,4.10485393921541,6.34975120427228));
#35644=CARTESIAN_POINT('Ctrl Pts',(0.96533761058682,5.19991006123149,6.42912309432572));
#35645=CARTESIAN_POINT('Ctrl Pts',(-1.63931253580277,5.02827960213728,6.50849498437909));
#35646=CARTESIAN_POINT('Ctrl Pts',(-3.84462977702757,3.63177136187054,6.58786687443252));
#35647=CARTESIAN_POINT('Ctrl Pts',(-5.11340371451209,1.35057165664169,6.6672387644859));
#35648=CARTESIAN_POINT('Ctrl Pts',(-5.13656382546863,-1.25962431470543,
6.74661065453933));
#35649=CARTESIAN_POINT('Ctrl Pts',(-3.90846835813217,-3.56297859112141,
6.82598254459271));
#35650=CARTESIAN_POINT('Ctrl Pts',(-1.72827865000271,-4.99839916925957,
6.90535443464612));
#35651=CARTESIAN_POINT('Ctrl Pts',(0.872915911787522,-5.21622077353501,
6.98472632469953));
#35652=CARTESIAN_POINT('Ctrl Pts',(3.26147008963291,-4.16338254328616,7.06409821475292));
#35653=CARTESIAN_POINT('Ctrl Pts',(4.7584325270959,-2.22226951355623,7.13863505473211));
#35654=CARTESIAN_POINT('Ctrl Pts',(5.07302701285767,-0.689094952273734,
7.18671459802684));
#35655=CARTESIAN_POINT('Ctrl Pts',(5.0737268532953,0.000123079057421736,
7.20833684463709));
#35656=CARTESIAN_POINT('Origin',(0.,0.,-2.20833684463713));
#35657=CARTESIAN_POINT('',(5.07326256235615,8.6340948239616E-5,5.20833684463708));
#35658=CARTESIAN_POINT('',(5.07345306532775,0.000126183674940957,5.29166315536293));
#35659=CARTESIAN_POINT('',(5.0736,-1.85409460923845E-12,-2.20833684463713));
#35660=CARTESIAN_POINT('Ctrl Pts',(5.07345306532775,0.000126183674940827,
5.29166315536293));
#35661=CARTESIAN_POINT('Ctrl Pts',(5.07368016839978,0.24263894378533,5.29927011912949));
#35662=CARTESIAN_POINT('Ctrl Pts',(4.99721910617995,1.32847790639321,5.33333437958052));
#35663=CARTESIAN_POINT('Ctrl Pts',(4.23545891089922,3.1673062942182,5.39385593671601));
#35664=CARTESIAN_POINT('Ctrl Pts',(2.20468883537238,4.80731614172549,5.47322782676942));
#35665=CARTESIAN_POINT('Ctrl Pts',(-0.363138560455233,5.27627441792221,
5.55259971682281));
#35666=CARTESIAN_POINT('Ctrl Pts',(-2.84250620674952,4.45994392474844,5.63197160687622));
#35667=CARTESIAN_POINT('Ctrl Pts',(-4.62944563286038,2.55718096342436,5.71134349692963));
#35668=CARTESIAN_POINT('Ctrl Pts',(-5.28866234991055,0.0314943796341776,
5.79071538698302));
#35669=CARTESIAN_POINT('Ctrl Pts',(-4.65957262477808,-2.50186416532327,
5.87008727703643));
#35670=CARTESIAN_POINT('Ctrl Pts',(-2.89542132203872,-4.42577413739037,
5.94945916708984));
#35671=CARTESIAN_POINT('Ctrl Pts',(-0.425951794157121,-5.27157532587407,
6.02883105714324));
#35672=CARTESIAN_POINT('Ctrl Pts',(2.14727864795285,-4.8332324334089,6.10820294719664));
#35673=CARTESIAN_POINT('Ctrl Pts',(4.19743676434218,-3.21752481834385,6.18757483725004));
#35674=CARTESIAN_POINT('Ctrl Pts',(4.98922373212554,-1.36879789494917,6.24872823997214));
#35675=CARTESIAN_POINT('Ctrl Pts',(5.0736256122357,-0.262783913782733,6.28342434600977));
#35676=CARTESIAN_POINT('Ctrl Pts',(5.07339692231655,-0.000119345805453183,
6.29166315536293));
#35677=CARTESIAN_POINT('Ctrl Pts',(5.07326256235615,8.63409482398936E-5,
5.20833684463708));
#35678=CARTESIAN_POINT('Ctrl Pts',(5.07345742030602,0.321133824030879,5.21840614426627));
#35679=CARTESIAN_POINT('Ctrl Pts',(4.96462985132702,1.48560987617541,5.25493274057992));
#35680=CARTESIAN_POINT('Ctrl Pts',(4.08394322312664,3.36040906700182,5.31791663357805));
#35681=CARTESIAN_POINT('Ctrl Pts',(1.979268164295,4.90443053586431,5.39728852363145));
#35682=CARTESIAN_POINT('Ctrl Pts',(-0.607552238323124,5.25374358196311,
5.47666041368485));
#35683=CARTESIAN_POINT('Ctrl Pts',(-3.04637426047979,4.32325632045987,5.55603230373826));
#35684=CARTESIAN_POINT('Ctrl Pts',(-4.74310625581864,2.33963338865815,5.63540419379165));
#35685=CARTESIAN_POINT('Ctrl Pts',(-5.28442806592769,-0.213919057930008,
5.71477608384507));
#35686=CARTESIAN_POINT('Ctrl Pts',(-4.53847489605989,-2.71536129550824,
5.79414797389846));
#35687=CARTESIAN_POINT('Ctrl Pts',(-2.68695928725567,-4.55534753185094,
5.87351986395187));
#35688=CARTESIAN_POINT('Ctrl Pts',(-0.180906343559476,-5.28566119252549,
5.95289175400528));
#35689=CARTESIAN_POINT('Ctrl Pts',(2.36921498499841,-4.72839948631341,6.03226364405867));
#35690=CARTESIAN_POINT('Ctrl Pts',(4.3422007873791,-3.01931013137013,6.1116355341121));
#35691=CARTESIAN_POINT('Ctrl Pts',(5.01896602830084,-1.21167525394927,6.17032660097155));
#35692=CARTESIAN_POINT('Ctrl Pts',(5.07382205657331,-0.184267811620037,
6.20256037114655));
#35693=CARTESIAN_POINT('Ctrl Pts',(5.07363207848188,-0.000130424372061667,
6.20833684463708));
#35694=CARTESIAN_POINT('Origin',(0.,0.,-2.20833684463713));
#35695=CARTESIAN_POINT('',(5.07402907570203,-1.82827833135855E-5,4.20833684463708));
#35696=CARTESIAN_POINT('',(5.07389532565035,-9.07960786141478E-5,4.29166315536292));
#35697=CARTESIAN_POINT('',(5.0736,-1.85409460923845E-12,-2.20833684463713));
#35698=CARTESIAN_POINT('Ctrl Pts',(5.07389532565035,-9.07960786142303E-5,
4.29166315536292));
#35699=CARTESIAN_POINT('Ctrl Pts',(5.07327433146367,0.747403143972462,4.3151158922492));
#35700=CARTESIAN_POINT('Ctrl Pts',(4.7173237838915,2.33872520323751,4.36502592581995));
#35701=CARTESIAN_POINT('Ctrl Pts',(3.11590430478523,4.27341569598967,4.44139325607517));
#35702=CARTESIAN_POINT('Ctrl Pts',(0.692451950200399,5.24322912373411,4.52076514612856));
#35703=CARTESIAN_POINT('Ctrl Pts',(-1.89968016673685,4.93580354262775,4.60013703618198));
#35704=CARTESIAN_POINT('Ctrl Pts',(-4.02905439992773,3.42602714375309,4.67950892623537));
#35705=CARTESIAN_POINT('Ctrl Pts',(-5.17695989945686,1.08167811604265,4.75888081628878));
#35706=CARTESIAN_POINT('Ctrl Pts',(-5.06376942648468,-1.5261653064819,4.83825270634218));
#35707=CARTESIAN_POINT('Ctrl Pts',(-3.71705592968434,-3.76223823845706,
4.91762459639559));
#35708=CARTESIAN_POINT('Ctrl Pts',(-1.46487583597662,-5.08183826311717,
4.996996486449));
#35709=CARTESIAN_POINT('Ctrl Pts',(1.14414476892732,-5.16351373534013,5.07636837650239));
#35710=CARTESIAN_POINT('Ctrl Pts',(3.47445424064207,-3.98736869087803,5.15574026655581));
#35711=CARTESIAN_POINT('Ctrl Pts',(4.81617424358115,-2.04572091909076,5.22750519284264));
#35712=CARTESIAN_POINT('Ctrl Pts',(5.07289029565433,-0.600829257314202,
5.27281282244502));
#35713=CARTESIAN_POINT('Ctrl Pts',(5.07345306532775,0.000126183674940827,
5.29166315536293));
#35714=CARTESIAN_POINT('Ctrl Pts',(5.07402907570203,-1.82827833134858E-5,
4.20833684463708));
#35715=CARTESIAN_POINT('Ctrl Pts',(5.07386028856637,0.825892891192897,4.23425191738599));
#35716=CARTESIAN_POINT('Ctrl Pts',(4.65820682968666,2.49515959185088,4.28662428681936));
#35717=CARTESIAN_POINT('Ctrl Pts',(2.91427384097298,4.41338297988409,4.36545395293721));
#35718=CARTESIAN_POINT('Ctrl Pts',(0.44843468320075,5.26971039832481,4.44482584299061));
#35719=CARTESIAN_POINT('Ctrl Pts',(-2.12664217080585,4.84234802803972,4.52419773304401));
#35720=CARTESIAN_POINT('Ctrl Pts',(-4.18367369924674,3.23540039647972,4.60356962309741));
#35721=CARTESIAN_POINT('Ctrl Pts',(-5.22157157495578,0.840316389774564,
4.68294151315082));
#35722=CARTESIAN_POINT('Ctrl Pts',(-4.98750617275825,-1.75946682947089,
4.76231340320422));
#35723=CARTESIAN_POINT('Ctrl Pts',(-3.53849530653447,-3.93064782357102,
4.84168529325762));
#35724=CARTESIAN_POINT('Ctrl Pts',(-1.22751481596538,-5.14433170819062,
4.92105718331103));
#35725=CARTESIAN_POINT('Ctrl Pts',(1.3824855667149,-5.10486777548008,5.00042907336443));
#35726=CARTESIAN_POINT('Ctrl Pts',(3.65571552542333,-3.82186935209575,5.07980096341784));
#35727=CARTESIAN_POINT('Ctrl Pts',(4.86300805809873,-1.88874478353847,5.14910355384205));
#35728=CARTESIAN_POINT('Ctrl Pts',(5.07294542694196,-0.522425194224716,
5.1919488475818));
#35729=CARTESIAN_POINT('Ctrl Pts',(5.07326256235615,8.63409482398936E-5,
5.20833684463708));
#35730=CARTESIAN_POINT('Origin',(0.,0.,-2.20833684463713));
#35731=CARTESIAN_POINT('',(5.0732079990561,-5.95000919163813E-5,3.20833684463708));
#35732=CARTESIAN_POINT('',(5.07316685382493,1.14989646604178E-5,3.29166315536292));
#35733=CARTESIAN_POINT('',(5.0736,-1.85409460923845E-12,-2.20833684463713));
#35734=CARTESIAN_POINT('Ctrl Pts',(5.07316685382493,1.14989646600797E-5,
3.29166315536292));
#35735=CARTESIAN_POINT('Ctrl Pts',(5.07319917633903,0.409460216043812,3.30450436868445));
#35736=CARTESIAN_POINT('Ctrl Pts',(4.923282999623,1.66249023374937,3.34380287869045));
#35737=CARTESIAN_POINT('Ctrl Pts',(3.90287063578958,3.56910943340232,3.40955868538091));
#35738=CARTESIAN_POINT('Ctrl Pts',(1.7204303939291,5.00110593838552,3.48893057543432));
#35739=CARTESIAN_POINT('Ctrl Pts',(-0.881102883784432,5.21484410653825,
3.56830246548772));
#35740=CARTESIAN_POINT('Ctrl Pts',(-3.26800144929621,4.15825779319991,3.64767435554113));
#35741=CARTESIAN_POINT('Ctrl Pts',(-4.85882209535798,2.08872908558557,3.72704624559453));
#35742=CARTESIAN_POINT('Ctrl Pts',(-5.2660444338108,-0.489609403954008,
3.80641813564793));
#35743=CARTESIAN_POINT('Ctrl Pts',(-4.39047000437897,-2.94868012642242,
3.88579002570134));
#35744=CARTESIAN_POINT('Ctrl Pts',(-2.44538680002092,-4.68945889688708,
3.96516191575474));
#35745=CARTESIAN_POINT('Ctrl Pts',(0.0953872160503347,-5.28789586001125,
4.04453380580815));
#35746=CARTESIAN_POINT('Ctrl Pts',(2.61292511742776,-4.59821309619564,4.12390569586154));
#35747=CARTESIAN_POINT('Ctrl Pts',(4.49396024381142,-2.78841580011883,4.20327758591496));
#35748=CARTESIAN_POINT('Ctrl Pts',(5.04793652990732,-1.03482867897542,4.25919673908208));
#35749=CARTESIAN_POINT('Ctrl Pts',(5.07397488200138,-0.0958531905725829,
4.28865859556473));
#35750=CARTESIAN_POINT('Ctrl Pts',(5.07389532565035,-9.07960786142303E-5,
4.29166315536292));
#35751=CARTESIAN_POINT('Ctrl Pts',(5.0732079990561,-5.95000919163813E-5,
3.20833684463708));
#35752=CARTESIAN_POINT('Ctrl Pts',(5.07300669336618,0.487890744857983,3.22364039382123));
#35753=CARTESIAN_POINT('Ctrl Pts',(4.88232843229471,1.81957999791209,3.26540123968986));
#35754=CARTESIAN_POINT('Ctrl Pts',(3.73307055280206,3.74634830136122,3.33361938224296));
#35755=CARTESIAN_POINT('Ctrl Pts',(1.48653991852054,5.07554336184363,3.41299127229636));
#35756=CARTESIAN_POINT('Ctrl Pts',(-1.12210854951228,5.16834729390561,3.49236316234976));
#35757=CARTESIAN_POINT('Ctrl Pts',(-3.45741385862906,4.00215326511488,3.57173505240317));
#35758=CARTESIAN_POINT('Ctrl Pts',(-4.95050080463958,1.86104355955814,3.65110694245657));
#35759=CARTESIAN_POINT('Ctrl Pts',(-5.23765671238755,-0.733412237756895,
3.73047883250997));
#35760=CARTESIAN_POINT('Ctrl Pts',(-4.24893103835441,-3.14921043733482,
3.80985072256337));
#35761=CARTESIAN_POINT('Ctrl Pts',(-2.22517516822744,-4.79786794503704,
3.88922261261678));
#35762=CARTESIAN_POINT('Ctrl Pts',(0.340628447538026,-5.2777754412288,3.96859450267018));
#35763=CARTESIAN_POINT('Ctrl Pts',(2.82345572745151,-4.472028522095,4.04796639272359));
#35764=CARTESIAN_POINT('Ctrl Pts',(4.61849544177105,-2.57690535364612,4.12733828277699));
#35765=CARTESIAN_POINT('Ctrl Pts',(5.06972869559084,-0.877769583505955,
4.18079510008149));
#35766=CARTESIAN_POINT('Ctrl Pts',(5.07403260725396,-0.0172989136932101,
4.20779462070152));
#35767=CARTESIAN_POINT('Ctrl Pts',(5.07402907570203,-1.82827833134858E-5,
4.20833684463708));
#35768=CARTESIAN_POINT('Origin',(0.,0.,-2.20833684463713));
#35769=CARTESIAN_POINT('',(5.07374102492394,0.00012139426775859,2.20833684463708));
#35770=CARTESIAN_POINT('',(5.07395289332891,7.08096438841769E-5,2.29166315536292));
#35771=CARTESIAN_POINT('',(5.0736,-1.85409460923845E-12,-2.20833684463713));
#35772=CARTESIAN_POINT('Ctrl Pts',(5.07395289332891,7.08096438841854E-5,
2.29166315536292));
#35773=CARTESIAN_POINT('Ctrl Pts',(5.07400149993288,0.0711339346777274,
2.2938928451197));
#35774=CARTESIAN_POINT('Ctrl Pts',(5.05519150559033,0.985399910949532,2.32257983156095));
#35775=CARTESIAN_POINT('Ctrl Pts',(4.53420692607935,2.72248212093367,2.37772411468667));
#35776=CARTESIAN_POINT('Ctrl Pts',(2.67980532059554,4.5595597146017,2.45709600474007));
#35777=CARTESIAN_POINT('Ctrl Pts',(0.172609070663326,5.28593865420646,2.53646789479348));
#35778=CARTESIAN_POINT('Ctrl Pts',(-2.37663436681889,4.72467463787357,2.61583978484688));
#35779=CARTESIAN_POINT('Ctrl Pts',(-4.34693493313492,3.01249033764445,2.69521167490029));
#35780=CARTESIAN_POINT('Ctrl Pts',(-5.25833177151656,0.56647005919948,2.77458356495369));
#35781=CARTESIAN_POINT('Ctrl Pts',(-4.88881062947673,-2.01754107180632,
2.85395545500709));
#35782=CARTESIAN_POINT('Ctrl Pts',(-3.32838603929513,-4.11008366347149,
2.93332734506049));
#35783=CARTESIAN_POINT('Ctrl Pts',(-0.957173977198773,-5.20141897223089,
3.0126992351139));
#35784=CARTESIAN_POINT('Ctrl Pts',(1.64720354707453,-5.02570013250045,3.0920711251673));
#35785=CARTESIAN_POINT('Ctrl Pts',(3.85032593330369,-3.62573186469146,3.1714430152207));
#35786=CARTESIAN_POINT('Ctrl Pts',(4.91082792455161,-1.71192991859137,3.23797369195258));
#35787=CARTESIAN_POINT('Ctrl Pts',(5.07313258089171,-0.434144349474542,
3.27804707199999));
#35788=CARTESIAN_POINT('Ctrl Pts',(5.07316685382493,1.14989646600797E-5,
3.29166315536292));
#35789=CARTESIAN_POINT('Ctrl Pts',(5.07374102492394,0.000121394267758555,
2.20833684463708));
#35790=CARTESIAN_POINT('Ctrl Pts',(5.07389186228029,0.149680441629337,2.21302887025649));
#35791=CARTESIAN_POINT('Ctrl Pts',(5.03086461164817,1.14248345247706,2.24417819256036));
#35792=CARTESIAN_POINT('Ctrl Pts',(4.40300813596794,2.92992503348825,2.3017848115487));
#35793=CARTESIAN_POINT('Ctrl Pts',(2.46536820371062,4.67898503603904,2.38115670160211));
#35794=CARTESIAN_POINT('Ctrl Pts',(-0.0728299659737919,5.28825464055465,
2.46052859165552));
#35795=CARTESIAN_POINT('Ctrl Pts',(-2.59328691715172,4.60931711999155,2.53990048170891));
#35796=CARTESIAN_POINT('Ctrl Pts',(-4.4820249154556,2.80756015154502,2.61927237176233));
#35797=CARTESIAN_POINT('Ctrl Pts',(-5.27895156514789,0.321887744613165,
2.69864426181572));
#35798=CARTESIAN_POINT('Ctrl Pts',(-4.7899372983315,-2.2421958044211,2.77801615186913));
#35799=CARTESIAN_POINT('Ctrl Pts',(-3.13410490798781,-4.26008541851404,
2.85738804192253));
#35800=CARTESIAN_POINT('Ctrl Pts',(-0.714811499281904,-5.2402276541964,
2.93675993197593));
#35801=CARTESIAN_POINT('Ctrl Pts',(1.8786084084407,-4.94386203236353,3.01613182202934));
#35802=CARTESIAN_POINT('Ctrl Pts',(4.01440346609632,-3.44318256249998,3.09550371208274));
#35803=CARTESIAN_POINT('Ctrl Pts',(4.9490470546202,-1.55481288423713,3.15957205295199));
#35804=CARTESIAN_POINT('Ctrl Pts',(5.07335471749433,-0.355694245953322,
3.19718309713677));
#35805=CARTESIAN_POINT('Ctrl Pts',(5.0732079990561,-5.95000919163813E-5,
3.20833684463708));
#35806=CARTESIAN_POINT('Origin',(0.,0.,-2.20833684463713));
#35807=CARTESIAN_POINT('',(5.07361762168166,-0.000130982038957922,1.20833684463708));
#35808=CARTESIAN_POINT('',(5.07338480805012,-0.000117445791330803,1.29166315536292));
#35809=CARTESIAN_POINT('',(5.0736,-1.85409460923845E-12,-2.20833684463713));
#35810=CARTESIAN_POINT('Ctrl Pts',(5.07338480805012,-0.000117445791331001,
1.29166315536292));
#35811=CARTESIAN_POINT('Ctrl Pts',(5.07289281667254,0.576157106237108,1.30973861823942));
#35812=CARTESIAN_POINT('Ctrl Pts',(4.83135991405541,1.99633436079896,1.35427137780039));
#35813=CARTESIAN_POINT('Ctrl Pts',(3.53232089954478,3.93619745533352,1.42526143404583));
#35814=CARTESIAN_POINT('Ctrl Pts',(1.21943810235538,5.14625223481536,1.50463332409923));
#35815=CARTESIAN_POINT('Ctrl Pts',(-1.39049711694202,5.10269135980955,1.58400521415263));
#35816=CARTESIAN_POINT('Ctrl Pts',(-3.66171031660135,3.81612616476449,1.66337710420604));
#35817=CARTESIAN_POINT('Ctrl Pts',(-5.04093898807,1.59996108251987,1.74274899425944));
#35818=CARTESIAN_POINT('Ctrl Pts',(-5.19220608004013,-1.00595097780601,
1.82212088431284));
#35819=CARTESIAN_POINT('Ctrl Pts',(-4.07866326363067,-3.3668156066614,1.90149277436625));
#35820=CARTESIAN_POINT('Ctrl Pts',(-1.97156710418735,-4.90753140600723,
1.98086466441965));
#35821=CARTESIAN_POINT('Ctrl Pts',(0.61579843785608,-5.25278341751101,2.06023655447306));
#35822=CARTESIAN_POINT('Ctrl Pts',(3.0531568434793,-4.31846901533485,2.13960844452646));
#35823=CARTESIAN_POINT('Ctrl Pts',(4.69919647653223,-2.38798317189229,2.21675064482308));
#35824=CARTESIAN_POINT('Ctrl Pts',(5.07342473837308,-0.772094669942323,
2.26743554843524));
#35825=CARTESIAN_POINT('Ctrl Pts',(5.07395289332891,7.08096438841854E-5,
2.29166315536292));
#35826=CARTESIAN_POINT('Ctrl Pts',(5.07361762168166,-0.000130982038957766,
1.20833684463708));
#35827=CARTESIAN_POINT('Ctrl Pts',(5.07294327622754,0.654560436527497,1.2288746433762));
#35828=CARTESIAN_POINT('Ctrl Pts',(4.78166373276894,2.15322402421039,1.2758697387998));
#35829=CARTESIAN_POINT('Ctrl Pts',(3.34588798700519,4.09584848370755,1.34932213090786));
#35830=CARTESIAN_POINT('Ctrl Pts',(0.979352771366438,5.19728867487042,1.42869402096127));
#35831=CARTESIAN_POINT('Ctrl Pts',(-1.6257506180571,5.03268082057239,1.50806591101467));
#35832=CARTESIAN_POINT('Ctrl Pts',(-3.83482475204895,3.64212307300266,1.58743780106807));
#35833=CARTESIAN_POINT('Ctrl Pts',(-5.10974406648874,1.36435219862418,1.66680969112148));
#35834=CARTESIAN_POINT('Ctrl Pts',(-5.13994103560183,-1.2457718471981,1.74618158117488));
#35835=CARTESIAN_POINT('Ctrl Pts',(-3.91805974601548,-3.55242863073578,
1.82555347122828));
#35836=CARTESIAN_POINT('Ctrl Pts',(-1.74174777450957,-4.99372166181597,
1.90492536128169));
#35837=CARTESIAN_POINT('Ctrl Pts',(0.858850099431454,-5.21855515011689,
1.98429725133509));
#35838=CARTESIAN_POINT('Ctrl Pts',(3.25023399025869,-4.17216015459491,2.0636691413885));
#35839=CARTESIAN_POINT('Ctrl Pts',(4.75530658628425,-2.2313729735679,2.13834900582249));
#35840=CARTESIAN_POINT('Ctrl Pts',(5.0730413237258,-0.693650010686127,2.18657157357202));
#35841=CARTESIAN_POINT('Ctrl Pts',(5.07374102492394,0.000121394267758555,
2.20833684463708));
#35842=CARTESIAN_POINT('Origin',(0.,0.,-2.20833684463713));
#35843=CARTESIAN_POINT('',(5.07327550687406,0.000108476183186546,0.208336844637077));
#35844=CARTESIAN_POINT('',(5.07346622253939,0.000127574377019038,0.291663155362924));
#35845=CARTESIAN_POINT('',(5.0736,-1.85409460923845E-12,-2.20833684463713));
#35846=CARTESIAN_POINT('',(1.3130361863565,-4.90075024188322,0.));
#35847=CARTESIAN_POINT('Ctrl Pts',(1.3130361863565,-4.90075024188322,0.));
#35848=CARTESIAN_POINT('Ctrl Pts',(2.12771778283771,-4.68247622999897,0.0264572966844678));
#35849=CARTESIAN_POINT('Ctrl Pts',(3.64531650851188,-3.8320815322798,0.0793718900534037));
#35850=CARTESIAN_POINT('Ctrl Pts',(4.86042636846397,-1.89775322538081,0.148817504932429));
#35851=CARTESIAN_POINT('Ctrl Pts',(5.07294944175775,-0.526932428119567,
0.191805823126987));
#35852=CARTESIAN_POINT('Ctrl Pts',(5.07327550687406,0.000108476183186372,
0.208336844637077));
#35853=CARTESIAN_POINT('',(-1.31317395760259,-4.90115117757553,2.08166817117217E-16));
#35854=CARTESIAN_POINT('Origin',(0.,0.,0.));
#35855=CARTESIAN_POINT('Ctrl Pts',(-1.31317395760259,-4.90115117757553,
2.32154790183459E-16));
#35856=CARTESIAN_POINT('Ctrl Pts',(-0.533836595431888,-5.10962665469163,
0.025313101045988));
#35857=CARTESIAN_POINT('Ctrl Pts',(1.16384881260007,-5.14969078544564,0.0770834987764434));
#35858=CARTESIAN_POINT('Ctrl Pts',(3.46369715057722,-3.99673439595713,0.155311193191368));
#35859=CARTESIAN_POINT('Ctrl Pts',(4.8133239766203,-2.05483010796368,0.22721914393302));
#35860=CARTESIAN_POINT('Ctrl Pts',(5.0728909576883,-0.605381739016801,0.272669797990206));
#35861=CARTESIAN_POINT('Ctrl Pts',(5.07346622253938,0.000127574377019116,
0.291663155362924));
#35862=CARTESIAN_POINT('Origin',(4.45462538595717E-16,-1.65775395963113E-16,
40.));
#35863=CARTESIAN_POINT('Ctrl Pts',(3.43378788736169,2.9358415841302,40.));
#35864=CARTESIAN_POINT('Ctrl Pts',(3.52814292550769,2.83820823955091,40.));
#35865=CARTESIAN_POINT('Ctrl Pts',(3.61787392647867,2.73637499985595,40.));
#35866=CARTESIAN_POINT('Ctrl Pts',(3.7028436241849,2.63075402506017,40.));
#35867=CARTESIAN_POINT('Ctrl Pts',(3.78889648523297,2.52378663182211,40.));
#35868=CARTESIAN_POINT('Ctrl Pts',(3.87006637156126,2.41293377092847,40.));
#35869=CARTESIAN_POINT('Ctrl Pts',(3.94617716449749,2.2985820569619,40.));
#35870=CARTESIAN_POINT('Ctrl Pts',(3.98452054291682,2.24097352507873,40.));
#35871=CARTESIAN_POINT('Ctrl Pts',(4.02157936104048,2.18247639180456,40.));
#35872=CARTESIAN_POINT('Ctrl Pts',(4.0573273224032,2.12313686354418,40.));
#35873=CARTESIAN_POINT('Ctrl Pts',(4.07057108419318,2.10115299237913,40.));
#35874=CARTESIAN_POINT('Ctrl Pts',(4.08363549665298,2.07905229886435,40.));
#35875=CARTESIAN_POINT('Ctrl Pts',(4.09651028112638,2.05685278711327,40.));
#35876=CARTESIAN_POINT('Ctrl Pts',(4.16636767341313,1.93640028523473,40.));
#35877=CARTESIAN_POINT('Ctrl Pts',(4.23070798356748,1.81293936852798,40.));
#35878=CARTESIAN_POINT('Ctrl Pts',(4.28936081037521,1.68687424953695,40.));
#35879=CARTESIAN_POINT('Ctrl Pts',(4.34350578332916,1.57049806053275,40.));
#35880=CARTESIAN_POINT('Ctrl Pts',(4.39280381894615,1.45190174917925,40.));
#35881=CARTESIAN_POINT('Ctrl Pts',(4.4370895395389,1.33137973638483,40.));
#35882=CARTESIAN_POINT('Ctrl Pts',(4.45048806014006,1.29491613932226,40.));
#35883=CARTESIAN_POINT('Ctrl Pts',(4.46342755329992,1.25827614359673,40.));
#35884=CARTESIAN_POINT('Ctrl Pts',(4.47590283035858,1.22146759434429,40.));
#35885=CARTESIAN_POINT('Ctrl Pts',(4.48543045669819,1.19335614625929,40.));
#35886=CARTESIAN_POINT('Ctrl Pts',(4.49468731429383,1.16514638329788,40.));
#35887=CARTESIAN_POINT('Ctrl Pts',(4.50367097326761,1.13684175481395,40.));
#35888=CARTESIAN_POINT('Ctrl Pts',(4.50984234488601,1.11739774192287,40.));
#35889=CARTESIAN_POINT('Ctrl Pts',(4.51588427541961,1.09791040265649,40.));
#35890=CARTESIAN_POINT('Ctrl Pts',(4.52179265714445,1.0783924896528,40.));
#35891=CARTESIAN_POINT('Ctrl Pts',(4.53324480098953,1.04056115821829,40.));
#35892=CARTESIAN_POINT('Ctrl Pts',(4.54419899621228,1.00260320591424,40.));
#35893=CARTESIAN_POINT('Ctrl Pts',(4.5546518960517,0.964527761093808,40.));
#35894=CARTESIAN_POINT('Ctrl Pts',(4.59117593379611,0.831486307992675,40.));
#35895=CARTESIAN_POINT('Ctrl Pts',(4.62158314424656,0.697012525339414,40.));
#35896=CARTESIAN_POINT('Ctrl Pts',(4.64596931935994,0.561539349137144,40.));
#35897=CARTESIAN_POINT('Ctrl Pts',(4.67073918176772,0.42393466456182,40.));
#35898=CARTESIAN_POINT('Ctrl Pts',(4.68929722659476,0.28529820513645,40.));
#35899=CARTESIAN_POINT('Ctrl Pts',(4.70169535323682,0.146060437529888,40.));
#35900=CARTESIAN_POINT('Ctrl Pts',(4.71417778478848,0.00587587951314419,
40.));
#35901=CARTESIAN_POINT('Ctrl Pts',(4.7204163646451,-0.134918963378981,40.));
#35902=CARTESIAN_POINT('Ctrl Pts',(4.72041312729179,-0.275897046739804,
40.));
#35903=CARTESIAN_POINT('Ctrl Pts',(4.72041101510801,-0.367877004659711,
40.));
#35904=CARTESIAN_POINT('Ctrl Pts',(4.71775084452937,-0.459935190334389,
40.));
#35905=CARTESIAN_POINT('Ctrl Pts',(4.71242122767243,-0.55195336772424,40.));
#35906=CARTESIAN_POINT('Ctrl Pts',(4.71074982773409,-0.580810822236322,
40.));
#35907=CARTESIAN_POINT('Ctrl Pts',(4.70881582061262,-0.609664336690085,
40.));
#35908=CARTESIAN_POINT('Ctrl Pts',(4.70661866095158,-0.638510242454293,
40.));
#35909=CARTESIAN_POINT('Ctrl Pts',(4.70521659891363,-0.65691752988966,40.));
#35910=CARTESIAN_POINT('Ctrl Pts',(4.70370712995809,-0.675324500804579,
40.));
#35911=CARTESIAN_POINT('Ctrl Pts',(4.70209092940465,-0.693720810758238,
40.));
#35912=CARTESIAN_POINT('Ctrl Pts',(4.68953110086222,-0.836682337618008,
40.));
#35913=CARTESIAN_POINT('Ctrl Pts',(4.67055276432277,-0.978761795279802,
40.));
#35914=CARTESIAN_POINT('Ctrl Pts',(4.64522498551854,-1.11951304986637,40.));
#35915=CARTESIAN_POINT('Ctrl Pts',(4.63006091029742,-1.20378268237205,40.));
#35916=CARTESIAN_POINT('Ctrl Pts',(4.61261985737539,-1.28757653832611,40.));
#35917=CARTESIAN_POINT('Ctrl Pts',(4.59290787692688,-1.37080047994428,40.));
#35918=CARTESIAN_POINT('Ctrl Pts',(4.56017758990635,-1.5089876856012,40.));
#35919=CARTESIAN_POINT('Ctrl Pts',(4.52118921321033,-1.64560413309505,40.));
#35920=CARTESIAN_POINT('Ctrl Pts',(4.47619425969956,-1.78030079004358,40.));
#35921=CARTESIAN_POINT('Ctrl Pts',(4.43085717885509,-1.91602163758472,40.));
#35922=CARTESIAN_POINT('Ctrl Pts',(4.3794215892058,-2.04979410792511,40.));
#35923=CARTESIAN_POINT('Ctrl Pts',(4.32209322112883,-2.18124988516394,40.));
#35924=CARTESIAN_POINT('Ctrl Pts',(4.29589299313303,-2.24132784395735,40.));
#35925=CARTESIAN_POINT('Ctrl Pts',(4.26846127047772,-2.30092169976294,40.));
#35926=CARTESIAN_POINT('Ctrl Pts',(4.23981435864377,-2.35999488119432,40.));
#35927=CARTESIAN_POINT('Ctrl Pts',(4.22808815540088,-2.38417564230685,40.));
#35928=CARTESIAN_POINT('Ctrl Pts',(4.21615831686625,-2.40826914901153,40.));
#35929=CARTESIAN_POINT('Ctrl Pts',(4.20402586547368,-2.43227283763382,40.));
#35930=CARTESIAN_POINT('Ctrl Pts',(4.19226175293326,-2.45554777896271,40.));
#35931=CARTESIAN_POINT('Ctrl Pts',(4.18030467857245,-2.47874278381504,40.));
#35932=CARTESIAN_POINT('Ctrl Pts',(4.16817016036066,-2.50182817485463,40.));
#35933=CARTESIAN_POINT('Ctrl Pts',(4.10062993280007,-2.63032050861895,40.));
#35934=CARTESIAN_POINT('Ctrl Pts',(4.02752679248241,-2.75556160907446,40.));
#35935=CARTESIAN_POINT('Ctrl Pts',(3.94914189359867,-2.87720021634157,40.));
#35936=CARTESIAN_POINT('Ctrl Pts',(3.87013649228652,-2.99980172656921,40.));
#35937=CARTESIAN_POINT('Ctrl Pts',(3.78576510402317,-3.11874421706065,40.));
#35938=CARTESIAN_POINT('Ctrl Pts',(3.69626453833047,-3.23365468399741,40.));
#35939=CARTESIAN_POINT('Ctrl Pts',(3.6256051940776,-3.3243747613366,40.));
#35940=CARTESIAN_POINT('Ctrl Pts',(3.55174784325694,-3.41258159925288,40.));
#35941=CARTESIAN_POINT('Ctrl Pts',(3.4747885470066,-3.49808125449705,40.));
#35942=CARTESIAN_POINT('Ctrl Pts',(3.37754842452615,-3.60611234824477,40.));
#35943=CARTESIAN_POINT('Ctrl Pts',(3.27535698426899,-3.70982288325437,40.));
#35944=CARTESIAN_POINT('Ctrl Pts',(3.16857103825032,-3.80899091582305,40.));
#35945=CARTESIAN_POINT('Ctrl Pts',(3.13709749914945,-3.83821919039451,40.));
#35946=CARTESIAN_POINT('Ctrl Pts',(3.10522459675968,-3.86705262006651,40.));
#35947=CARTESIAN_POINT('Ctrl Pts',(3.07296088810501,-3.89548488187744,40.));
#35948=CARTESIAN_POINT('Ctrl Pts',(3.05413623645007,-3.91207402945752,40.));
#35949=CARTESIAN_POINT('Ctrl Pts',(3.03517853882814,-3.92852660249152,40.));
#35950=CARTESIAN_POINT('Ctrl Pts',(3.01608945850777,-3.94484129509693,40.));
#35951=CARTESIAN_POINT('Ctrl Pts',(3.00324987792049,-3.95581478396849,40.));
#35952=CARTESIAN_POINT('Ctrl Pts',(2.99035184084321,-3.96672500977969,40.));
#35953=CARTESIAN_POINT('Ctrl Pts',(2.97740348730282,-3.97756535219416,40.));
#35954=CARTESIAN_POINT('Ctrl Pts',(2.86172546572695,-4.07441082060052,40.));
#35955=CARTESIAN_POINT('Ctrl Pts',(2.74187291014631,-4.16582105105552,40.));
#35956=CARTESIAN_POINT('Ctrl Pts',(2.61830752500134,-4.25161650299712,40.));
#35957=CARTESIAN_POINT('Ctrl Pts',(2.49666368456262,-4.33607776416752,40.));
#35958=CARTESIAN_POINT('Ctrl Pts',(2.37142082394795,-4.41509790443455,40.));
#35959=CARTESIAN_POINT('Ctrl Pts',(2.24297630552737,-4.4884725438774,40.));
#35960=CARTESIAN_POINT('Ctrl Pts',(2.11148832986889,-4.56358577505025,40.));
#35961=CARTESIAN_POINT('Ctrl Pts',(1.97664462468232,-4.63278348201276,40.));
#35962=CARTESIAN_POINT('Ctrl Pts',(1.83883549494666,-4.69580305762063,40.));
#35963=CARTESIAN_POINT('Ctrl Pts',(1.701026365211,-4.7588226332285,40.));
#35964=CARTESIAN_POINT('Ctrl Pts',(1.56025109502399,-4.81566463443687,40.));
#35965=CARTESIAN_POINT('Ctrl Pts',(1.41687422066896,-4.86601447289837,40.));
#35966=CARTESIAN_POINT('Ctrl Pts',(1.38245545626202,-4.8781013539643,40.));
#35967=CARTESIAN_POINT('Ctrl Pts',(1.34788667776073,-4.88981384734562,40.));
#35968=CARTESIAN_POINT('Ctrl Pts',(1.31317395760249,-4.90115117757556,40.));
#35969=CARTESIAN_POINT('Ctrl Pts',(-1.31303618635638,-4.90075024188325,
40.));
#35970=CARTESIAN_POINT('Ctrl Pts',(-1.45437915259461,-4.85452838596849,
40.));
#35971=CARTESIAN_POINT('Ctrl Pts',(-1.59345673045457,-4.80203124199391,
40.));
#35972=CARTESIAN_POINT('Ctrl Pts',(-1.72991111250498,-4.74351762389719,
40.));
#35973=CARTESIAN_POINT('Ctrl Pts',(-1.86679415923463,-4.68482018816886,
40.));
#35974=CARTESIAN_POINT('Ctrl Pts',(-2.001038164382,-4.62006797676633,40.));
#35975=CARTESIAN_POINT('Ctrl Pts',(-2.1322557155067,-4.54947707893507,40.));
#35976=CARTESIAN_POINT('Ctrl Pts',(-2.19315308373731,-4.5167162183481,40.));
#35977=CARTESIAN_POINT('Ctrl Pts',(-2.25339817251141,-4.48269720490963,
40.));
#35978=CARTESIAN_POINT('Ctrl Pts',(-2.31294973629581,-4.44743875160342,
40.));
#35979=CARTESIAN_POINT('Ctrl Pts',(-2.33562884151057,-4.43401122558351,
40.));
#35980=CARTESIAN_POINT('Ctrl Pts',(-2.35820900730168,-4.42040290103079,
40.));
#35981=CARTESIAN_POINT('Ctrl Pts',(-2.38068262652232,-4.40661797963936,
40.));
#35982=CARTESIAN_POINT('Ctrl Pts',(-2.50650561756839,-4.32944037759069,
40.));
#35983=CARTESIAN_POINT('Ctrl Pts',(-2.62877991395688,-4.24686153480494,
40.));
#35984=CARTESIAN_POINT('Ctrl Pts',(-2.74713717330506,-4.15910670751388,
40.));
#35985=CARTESIAN_POINT('Ctrl Pts',(-2.86467013316358,-4.07196304898213,
40.));
#35986=CARTESIAN_POINT('Ctrl Pts',(-2.97834099898066,-3.97971476207056,
40.));
#35987=CARTESIAN_POINT('Ctrl Pts',(-3.08775357309594,-3.88254556003572,
40.));
#35988=CARTESIAN_POINT('Ctrl Pts',(-3.14513584653695,-3.8315844180802,40.));
#35989=CARTESIAN_POINT('Ctrl Pts',(-3.2013462077245,-3.77926917964798,40.));
#35990=CARTESIAN_POINT('Ctrl Pts',(-3.25632275100474,-3.72562292402786,
40.));
#35991=CARTESIAN_POINT('Ctrl Pts',(-3.27574922848208,-3.70666651617886,
40.));
#35992=CARTESIAN_POINT('Ctrl Pts',(-3.29502416873062,-3.6875411953518,40.));
#35993=CARTESIAN_POINT('Ctrl Pts',(-3.31412620910246,-3.66826697432299,
40.));
#35994=CARTESIAN_POINT('Ctrl Pts',(-3.34404060290358,-3.63808294021764,
40.));
#35995=CARTESIAN_POINT('Ctrl Pts',(-3.37353997543889,-3.60752519082335,
40.));
#35996=CARTESIAN_POINT('Ctrl Pts',(-3.40261591802411,-3.57659932769541,
40.));
#35997=CARTESIAN_POINT('Ctrl Pts',(-3.50164274205642,-3.47127204562902,
40.));
#35998=CARTESIAN_POINT('Ctrl Pts',(-3.59576101414824,-3.36167756876611,
40.));
#35999=CARTESIAN_POINT('Ctrl Pts',(-3.68480291336662,-3.24822038520781,
40.));
#36000=CARTESIAN_POINT('Ctrl Pts',(-3.77450749603108,-3.13391881043548,
40.));
#36001=CARTESIAN_POINT('Ctrl Pts',(-3.85906025603562,-3.01569612122462,
40.));
#36002=CARTESIAN_POINT('Ctrl Pts',(-3.93824649098464,-2.893935566612,40.));
#36003=CARTESIAN_POINT('Ctrl Pts',(-4.01670520549023,-2.7732936823433,40.));
#36004=CARTESIAN_POINT('Ctrl Pts',(-4.08989581732523,-2.64917791019356,
40.));
#36005=CARTESIAN_POINT('Ctrl Pts',(-4.15756259897637,-2.52194215997081,
40.));
#36006=CARTESIAN_POINT('Ctrl Pts',(-4.20177691057784,-2.43880474793609,
40.));
#36007=CARTESIAN_POINT('Ctrl Pts',(-4.24363187369716,-2.35433490941293,
40.));
#36008=CARTESIAN_POINT('Ctrl Pts',(-4.2830443332661,-2.26862918510464,40.));
#36009=CARTESIAN_POINT('Ctrl Pts',(-4.30136127527663,-2.22879744663171,
40.));
#36010=CARTESIAN_POINT('Ctrl Pts',(-4.31915051766851,-2.18869875186795,
40.));
#36011=CARTESIAN_POINT('Ctrl Pts',(-4.33640298127534,-2.14834275431588,
40.));
#36012=CARTESIAN_POINT('Ctrl Pts',(-4.3436590160159,-2.13136984384344,40.));
#36013=CARTESIAN_POINT('Ctrl Pts',(-4.35081962128211,-2.11435240712678,
40.));
#36014=CARTESIAN_POINT('Ctrl Pts',(-4.35787943356684,-2.09730289812436,
40.));
#36015=CARTESIAN_POINT('Ctrl Pts',(-4.41262610226673,-1.96508920982698,
40.));
#36016=CARTESIAN_POINT('Ctrl Pts',(-4.46139597719794,-1.83076168016892,
40.));
#36017=CARTESIAN_POINT('Ctrl Pts',(-4.50399603348697,-1.69468832090704,
40.));
#36018=CARTESIAN_POINT('Ctrl Pts',(-4.527154798591,-1.62071445235899,40.));
#36019=CARTESIAN_POINT('Ctrl Pts',(-4.54848933959424,-1.54622425456777,
40.));
#36020=CARTESIAN_POINT('Ctrl Pts',(-4.56796247846724,-1.47127487515815,
40.));
#36021=CARTESIAN_POINT('Ctrl Pts',(-4.60386684913915,-1.33308398988268,
40.));
#36022=CARTESIAN_POINT('Ctrl Pts',(-4.633446346586,-1.19333212031901,40.));
#36023=CARTESIAN_POINT('Ctrl Pts',(-4.65669710227076,-1.05245525970538,
40.));
#36024=CARTESIAN_POINT('Ctrl Pts',(-4.67988218362711,-0.911976321350021,
40.));
#36025=CARTESIAN_POINT('Ctrl Pts',(-4.6967741641367,-0.770377936579903,
40.));
#36026=CARTESIAN_POINT('Ctrl Pts',(-4.70731777033656,-0.628096038990404,
40.));
#36027=CARTESIAN_POINT('Ctrl Pts',(-4.71196239382317,-0.565418637090442,
40.));
#36028=CARTESIAN_POINT('Ctrl Pts',(-4.71537442348699,-0.502608716141042,
40.));
#36029=CARTESIAN_POINT('Ctrl Pts',(-4.71754599609844,-0.439704378705418,
40.));
#36030=CARTESIAN_POINT('Ctrl Pts',(-4.71847271903558,-0.412859827415833,
40.));
#36031=CARTESIAN_POINT('Ctrl Pts',(-4.71917350957111,-0.385998089715844,
40.));
#36032=CARTESIAN_POINT('Ctrl Pts',(-4.71964765055488,-0.359122168611144,
40.));
#36033=CARTESIAN_POINT('Ctrl Pts',(-4.72007766112019,-0.334747709487924,
40.));
#36034=CARTESIAN_POINT('Ctrl Pts',(-4.72032117948226,-0.310357499793734,
40.));
#36035=CARTESIAN_POINT('Ctrl Pts',(-4.72037779701569,-0.28598141917232,
40.));
#36036=CARTESIAN_POINT('Ctrl Pts',(-4.72070503729545,-0.145091575346323,
40.));
#36037=CARTESIAN_POINT('Ctrl Pts',(-4.71479792201471,-0.00450394063596596,
40.));
#36038=CARTESIAN_POINT('Ctrl Pts',(-4.7026779767235,0.135364936808135,40.));
#36039=CARTESIAN_POINT('Ctrl Pts',(-4.6906385436001,0.274304672555548,40.));
#36040=CARTESIAN_POINT('Ctrl Pts',(-4.67246842821977,0.412535934949348,
40.));
#36041=CARTESIAN_POINT('Ctrl Pts',(-4.64813815685378,0.549644620304502,
40.));
#36042=CARTESIAN_POINT('Ctrl Pts',(-4.62922788638654,0.656209906177027,
40.));
#36043=CARTESIAN_POINT('Ctrl Pts',(-4.60659531784607,0.762097046731738,
40.));
#36044=CARTESIAN_POINT('Ctrl Pts',(-4.58020591978812,0.867104757427845,
40.));
#36045=CARTESIAN_POINT('Ctrl Pts',(-4.54608550784896,1.00287543085781,40.));
#36046=CARTESIAN_POINT('Ctrl Pts',(-4.5056856677851,1.13717725960422,40.));
#36047=CARTESIAN_POINT('Ctrl Pts',(-4.45916773762384,1.26960241773677,40.));
#36048=CARTESIAN_POINT('Ctrl Pts',(-4.44595800567878,1.30720729043101,40.));
#36049=CARTESIAN_POINT('Ctrl Pts',(-4.43225465907289,1.34466063579127,40.));
#36050=CARTESIAN_POINT('Ctrl Pts',(-4.41806080497834,1.381952618119,40.));
#36051=CARTESIAN_POINT('Ctrl Pts',(-4.41034395548629,1.40222735202608,40.));
#36052=CARTESIAN_POINT('Ctrl Pts',(-4.40248211604979,1.42245438558641,40.));
#36053=CARTESIAN_POINT('Ctrl Pts',(-4.39447575604619,1.44263210700853,40.));
#36054=CARTESIAN_POINT('Ctrl Pts',(-4.38774337392406,1.45959913458491,40.));
#36055=CARTESIAN_POINT('Ctrl Pts',(-4.38091020364865,1.47652766568619,40.));
#36056=CARTESIAN_POINT('Ctrl Pts',(-4.37398035764513,1.49340802308437,40.));
#36057=CARTESIAN_POINT('Ctrl Pts',(-4.32139777601335,1.62149352028206,40.));
#36058=CARTESIAN_POINT('Ctrl Pts',(-4.26319329324451,1.74695839038908,40.));
#36059=CARTESIAN_POINT('Ctrl Pts',(-4.19959993118347,1.86944841739778,40.));
#36060=CARTESIAN_POINT('Ctrl Pts',(-4.13606105752427,1.99183349185173,40.));
#36061=CARTESIAN_POINT('Ctrl Pts',(-4.06714208355231,2.1112494937512,40.));
#36062=CARTESIAN_POINT('Ctrl Pts',(-3.99303011697524,2.22731770598438,40.));
#36063=CARTESIAN_POINT('Ctrl Pts',(-3.9202059518248,2.34136906700981,40.));
#36064=CARTESIAN_POINT('Ctrl Pts',(-3.84236718991447,2.45218850722107,40.));
#36065=CARTESIAN_POINT('Ctrl Pts',(-3.75965485123955,2.55938335127685,40.));
#36066=CARTESIAN_POINT('Ctrl Pts',(-3.67819754057762,2.66495168429094,40.));
#36067=CARTESIAN_POINT('Ctrl Pts',(-3.59201299654429,2.76700506575445,40.));
#36068=CARTESIAN_POINT('Ctrl Pts',(-3.50120707213067,2.86512829543056,40.));
#36069=CARTESIAN_POINT('Ctrl Pts',(-3.47910751146495,2.88900867857677,40.));
#36070=CARTESIAN_POINT('Ctrl Pts',(-3.45673410716774,2.91265607078183,40.));
#36071=CARTESIAN_POINT('Ctrl Pts',(-3.43409108914464,2.93606647242288,40.));
#36072=CARTESIAN_POINT('Origin',(0.,0.,-2.20833684463713));
#36073=CARTESIAN_POINT('Ctrl Pts',(5.07346622253938,0.000127574377019116,
0.291663155362924));
#36074=CARTESIAN_POINT('Ctrl Pts',(5.07369228799229,0.238078384188188,0.299127094674674));
#36075=CARTESIAN_POINT('Ctrl Pts',(4.99899491470862,1.31934885093053,0.333048330670892));
#36076=CARTESIAN_POINT('Ctrl Pts',(4.24398161873799,3.15587819282154,0.393426863351577));
#36077=CARTESIAN_POINT('Ctrl Pts',(2.21764149317933,4.80135391043019,0.472798753404982));
#36078=CARTESIAN_POINT('Ctrl Pts',(-0.348912918530393,5.27723479734493,
0.552170643458385));
#36079=CARTESIAN_POINT('Ctrl Pts',(-2.83047200092439,4.46759066254957,0.631542533511789));
#36080=CARTESIAN_POINT('Ctrl Pts',(-4.62253485344812,2.56965255248809,0.710914423565193));
#36081=CARTESIAN_POINT('Ctrl Pts',(-5.28855819093304,0.045752121671659,
0.790286313618596));
#36082=CARTESIAN_POINT('Ctrl Pts',(-4.66630059499956,-2.48929308216644,
0.869658203672));
#36083=CARTESIAN_POINT('Ctrl Pts',(-2.90734243084918,-4.4179521825598,0.949030093725403));
#36084=CARTESIAN_POINT('Ctrl Pts',(-0.440162123945536,-5.27040781417518,
1.02840198377881));
#36085=CARTESIAN_POINT('Ctrl Pts',(2.1342407222512,-4.83900381899044,1.10777387383221));
#36086=CARTESIAN_POINT('Ctrl Pts',(4.18874724188064,-3.228829177505,1.18714576388562));
#36087=CARTESIAN_POINT('Ctrl Pts',(4.9873788651986,-1.37792482956251,1.24844219106252));
#36088=CARTESIAN_POINT('Ctrl Pts',(5.07361295102991,-0.267343660459586,
1.28328132155495));
#36089=CARTESIAN_POINT('Ctrl Pts',(5.07338480805012,-0.000117445791331001,
1.29166315536292));
#36090=CARTESIAN_POINT('Ctrl Pts',(5.07327550687406,0.000108476183186372,
0.208336844637077));
#36091=CARTESIAN_POINT('Ctrl Pts',(5.07347129707779,0.316577306682802,0.218263119811455));
#36092=CARTESIAN_POINT('Ctrl Pts',(4.96661393653962,1.47641857544861,0.254646691670301));
#36093=CARTESIAN_POINT('Ctrl Pts',(4.09299916691648,3.34943642687043,0.317487560213614));
#36094=CARTESIAN_POINT('Ctrl Pts',(1.99247705733062,4.89905044646781,0.396859450267019));
#36095=CARTESIAN_POINT('Ctrl Pts',(-0.593383061700938,5.2553763257097,0.476231340320422));
#36096=CARTESIAN_POINT('Ctrl Pts',(-3.03470961035893,4.33144609848054,0.555603230373826));
#36097=CARTESIAN_POINT('Ctrl Pts',(-4.73678060915323,2.35241593705463,0.634975120427228));
#36098=CARTESIAN_POINT('Ctrl Pts',(-5.28498604656423,-0.199673823356779,
0.714347010480634));
#36099=CARTESIAN_POINT('Ctrl Pts',(-4.5457786161601,-2.703114858517,0.793718900534037));
#36100=CARTESIAN_POINT('Ctrl Pts',(-2.69923061743508,-4.5480876646044,0.87309079058744));
#36101=CARTESIAN_POINT('Ctrl Pts',(-0.195155463808127,-5.28515396379925,
0.952462680640845));
#36102=CARTESIAN_POINT('Ctrl Pts',(2.35645883694709,-4.73476973691702,1.03183457069425));
#36103=CARTESIAN_POINT('Ctrl Pts',(4.33404513553918,-3.03100540392648,1.11120646074765));
#36104=CARTESIAN_POINT('Ctrl Pts',(5.01734225874463,-1.22080114526538,1.17004055206193));
#36105=CARTESIAN_POINT('Ctrl Pts',(5.0738119846015,-0.188829126190742,1.20241734669174));
#36106=CARTESIAN_POINT('Ctrl Pts',(5.07361762168166,-0.000130982038957766,
1.20833684463708));
#36107=CARTESIAN_POINT('Ctrl Pts',(-3.43378788736187,2.93584158412999,-1.38777878078145E-15));
#36108=CARTESIAN_POINT('Ctrl Pts',(-3.92183073605352,2.36502208507736,0.0264572966844665));
#36109=CARTESIAN_POINT('Ctrl Pts',(-4.60729903172261,0.975909964327098,
0.0793718900534022));
#36110=CARTESIAN_POINT('Ctrl Pts',(-4.51258247789853,-1.34695556252418,
0.158743780106806));
#36111=CARTESIAN_POINT('Ctrl Pts',(-3.3188765366808,-3.34104229843846,0.23811567016021));
#36112=CARTESIAN_POINT('Ctrl Pts',(-1.31656588610641,-4.52159485055713,
0.317487560213613));
#36113=CARTESIAN_POINT('Ctrl Pts',(1.00638734295355,-4.60052063353559,0.396859450267017));
#36114=CARTESIAN_POINT('Ctrl Pts',(3.08422378627015,-3.55886290155616,0.476231340320421));
#36115=CARTESIAN_POINT('Ctrl Pts',(4.41073058968579,-1.65022475069956,0.555603230373823));
#36116=CARTESIAN_POINT('Ctrl Pts',(4.66280353786907,0.660378394082181,0.634975120427229));
#36117=CARTESIAN_POINT('Ctrl Pts',(3.77902238214553,2.81012864743368,0.71434701048063));
#36118=CARTESIAN_POINT('Ctrl Pts',(1.9746826426622,4.27533046137772,0.793718900534036));
#36119=CARTESIAN_POINT('Ctrl Pts',(-0.310686955552407,4.69907511544172,
0.873090790587439));
#36120=CARTESIAN_POINT('Ctrl Pts',(-2.52037308462949,3.97813341921581,0.952462680640842));
#36121=CARTESIAN_POINT('Ctrl Pts',(-4.11610234038262,2.28812831500376,1.03183457069425));
#36122=CARTESIAN_POINT('Ctrl Pts',(-4.70915794841686,0.0407396420060994,
1.11120646074765));
#36123=CARTESIAN_POINT('Ctrl Pts',(-4.15507322474362,-2.21657281259016,
1.19057835080105));
#36124=CARTESIAN_POINT('Ctrl Pts',(-2.58882179654858,-3.93393319787912,
1.26995024085446));
#36125=CARTESIAN_POINT('Ctrl Pts',(-0.391939142907391,-4.69299607822649,
1.34932213090786));
#36126=CARTESIAN_POINT('Ctrl Pts',(1.90041903637464,-4.30885554699701,1.42869402096126));
#36127=CARTESIAN_POINT('Ctrl Pts',(3.72983933538439,-2.87508731801348,1.50806591101467));
#36128=CARTESIAN_POINT('Ctrl Pts',(4.65067903319439,-0.740954194967835,
1.58743780106807));
#36129=CARTESIAN_POINT('Ctrl Pts',(4.43862360995218,1.57367373662795,1.66680969112148));
#36130=CARTESIAN_POINT('Ctrl Pts',(3.1453293014661,3.50495822568453,1.74618158117488));
#36131=CARTESIAN_POINT('Ctrl Pts',(1.08583973646247,4.58244265094549,1.82555347122828));
#36132=CARTESIAN_POINT('Ctrl Pts',(-1.2381579844814,4.54365418850119,1.90492536128169));
#36133=CARTESIAN_POINT('Ctrl Pts',(-3.26054316123182,3.39804162347539,1.98429725133509));
#36134=CARTESIAN_POINT('Ctrl Pts',(-4.48866724088482,1.42467364012815,2.0636691413885));
#36135=CARTESIAN_POINT('Ctrl Pts',(-4.62336191621359,-0.895741688344198,
2.1430410314419));
#36136=CARTESIAN_POINT('Ctrl Pts',(-3.63181586235956,-2.99795632430514,
2.2224129214953));
#36137=CARTESIAN_POINT('Ctrl Pts',(-1.75556750333933,-4.36987543548745,
2.30178481154871));
#36138=CARTESIAN_POINT('Ctrl Pts',(0.548333213620371,-4.67730256316232,
2.38115670160211));
#36139=CARTESIAN_POINT('Ctrl Pts',(2.71866117345249,-3.84534913947276,2.46052859165552));
#36140=CARTESIAN_POINT('Ctrl Pts',(4.22672928908848,-2.07667717694978,2.53990048170891));
#36141=CARTESIAN_POINT('Ctrl Pts',(4.7051755056078,0.19786874923449,2.61927237176232));
#36142=CARTESIAN_POINT('Ctrl Pts',(4.03745138369107,2.42421428607854,2.69864426181572));
#36143=CARTESIAN_POINT('Ctrl Pts',(2.38621304145389,4.06002658874208,2.77801615186912));
#36144=CARTESIAN_POINT('Ctrl Pts',(0.153698484111727,4.70682540110399,2.85738804192253));
#36145=CARTESIAN_POINT('Ctrl Pts',(-2.11625668375435,4.20705196413855,2.93675993197593));
#36146=CARTESIAN_POINT('Ctrl Pts',(-3.87069640771252,2.68244998086038,3.01613182202934));
#36147=CARTESIAN_POINT('Ctrl Pts',(-4.68224305439313,0.504409119747013,
3.09550371208274));
#36148=CARTESIAN_POINT('Ctrl Pts',(-4.35320565699276,-1.79650468644612,
3.17487560213615));
#36149=CARTESIAN_POINT('Ctrl Pts',(-2.96373699720624,-3.65979392751662,
3.25424749218954));
#36150=CARTESIAN_POINT('Ctrl Pts',(-0.852308565020845,-4.63156546866054,
3.33361938224295));
#36151=CARTESIAN_POINT('Ctrl Pts',(1.46674034705061,-4.47509791343502,3.41299127229636));
#36152=CARTESIAN_POINT('Ctrl Pts',(3.42849455715522,-3.22850641195795,3.49236316234976));
#36153=CARTESIAN_POINT('Ctrl Pts',(4.55507508198081,-1.19545789470566,3.57173505240317));
#36154=CARTESIAN_POINT('Ctrl Pts',(4.57204939932356,1.12880151959577,3.65110694245656));
#36155=CARTESIAN_POINT('Ctrl Pts',(3.47528260305076,3.17808738228345,3.73047883250997));
#36156=CARTESIAN_POINT('Ctrl Pts',(1.53194465708238,4.45319819322398,3.80985072256337));
#36157=CARTESIAN_POINT('Ctrl Pts',(-0.784571616449287,4.64351978128216,
3.88922261261678));
#36158=CARTESIAN_POINT('Ctrl Pts',(-2.90996798083373,3.70269022887672,3.96859450267018));
#36159=CARTESIAN_POINT('Ctrl Pts',(-4.32650258619195,1.85989353248269,4.04796639272359));
#36160=CARTESIAN_POINT('Ctrl Pts',(-4.68911073810485,-0.4359691116196,4.12733828277699));
#36161=CARTESIAN_POINT('Ctrl Pts',(-3.90946189338598,-2.62563064513263,
4.2067101728304));
#36162=CARTESIAN_POINT('Ctrl Pts',(-2.17747678488539,-4.17569436522619,
4.28608206288379));
#36163=CARTESIAN_POINT('Ctrl Pts',(0.0849368486501527,-4.70856818069336,
4.3654539529372));
#36164=CARTESIAN_POINT('Ctrl Pts',(2.32666005385904,-4.09444520958252,4.4448258429906));
#36165=CARTESIAN_POINT('Ctrl Pts',(4.00161401992256,-2.48292444831813,4.52419773304401));
#36166=CARTESIAN_POINT('Ctrl Pts',(4.70178366815532,-0.266568787303479,
4.60356962309741));
#36167=CARTESIAN_POINT('Ctrl Pts',(4.25660922204708,2.0147224402583,4.68294151315081));
#36168=CARTESIAN_POINT('Ctrl Pts',(2.77453419129287,3.80523174088563,4.76231340320422));
#36169=CARTESIAN_POINT('Ctrl Pts',(0.616588772866969,4.6687950121708,4.84168529325762));
#36170=CARTESIAN_POINT('Ctrl Pts',(-1.69155630583321,4.39505015269366,4.92105718331103));
#36171=CARTESIAN_POINT('Ctrl Pts',(-3.5876420126288,3.05068080429882,5.00042907336443));
#36172=CARTESIAN_POINT('Ctrl Pts',(-4.60978606625892,0.96317236454425,5.07980096341783));
#36173=CARTESIAN_POINT('Ctrl Pts',(-4.50899643773674,-1.35896273126747,
5.15917285347124));
#36174=CARTESIAN_POINT('Ctrl Pts',(-3.30982525747623,-3.3500575137554,5.23854474352463));
#36175=CARTESIAN_POINT('Ctrl Pts',(-1.30438797066844,-4.52508570111905,
5.31791663357805));
#36176=CARTESIAN_POINT('Ctrl Pts',(1.01879533858038,-4.5978130277974,5.39728852363144));
#36177=CARTESIAN_POINT('Ctrl Pts',(3.09380235841625,-3.55052327799082,5.47666041368486));
#36178=CARTESIAN_POINT('Ctrl Pts',(4.41516597175728,-1.63833391661564,5.55603230373825));
#36179=CARTESIAN_POINT('Ctrl Pts',(4.66100492718236,0.672949960456484,5.63540419379167));
#36180=CARTESIAN_POINT('Ctrl Pts',(3.77143339930522,2.82030471671088,5.71477608384506));
#36181=CARTESIAN_POINT('Ctrl Pts',(1.96314904328358,4.28063948661312,5.79414797389847));
#36182=CARTESIAN_POINT('Ctrl Pts',(-0.323354074325263,4.69821995261119,
5.87351986395187));
#36183=CARTESIAN_POINT('Ctrl Pts',(-2.53108885516056,3.97132443748664,5.95289175400528));
#36184=CARTESIAN_POINT('Ctrl Pts',(-4.1222559933489,2.2770230797679,6.03226364405868));
#36185=CARTESIAN_POINT('Ctrl Pts',(-4.70925069601632,0.0280439399227974,
6.11163553411208));
#36186=CARTESIAN_POINT('Ctrl Pts',(-4.14908235288379,-2.22776664161329,
6.19100742416549));
#36187=CARTESIAN_POINT('Ctrl Pts',(-2.57820673242676,-3.94089820033021,
6.27037931421889));
#36188=CARTESIAN_POINT('Ctrl Pts',(-0.37928565871439,-4.6940356804769,6.34975120427229));
#36189=CARTESIAN_POINT('Ctrl Pts',(1.91202856192625,-4.30371645893114,6.42912309432569));
#36190=CARTESIAN_POINT('Ctrl Pts',(3.73757685708508,-2.86502143410457,6.5084949843791));
#36191=CARTESIAN_POINT('Ctrl Pts',(4.65265970284404,-0.728413529547492,
6.58786687443251));
#36192=CARTESIAN_POINT('Ctrl Pts',(4.43436494347775,1.58563429849135,6.6672387644859));
#36193=CARTESIAN_POINT('Ctrl Pts',(3.13586869918061,3.51342512115968,6.74661065453932));
#36194=CARTESIAN_POINT('Ctrl Pts',(1.07348178089069,4.58535336114812,6.8259825445927));
#36195=CARTESIAN_POINT('Ctrl Pts',(-1.25040292311256,4.54029967186839,6.90535443464612));
#36196=CARTESIAN_POINT('Ctrl Pts',(-3.26969224276554,3.38923903230437,6.98472632469952));
#36197=CARTESIAN_POINT('Ctrl Pts',(-4.49249176942184,1.41256726642436,7.06409821475293));
#36198=CARTESIAN_POINT('Ctrl Pts',(-4.62093024500886,-0.908202758892002,
7.14347010480633));
#36199=CARTESIAN_POINT('Ctrl Pts',(-3.62372034116731,-3.00773660241498,
7.22284199485974));
#36200=CARTESIAN_POINT('Ctrl Pts',(-1.74378018318635,-4.37459246710173,
7.30221388491313));
#36201=CARTESIAN_POINT('Ctrl Pts',(0.560940967626854,-4.67580728979868,
7.38158577496654));
#36202=CARTESIAN_POINT('Ctrl Pts',(2.72901814034792,-3.83800580642455,7.46095766501994));
#36203=CARTESIAN_POINT('Ctrl Pts',(4.23231253465944,-2.06527460388716,7.54032955507336));
#36204=CARTESIAN_POINT('Ctrl Pts',(4.70462496359279,0.210552920749357,7.61970144512673));
#36205=CARTESIAN_POINT('Ctrl Pts',(4.03090116490568,2.4350902199423,7.69907333518017));
#36206=CARTESIAN_POINT('Ctrl Pts',(2.37525876469593,4.06644493153808,7.77844522523354));
#36207=CARTESIAN_POINT('Ctrl Pts',(0.141008586952364,4.70722265873438,7.85781711528697));
#36208=CARTESIAN_POINT('Ctrl Pts',(-2.1275909704556,4.2013313655236,7.93718900534037));
#36209=CARTESIAN_POINT('Ctrl Pts',(-3.87791407680332,2.67200505116051,8.01656089539376));
#36210=CARTESIAN_POINT('Ctrl Pts',(-4.68358589765895,0.491784220717585,
8.09593278544718));
#36211=CARTESIAN_POINT('Ctrl Pts',(-4.3483465607864,-1.80823415734624,8.17530467550056));
#36212=CARTESIAN_POINT('Ctrl Pts',(-2.95385962660815,-3.66777069713892,
8.25467656555399));
#36213=CARTESIAN_POINT('Ctrl Pts',(-0.839819025645543,-4.63384641358131,
8.33404845560737));
#36214=CARTESIAN_POINT('Ctrl Pts',(1.47879963105641,-4.47112740052035,8.41342034566079));
#36215=CARTESIAN_POINT('Ctrl Pts',(3.43718597090052,-3.21925164936531,8.49279223571418));
#36216=CARTESIAN_POINT('Ctrl Pts',(4.55828141631537,-1.1831733221175,8.57216412576761));
#36217=CARTESIAN_POINT('Ctrl Pts',(4.56898959830056,1.1411234074884,8.65153601582098));
#36218=CARTESIAN_POINT('Ctrl Pts',(3.46670202742665,3.18744500086393,8.73090790587441));
#36219=CARTESIAN_POINT('Ctrl Pts',(1.51993351608642,4.45731204731885,8.8102797959278));
#36220=CARTESIAN_POINT('Ctrl Pts',(-0.797087435456723,4.64138774513978,
8.88965168598121));
#36221=CARTESIAN_POINT('Ctrl Pts',(-2.91993965204571,3.69483166178214,8.96902357603462));
#36222=CARTESIAN_POINT('Ctrl Pts',(-4.33150103257314,1.84822276398555,9.04839546608801));
#36223=CARTESIAN_POINT('Ctrl Pts',(-4.68791834918067,-0.448609108146216,
9.12776735614143));
#36224=CARTESIAN_POINT('Ctrl Pts',(-3.90236913245906,-2.63616079451299,
9.20713924619481));
#36225=CARTESIAN_POINT('Ctrl Pts',(-2.16621143281798,-4.18154954637933,
9.28651113624823));
#36226=CARTESIAN_POINT('Ctrl Pts',(0.0976305770298679,-4.70832208445062,
9.36588302630162));
#36227=CARTESIAN_POINT('Ctrl Pts',(2.33768999441487,-4.08815778444389,9.44525491635505));
#36228=CARTESIAN_POINT('Ctrl Pts',(4.00829330354943,-2.47212729713041,9.52462680640842));
#36229=CARTESIAN_POINT('Ctrl Pts',(4.70248523614611,-0.253892072196923,
9.60399869646185));
#36230=CARTESIAN_POINT('Ctrl Pts',(4.25116217399211,2.02619069954319,9.68337058651524));
#36231=CARTESIAN_POINT('Ctrl Pts',(2.76426541604147,3.81269790177162,9.76274247656865));
#36232=CARTESIAN_POINT('Ctrl Pts',(0.603999721340871,4.67044033439211,9.84211436662206));
#36233=CARTESIAN_POINT('Ctrl Pts',(-1.70339896854767,4.39047383939904,9.92148625667545));
#36234=CARTESIAN_POINT('Ctrl Pts',(-3.59585344010767,3.04099763527736,10.0008581467289));
#36235=CARTESIAN_POINT('Ctrl Pts',(-4.61236597294403,0.95074113833618,10.0802300367823));
#36236=CARTESIAN_POINT('Ctrl Pts',(-4.5053163640701,-1.37111379547384,10.1596019268357));
#36237=CARTESIAN_POINT('Ctrl Pts',(-3.30078166125737,-3.35896844361534,
10.2389738168891));
#36238=CARTESIAN_POINT('Ctrl Pts',(-1.29218385191862,-4.5285858138427,10.3183457069425));
#36239=CARTESIAN_POINT('Ctrl Pts',(1.03118708354706,-4.59504970367267,10.3977175969959));
#36240=CARTESIAN_POINT('Ctrl Pts',(3.1033631279546,-3.54216965665798,10.4770894870493));
#36241=CARTESIAN_POINT('Ctrl Pts',(4.41956678357015,-1.62642492174092,10.5564613771027));
#36242=CARTESIAN_POINT('Ctrl Pts',(4.65917375325315,0.68551332408169,10.6358332671561));
#36243=CARTESIAN_POINT('Ctrl Pts',(3.76381630954987,2.83046204151602,10.7152051572095));
#36244=CARTESIAN_POINT('Ctrl Pts',(1.95160154390631,4.28591647075852,10.7945770472629));
#36245=CARTESIAN_POINT('Ctrl Pts',(-0.336019038036085,4.69733113443942,
10.8739489373163));
#36246=CARTESIAN_POINT('Ctrl Pts',(-2.54178612607839,3.96448633113698,10.9533208273697));
#36247=CARTESIAN_POINT('Ctrl Pts',(-4.12837973995617,2.26590143281123,11.0326927174231));
#36248=CARTESIAN_POINT('Ctrl Pts',(-4.70930918719419,0.0153479609404256,
11.1120646074765));
#36249=CARTESIAN_POINT('Ctrl Pts',(-4.14306134031078,-2.23894424024334,
11.1914364975299));
#36250=CARTESIAN_POINT('Ctrl Pts',(-2.5675729214384,-3.94783458032284,11.2708083875833));
#36251=CARTESIAN_POINT('Ctrl Pts',(-0.366629422129896,-4.69504115501934,
11.3501802776367));
#36252=CARTESIAN_POINT('Ctrl Pts',(1.92362419288899,-4.29854609665044,11.4295521676901));
#36253=CARTESIAN_POINT('Ctrl Pts',(3.74528721239005,-2.85493472380791,11.5089240577435));
#36254=CARTESIAN_POINT('Ctrl Pts',(4.65460655700554,-0.715867571536574,
11.5882959477969));
#36255=CARTESIAN_POINT('Ctrl Pts',(4.43007404713131,1.59758333661508,11.6676678378504));
#36256=CARTESIAN_POINT('Ctrl Pts',(3.12638530517848,3.52186648015801,11.7470397279037));
#36257=CARTESIAN_POINT('Ctrl Pts',(1.06111602302068,4.5882307446537,11.8264116179572));
#36258=CARTESIAN_POINT('Ctrl Pts',(-1.26263877360451,4.53691215562823,11.9057835080105));
#36259=CARTESIAN_POINT('Ctrl Pts',(-3.27881755978316,3.38041180777642,11.985155398064));
#36260=CARTESIAN_POINT('Ctrl Pts',(-4.49628364593817,1.40045062596491,12.0645272881173));
#36261=CARTESIAN_POINT('Ctrl Pts',(-4.6184649882977,-0.920657228486762,
12.1438991781708));
#36262=CARTESIAN_POINT('Ctrl Pts',(-3.61559848230676,-3.01749501991928,
12.2232710682242));
#36263=CARTESIAN_POINT('Ctrl Pts',(-1.7319801890174,-4.37927770361138,12.3026429582776));
#36264=CARTESIAN_POINT('Ctrl Pts',(0.573544644643477,-4.67427803207056,
12.382014848331));
#36265=CARTESIAN_POINT('Ctrl Pts',(2.73935527238874,-3.83063457825627,12.4613867383844));
#36266=CARTESIAN_POINT('Ctrl Pts',(4.23786501924016,-2.05385702014458,12.5407586284378));
#36267=CARTESIAN_POINT('Ctrl Pts',(4.7040402277598,0.22323556193892,12.6201305184912));
#36268=CARTESIAN_POINT('Ctrl Pts',(4.02432164901358,2.44594845525766,12.6995024085446));
#36269=CARTESIAN_POINT('Ctrl Pts',(2.3642872242525,4.0728337188907,12.778874298598));
#36270=CARTESIAN_POINT('Ctrl Pts',(0.12831766492455,4.70758570366646,12.8582461886514));
#36271=CARTESIAN_POINT('Ctrl Pts',(-2.13890979355269,4.19558023109331,12.9376180787048));
#36272=CARTESIAN_POINT('Ctrl Pts',(-3.88510356071705,2.66154070098513,13.0169899687582));
#36273=CARTESIAN_POINT('Ctrl Pts',(-4.68489470002156,0.479155747337376,
13.0963618588116));
#36274=CARTESIAN_POINT('Ctrl Pts',(-4.34345586023936,-1.81995048576848,
13.175733748865));
#36275=CARTESIAN_POINT('Ctrl Pts',(-2.94396078697933,-3.67572080893321,
13.2551056389184));
#36276=CARTESIAN_POINT('Ctrl Pts',(-0.827323382357809,-4.63609367911183,
13.3344775289718));
#36277=CARTESIAN_POINT('Ctrl Pts',(1.49084816695683,-4.4671243908781,13.4138494190252));
#36278=CARTESIAN_POINT('Ctrl Pts',(3.44585240273723,-3.2099734888386,13.4932213090786));
#36279=CARTESIAN_POINT('Ctrl Pts',(4.56145462047577,-1.17088015007382,13.572593199132));
#36280=CARTESIAN_POINT('Ctrl Pts',(4.56589658927495,1.15343700154968,13.6519650891854));
#36281=CARTESIAN_POINT('Ctrl Pts',(3.45809625536746,3.19677945268519,13.7313369792388));
#36282=CARTESIAN_POINT('Ctrl Pts',(1.50791132801865,4.4613935050979,13.8107088692922));
#36283=CARTESIAN_POINT('Ctrl Pts',(-0.809597461130395,4.63922197479575,
13.8900807593457));
#36284=CARTESIAN_POINT('Ctrl Pts',(-2.92989010076163,3.68694624017703,13.969452649399));
#36285=CARTESIAN_POINT('Ctrl Pts',(-4.33646799704908,1.83653856236827,14.0488245394525));
#36286=CARTESIAN_POINT('Ctrl Pts',(-4.68669188786449,-0.461245844124263,
14.1281964295058));
#36287=CARTESIAN_POINT('Ctrl Pts',(-3.8952480086126,-2.64667178393849,14.2075683195593));
#36288=CARTESIAN_POINT('Ctrl Pts',(-2.15493033644793,-4.1873743354939,14.2869402096127));
#36289=CARTESIAN_POINT('Ctrl Pts',(0.110323595818042,-4.70804176751889,
14.3663120996661));
#36290=CARTESIAN_POINT('Ctrl Pts',(2.34870294433987,-4.08184064604999,14.4456839897195));
#36291=CARTESIAN_POINT('Ctrl Pts',(4.01494345438633,-2.46131217820434,14.5250558797729));
#36292=CARTESIAN_POINT('Ctrl Pts',(4.70315262587088,-0.241213511770193,
14.6044277698263));
#36293=CARTESIAN_POINT('Ctrl Pts',(4.24568422794502,2.03764423221413,14.6837996598797));
#36294=CARTESIAN_POINT('Ctrl Pts',(2.7539765497544,3.82013635148006,14.7631715499331));
#36295=CARTESIAN_POINT('Ctrl Pts',(0.591406279867313,4.67205171125386,14.8425434399865));
#36296=CARTESIAN_POINT('Ctrl Pts',(-1.71522925073988,4.38586561557727,14.9219153300399));
#36297=CARTESIAN_POINT('Ctrl Pts',(-3.60403873246238,3.0312923638949,15.0012872200933));
#36298=CARTESIAN_POINT('Ctrl Pts',(-4.61491235636145,0.938303002019602,
15.0806591101467));
#36299=CARTESIAN_POINT('Ctrl Pts',(-4.50160354518612,-1.38325489424921,
15.1600310002001));
#36300=CARTESIAN_POINT('Ctrl Pts',(-3.29171407453388,-3.36785496006171,
15.2394028902535));
#36301=CARTESIAN_POINT('Ctrl Pts',(-1.27997034141067,-4.53205301222367,
15.3187747803069));
#36302=CARTESIAN_POINT('Ctrl Pts',(1.04357133371383,-4.59225298213712,15.3981466703603));
#36303=CARTESIAN_POINT('Ctrl Pts',(3.11290134185163,-3.53379029038156,15.4775185604137));
#36304=CARTESIAN_POINT('Ctrl Pts',(4.42393547340459,-1.6145041058012,15.5568904504671));
#36305=CARTESIAN_POINT('Ctrl Pts',(4.65730871585136,0.69807170530811,15.6362623405205));
#36306=CARTESIAN_POINT('Ctrl Pts',(3.75617186389461,2.84059879415993,15.7156342305739));
#36307=CARTESIAN_POINT('Ctrl Pts',(1.94003986003872,4.2911623043131,15.7950061206273));
#36308=CARTESIAN_POINT('Ctrl Pts',(-0.348681559517582,4.69640817546235,
15.8743780106807));
#36309=CARTESIAN_POINT('Ctrl Pts',(-2.55246492296822,3.95761941039193,15.9537499007341));
#36310=CARTESIAN_POINT('Ctrl Pts',(-4.13447348097045,2.25476331699244,16.0331217907876));
#36311=CARTESIAN_POINT('Ctrl Pts',(-4.70933345050753,0.00265187040668795,
16.1124936808409));
#36312=CARTESIAN_POINT('Ctrl Pts',(-4.13701021543854,-2.25010556593871,
16.1918655708943));
#36313=CARTESIAN_POINT('Ctrl Pts',(-2.55692044899651,-3.95474226694862,
16.2712374609477));
#36314=CARTESIAN_POINT('Ctrl Pts',(-0.353970520843347,-4.69601250539775,
16.3506093510012));
#36315=CARTESIAN_POINT('Ctrl Pts',(1.93520584271894,-4.29334449198998,16.4299812410546));
#36316=CARTESIAN_POINT('Ctrl Pts',(3.75297034643966,-2.8448272634702,16.509353131108));
#36317=CARTESIAN_POINT('Ctrl Pts',(4.65651958094123,-0.703316410525392,
16.5887250211614));
#36318=CARTESIAN_POINT('Ctrl Pts',(4.42575095234045,1.60952076333056,16.6680969112148));
#36319=CARTESIAN_POINT('Ctrl Pts',(3.11687918839165,3.53028224171774,16.7474688012682));
#36320=CARTESIAN_POINT('Ctrl Pts',(1.04874255247428,4.59107478042509,16.8268406913216));
#36321=CARTESIAN_POINT('Ctrl Pts',(-1.27486544641699,4.53349166431028,16.906212581375));
#36322=CARTESIAN_POINT('Ctrl Pts',(-3.28791904717816,3.37156001439364,16.9855844714284));
#36323=CARTESIAN_POINT('Ctrl Pts',(-4.50004284053898,1.38832380607291,17.0649563614818));
#36324=CARTESIAN_POINT('Ctrl Pts',(-4.61596616842608,-0.933105005158158,
17.1443282515352));
#36325=CARTESIAN_POINT('Ctrl Pts',(-3.60745033643721,-3.02723150865552,
17.2237001415886));
#36326=CARTESIAN_POINT('Ctrl Pts',(-1.72016762240852,-4.3839311057331,17.303072031642));
#36327=CARTESIAN_POINT('Ctrl Pts',(0.586144182924747,-4.67271481097615,
17.3824439216954));
#36328=CARTESIAN_POINT('Ctrl Pts',(2.74967243806105,-3.82323548987727,17.4618158117488));
#36329=CARTESIAN_POINT('Ctrl Pts',(4.24338680893684,-2.04242454395285,17.5411877018022));
#36330=CARTESIAN_POINT('Ctrl Pts',(4.70342110133588,0.235916647177909,17.6205595918556));
#36331=CARTESIAN_POINT('Ctrl Pts',(4.01771326340766,2.45678878743836,17.699931481909));
#36332=CARTESIAN_POINT('Ctrl Pts',(2.35329778315649,4.07919314165109,17.7793033719624));
#36333=CARTESIAN_POINT('Ctrl Pts',(0.115627163561191,4.70791408521782,17.8586752620158));
#36334=CARTESIAN_POINT('Ctrl Pts',(-2.15021562607272,4.18979944864554,17.9380471520692));
#36335=CARTESIAN_POINT('Ctrl Pts',(-3.89225998228542,2.6510554089743,18.0174190421226));
#36336=CARTESIAN_POINT('Ctrl Pts',(-4.68617856238767,0.466526807638264,
18.096790932176));
#36337=CARTESIAN_POINT('Ctrl Pts',(-4.33851638857381,-1.83165928184378,
18.1761628222294));
#36338=CARTESIAN_POINT('Ctrl Pts',(-2.93407303174987,-3.68363345125881,
18.2555347122828));
#36339=CARTESIAN_POINT('Ctrl Pts',(-0.814760394348088,-4.63832755437977,
18.3349066023362));
#36340=CARTESIAN_POINT('Ctrl Pts',(1.50277006074129,-4.46305057284721,18.4142784923896));
#36341=CARTESIAN_POINT('Ctrl Pts',(3.45471245456617,-3.20074439226408,18.493650382443));
#36342=CARTESIAN_POINT('Ctrl Pts',(4.56418179760217,-1.15844177813615,18.5730222724965));
#36343=CARTESIAN_POINT('Ctrl Pts',(4.56354990278295,1.16548416044567,18.6523941625499));
#36344=CARTESIAN_POINT('Ctrl Pts',(3.44799414715945,3.20657754587687,18.7317660526033));
#36345=CARTESIAN_POINT('Ctrl Pts',(1.49865065220682,4.46452630956668,18.8111379426567));
#36346=CARTESIAN_POINT('Ctrl Pts',(-0.827291992766502,4.63872722375952,
18.8905098327101));
#36347=CARTESIAN_POINT('Ctrl Pts',(-2.93038174053102,3.67602118591242,18.9698817227635));
#36348=CARTESIAN_POINT('Ctrl Pts',(-4.8317659974063,1.21320979378885,19.0757109095013));
#36349=CARTESIAN_POINT('Ctrl Pts',(-4.41154214902252,-3.00742829557681,
19.2079973929237));
#36350=CARTESIAN_POINT('Ctrl Pts',(0.14114360583215,-5.34031031892966,19.3667411730305));
#36351=CARTESIAN_POINT('Ctrl Pts',(4.55878074835922,-2.77696271962162,19.5254849531373));
#36352=CARTESIAN_POINT('Ctrl Pts',(4.80798654830346,2.32253130646654,19.6842287332441));
#36353=CARTESIAN_POINT('Ctrl Pts',(0.656009676029318,5.29932988758691,19.8429725133509));
#36354=CARTESIAN_POINT('Ctrl Pts',(-4.09539160933947,3.42571876325565,20.0017162934577));
#36355=CARTESIAN_POINT('Ctrl Pts',(-5.09974667860472,-1.58211192901314,
20.1604600735645));
#36356=CARTESIAN_POINT('Ctrl Pts',(-1.43734916996091,-5.14215993940121,
20.3192038536714));
#36357=CARTESIAN_POINT('Ctrl Pts',(3.54020456892056,-3.99752392897281,20.4779476337781));
#36358=CARTESIAN_POINT('Ctrl Pts',(5.27828887711237,0.806568563691912,20.636691413885));
#36359=CARTESIAN_POINT('Ctrl Pts',(2.1865632094635,4.86959394496087,20.7954351939918));
#36360=CARTESIAN_POINT('Ctrl Pts',(-2.90621803008048,4.48249178265495,20.9541789740986));
#36361=CARTESIAN_POINT('Ctrl Pts',(-5.339103029404,-0.0175478502156508,
21.1129227542054));
#36362=CARTESIAN_POINT('Ctrl Pts',(-3.29668819545046,-3.73492805813105,
21.2452092376277));
#36363=CARTESIAN_POINT('Ctrl Pts',(-0.335233909123966,-4.68912434583344,
21.3510384243656));
#36364=CARTESIAN_POINT('Ctrl Pts',(1.9434592869775,-4.29245481019942,21.430410314419));
#36365=CARTESIAN_POINT('Ctrl Pts',(3.76239327895729,-2.83237457985877,21.5097822044724));
#36366=CARTESIAN_POINT('Ctrl Pts',(4.65746145505442,-0.691994213306775,
21.5891540945258));
#36367=CARTESIAN_POINT('Ctrl Pts',(4.42189226956134,1.62210042840564,21.6685259845792));
#36368=CARTESIAN_POINT('Ctrl Pts',(3.10708740551244,3.53832597274477,21.7478978746326));
#36369=CARTESIAN_POINT('Ctrl Pts',(1.03650075501011,4.59406889295405,21.827269764686));
#36370=CARTESIAN_POINT('Ctrl Pts',(-1.28715662605568,4.52994106929143,21.9066416547395));
#36371=CARTESIAN_POINT('Ctrl Pts',(-3.29695756540469,3.36273516855513,21.9860135447928));
#36372=CARTESIAN_POINT('Ctrl Pts',(-4.5037900244027,1.37615964733944,22.0653854348462));
#36373=CARTESIAN_POINT('Ctrl Pts',(-4.61342283197247,-0.945531571193242,
22.1447573248996));
#36374=CARTESIAN_POINT('Ctrl Pts',(-3.59928179145312,-3.03695363259649,
22.224129214953));
#36375=CARTESIAN_POINT('Ctrl Pts',(-1.70833944819064,-4.388548607559,22.3035011050065));
#36376=CARTESIAN_POINT('Ctrl Pts',(0.598737773532913,-4.67111975194625,
22.3828729950598));
#36377=CARTESIAN_POINT('Ctrl Pts',(2.75997059360609,-3.81580751573965,22.4622448851133));
#36378=CARTESIAN_POINT('Ctrl Pts',(4.24887708766878,-2.03097775393672,22.5416167751666));
#36379=CARTESIAN_POINT('Ctrl Pts',(4.7027684336848,0.248596203073706,22.6209886652201));
#36380=CARTESIAN_POINT('Ctrl Pts',(4.01107478934813,2.46761134605171,22.7003605552734));
#36381=CARTESIAN_POINT('Ctrl Pts',(2.34229273922348,4.08552253105782,22.7797324453269));
#36382=CARTESIAN_POINT('Ctrl Pts',(0.10293307930986,4.70820909782832,22.8591043353802));
#36383=CARTESIAN_POINT('Ctrl Pts',(-2.16150070095897,4.18398654725925,22.9384762254337));
#36384=CARTESIAN_POINT('Ctrl Pts',(-3.89939777427635,2.64055403030605,23.017848115487));
#36385=CARTESIAN_POINT('Ctrl Pts',(-4.6874101388992,0.453888451717589,23.0972200055405));
#36386=CARTESIAN_POINT('Ctrl Pts',(-4.33357979136315,-1.84334337837373,
23.1765918955938));
#36387=CARTESIAN_POINT('Ctrl Pts',(-2.92409898707257,-3.69154082613157,
23.2559637856473));
#36388=CARTESIAN_POINT('Ctrl Pts',(-0.802314148160901,-4.64048710795707,
23.3353356757007));
#36389=CARTESIAN_POINT('Ctrl Pts',(1.51491264465863,-4.45902099747155,23.4147075657541));
#36390=CARTESIAN_POINT('Ctrl Pts',(3.46311006868958,-3.19134724418486,23.4940794558075));
#36391=CARTESIAN_POINT('Ctrl Pts',(4.56770154637975,-1.14626836492011,23.5734513458609));
#36392=CARTESIAN_POINT('Ctrl Pts',(4.55961103731633,1.17803895017003,23.6528232359143));
#36393=CARTESIAN_POINT('Ctrl Pts',(3.44080937235073,3.21537858488653,23.7321951259677));
#36394=CARTESIAN_POINT('Ctrl Pts',(1.48383416024502,4.46945911326291,23.8115670160211));
#36395=CARTESIAN_POINT('Ctrl Pts',(-0.834599768812189,4.6347892947245,23.8909389060745));
#36396=CARTESIAN_POINT('Ctrl Pts',(-2.94972704158065,3.67109506287238,23.9703107961279));
#36397=CARTESIAN_POINT('Ctrl Pts',(-4.34630733610966,1.81313019956259,24.0496826861813));
#36398=CARTESIAN_POINT('Ctrl Pts',(-4.68413678396127,-0.486509167079313,
24.1290545762347));
#36399=CARTESIAN_POINT('Ctrl Pts',(-3.8809208793951,-2.66763597748286,24.2084264662881));
#36400=CARTESIAN_POINT('Ctrl Pts',(-2.13232123888401,-4.19893256848769,
24.2877983563416));
#36401=CARTESIAN_POINT('Ctrl Pts',(0.13570713560786,-4.70737847998643,24.3671702463949));
#36402=CARTESIAN_POINT('Ctrl Pts',(2.37067755224746,-4.06911741336709,24.4465421364484));
#36403=CARTESIAN_POINT('Ctrl Pts',(4.02815616456577,-2.43962835168955,24.5259140265017));
#36404=CARTESIAN_POINT('Ctrl Pts',(4.70438485136804,-0.215851223566548,
24.6052859165551));
#36405=CARTESIAN_POINT('Ctrl Pts',(4.23463580135646,2.06050678483885,24.6846578066085));
#36406=CARTESIAN_POINT('Ctrl Pts',(2.73333884334173,3.83492990131186,24.7640296966619));
#36407=CARTESIAN_POINT('Ctrl Pts',(0.566206593231879,4.6751725822987,24.8434015867153));
#36408=CARTESIAN_POINT('Ctrl Pts',(-1.73885232971224,4.3765535705565,24.9227734767688));
#36409=CARTESIAN_POINT('Ctrl Pts',(-3.62033067402275,3.0118157963638,25.0021453668221));
#36410=CARTESIAN_POINT('Ctrl Pts',(-4.61990447960738,0.913406360718075,
25.0815172568756));
#36411=CARTESIAN_POINT('Ctrl Pts',(-4.49407977994478,-1.40750684260792,
25.1608891469289));
#36412=CARTESIAN_POINT('Ctrl Pts',(-3.27350719336448,-3.38555449453819,
25.2402610369824));
#36413=CARTESIAN_POINT('Ctrl Pts',(-1.25551550026584,-4.53888856539668,
25.3196329270357));
#36414=CARTESIAN_POINT('Ctrl Pts',(1.06831698966113,-4.58655942838399,25.3990048170892));
#36415=CARTESIAN_POINT('Ctrl Pts',(3.1319098255862,-3.51695456679402,25.4783767071426));
#36416=CARTESIAN_POINT('Ctrl Pts',(4.43257636036326,-1.59062735737991,25.557748597196));
#36417=CARTESIAN_POINT('Ctrl Pts',(4.65347710509718,0.723173155497971,25.6371204872493));
#36418=CARTESIAN_POINT('Ctrl Pts',(3.74080112732632,2.86081028841317,25.7164923773028));
#36419=CARTESIAN_POINT('Ctrl Pts',(1.91687427506164,4.30156036736711,25.7958642673562));
#36420=CARTESIAN_POINT('Ctrl Pts',(-0.373998907678805,4.69445986217281,
25.8752361574096));
#36421=CARTESIAN_POINT('Ctrl Pts',(-2.57376678434128,3.9437993255639,25.954608047463));
#36422=CARTESIAN_POINT('Ctrl Pts',(-4.14657076927436,2.23243800269932,26.0339799375164));
#36423=CARTESIAN_POINT('Ctrl Pts',(-4.70927929309089,-0.0227402762051125,
26.1133518275698));
#36424=CARTESIAN_POINT('Ctrl Pts',(-4.1248178049234,-2.27237907416072,26.1927237176232));
#36425=CARTESIAN_POINT('Ctrl Pts',(-2.53555982960589,-3.96847135947655,
26.2720956076766));
#36426=CARTESIAN_POINT('Ctrl Pts',(-0.328645092162861,-4.69785280568621,
26.35146749773));
#36427=CARTESIAN_POINT('Ctrl Pts',(1.95832686228742,-4.28284770695154,26.4308393877834));
#36428=CARTESIAN_POINT('Ctrl Pts',(3.76825472776749,-2.8245503867261,26.5102112778369));
#36429=CARTESIAN_POINT('Ctrl Pts',(4.66024408245379,-0.67819884433039,26.5895831678902));
#36430=CARTESIAN_POINT('Ctrl Pts',(4.41700829392964,1.63336043537654,26.6689550579436));
#36431=CARTESIAN_POINT('Ctrl Pts',(3.09779906188623,3.54703672840772,26.748326947997));
#36432=CARTESIAN_POINT('Ctrl Pts',(1.0239728352293,4.59666272563139,26.8276988380504));
#36433=CARTESIAN_POINT('Ctrl Pts',(-1.29929090756406,4.52655185743165,26.9070707281039));
#36434=CARTESIAN_POINT('Ctrl Pts',(-3.30605026120649,3.35378297611415,26.9864426181572));
#36435=CARTESIAN_POINT('Ctrl Pts',(-4.50746308903716,1.36403998528792,27.0658145082107));
#36436=CARTESIAN_POINT('Ctrl Pts',(-4.61086788547865,-0.957980126703151,
27.1451863982641));
#36437=CARTESIAN_POINT('Ctrl Pts',(-3.59107547100053,-3.04663840028233,
27.2245582883174));
#36438=CARTESIAN_POINT('Ctrl Pts',(-1.69650502049742,-4.39314230317249,
27.3039301783709));
#36439=CARTESIAN_POINT('Ctrl Pts',(0.611330297848721,-4.66948646506538,
27.3833020684242));
#36440=CARTESIAN_POINT('Ctrl Pts',(2.77024690879558,-3.80835405980132,27.4626739584777));
#36441=CARTESIAN_POINT('Ctrl Pts',(4.25433750459734,-2.01951503521836,27.542045848531));
#36442=CARTESIAN_POINT('Ctrl Pts',(4.70208090109553,0.261273381823074,27.6214177385845));
#36443=CARTESIAN_POINT('Ctrl Pts',(4.00440779796637,2.47841618137125,27.7007896286379));
#36444=CARTESIAN_POINT('Ctrl Pts',(2.33126981885889,4.09182228501852,27.7801615186913));
#36445=CARTESIAN_POINT('Ctrl Pts',(0.0902396720556605,4.70846953713028,
27.8595334087446));
#36446=CARTESIAN_POINT('Ctrl Pts',(-2.17277265911822,4.17814403201768,27.9389052987981));
#36447=CARTESIAN_POINT('Ctrl Pts',(-3.90650237988159,2.63003188887054,28.0182771888515));
#36448=CARTESIAN_POINT('Ctrl Pts',(-4.68861676780222,0.441249799071397,
28.0976490789049));
#36449=CARTESIAN_POINT('Ctrl Pts',(-4.32859448916339,-1.85501976509172,
28.1770209689583));
#36450=CARTESIAN_POINT('Ctrl Pts',(-2.91413617414575,-3.69941062049508,
28.2563928590117));
#36451=CARTESIAN_POINT('Ctrl Pts',(-0.78980073743719,-4.64263323725236,
28.3357647490651));
#36452=CARTESIAN_POINT('Ctrl Pts',(1.52692841071678,-4.4549206737093,28.4151366391185));
#36453=CARTESIAN_POINT('Ctrl Pts',(3.47170117781886,-3.18199929485031,28.494508529172));
#36454=CARTESIAN_POINT('Ctrl Pts',(4.57077522248444,-1.13394993100173,28.5738804192253));
#36455=CARTESIAN_POINT('Ctrl Pts',(4.55641854019218,1.19032712608322,28.6532523092787));
#36456=CARTESIAN_POINT('Ctrl Pts',(3.43212838697049,3.22464312999871,28.7326241993321));
#36457=CARTESIAN_POINT('Ctrl Pts',(1.47177935557015,4.47344320507303,28.8119960893855));
#36458=CARTESIAN_POINT('Ctrl Pts',(-0.84709186911874,4.63252241719017,28.891367979439));
#36459=CARTESIAN_POINT('Ctrl Pts',(-2.95961338949639,3.66312942239424,28.9707398694923));
#36460=CARTESIAN_POINT('Ctrl Pts',(-4.35117963918583,1.80140620850249,29.0501117595457));
#36461=CARTESIAN_POINT('Ctrl Pts',(-4.68280815994235,-0.499135570435458,
29.1294836495992));
#36462=CARTESIAN_POINT('Ctrl Pts',(-3.87371497815696,-2.67808902923317,
29.2088555396525));
#36463=CARTESIAN_POINT('Ctrl Pts',(-2.12099340201518,-4.2046659283592,29.288227429706));
#36464=CARTESIAN_POINT('Ctrl Pts',(0.148397472118242,-4.70699551420707,
29.3675993197594));
#36465=CARTESIAN_POINT('Ctrl Pts',(2.38163905051584,-4.06271141155196,29.4469712098127));
#36466=CARTESIAN_POINT('Ctrl Pts',(4.03471862787643,-2.428759801702,29.5263430998662));
#36467=CARTESIAN_POINT('Ctrl Pts',(4.70494967818454,-0.203167680126035,
29.6057149899196));
#36468=CARTESIAN_POINT('Ctrl Pts',(4.22906540111636,2.07191563862461,29.685086879973));
#36469=CARTESIAN_POINT('Ctrl Pts',(2.72299015321369,3.84228489391376,29.7644587700264));
#36470=CARTESIAN_POINT('Ctrl Pts',(0.553600531224683,4.67668205379885,29.8438306600798));
#36471=CARTESIAN_POINT('Ctrl Pts',(-1.75064495479666,4.37184981703873,29.9232025501332));
#36472=CARTESIAN_POINT('Ctrl Pts',(-3.62843720481647,3.00204464177339,30.0025744401866));
#36473=CARTESIAN_POINT('Ctrl Pts',(-4.62235018315249,0.900948036685143,
30.08194633024));
#36474=CARTESIAN_POINT('Ctrl Pts',(-4.49026888827113,-1.41961751592495,
30.1613182202934));
#36475=CARTESIAN_POINT('Ctrl Pts',(-3.26436803124854,-3.39436738392576,
30.2406901103467));
#36476=CARTESIAN_POINT('Ctrl Pts',(-1.24327434736992,-4.54225687050705,
30.3200620004003));
#36477=CARTESIAN_POINT('Ctrl Pts',(1.08067821558697,-4.58366263754788,30.3994338904535));
#36478=CARTESIAN_POINT('Ctrl Pts',(3.14137995726753,-3.50849833184719,30.4788057805071));
#36479=CARTESIAN_POINT('Ctrl Pts',(4.4368484946843,-1.57867159843783,30.5581776705604));
#36480=CARTESIAN_POINT('Ctrl Pts',(4.65151055959353,0.735716042020659,30.6375495606138));
#36481=CARTESIAN_POINT('Ctrl Pts',(3.73307494812974,2.87088488312276,30.7169214506672));
#36482=CARTESIAN_POINT('Ctrl Pts',(1.90527054232277,4.30671252129204,30.7962933407206));
#36483=CARTESIAN_POINT('Ctrl Pts',(-0.386653550349159,4.69343452202104,
30.875665230774));
#36484=CARTESIAN_POINT('Ctrl Pts',(-2.58438969399916,3.93684626192686,30.9550371208274));
#36485=CARTESIAN_POINT('Ctrl Pts',(-4.15257422864054,2.2212509664887,31.0344090108808));
#36486=CARTESIAN_POINT('Ctrl Pts',(-4.70920087275226,-0.0354361477304668,
31.1137809009342));
#36487=CARTESIAN_POINT('Ctrl Pts',(-4.11867660790086,-2.28349109479913,
31.1931527909877));
#36488=CARTESIAN_POINT('Ctrl Pts',(-2.52485183790083,-3.97529266559651,
31.272524681041));
#36489=CARTESIAN_POINT('Ctrl Pts',(-0.315978748852904,-4.69872174221564,
31.3518965710945));
#36490=CARTESIAN_POINT('Ctrl Pts',(1.9698660640085,-4.27755260287519,31.4312684611479));
#36491=CARTESIAN_POINT('Ctrl Pts',(3.77585586390199,-2.81438111767642,31.5106403512012));
#36492=CARTESIAN_POINT('Ctrl Pts',(4.66205553306415,-0.665632621738598,
31.5900122412547));
#36493=CARTESIAN_POINT('Ctrl Pts',(4.41258879365675,1.64526250750188,31.669384131308));
#36494=CARTESIAN_POINT('Ctrl Pts',(3.08822519121424,3.55537533164171,31.7487560213615));
#36495=CARTESIAN_POINT('Ctrl Pts',(1.01157676786242,4.59940659468345,31.8281279114149));
#36496=CARTESIAN_POINT('Ctrl Pts',(-1.31148951705349,4.52303259187412,31.9074998014683));
#36497=CARTESIAN_POINT('Ctrl Pts',(-3.31507985854797,3.34485786124704,31.9868716915217));
#36498=CARTESIAN_POINT('Ctrl Pts',(-4.51112408430495,1.35188315933753,32.066243581575));
#36499=CARTESIAN_POINT('Ctrl Pts',(-4.60826846832906,-0.970407287843986,
32.1456154716285));
#36500=CARTESIAN_POINT('Ctrl Pts',(-3.58284885369746,-3.05630866766684,
32.2249873616819));
#36501=CARTESIAN_POINT('Ctrl Pts',(-1.68465518880656,-4.39770002107054,
32.3043592517353));
#36502=CARTESIAN_POINT('Ctrl Pts',(0.623916751156621,-4.66782138348531,
32.3837311417887));
#36503=CARTESIAN_POINT('Ctrl Pts',(2.7805039515543,-3.80087178893047,32.4631030318421));
#36504=CARTESIAN_POINT('Ctrl Pts',(4.25976654389448,-2.00803823967918,32.5424749218955));
#36505=CARTESIAN_POINT('Ctrl Pts',(4.7013594349753,0.273948980040725,32.6218468119489));
#36506=CARTESIAN_POINT('Ctrl Pts',(3.99771157397872,2.4892028345985,32.7012187020023));
#36507=CARTESIAN_POINT('Ctrl Pts',(2.32023002234538,4.09809238840509,32.7805905920557));
#36508=CARTESIAN_POINT('Ctrl Pts',(0.0775455730107522,4.70869570736983,
32.8599624821091));
#36509=CARTESIAN_POINT('Ctrl Pts',(-2.18402880626508,4.17227117454043,32.9393343721625));
#36510=CARTESIAN_POINT('Ctrl Pts',(-3.91357860260051,2.61949061875855,33.018706262216));
#36511=CARTESIAN_POINT('Ctrl Pts',(-4.68978931390171,0.42860794639128,33.0980781522693));
#36512=CARTESIAN_POINT('Ctrl Pts',(-4.32357772900909,-1.86668267300931,
33.1774500423228));
#36513=CARTESIAN_POINT('Ctrl Pts',(-2.90415217940683,-3.70725352509686,
33.2568219323761));
#36514=CARTESIAN_POINT('Ctrl Pts',(-0.777281587132916,-4.64474562433732,
33.3361938224295));
#36515=CARTESIAN_POINT('Ctrl Pts',(1.53893307928302,-4.45078797045929,33.4155657124829));
#36516=CARTESIAN_POINT('Ctrl Pts',(3.4802670539562,-3.17262821862943,33.4949376025364));
#36517=CARTESIAN_POINT('Ctrl Pts',(4.57381567772608,-1.12162325523486,33.5743094925897));
#36518=CARTESIAN_POINT('Ctrl Pts',(4.55319292637118,1.20260665046394,33.6536813826432));
#36519=CARTESIAN_POINT('Ctrl Pts',(3.42342245647383,3.23388423803441,33.7330532726965));
#36520=CARTESIAN_POINT('Ctrl Pts',(1.45971385379651,4.47739478330101,33.81242516275));
#36521=CARTESIAN_POINT('Ctrl Pts',(-0.859577812643769,4.63022186990074,
33.8917970528033));
#36522=CARTESIAN_POINT('Ctrl Pts',(-2.96947822656726,3.65513715781495,33.9711689428568));
#36523=CARTESIAN_POINT('Ctrl Pts',(-4.35602031732756,1.78966912459429,34.0505408329101));
#36524=CARTESIAN_POINT('Ctrl Pts',(-4.6814455006743,-0.511758346012144,
34.1299127229636));
#36525=CARTESIAN_POINT('Ctrl Pts',(-3.86648092226059,-2.68852261628789,
34.209284613017));
#36526=CARTESIAN_POINT('Ctrl Pts',(-2.1096501494946,-4.21036872817975,34.2886565030704));
#36527=CARTESIAN_POINT('Ctrl Pts',(0.161086730056863,-4.70657833738016,
34.3680283931238));
#36528=CARTESIAN_POINT('Ctrl Pts',(2.39258323872595,-4.05627588142921,34.4474002831772));
#36529=CARTESIAN_POINT('Ctrl Pts',(4.04125176633455,-2.41787359917646,34.5267721732306));
#36530=CARTESIAN_POINT('Ctrl Pts',(4.7054803088231,-0.190482660036747,34.606144063284));
#36531=CARTESIAN_POINT('Ctrl Pts',(4.22346426348634,2.08330943346165,34.6855159533374));
#36532=CARTESIAN_POINT('Ctrl Pts',(2.71262167204393,3.84961196029602,34.7648878433908));
#36533=CARTESIAN_POINT('Ctrl Pts',(0.540990445577805,4.67815753457386,34.8442597334442));
#36534=CARTESIAN_POINT('Ctrl Pts',(-1.76242485596904,4.36711428835555,34.9236316234976));
#36535=CARTESIAN_POINT('Ctrl Pts',(-3.63651736366306,2.99225166793732,35.0030035135511));
#36536=CARTESIAN_POINT('Ctrl Pts',(-4.62476229086341,0.888483164446288,
35.0823754036044));
#36537=CARTESIAN_POINT('Ctrl Pts',(-4.48642536074711,-1.43171787127975,
35.1617472936579));
#36538=CARTESIAN_POINT('Ctrl Pts',(-3.25520514328689,-3.40315560261577,
35.2411191837112));
#36539=CARTESIAN_POINT('Ctrl Pts',(-1.2310241581964,-4.54559216191174,35.3204910737646));
#36540=CARTESIAN_POINT('Ctrl Pts',(1.09303158700498,-4.58073253206361,35.399862963818));
#36541=CARTESIAN_POINT('Ctrl Pts',(3.15082725699632,-3.50001659668431,35.4792348538714));
#36542=CARTESIAN_POINT('Ctrl Pts',(4.44108838142123,-1.56670436550804,35.5586067439248));
#36543=CARTESIAN_POINT('Ctrl Pts',(4.64951020631433,0.748253581264717,35.6379786339782));
#36544=CARTESIAN_POINT('Ctrl Pts',(3.72532163646553,2.8809386118726,35.7173505240316));
#36545=CARTESIAN_POINT('Ctrl Pts',(1.89365296183327,4.31183337347777,35.7967224140851));
#36546=CARTESIAN_POINT('Ctrl Pts',(-0.399305382771815,4.69237506938502,
35.8760943041384));
#36547=CARTESIAN_POINT('Ctrl Pts',(-2.59499381998119,3.92986458478612,35.9554661941919));
#36548=CARTESIAN_POINT('Ctrl Pts',(-4.1585475065645,2.210047785941,36.0348380842453));
#36549=CARTESIAN_POINT('Ctrl Pts',(-4.70908822533747,-0.0481317617014899,
36.1142099742986));
#36550=CARTESIAN_POINT('Ctrl Pts',(-4.11250547580826,-2.29458651873135,
36.1935818643521));
#36551=CARTESIAN_POINT('Ctrl Pts',(-2.51412549524861,-3.98208507877941,
36.2729537544055));
#36552=CARTESIAN_POINT('Ctrl Pts',(-0.303310108968769,-4.6995565278326,
36.3523256444589));
#36553=CARTESIAN_POINT('Ctrl Pts',(1.98139094849032,-4.27222640899768,36.4316975345123));
#36554=CARTESIAN_POINT('Ctrl Pts',(3.7834295566316,-2.80419139334371,36.5110694245656));
#36555=CARTESIAN_POINT('Ctrl Pts',(4.66383309925673,-0.653061561243602,
36.5904413146191));
#36556=CARTESIAN_POINT('Ctrl Pts',(4.4081372221224,1.65715262164824,36.6698132046725));
#36557=CARTESIAN_POINT('Ctrl Pts',(3.07862887492527,3.56368809395169,36.7491850947259));
#36558=CARTESIAN_POINT('Ctrl Pts',(0.999173348225765,4.60211703465827,36.8285569847793));
#36559=CARTESIAN_POINT('Ctrl Pts',(-1.3236785944688,4.51948045233538,36.9079288748327));
#36560=CARTESIAN_POINT('Ctrl Pts',(-3.32408536146365,3.33590843552393,36.9873007648862));
#36561=CARTESIAN_POINT('Ctrl Pts',(-4.51475229214413,1.33971650772689,37.0666726549395));
#36562=CARTESIAN_POINT('Ctrl Pts',(-4.60563555769299,-0.982827395940232,
37.146044544993));
#36563=CARTESIAN_POINT('Ctrl Pts',(-3.57459619578919,-3.06595672140786,
37.2254164350463));
#36564=CARTESIAN_POINT('Ctrl Pts',(-1.67279311282567,-4.40222577592056,
37.3047883250997));
#36565=CARTESIAN_POINT('Ctrl Pts',(0.636498669757439,-4.6661223755806,37.3841602151531));
#36566=CARTESIAN_POINT('Ctrl Pts',(2.79074078525356,-3.79336189283575,37.4635321052066));
#36567=CARTESIAN_POINT('Ctrl Pts',(4.26516462266191,-1.9965468494605,37.5429039952599));
#36568=CARTESIAN_POINT('Ctrl Pts',(4.70060379877145,0.286622587162363,37.6222758853134));
#36569=CARTESIAN_POINT('Ctrl Pts',(3.99098629411051,2.49997139597979,37.7016477753667));
#36570=CARTESIAN_POINT('Ctrl Pts',(2.3091733621022,4.10433270633122,37.7810196654202));
#36571=CARTESIAN_POINT('Ctrl Pts',(0.0648509103550771,4.70888765420329,
37.8603915554735));
#36572=CARTESIAN_POINT('Ctrl Pts',(-2.19526907961097,4.16636799246395,37.9397634455269));
#36573=CARTESIAN_POINT('Ctrl Pts',(-3.92062638092667,2.60893030984724,38.0191353355804));
#36574=CARTESIAN_POINT('Ctrl Pts',(-4.69092777401319,0.415962978544177,
38.0985072256337));
#36575=CARTESIAN_POINT('Ctrl Pts',(-4.31852954453265,-1.87833201365752,
38.1778791156872));
#36576=CARTESIAN_POINT('Ctrl Pts',(-2.89414707692572,-3.71506948486711,
38.2572510057405));
#36577=CARTESIAN_POINT('Ctrl Pts',(-0.764756787430149,-4.64682425288566,
38.336622895794));
#36578=CARTESIAN_POINT('Ctrl Pts',(1.55092656265596,-4.44662291817819,38.4159947858474));
#36579=CARTESIAN_POINT('Ctrl Pts',(3.48880763512333,-3.16323408359078,38.4953666759007));
#36580=CARTESIAN_POINT('Ctrl Pts',(4.57682288978048,-1.10928842689192,38.5747385659542));
#36581=CARTESIAN_POINT('Ctrl Pts',(4.5499342195639,1.21487743324952,38.6541104560075));
#36582=CARTESIAN_POINT('Ctrl Pts',(3.41469164371823,3.24310184347568,38.733482346061));
#36583=CARTESIAN_POINT('Ctrl Pts',(1.44763774336306,4.48131381605587,38.8128542361143));
#36584=CARTESIAN_POINT('Ctrl Pts',(-0.872057510020701,4.62788767559439,
38.8922261261678));
#36585=CARTESIAN_POINT('Ctrl Pts',(-2.9793214784951,3.6471183158447,38.9715980162212));
#36586=CARTESIAN_POINT('Ctrl Pts',(-4.36082934025308,1.77791905463904,39.0509699062746));
#36587=CARTESIAN_POINT('Ctrl Pts',(-4.68004880681061,-0.524377442655287,
39.130341796328));
#36588=CARTESIAN_POINT('Ctrl Pts',(-3.85921878174905,-2.6989365861694,39.2097136863814));
#36589=CARTESIAN_POINT('Ctrl Pts',(-2.09829153079023,-4.21604107122303,
39.2890855764348));
#36590=CARTESIAN_POINT('Ctrl Pts',(0.173774754931348,-4.70612667927191,
39.3684574664882));
#36591=CARTESIAN_POINT('Ctrl Pts',(2.40351015490339,-4.04981138575493,39.4478293565416));
#36592=CARTESIAN_POINT('Ctrl Pts',(4.04775531046155,-2.40696884895629,39.527201246595));
#36593=CARTESIAN_POINT('Ctrl Pts',(4.70597715859854,-0.177798095133498,
39.6065731366484));
#36594=CARTESIAN_POINT('Ctrl Pts',(4.21783163769349,2.0946915601602,39.6859450267019));
#36595=CARTESIAN_POINT('Ctrl Pts',(2.70223496968604,3.85690448821556,39.7653169167552));
#36596=CARTESIAN_POINT('Ctrl Pts',(0.528373605920714,4.67961139929736,39.8446888068086));
#36597=CARTESIAN_POINT('Ctrl Pts',(-1.77418661813221,4.36232362711485,39.9240606968621));
#36598=CARTESIAN_POINT('Ctrl Pts',(-3.6445811625546,2.98248116081159,40.0034325869154));
#36599=CARTESIAN_POINT('Ctrl Pts',(-4.62712170766669,0.875927969712799,
40.0828044769689));
#36600=CARTESIAN_POINT('Ctrl Pts',(-4.48258575488106,-1.44364637546354,
40.1621763670223));
#36601=CARTESIAN_POINT('Ctrl Pts',(-3.24594541476057,-3.41224896374515,
40.2415482570757));
#36602=CARTESIAN_POINT('Ctrl Pts',(-1.89461073269764,-4.16947670058303,
40.2944628504446));
#36603=CARTESIAN_POINT('Ctrl Pts',(-1.16918346556913,-4.36383719750631,
40.3209201471291));
#36604=CARTESIAN_POINT('Ctrl Pts',(-3.57461543774205,3.05624720968391,-0.106973382376353));
#36605=CARTESIAN_POINT('Ctrl Pts',(-4.08267404777841,2.46201708819397,-0.0805160856918847));
#36606=CARTESIAN_POINT('Ctrl Pts',(-4.79625497710715,1.01593427979912,-0.027601492322949));
#36607=CARTESIAN_POINT('Ctrl Pts',(-4.69765387924802,-1.40219731261579,
0.051770397730455));
#36608=CARTESIAN_POINT('Ctrl Pts',(-3.45499130789169,-3.47806613859392,
0.131142287783858));
#36609=CARTESIAN_POINT('Ctrl Pts',(-1.37056128557091,-4.70703587006775,
0.210514177837262));
#36610=CARTESIAN_POINT('Ctrl Pts',(1.04766160592227,-4.78919858119765,0.289886067890666));
#36611=CARTESIAN_POINT('Ctrl Pts',(3.21071490770584,-3.70482006635648,0.36925795794407));
#36612=CARTESIAN_POINT('Ctrl Pts',(4.59162481050196,-1.71790426872487,0.448629847997472));
#36613=CARTESIAN_POINT('Ctrl Pts',(4.85403585089543,0.687462033087635,0.528001738050878));
#36614=CARTESIAN_POINT('Ctrl Pts',(3.93400879434301,2.92537849589629,0.607373628104279));
#36615=CARTESIAN_POINT('Ctrl Pts',(2.05566892616791,4.45067161106188,0.686745518157684));
#36616=CARTESIAN_POINT('Ctrl Pts',(-0.323428943211738,4.89179500940945,
0.766117408211087));
#36617=CARTESIAN_POINT('Ctrl Pts',(-2.62373939006112,4.1412858336604,0.845489298264492));
#36618=CARTESIAN_POINT('Ctrl Pts',(-4.28491317807112,2.38196972749854,0.924861188317894));
#36619=CARTESIAN_POINT('Ctrl Pts',(-4.90229136258891,0.042410468561284,
1.0042330783713));
#36620=CARTESIAN_POINT('Ctrl Pts',(-4.32548234816227,-2.30747956911558,
1.0836049684247));
#36621=CARTESIAN_POINT('Ctrl Pts',(-2.69499534131545,-4.09527285943935,
1.16297685847811));
#36622=CARTESIAN_POINT('Ctrl Pts',(-0.408013469920106,-4.88546665687605,
1.24234874853151));
#36623=CARTESIAN_POINT('Ctrl Pts',(1.97835959833349,-4.48557163766149,1.32172063858491));
#36624=CARTESIAN_POINT('Ctrl Pts',(3.8828086375498,-2.99300127117732,1.40109252863832));
#36625=CARTESIAN_POINT('Ctrl Pts',(4.84141409235741,-0.771342433159628,
1.48046441869172));
#36626=CARTESIAN_POINT('Ctrl Pts',(4.62066178777609,1.63821372124453,1.55983630874512));
#36627=CARTESIAN_POINT('Ctrl Pts',(3.27432650082566,3.64870463556752,1.63920819879853));
#36628=CARTESIAN_POINT('Ctrl Pts',(1.13037252509344,4.77037917890212,1.71858008885193));
#36629=CARTESIAN_POINT('Ctrl Pts',(-1.2889376953016,4.72999991227064,1.79795197890533));
#36630=CARTESIAN_POINT('Ctrl Pts',(-3.394265546355,3.53740313723842,1.87732386895874));
#36631=CARTESIAN_POINT('Ctrl Pts',(-4.67275782327988,1.48310278759205,1.95669575901214));
#36632=CARTESIAN_POINT('Ctrl Pts',(-4.81297663748911,-0.9324781181648,2.03606764906555));
#36633=CARTESIAN_POINT('Ctrl Pts',(-3.78076499611659,-3.12090941842389,
2.11543953911895));
#36634=CARTESIAN_POINT('Ctrl Pts',(-1.82756737028867,-4.54909409232738,
2.19481142917235));
#36635=CARTESIAN_POINT('Ctrl Pts',(0.57082162169894,-4.86912951461188,2.27418331922576));
#36636=CARTESIAN_POINT('Ctrl Pts',(2.8301597301281,-4.00305576476012,2.35355520927916));
#36637=CARTESIAN_POINT('Ctrl Pts',(4.40007719275289,-2.16184649123289,2.43292709933256));
#36638=CARTESIAN_POINT('Ctrl Pts',(4.89814559062742,0.205983802396055,2.51229898938597));
#36639=CARTESIAN_POINT('Ctrl Pts',(4.20303656448716,2.52363689769692,2.59167087943937));
#36640=CARTESIAN_POINT('Ctrl Pts',(2.48407713450111,4.22653763069529,2.67104276949277));
#36641=CARTESIAN_POINT('Ctrl Pts',(0.160002012962259,4.89986315213815,2.75041465954618));
#36642=CARTESIAN_POINT('Ctrl Pts',(-2.20304924477586,4.37959285538356,2.82978654959959));
#36643=CARTESIAN_POINT('Ctrl Pts',(-4.02944258285332,2.79246343312173,2.90915843965298));
#36644=CARTESIAN_POINT('Ctrl Pts',(-4.8742726267676,0.525096099564501,2.9885303297064));
#36645=CARTESIAN_POINT('Ctrl Pts',(-4.53174064782075,-1.87018348156618,
3.06790221975979));
#36646=CARTESIAN_POINT('Ctrl Pts',(-3.08528667790254,-3.80989050616825,
3.1472741098132));
#36647=CARTESIAN_POINT('Ctrl Pts',(-0.887263702413488,-4.82151663651732,
3.2266459998666));
#36648=CARTESIAN_POINT('Ctrl Pts',(1.52689474705858,-4.65863198645683,3.30601788992001));
#36649=CARTESIAN_POINT('Ctrl Pts',(3.56910501587138,-3.36091489620245,3.38538977997341));
#36650=CARTESIAN_POINT('Ctrl Pts',(4.74188920289787,-1.24448637649211,3.46476167002681));
#36651=CARTESIAN_POINT('Ctrl Pts',(4.75955967609216,1.17509626990786,3.54413356008022));
#36652=CARTESIAN_POINT('Ctrl Pts',(3.61781194729703,3.30842806598974,3.62350545013362));
#36653=CARTESIAN_POINT('Ctrl Pts',(1.59477323603129,4.63583410827783,3.70287734018703));
#36654=CARTESIAN_POINT('Ctrl Pts',(-0.816748705561003,4.83396122303419,
3.78224923024042));
#36655=CARTESIAN_POINT('Ctrl Pts',(-3.02931247032122,3.85454608365112,3.86162112029383));
#36656=CARTESIAN_POINT('Ctrl Pts',(-4.50394242258063,1.93617205018365,3.94099301034724));
#36657=CARTESIAN_POINT('Ctrl Pts',(-4.88142197000684,-0.453849209064403,
4.02036490040064));
#36658=CARTESIAN_POINT('Ctrl Pts',(-4.06979793038364,-2.73331380556256,
4.09973679045404));
#36659=CARTESIAN_POINT('Ctrl Pts',(-2.2667801232639,-4.34694920911316,4.17910868050745));
#36660=CARTESIAN_POINT('Ctrl Pts',(0.0884203044502142,-4.90167740713265,
4.25848057056085));
#36661=CARTESIAN_POINT('Ctrl Pts',(2.42208174171528,-4.26236783845356,4.33785246061425));
#36662=CARTESIAN_POINT('Ctrl Pts',(4.16572942788551,-2.58475489891836,4.41722435066765));
#36663=CARTESIAN_POINT('Ctrl Pts',(4.89461464610853,-0.277501387264568,
4.49659624072106));
#36664=CARTESIAN_POINT('Ctrl Pts',(4.43118257058524,2.09735084808797,4.57596813077446));
#36665=CARTESIAN_POINT('Ctrl Pts',(2.88832422912366,3.96129305925364,4.65534002082787));
#36666=CARTESIAN_POINT('Ctrl Pts',(0.641876498644775,4.86027304935857,4.73471191088126));
#36667=CARTESIAN_POINT('Ctrl Pts',(-1.76093092613442,4.57530128267169,4.81408380093468));
#36668=CARTESIAN_POINT('Ctrl Pts',(-3.73477947506178,3.17579625078358,4.89345569098808));
#36669=CARTESIAN_POINT('Ctrl Pts',(-4.79884401065823,1.00267428171038,4.97282758104148));
#36670=CARTESIAN_POINT('Ctrl Pts',(-4.6939207673194,-1.41469692300561,5.05219947109488));
#36671=CARTESIAN_POINT('Ctrl Pts',(-3.44556881487893,-3.48745108865595,
5.13157136114829));
#36672=CARTESIAN_POINT('Ctrl Pts',(-1.35788392577118,-4.71066988845176,
5.21094325120169));
#36673=CARTESIAN_POINT('Ctrl Pts',(1.06057848202937,-4.78637993031164,5.2903151412551));
#36674=CARTESIAN_POINT('Ctrl Pts',(3.22068631915819,-3.69613841561989,5.3696870313085));
#36675=CARTESIAN_POINT('Ctrl Pts',(4.59624209780833,-1.70552576414673,5.44905892136191));
#36676=CARTESIAN_POINT('Ctrl Pts',(4.85216347504167,0.700549188355308,5.52843081141531));
#36677=CARTESIAN_POINT('Ctrl Pts',(3.92610856983656,2.93597190921332,5.60780270146871));
#36678=CARTESIAN_POINT('Ctrl Pts',(2.04366230731317,4.45619837165057,5.68717459152211));
#36679=CARTESIAN_POINT('Ctrl Pts',(-0.336615569701915,4.89090477438153,
5.76654648157553));
#36680=CARTESIAN_POINT('Ctrl Pts',(-2.63489463902355,4.13419759990724,5.84591837162891));
#36681=CARTESIAN_POINT('Ctrl Pts',(-4.29131920651939,2.37040904098672,5.92529026168234));
#36682=CARTESIAN_POINT('Ctrl Pts',(-4.90238791398106,0.0291940864932555,
6.00466215173572));
#36683=CARTESIAN_POINT('Ctrl Pts',(-4.31924577684855,-2.31913248284995,
6.08403404178914));
#36684=CARTESIAN_POINT('Ctrl Pts',(-2.68394492896408,-4.1025235126836,6.16340593184253));
#36685=CARTESIAN_POINT('Ctrl Pts',(-0.394841037195299,-4.88654889560929,
6.24277782189594));
#36686=CARTESIAN_POINT('Ctrl Pts',(1.99044525726845,-4.48022178375707,6.32214971194934));
#36687=CARTESIAN_POINT('Ctrl Pts',(3.89086349283745,-2.98252256218433,6.40152160200274));
#36688=CARTESIAN_POINT('Ctrl Pts',(4.84347599383151,-0.758287446165202,
6.48089349205615));
#36689=CARTESIAN_POINT('Ctrl Pts',(4.61622846358046,1.65066481329898,6.56026538210956));
#36690=CARTESIAN_POINT('Ctrl Pts',(3.26447789744962,3.65751877792811,6.63963727216296));
#36691=CARTESIAN_POINT('Ctrl Pts',(1.11750774129931,4.77340926403445,6.71900916221636));
#36692=CARTESIAN_POINT('Ctrl Pts',(-1.30168482707007,4.7265078191842,6.79838105226977));
#36693=CARTESIAN_POINT('Ctrl Pts',(-3.4037898527957,3.52823953152828,6.87775294232317));
#36694=CARTESIAN_POINT('Ctrl Pts',(-4.67673920454132,1.4704999036178,6.95712483237657));
#36695=CARTESIAN_POINT('Ctrl Pts',(-4.81044523784733,-0.945450245917632,
7.03649672242998));
#36696=CARTESIAN_POINT('Ctrl Pts',(-3.77233745895366,-3.13109080826615,
7.11586861248337));
#36697=CARTESIAN_POINT('Ctrl Pts',(-1.81529662498623,-4.554004580273,7.19524050253679));
#36698=CARTESIAN_POINT('Ctrl Pts',(0.583946448736947,-4.8675729166435,7.27461239259018));
#36699=CARTESIAN_POINT('Ctrl Pts',(2.84094146009133,-3.99541126470955,7.3539842826436));
#36700=CARTESIAN_POINT('Ctrl Pts',(4.40588942008474,-2.14997627238517,7.433356172697));
#36701=CARTESIAN_POINT('Ctrl Pts',(4.8975724696163,0.219188181000477,7.51272806275039));
#36702=CARTESIAN_POINT('Ctrl Pts',(4.19621770614212,2.53495887865921,7.59209995280381));
#36703=CARTESIAN_POINT('Ctrl Pts',(2.47267359762208,4.23321920451286,7.6714718428572));
#36704=CARTESIAN_POINT('Ctrl Pts',(0.14679167389147,4.90027670221897,7.75084373291062));
#36705=CARTESIAN_POINT('Ctrl Pts',(-2.21484837668125,4.37363764184302,7.83021562296401));
#36706=CARTESIAN_POINT('Ctrl Pts',(-4.03695626517815,2.78159013279685,7.90958751301742));
#36707=CARTESIAN_POINT('Ctrl Pts',(-4.87567054312876,0.511953424346666,
7.98895940307082));
#36708=CARTESIAN_POINT('Ctrl Pts',(-4.52668226888691,-1.88239400508467,
8.06833129312423));
#36709=CARTESIAN_POINT('Ctrl Pts',(-3.07500421358545,-3.81819442148583,
8.14770318317762));
#36710=CARTESIAN_POINT('Ctrl Pts',(-0.874261938260974,-4.82389112824304,
8.22707507323104));
#36711=CARTESIAN_POINT('Ctrl Pts',(1.53944861007788,-4.65449863366217,8.30644696328443));
#36712=CARTESIAN_POINT('Ctrl Pts',(3.5781528845135,-3.35128057447919,8.38581885333784));
#36713=CARTESIAN_POINT('Ctrl Pts',(4.74522703638871,-1.23169798528678,8.46519074339124));
#36714=CARTESIAN_POINT('Ctrl Pts',(4.75637438558149,1.18792350680425,8.54456263344465));
#36715=CARTESIAN_POINT('Ctrl Pts',(3.60887946250276,3.31816946206181,8.62393452349805));
#36716=CARTESIAN_POINT('Ctrl Pts',(1.58226949047756,4.64011668100466,8.70330641355145));
#36717=CARTESIAN_POINT('Ctrl Pts',(-0.829777827133893,4.83174174717884,
8.78267830360486));
#36718=CARTESIAN_POINT('Ctrl Pts',(-3.03969310273758,3.84636521861918,8.86205019365827));
#36719=CARTESIAN_POINT('Ctrl Pts',(-4.50914586676094,1.9240226365889,8.94142208371166));
#36720=CARTESIAN_POINT('Ctrl Pts',(-4.88018067846642,-0.467007600962554,
9.02079397376508));
#36721=CARTESIAN_POINT('Ctrl Pts',(-4.0624142789942,-2.74427582062334,9.10016586381847));
#36722=CARTESIAN_POINT('Ctrl Pts',(-2.25505275316047,-4.35304452473175,
9.17953775387187));
#36723=CARTESIAN_POINT('Ctrl Pts',(0.101634631868527,-4.90142121791617,
9.25890964392528));
#36724=CARTESIAN_POINT('Ctrl Pts',(2.4335640455388,-4.25582255152803,9.33828153397868));
#36725=CARTESIAN_POINT('Ctrl Pts',(4.17268264431847,-2.57351493169112,9.41765342403209));
#36726=CARTESIAN_POINT('Ctrl Pts',(4.89534498701854,-0.264304770872935,
9.49702531408549));
#36727=CARTESIAN_POINT('Ctrl Pts',(4.42551212654324,2.10928944710123,9.57639720413889));
#36728=CARTESIAN_POINT('Ctrl Pts',(2.8776343077469,3.96906542459454,9.65576909419229));
#36729=CARTESIAN_POINT('Ctrl Pts',(0.628771141118955,4.86198585003388,9.73514098424571));
#36730=CARTESIAN_POINT('Ctrl Pts',(-1.77325928372426,4.57053728422814,9.81451287429909));
#36731=CARTESIAN_POINT('Ctrl Pts',(-3.74332767209512,3.16571595269709,9.89388476435253));
#36732=CARTESIAN_POINT('Ctrl Pts',(-4.80152972525885,0.989733222282404,
9.97325665440589));
#36733=CARTESIAN_POINT('Ctrl Pts',(-4.69008976535528,-1.42734633034291,
10.0526285444593));
#36734=CARTESIAN_POINT('Ctrl Pts',(-3.43615431994881,-3.49672747627419,
10.1320004345127));
#36735=CARTESIAN_POINT('Ctrl Pts',(-1.34517928800141,-4.71431354886008,
10.2113723245661));
#36736=CARTESIAN_POINT('Ctrl Pts',(1.07347844099931,-4.78350327589974,10.2907442146195));
#36737=CARTESIAN_POINT('Ctrl Pts',(3.23063919787684,-3.68744219303511,10.3701161046729));
#36738=CARTESIAN_POINT('Ctrl Pts',(4.60082339705013,-1.69312835396196,10.4494879947263));
#36739=CARTESIAN_POINT('Ctrl Pts',(4.85025720045185,0.713627804460256,10.5288598847798));
#36740=CARTESIAN_POINT('Ctrl Pts',(3.91817908568572,2.94654580930431,10.6082317748331));
#36741=CARTESIAN_POINT('Ctrl Pts',(2.03164121838884,4.46169177707037,10.6876036648866));
#36742=CARTESIAN_POINT('Ctrl Pts',(-0.349799952746016,4.8899795037293,10.7669755549399));
#36743=CARTESIAN_POINT('Ctrl Pts',(-2.64603062966098,4.12707904706582,10.8463474449934));
#36744=CARTESIAN_POINT('Ctrl Pts',(-4.29769410207999,2.35883126967163,10.9257193350467));
#36745=CARTESIAN_POINT('Ctrl Pts',(-4.90244880401686,0.0159774161698882,
11.0050912251002));
#36746=CARTESIAN_POINT('Ctrl Pts',(-4.31297782868159,-2.33076850054543,
11.0844631151536));
#36747=CARTESIAN_POINT('Ctrl Pts',(-2.672875000894,-4.10974436959645,11.163835005207));
#36748=CARTESIAN_POINT('Ctrl Pts',(-0.381665739197088,-4.88759560697865,
11.2432068952604));
#36749=CARTESIAN_POINT('Ctrl Pts',(2.00251645176545,-4.47483937301022,11.3225787853138));
#36750=CARTESIAN_POINT('Ctrl Pts',(3.89889006757291,-2.97202217266546,11.4019506753672));
#36751=CARTESIAN_POINT('Ctrl Pts',(4.84550269296641,-0.745226949518873,
11.4813225654206));
#36752=CARTESIAN_POINT('Ctrl Pts',(4.61176158769154,1.66310390899864,11.560694455474));
#36753=CARTESIAN_POINT('Ctrl Pts',(3.25460556761616,3.66630633650213,11.6400663455274));
#36754=CARTESIAN_POINT('Ctrl Pts',(1.10463483521672,4.77640465566513,11.7194382355808));
#36755=CARTESIAN_POINT('Ctrl Pts',(-1.3144224979738,4.72298137310049,11.7988101256342));
#36756=CARTESIAN_POINT('Ctrl Pts',(-3.41328942008276,3.51905028219049,11.8781820156876));
#36757=CARTESIAN_POINT('Ctrl Pts',(-4.6806865946475,1.45788633182458,11.957553905741));
#36758=CARTESIAN_POINT('Ctrl Pts',(-4.80787887528018,-0.95841550199713,
12.0369257957944));
#36759=CARTESIAN_POINT('Ctrl Pts',(-3.76388250395398,-3.14124944094907,
12.1162976858478));
#36760=CARTESIAN_POINT('Ctrl Pts',(-1.80301268587722,-4.55888196912352,
12.1956695759012));
#36761=CARTESIAN_POINT('Ctrl Pts',(0.59706703157835,-4.86598094053357,12.2750414659546));
#36762=CARTESIAN_POINT('Ctrl Pts',(2.8517025417269,-3.98773772549578,12.354413356008));
#36763=CARTESIAN_POINT('Ctrl Pts',(4.41166962484727,-2.13809042723494,12.4337852460614));
#36764=CARTESIAN_POINT('Ctrl Pts',(4.89696375241996,0.232390966517433,12.5131571361148));
#36765=CARTESIAN_POINT('Ctrl Pts',(4.18936834914853,2.54626243521486,12.5925290261683));
#36766=CARTESIAN_POINT('Ctrl Pts',(2.46125208903407,4.23987001075024,12.6719009162216));
#36767=CARTESIAN_POINT('Ctrl Pts',(0.133580267920011,4.90065463645993,12.751272806275));
#36768=CARTESIAN_POINT('Ctrl Pts',(-2.22663141078444,4.36765064014303,12.8306446963284));
#36769=CARTESIAN_POINT('Ctrl Pts',(-4.04444060638688,2.770696615518,12.9100165863818));
#36770=CARTESIAN_POINT('Ctrl Pts',(-4.87703302249085,0.498807028185692,
12.9893884764353));
#36771=CARTESIAN_POINT('Ctrl Pts',(-4.52159098944558,-1.89459084712199,
13.0687603664886));
#36772=CARTESIAN_POINT('Ctrl Pts',(-3.06469939974324,-3.82647058567648,
13.1481322565421));
#36773=CARTESIAN_POINT('Ctrl Pts',(-0.861253819860521,-4.82623055930914,
13.2275041465954));
#36774=CARTESIAN_POINT('Ctrl Pts',(1.55199128418723,-4.65033145137426,13.3068760366489));
#36775=CARTESIAN_POINT('Ctrl Pts',(3.58717474668141,-3.34162189521869,13.3862479267023));
#36776=CARTESIAN_POINT('Ctrl Pts',(4.74853038096063,-1.21890064194246,13.4656198167557));
#36777=CARTESIAN_POINT('Ctrl Pts',(4.75315452513156,1.20074210972015,13.5449917068091));
#36778=CARTESIAN_POINT('Ctrl Pts',(3.59992074790953,3.32788674125251,13.6243635968625));
#36779=CARTESIAN_POINT('Ctrl Pts',(1.56975424478615,4.64436552876813,13.7037354869159));
#36780=CARTESIAN_POINT('Ctrl Pts',(-0.842800917775063,4.82948715360455,
13.7831073769693));
#36781=CARTESIAN_POINT('Ctrl Pts',(-3.05005164227443,3.83815639771137,13.8624792670227));
#36782=CARTESIAN_POINT('Ctrl Pts',(-4.51431653789056,1.91185923895083,13.9418511570761));
#36783=CARTESIAN_POINT('Ctrl Pts',(-4.87890391714672,-0.480162598589543,
14.0212230471295));
#36784=CARTESIAN_POINT('Ctrl Pts',(-4.05500110145656,-2.75521788993537,
14.1005949371829));
#36785=CARTESIAN_POINT('Ctrl Pts',(-2.24330899304429,-4.35910820186428,
14.1799668272363));
#36786=CARTESIAN_POINT('Ctrl Pts',(0.114848220593315,-4.90112940454139,
14.2593387172897));
#36787=CARTESIAN_POINT('Ctrl Pts',(2.4450286619066,-4.2492463327382,14.3387106073431));
#36788=CARTESIAN_POINT('Ctrl Pts',(4.17960553315863,-2.56225625982719,14.4180824973965));
#36789=CARTESIAN_POINT('Ctrl Pts',(4.89603974793314,-0.2511062334803,14.4974543874499));
#36790=CARTESIAN_POINT('Ctrl Pts',(4.41980951731128,2.12121271552818,14.5768262775033));
#36791=CARTESIAN_POINT('Ctrl Pts',(2.86692347135483,3.97680894225867,14.6561981675567));
#36792=CARTESIAN_POINT('Ctrl Pts',(0.615661213603817,4.86366331317225,14.7355700576101));
#36793=CARTESIAN_POINT('Ctrl Pts',(-1.78557475303814,4.56574006653321,14.8149419476636));
#36794=CARTESIAN_POINT('Ctrl Pts',(-3.75184866214265,3.15561264578087,14.8943138377169));
#36795=CARTESIAN_POINT('Ctrl Pts',(-4.80418054172537,0.976784969346447,
14.9736857277704));
#36796=CARTESIAN_POINT('Ctrl Pts',(-4.68622467521704,-1.43998536354391,
15.0530576178237));
#36797=CARTESIAN_POINT('Ctrl Pts',(-3.42671485060823,-3.50597844922854,
15.1324295078772));
#36798=CARTESIAN_POINT('Ctrl Pts',(-1.33246487329588,-4.71792294503274,
15.2118013979305));
#36799=CARTESIAN_POINT('Ctrl Pts',(1.08637059779033,-4.78059185437226,15.291173287984));
#36800=CARTESIAN_POINT('Ctrl Pts',(3.24056859589536,-3.67871916964732,15.3705451780373));
#36801=CARTESIAN_POINT('Ctrl Pts',(4.60537125691718,-1.68071863790306,15.4499170680908));
#36802=CARTESIAN_POINT('Ctrl Pts',(4.84831567357043,0.726701233826767,15.5292889581442));
#36803=CARTESIAN_POINT('Ctrl Pts',(3.91022112370653,2.95709829352236,15.6086608481976));
#36804=CARTESIAN_POINT('Ctrl Pts',(2.01960536323555,4.46715275434186,15.688032738251));
#36805=CARTESIAN_POINT('Ctrl Pts',(-0.362981793399331,4.88901869207872,
15.7674046283044));
#36806=CARTESIAN_POINT('Ctrl Pts',(-2.65714738860797,4.11993049808428,15.8467765183578));
#36807=CARTESIAN_POINT('Ctrl Pts',(-4.3040377614491,2.34723635406844,15.9261484084112));
#36808=CARTESIAN_POINT('Ctrl Pts',(-4.90247406242457,0.00276062972017743,
16.0055202984646));
#36809=CARTESIAN_POINT('Ctrl Pts',(-4.30667853324066,-2.34238757791569,
16.084892188518));
#36810=CARTESIAN_POINT('Ctrl Pts',(-2.66178564602119,-4.11693535636137,
16.1642640785714));
#36811=CARTESIAN_POINT('Ctrl Pts',(-0.368487667211246,-4.88860679467341,
16.2436359686248));
#36812=CARTESIAN_POINT('Ctrl Pts',(2.01457309173119,-4.46942443856166,16.3230078586782));
#36813=CARTESIAN_POINT('Ctrl Pts',(3.90688830464663,-2.96150018209857,16.4023797487316));
#36814=CARTESIAN_POINT('Ctrl Pts',(4.84749417442,-0.732161036485258,16.481751638785));
#36815=CARTESIAN_POINT('Ctrl Pts',(4.60726119282582,1.67553091707946,16.5611235288384));
#36816=CARTESIAN_POINT('Ctrl Pts',(3.24470958308425,3.67506724782763,16.6404954188918));
#36817=CARTESIAN_POINT('Ctrl Pts',(1.09175390014313,4.77936533189424,16.7198673089452));
#36818=CARTESIAN_POINT('Ctrl Pts',(-1.32715061480029,4.7194205995551,16.7992391989986));
#36819=CARTESIAN_POINT('Ctrl Pts',(-3.42276418043948,3.50983545637255,16.878611089052));
#36820=CARTESIAN_POINT('Ctrl Pts',(-4.68459996247752,1.44526216311684,16.9579829791054));
#36821=CARTESIAN_POINT('Ctrl Pts',(-4.80527757305004,-0.971373790661056,
17.0373548691589));
#36822=CARTESIAN_POINT('Ctrl Pts',(-3.75540018385452,-3.15138524551466,
17.1167267592122));
#36823=CARTESIAN_POINT('Ctrl Pts',(-1.79071565870356,-4.56372621798453,
17.1960986492656));
#36824=CARTESIAN_POINT('Ctrl Pts',(0.610183305945333,-4.86435360814148,
17.275470539319));
#36825=CARTESIAN_POINT('Ctrl Pts',(2.86244283812717,-3.98003518345987,17.3548424293725));
#36826=CARTESIAN_POINT('Ctrl Pts',(4.41741787585788,-2.1261890788619,17.4342143194258));
#36827=CARTESIAN_POINT('Ctrl Pts',(4.89631923419534,0.245592132270697,17.5135862094793));
#36828=CARTESIAN_POINT('Ctrl Pts',(4.1824889384277,2.55754735438707,17.5929580995327));
#36829=CARTESIAN_POINT('Ctrl Pts',(2.44981194564648,4.24649024808584,17.6723299895861));
#36830=CARTESIAN_POINT('Ctrl Pts',(0.120369299865439,4.90099648569508,17.7517018796395));
#36831=CARTESIAN_POINT('Ctrl Pts',(-2.2384009215371,4.36163277449207,17.8310737696929));
#36832=CARTESIAN_POINT('Ctrl Pts',(-4.0518905292873,2.75978129753081,17.9104456597463));
#36833=CARTESIAN_POINT('Ctrl Pts',(-4.87836953900975,0.485660146581001,
17.9898175497997));
#36834=CARTESIAN_POINT('Ctrl Pts',(-4.51644893866981,-1.90677984789346,
18.0691894398531));
#36835=CARTESIAN_POINT('Ctrl Pts',(-3.05440612489714,-3.83470774368921,
18.1485613299065));
#36836=CARTESIAN_POINT('Ctrl Pts',(-0.848175594775907,-4.82855605094715,
18.2279332199599));
#36837=CARTESIAN_POINT('Ctrl Pts',(1.56440212229575,-4.64609055668262,18.3073051100133));
#36838=CARTESIAN_POINT('Ctrl Pts',(3.59639816964341,-3.33201429213606,18.3866770000667));
#36839=CARTESIAN_POINT('Ctrl Pts',(4.75136940590255,-1.20595214372204,18.4660488901201));
#36840=CARTESIAN_POINT('Ctrl Pts',(4.75071159562135,1.21328335035095,18.5454207801735));
#36841=CARTESIAN_POINT('Ctrl Pts',(3.58940432897552,3.33808667681415,18.6247926702269));
#36842=CARTESIAN_POINT('Ctrl Pts',(1.56011376732896,4.64762681676405,18.7041645602803));
#36843=CARTESIAN_POINT('Ctrl Pts',(-0.861221142909775,4.82897211168874,
18.7835364503337));
#36844=CARTESIAN_POINT('Ctrl Pts',(-3.05056344532316,3.82678328180746,18.8629083403871));
#36845=CARTESIAN_POINT('Ctrl Pts',(-5.02992785007326,1.26296632184503,18.968737527125));
#36846=CARTESIAN_POINT('Ctrl Pts',(-4.59246965375637,-3.13076985705441,
19.1010240105473));
#36847=CARTESIAN_POINT('Ctrl Pts',(0.146932230206506,-5.55932874556365,
19.2597677906541));
#36848=CARTESIAN_POINT('Ctrl Pts',(4.74574684718979,-2.89085235699285,19.418511570761));
#36849=CARTESIAN_POINT('Ctrl Pts',(5.00517315099097,2.41778366488237,19.5772553508677));
#36850=CARTESIAN_POINT('Ctrl Pts',(0.682914143844855,5.5166676123404,19.7359991309746));
#36851=CARTESIAN_POINT('Ctrl Pts',(-4.26335305224441,3.56621538027044,19.8947429110814));
#36852=CARTESIAN_POINT('Ctrl Pts',(-5.30889903625343,-1.64699798333531,
20.0534866911882));
#36853=CARTESIAN_POINT('Ctrl Pts',(-1.49629817009909,-5.35305176256659,
20.212230471295));
#36854=CARTESIAN_POINT('Ctrl Pts',(3.68539651252336,-4.16147159288513,20.3709742514018));
#36855=CARTESIAN_POINT('Ctrl Pts',(5.49476366156206,0.839647798276105,20.5297180315086));
#36856=CARTESIAN_POINT('Ctrl Pts',(2.27623920304293,5.06930720888698,20.6884618116154));
#36857=CARTESIAN_POINT('Ctrl Pts',(-3.02540872545025,4.66632909528393,20.8472055917223));
#36858=CARTESIAN_POINT('Ctrl Pts',(-5.55807194231375,-0.0182675279713449,
21.005949371829));
#36859=CARTESIAN_POINT('Ctrl Pts',(-3.4318929716806,-3.88810606053727,21.1382358552514));
#36860=CARTESIAN_POINT('Ctrl Pts',(-0.348982623888803,-4.88143613581972,
21.2440650419892));
#36861=CARTESIAN_POINT('Ctrl Pts',(2.02316502874914,-4.46849826887164,21.3234369320426));
#36862=CARTESIAN_POINT('Ctrl Pts',(3.91669769333085,-2.94853678524969,21.4028088220961));
#36863=CARTESIAN_POINT('Ctrl Pts',(4.84847467696001,-0.720374489880037,
21.4821807121494));
#36864=CARTESIAN_POINT('Ctrl Pts',(4.60324425657816,1.68862650319429,21.5615526022029));
#36865=CARTESIAN_POINT('Ctrl Pts',(3.23451621663553,3.68344087079137,21.6409244922562));
#36866=CARTESIAN_POINT('Ctrl Pts',(1.07901003836815,4.78248223987442,21.7202963823097));
#36867=CARTESIAN_POINT('Ctrl Pts',(-1.33994588402651,4.71572438645636,21.7996682723631));
#36868=CARTESIAN_POINT('Ctrl Pts',(-3.4321733891171,3.50064868327975,21.8790401624164));
#36869=CARTESIAN_POINT('Ctrl Pts',(-4.68850082698247,1.43259912421573,21.9584120524699));
#36870=CARTESIAN_POINT('Ctrl Pts',(-4.80262992851033,-0.984309998791622,
22.0377839425233));
#36871=CARTESIAN_POINT('Ctrl Pts',(-3.74689662802585,-3.16150609615164,
22.1171558325767));
#36872=CARTESIAN_POINT('Ctrl Pts',(-1.77840238381691,-4.56853309419591,
22.1965277226301));
#36873=CARTESIAN_POINT('Ctrl Pts',(0.62329338871143,-4.86269313206684,22.2758996126835));
#36874=CARTESIAN_POINT('Ctrl Pts',(2.87316334475109,-3.97230257099384,22.3552715027369));
#36875=CARTESIAN_POINT('Ctrl Pts',(4.4231333235665,-2.11427282962158,22.4346433927903));
#36876=CARTESIAN_POINT('Ctrl Pts',(4.89563979914059,0.258791705958885,22.5140152828437));
#36877=CARTESIAN_POINT('Ctrl Pts',(4.17557820525643,2.56881377105699,22.5933871728971));
#36878=CARTESIAN_POINT('Ctrl Pts',(2.43835555951363,4.25307922033076,22.6727590629505));
#36879=CARTESIAN_POINT('Ctrl Pts',(0.107154601980389,4.90130359745224,22.7521309530039));
#36880=CARTESIAN_POINT('Ctrl Pts',(-2.25014882333759,4.35558147263095,22.8315028430573));
#36881=CARTESIAN_POINT('Ctrl Pts',(-4.05932105856842,2.74884923313531,22.9108747331107));
#36882=CARTESIAN_POINT('Ctrl Pts',(-4.87965162531074,0.472503462573818,
22.9902466231641));
#36883=CARTESIAN_POINT('Ctrl Pts',(-4.51130988023697,-1.91894313613435,
23.0696185132175));
#36884=CARTESIAN_POINT('Ctrl Pts',(-3.04402302167418,-3.84293941821872,
23.1489904032709));
#36885=CARTESIAN_POINT('Ctrl Pts',(-0.835218899364871,-4.83080417279082,
23.2283622933243));
#36886=CARTESIAN_POINT('Ctrl Pts',(1.57704270154782,-4.64189571913938,23.3077341833777));
#36887=CARTESIAN_POINT('Ctrl Pts',(3.60514018926443,-3.32223174536946,23.3871060734312));
#36888=CARTESIAN_POINT('Ctrl Pts',(4.75503350768461,-1.19327947079072,23.4664779634845));
#36889=CARTESIAN_POINT('Ctrl Pts',(4.74661118820946,1.22635304091963,23.545849853538));
#36890=CARTESIAN_POINT('Ctrl Pts',(3.58192489000304,3.34724866670522,23.6252217435913));
#36891=CARTESIAN_POINT('Ctrl Pts',(1.54468961690465,4.65276192610169,23.7045936336447));
#36892=CARTESIAN_POINT('Ctrl Pts',(-0.868828627683255,4.82487267911367,
23.7839655236982));
#36893=CARTESIAN_POINT('Ctrl Pts',(-3.0707021417273,3.8216551271151,23.8633374137516));
#36894=CARTESIAN_POINT('Ctrl Pts',(-4.52455941090918,1.88749084526948,23.9427093038049));
#36895=CARTESIAN_POINT('Ctrl Pts',(-4.8762440225472,-0.506462028608541,
24.0220811938584));
#36896=CARTESIAN_POINT('Ctrl Pts',(-4.04008638366986,-2.77704187334428,
24.1014530839117));
#36897=CARTESIAN_POINT('Ctrl Pts',(-2.21977264431323,-4.37114046461548,
24.1808249739652));
#36898=CARTESIAN_POINT('Ctrl Pts',(0.141272797816377,-4.90043891405946,
24.2601968640185));
#36899=CARTESIAN_POINT('Ctrl Pts',(2.46790449909909,-4.23600129097727,24.339568754072));
#36900=CARTESIAN_POINT('Ctrl Pts',(4.19336012701565,-2.53968312964219,24.4189406441254));
#36901=CARTESIAN_POINT('Ctrl Pts',(4.89732250983615,-0.224703779419903,
24.4983125341788));
#36902=CARTESIAN_POINT('Ctrl Pts',(4.40830796930024,2.14501291409586,24.5776844242322));
#36903=CARTESIAN_POINT('Ctrl Pts',(2.84543936506689,3.99220920964338,24.6570563142856));
#36904=CARTESIAN_POINT('Ctrl Pts',(0.589428029776467,4.86691217832701,24.736428204339));
#36905=CARTESIAN_POINT('Ctrl Pts',(-1.8101666688907,4.5560461130975,24.8158000943924));
#36906=CARTESIAN_POINT('Ctrl Pts',(-3.76880877375201,3.13533729935451,24.8951719844458));
#36907=CARTESIAN_POINT('Ctrl Pts',(-4.80937740344408,0.950867259440163,
24.9745438744992));
#36908=CARTESIAN_POINT('Ctrl Pts',(-4.67839234303351,-1.46523194016486,
25.0539157645526));
#36909=CARTESIAN_POINT('Ctrl Pts',(-3.40776126330575,-3.52440388238162,
25.133287654606));
#36910=CARTESIAN_POINT('Ctrl Pts',(-1.30700708278832,-4.72503883998586,
25.2126595446594));
#36911=CARTESIAN_POINT('Ctrl Pts',(1.11213113008524,-4.77466479486562,25.2920314347128));
#36912=CARTESIAN_POINT('Ctrl Pts',(3.26035666133054,-3.66119297425736,25.3714033247662));
#36913=CARTESIAN_POINT('Ctrl Pts',(4.61436652655277,-1.65586264903317,25.4507752148196));
#36914=CARTESIAN_POINT('Ctrl Pts',(4.84432691963378,0.752832152305638,25.530147104873));
#36915=CARTESIAN_POINT('Ctrl Pts',(3.89421999782782,2.97813870770851,25.6095189949265));
#36916=CARTESIAN_POINT('Ctrl Pts',(1.99548970426076,4.47797726591181,25.6888908849798));
#36917=CARTESIAN_POINT('Ctrl Pts',(-0.389337464322654,4.88699047397359,
25.7682627750333));
#36918=CARTESIAN_POINT('Ctrl Pts',(-2.67932288838098,4.10554361974534,25.8476346650867));
#36919=CARTESIAN_POINT('Ctrl Pts',(-4.31663118741032,2.32399542721376,25.92700655514));
#36920=CARTESIAN_POINT('Ctrl Pts',(-4.90241768388754,-0.0236729073104641,
26.0063784451935));
#36921=CARTESIAN_POINT('Ctrl Pts',(-4.29398608388724,-2.36557457401295,
26.0857503352468));
#36922=CARTESIAN_POINT('Ctrl Pts',(-2.63954897842897,-4.13122751059639,
26.1651222253003));
#36923=CARTESIAN_POINT('Ctrl Pts',(-0.342123584367958,-4.89052256991551,
26.2444941153537));
#36924=CARTESIAN_POINT('Ctrl Pts',(2.03864235756733,-4.45849715619131,26.323866005407));
#36925=CARTESIAN_POINT('Ctrl Pts',(3.92279953365755,-2.94039170393502,26.4032378954605));
#36926=CARTESIAN_POINT('Ctrl Pts',(4.85137142631832,-0.706013341046749,
26.4826097855139));
#36927=CARTESIAN_POINT('Ctrl Pts',(4.59815997785643,1.70034830898648,26.5619816755673));
#36928=CARTESIAN_POINT('Ctrl Pts',(3.22484693664317,3.69250887460774,26.6413535656207));
#36929=CARTESIAN_POINT('Ctrl Pts',(1.06596831974129,4.78518245160429,26.7207254556741));
#36930=CARTESIAN_POINT('Ctrl Pts',(-1.3525778203687,4.71219617521178,26.8000973457275));
#36931=CARTESIAN_POINT('Ctrl Pts',(-3.44163899731715,3.49132934080697,26.8794692357809));
#36932=CARTESIAN_POINT('Ctrl Pts',(-4.69232453245783,1.419982406908,26.9588411258343));
#36933=CARTESIAN_POINT('Ctrl Pts',(-4.79997019777595,-0.997269098236029,
27.0382130158877));
#36934=CARTESIAN_POINT('Ctrl Pts',(-3.73835374746968,-3.17158805846741,
27.1175849059411));
#36935=CARTESIAN_POINT('Ctrl Pts',(-1.7660825989855,-4.57331518784726,27.1969567959945));
#36936=CARTESIAN_POINT('Ctrl Pts',(0.636402361454069,-4.860992860329,27.2763286860479));
#36937=CARTESIAN_POINT('Ctrl Pts',(2.88386111529617,-3.96454343165977,27.3557005761013));
#36938=CARTESIAN_POINT('Ctrl Pts',(4.42881768477039,-2.10233999840624,27.4350724661547));
#36939=CARTESIAN_POINT('Ctrl Pts',(4.89492406925623,0.271988805008393,27.5144443562081));
#36940=CARTESIAN_POINT('Ctrl Pts',(4.16863778520187,2.58006173756,27.5938162462615));
#36941=CARTESIAN_POINT('Ctrl Pts',(2.42688056379555,4.25963734171175,27.673188136315));
#36942=CARTESIAN_POINT('Ctrl Pts',(0.0939406088576867,4.90157471796985,
27.7525600263683));
#36943=CARTESIAN_POINT('Ctrl Pts',(-2.2618830704639,4.34949934238213,27.8319319164218));
#36944=CARTESIAN_POINT('Ctrl Pts',(-4.06671704041374,2.73789555444364,27.9113038064751));
#36945=CARTESIAN_POINT('Ctrl Pts',(-4.88090774084432,0.45934646967172,27.9906756965286));
#36946=CARTESIAN_POINT('Ctrl Pts',(-4.50612011931125,-1.93109839836612,
28.0700475865819));
#36947=CARTESIAN_POINT('Ctrl Pts',(-3.03365161084166,-3.85113197097576,
28.1494194766353));
#36948=CARTESIAN_POINT('Ctrl Pts',(-0.822192284844965,-4.83303831979172,
28.2287913666888));
#36949=CARTESIAN_POINT('Ctrl Pts',(1.5895512618482,-4.63762723165528,28.3081632567421));
#36950=CARTESIAN_POINT('Ctrl Pts',(3.61408363956719,-3.31250041510136,28.3875351467956));
#36951=CARTESIAN_POINT('Ctrl Pts',(4.75823324232603,-1.18045582952402,28.4669070368489));
#36952=CARTESIAN_POINT('Ctrl Pts',(4.7432877594249,1.23914518323065,28.5462789269024));
#36953=CARTESIAN_POINT('Ctrl Pts',(3.57288787741725,3.35689317215169,28.6256508169558));
#36954=CARTESIAN_POINT('Ctrl Pts',(1.53214041692396,4.65690941469359,28.7050227070092));
#36955=CARTESIAN_POINT('Ctrl Pts',(-0.881833057796704,4.82251283171032,
28.7843945970626));
#36956=CARTESIAN_POINT('Ctrl Pts',(-3.08099395154251,3.81336279737351,28.863766487116));
#36957=CARTESIAN_POINT('Ctrl Pts',(-4.52963153835698,1.87528602633188,28.9431383771694));
#36958=CARTESIAN_POINT('Ctrl Pts',(-4.87486090859702,-0.519606269848997,
29.0225102672228));
#36959=CARTESIAN_POINT('Ctrl Pts',(-4.03258495182442,-2.78792362882362,
29.1018821572762));
#36960=CARTESIAN_POINT('Ctrl Pts',(-2.20798022676276,-4.37710896278109,
29.1812540473296));
#36961=CARTESIAN_POINT('Ctrl Pts',(0.154483594256982,-4.90004024197141,
29.260625937383));
#36962=CARTESIAN_POINT('Ctrl Pts',(2.47931555365931,-4.22933256427261,29.3399978274364));
#36963=CARTESIAN_POINT('Ctrl Pts',(4.20019173206215,-2.52836883538588,29.4193697174898));
#36964=CARTESIAN_POINT('Ctrl Pts',(4.89791050150138,-0.211500054648609,
29.4987416075432));
#36965=CARTESIAN_POINT('Ctrl Pts',(4.40250911411586,2.15688967125365,29.5781134975966));
#36966=CARTESIAN_POINT('Ctrl Pts',(2.83466625132033,3.9998658474328,29.65748538765));
#36967=CARTESIAN_POINT('Ctrl Pts',(0.576304964130538,4.86848355673019,29.7368572777034));
#36968=CARTESIAN_POINT('Ctrl Pts',(-1.82244293669206,4.55114944781371,29.8162291677568));
#36969=CARTESIAN_POINT('Ctrl Pts',(-3.77724777204552,3.12516540720823,29.8956010578102));
#36970=CARTESIAN_POINT('Ctrl Pts',(-4.81192341092482,0.937897990843109,
29.9749729478637));
#36971=CARTESIAN_POINT('Ctrl Pts',(-4.67442515791461,-1.47783930008941,
30.0543448379171));
#36972=CARTESIAN_POINT('Ctrl Pts',(-3.39824728310101,-3.5335782086619,30.1337167279704));
#36973=CARTESIAN_POINT('Ctrl Pts',(-1.29426389201682,-4.7285452870471,30.2130886180239));
#36974=CARTESIAN_POINT('Ctrl Pts',(1.12499931835819,-4.77164919996508,30.2924605080772));
#36975=CARTESIAN_POINT('Ctrl Pts',(3.27021518492489,-3.65238992963792,30.3718323981307));
#36976=CARTESIAN_POINT('Ctrl Pts',(4.61881387094242,-1.64341655687892,30.451204288184));
#36977=CARTESIAN_POINT('Ctrl Pts',(4.84227972156944,0.765889451494932,30.5305761782375));
#36978=CARTESIAN_POINT('Ctrl Pts',(3.88617695022651,2.98862648475217,30.6099480682908));
#36979=CARTESIAN_POINT('Ctrl Pts',(1.98341007571514,4.48334072153628,30.6893199583443));
#36980=CARTESIAN_POINT('Ctrl Pts',(-0.40251110303664,4.8859230822605,30.7686918483976));
#36981=CARTESIAN_POINT('Ctrl Pts',(-2.69038146803192,4.09830539495341,30.8480637384511));
#36982=CARTESIAN_POINT('Ctrl Pts',(-4.322880862473,2.3123495848808,30.9274356285044));
#36983=CARTESIAN_POINT('Ctrl Pts',(-4.90233604735018,-0.0368894657697565,
31.0068075185579));
#36984=CARTESIAN_POINT('Ctrl Pts',(-4.28759302222965,-2.3771423242123,31.0861794086113));
#36985=CARTESIAN_POINT('Ctrl Pts',(-2.62840182732014,-4.13832857419201,
31.1655512986647));
#36986=CARTESIAN_POINT('Ctrl Pts',(-0.328937765144189,-4.89142714353344,
31.2449231887181));
#36987=CARTESIAN_POINT('Ctrl Pts',(2.05065480852948,-4.45298488770047,31.3242950787715));
#36988=CARTESIAN_POINT('Ctrl Pts',(3.93071240989281,-2.9298053697385,31.4036669688249));
#36989=CARTESIAN_POINT('Ctrl Pts',(4.85325716869055,-0.692931748722414,
31.4830388588783));
#36990=CARTESIAN_POINT('Ctrl Pts',(4.59355922369783,1.712738512504,31.5624107489317));
#36991=CARTESIAN_POINT('Ctrl Pts',(3.21488041948321,3.70118946316684,31.6417826389851));
#36992=CARTESIAN_POINT('Ctrl Pts',(1.05306386109957,4.78803885304619,31.7211545290385));
#36993=CARTESIAN_POINT('Ctrl Pts',(-1.36527672293062,4.70853257646772,31.8005264190919));
#36994=CARTESIAN_POINT('Ctrl Pts',(-3.45103891924366,3.48203818642175,31.8798983091454));
#36995=CARTESIAN_POINT('Ctrl Pts',(-4.69613567357401,1.40732700152429,31.9592701991987));
#36996=CARTESIAN_POINT('Ctrl Pts',(-4.79726417254176,-1.010205925879,32.0386420892522));
#36997=CARTESIAN_POINT('Ctrl Pts',(-3.72978973764247,-3.1816549257911,32.1180139793055));
#36998=CARTESIAN_POINT('Ctrl Pts',(-1.75374677840301,-4.57805982825421,
32.197385869359));
#36999=CARTESIAN_POINT('Ctrl Pts',(0.649505014202782,-4.85925948991811,
32.2767577594123));
#37000=CARTESIAN_POINT('Ctrl Pts',(2.89453882300369,-3.95675429562642,32.3561296494657));
#37001=CARTESIAN_POINT('Ctrl Pts',(4.43446938147393,-2.09039251304725,32.4355015395192));
#37002=CARTESIAN_POINT('Ctrl Pts',(4.89417301414864,0.285184258704931,32.5148734295725));
#37003=CARTESIAN_POINT('Ctrl Pts',(4.16166693364494,2.59129077628124,32.594245319626));
#37004=CARTESIAN_POINT('Ctrl Pts',(2.41538799979881,4.26616459648027,32.6736172096793));
#37005=CARTESIAN_POINT('Ctrl Pts',(0.0807258955723594,4.90181016397187,
32.7529890997328));
#37006=CARTESIAN_POINT('Ctrl Pts',(-2.2736008581318,4.34338562549266,32.8323609897862));
#37007=CARTESIAN_POINT('Ctrl Pts',(-4.07408347532516,2.72692196256443,32.9117328798396));
#37008=CARTESIAN_POINT('Ctrl Pts',(-4.88212837576012,0.446186145494932,
32.991104769893));
#37009=CARTESIAN_POINT('Ctrl Pts',(-4.5008976102678,-1.94323962900084,33.0704766599464));
#37010=CARTESIAN_POINT('Ctrl Pts',(-3.02325814948215,-3.85929653115999,
33.1498485499998));
#37011=CARTESIAN_POINT('Ctrl Pts',(-0.809159695351077,-4.83523734073656,
33.2292204400532));
#37012=CARTESIAN_POINT('Ctrl Pts',(1.60204826952296,-4.63332503672604,33.3085923301066));
#37013=CARTESIAN_POINT('Ctrl Pts',(3.6230008220149,-3.30274500946005,33.3879642201599));
#37014=CARTESIAN_POINT('Ctrl Pts',(4.76139839364027,-1.16762360839165,33.4673361102135));
#37015=CARTESIAN_POINT('Ctrl Pts',(4.73992985575147,1.25192831918992,33.5467080002668));
#37016=CARTESIAN_POINT('Ctrl Pts',(3.56382489665835,3.36651327931318,33.6260798903203));
#37017=CARTESIAN_POINT('Ctrl Pts',(1.51958008113186,4.66102305624645,33.7054517803736));
#37018=CARTESIAN_POINT('Ctrl Pts',(-0.894831078624851,4.82011793367764,
33.784823670427));
#37019=CARTESIAN_POINT('Ctrl Pts',(-3.09126336830355,3.80504275161507,33.8641955604804));
#37020=CARTESIAN_POINT('Ctrl Pts',(-4.53467074385896,1.86306757757831,33.9435674505338));
#37021=CARTESIAN_POINT('Ctrl Pts',(-4.87344236353374,-0.532746734526401,
34.0229393405872));
#37022=CARTESIAN_POINT('Ctrl Pts',(-4.02505421063338,-2.79878512131536,
34.1023112306406));
#37023=CARTESIAN_POINT('Ctrl Pts',(-2.19617176132914,-4.38304564755766,
34.181683120694));
#37024=CARTESIAN_POINT('Ctrl Pts',(0.167693267891119,-4.89960595576193,
34.2610550107475));
#37025=CARTESIAN_POINT('Ctrl Pts',(2.4907085882359,-4.22263309823643,34.3404269008008));
#37026=CARTESIAN_POINT('Ctrl Pts',(4.20699280957637,-2.51703616462034,34.4197987908543));
#37027=CARTESIAN_POINT('Ctrl Pts',(4.89846289452463,-0.198294792667773,
34.4991706809077));
#37028=CARTESIAN_POINT('Ctrl Pts',(4.39667826093041,2.16875075186054,34.578542570961));
#37029=CARTESIAN_POINT('Ctrl Pts',(2.82387253485585,4.00749341368399,34.6579144610145));
#37030=CARTESIAN_POINT('Ctrl Pts',(0.563177709826186,4.87001955037029,34.7372863510678));
#37031=CARTESIAN_POINT('Ctrl Pts',(-1.83470595874441,4.54621970419178,34.8166582411213));
#37032=CARTESIAN_POINT('Ctrl Pts',(-3.78565931681763,3.11497080095877,34.8960301311746));
#37033=CARTESIAN_POINT('Ctrl Pts',(-4.81443444472882,0.924921905483118,
34.9754020212281));
#37034=CARTESIAN_POINT('Ctrl Pts',(-4.67042399847396,-1.49043591888832,
35.0547739112815));
#37035=CARTESIAN_POINT('Ctrl Pts',(-3.38870860399896,-3.5427268524425,35.1341458013349));
#37036=CARTESIAN_POINT('Ctrl Pts',(-1.28151129436916,-4.73201736643453,
35.2135176913883));
#37037=CARTESIAN_POINT('Ctrl Pts',(1.13785932999185,-4.76859892410594,35.2928895814417));
#37038=CARTESIAN_POINT('Ctrl Pts',(3.28004994017574,-3.64356033897983,35.3722614714951));
#37039=CARTESIAN_POINT('Ctrl Pts',(4.62322764520025,-1.63095852016229,35.4516333615485));
#37040=CARTESIAN_POINT('Ctrl Pts',(4.84019732919482,0.77894118410138,35.5310052516019));
#37041=CARTESIAN_POINT('Ctrl Pts',(3.87810565739256,2.99909254007502,35.6103771416553));
#37042=CARTESIAN_POINT('Ctrl Pts',(1.97131603149074,4.48867159166511,35.6897490317087));
#37043=CARTESIAN_POINT('Ctrl Pts',(-0.415681816248198,4.88482017903162,
35.7691209217621));
#37044=CARTESIAN_POINT('Ctrl Pts',(-2.70142049364518,4.09103738315207,35.8484928118155));
#37045=CARTESIAN_POINT('Ctrl Pts',(-4.32909911828301,2.30068693609431,35.9278647018689));
#37046=CARTESIAN_POINT('Ctrl Pts',(-4.90221878000546,-0.0501057561118174,
36.0072365919223));
#37047=CARTESIAN_POINT('Ctrl Pts',(-4.28116879779583,-2.38869279703632,
36.0866084819757));
#37048=CARTESIAN_POINT('Ctrl Pts',(-2.61723557264952,-4.14539955988464,
36.1659803720291));
#37049=CARTESIAN_POINT('Ctrl Pts',(-0.315749555158452,-4.89229616563135,
36.2453522620825));
#37050=CARTESIAN_POINT('Ctrl Pts',(2.06265235506943,-4.44744025434409,36.3247241521359));
#37051=CARTESIAN_POINT('Ctrl Pts',(3.93859671720591,-2.9191977413407,36.4040960421893));
#37052=CARTESIAN_POINT('Ctrl Pts',(4.85510763696701,-0.679845120081316,
36.4834679322428));
#37053=CARTESIAN_POINT('Ctrl Pts',(4.58892508296144,1.72511626761826,36.5628398222961));
#37054=CARTESIAN_POINT('Ctrl Pts',(3.20489053615983,3.70984315100612,36.6422117123496));
#37055=CARTESIAN_POINT('Ctrl Pts',(1.04015174865454,4.7908604544074,36.721583602403));
#37056=CARTESIAN_POINT('Ctrl Pts',(-1.37796570248609,4.70483475550478,36.8009554924563));
#37057=CARTESIAN_POINT('Ctrl Pts',(-3.46041375857649,3.47272172413633,36.8803273825098));
#37058=CARTESIAN_POINT('Ctrl Pts',(-4.69991268257361,1.39466136750738,36.9596992725631));
#37059=CARTESIAN_POINT('Ctrl Pts',(-4.79452328017606,-1.02313541121578,
37.0390711626166));
#37060=CARTESIAN_POINT('Ctrl Pts',(-3.72119861922486,-3.19169866843862,
37.11844305267));
#37061=CARTESIAN_POINT('Ctrl Pts',(-1.74139821136397,-4.5827711947349,37.1978149427234));
#37062=CARTESIAN_POINT('Ctrl Pts',(0.66260294626563,-4.85749080178586,37.2771868327768));
#37063=CARTESIAN_POINT('Ctrl Pts',(2.90519549283168,-3.94893640139516,37.3565587228302));
#37064=CARTESIAN_POINT('Ctrl Pts',(4.44008884788513,-2.07842983444732,37.4359306128835));
#37065=CARTESIAN_POINT('Ctrl Pts',(4.8933863875636,0.298377639646022,37.515302502937));
#37066=CARTESIAN_POINT('Ctrl Pts',(4.15466583455884,2.60250098116825,37.5946743929904));
#37067=CARTESIAN_POINT('Ctrl Pts',(2.40387788045201,4.272660844218,37.6740462830438));
#37068=CARTESIAN_POINT('Ctrl Pts',(0.0675105955612736,4.90200998298708,
37.7534181730972));
#37069=CARTESIAN_POINT('Ctrl Pts',(-2.28530212097756,4.33724034032229,37.8327900631506));
#37070=CARTESIAN_POINT('Ctrl Pts',(-4.08142029927378,2.71592855106086,37.9121619532041));
#37071=CARTESIAN_POINT('Ctrl Pts',(-4.883313526743,0.433022578390986,37.9915338432574));
#37072=CARTESIAN_POINT('Ctrl Pts',(-4.49564238811839,-1.95536673594121,
38.0709057333108));
#37073=CARTESIAN_POINT('Ctrl Pts',(-3.01284271470332,-3.86743304144309,
38.1502776233642));
#37074=CARTESIAN_POINT('Ctrl Pts',(-0.796121224763853,-4.8374012186294,
38.2296495134176));
#37075=CARTESIAN_POINT('Ctrl Pts',(1.61453363327388,-4.62898916605744,38.309021403471));
#37076=CARTESIAN_POINT('Ctrl Pts',(3.63189167208741,-3.29296559930574,38.3883932935244));
#37077=CARTESIAN_POINT('Ctrl Pts',(4.76452893838759,-1.15478290032729,38.4677651835778));
#37078=CARTESIAN_POINT('Ctrl Pts',(4.73653750187218,1.26470235504111,38.5471370736312));
#37079=CARTESIAN_POINT('Ctrl Pts',(3.55473601316178,3.37610891998471,38.6265089636846));
#37080=CARTESIAN_POINT('Ctrl Pts',(1.50700870159436,4.66510281756139,38.705880853738));
#37081=CARTESIAN_POINT('Ctrl Pts',(-0.907822597135966,4.81768800868639,
38.7852527437914));
#37082=CARTESIAN_POINT('Ctrl Pts',(-3.10151031466514,3.79669503846564,38.8646246338448));
#37083=CARTESIAN_POINT('Ctrl Pts',(-4.53967699589137,1.85083561019,38.9439965238982));
#37084=CARTESIAN_POINT('Ctrl Pts',(-4.87198838803768,-0.545883369388725,
39.0233684139517));
#37085=CARTESIAN_POINT('Ctrl Pts',(-4.01749423301241,-2.80962619208844,
39.102740304005));
#37086=CARTESIAN_POINT('Ctrl Pts',(-2.18434729950916,-4.38895062645438,
39.1821121940585));
#37087=CARTESIAN_POINT('Ctrl Pts',(0.180901657890313,-4.89913577411435,
39.2614840841118));
#37088=CARTESIAN_POINT('Ctrl Pts',(2.50208364241399,-4.21590347870473,39.3408559741653));
#37089=CARTESIAN_POINT('Ctrl Pts',(4.21376307902776,-2.50568418547649,39.4202278642187));
#37090=CARTESIAN_POINT('Ctrl Pts',(4.89898012125377,-0.185090004541199,
39.4995997542721));
#37091=CARTESIAN_POINT('Ctrl Pts',(4.39081462818005,2.18059968579169,39.5789716443255));
#37092=CARTESIAN_POINT('Ctrl Pts',(2.81305984991034,4.01508502497055,39.6583435343788));
#37093=CARTESIAN_POINT('Ctrl Pts',(0.55004342451412,4.87153304143481,39.7377154244323));
#37094=CARTESIAN_POINT('Ctrl Pts',(-1.84695009786503,4.54123256689917,39.8170873144857));
#37095=CARTESIAN_POINT('Ctrl Pts',(-3.79405383067523,3.10479958283119,39.8964592045391));
#37096=CARTESIAN_POINT('Ctrl Pts',(-4.8168906266497,0.911851793294956,39.9758310945925));
#37097=CARTESIAN_POINT('Ctrl Pts',(-4.66642692152748,-1.50285363850387,
40.0552029846459));
#37098=CARTESIAN_POINT('Ctrl Pts',(-3.37906911267765,-3.55219315325672,
40.1345748746994));
#37099=CARTESIAN_POINT('Ctrl Pts',(-1.9723130827443,-4.34047654372169,40.1874894680682));
#37100=CARTESIAN_POINT('Ctrl Pts',(-1.21713437249821,-4.54280821229862,
40.2139467647527));
#37101=CARTESIAN_POINT('Ctrl Pts',(-3.71544298812222,3.17665283523783,-0.213946764752703));
#37102=CARTESIAN_POINT('Ctrl Pts',(-4.2435173595033,2.55901209131059,-0.187489468068236));
#37103=CARTESIAN_POINT('Ctrl Pts',(-4.98521092249169,1.05595859527115,-0.1345748746993));
#37104=CARTESIAN_POINT('Ctrl Pts',(-4.8827252805975,-1.45743906270739,-0.0552029846458962));
#37105=CARTESIAN_POINT('Ctrl Pts',(-3.59110607910258,-3.61508997874938,
0.0241689054075074));
#37106=CARTESIAN_POINT('Ctrl Pts',(-1.42455668503541,-4.89247688957836,
0.103540795460911));
#37107=CARTESIAN_POINT('Ctrl Pts',(1.08893586889099,-4.9778765288597,0.182912685514315));
#37108=CARTESIAN_POINT('Ctrl Pts',(3.33720602914152,-3.85077723115681,0.262284575567719));
#37109=CARTESIAN_POINT('Ctrl Pts',(4.77251903131815,-1.78558378675016,0.341656465621122));
#37110=CARTESIAN_POINT('Ctrl Pts',(5.04526816392178,0.714545672093079,0.421028355674526));
#37111=CARTESIAN_POINT('Ctrl Pts',(4.0889952065405,3.04062834435892,0.500400245727928));
#37112=CARTESIAN_POINT('Ctrl Pts',(2.13665520967362,4.62601276074604,0.579772135781332));
#37113=CARTESIAN_POINT('Ctrl Pts',(-0.336170930871067,5.08451490337719,
0.659144025834737));
#37114=CARTESIAN_POINT('Ctrl Pts',(-2.72710569549275,4.30443824810499,0.738515915888139));
#37115=CARTESIAN_POINT('Ctrl Pts',(-4.45372401575963,2.47581113999331,0.817887805941545));
#37116=CARTESIAN_POINT('Ctrl Pts',(-5.09542477676098,0.0440812951164733,
0.897259695994947));
#37117=CARTESIAN_POINT('Ctrl Pts',(-4.49589147158092,-2.39838632564101,
0.976631586048351));
#37118=CARTESIAN_POINT('Ctrl Pts',(-2.80116888608231,-4.25661252099957,
1.05600347610176));
#37119=CARTESIAN_POINT('Ctrl Pts',(-0.424087796932823,-5.07793723552562,
1.13537536615516));
#37120=CARTESIAN_POINT('Ctrl Pts',(2.05630016029234,-4.66228772832596,1.21474725620856));
#37121=CARTESIAN_POINT('Ctrl Pts',(4.03577793971522,-3.11091522434116,1.29411914626197));
#37122=CARTESIAN_POINT('Ctrl Pts',(5.03214915152042,-0.801730671351417,
1.37349103631537));
#37123=CARTESIAN_POINT('Ctrl Pts',(4.80269996559999,1.70275370586111,1.45286292636877));
#37124=CARTESIAN_POINT('Ctrl Pts',(3.40332370018522,3.79245104545052,1.53223481642218));
#37125=CARTESIAN_POINT('Ctrl Pts',(1.17490531372441,4.95831570685873,1.61160670647558));
#37126=CARTESIAN_POINT('Ctrl Pts',(-1.33971740612181,4.9163456360401,1.69097859652898));
#37127=CARTESIAN_POINT('Ctrl Pts',(-3.52798793147818,3.67676465100145,1.77035048658239));
#37128=CARTESIAN_POINT('Ctrl Pts',(-4.85684840567494,1.54153193505596,1.84972237663579));
#37129=CARTESIAN_POINT('Ctrl Pts',(-5.00259135876462,-0.969214547985408,
1.9290942666892));
#37130=CARTESIAN_POINT('Ctrl Pts',(-3.92971412987363,-3.24386251254264,
2.0084661567426));
#37131=CARTESIAN_POINT('Ctrl Pts',(-1.89956723723801,-4.72831274916731,
2.087838046796));
#37132=CARTESIAN_POINT('Ctrl Pts',(0.593310029777512,-5.06095646606144,
2.16720993684941));
#37133=CARTESIAN_POINT('Ctrl Pts',(2.94165828680369,-4.16076239004749,2.24658182690281));
#37134=CARTESIAN_POINT('Ctrl Pts',(4.57342509641733,-2.24701580551599,2.32595371695621));
#37135=CARTESIAN_POINT('Ctrl Pts',(5.09111567564703,0.214098855557618,2.40532560700962));
#37136=CARTESIAN_POINT('Ctrl Pts',(4.36862174528326,2.62305950931529,2.48469749706302));
#37137=CARTESIAN_POINT('Ctrl Pts',(2.58194122754832,4.39304867264849,2.56406938711643));
#37138=CARTESIAN_POINT('Ctrl Pts',(0.166305541812792,5.09290090317231,2.64344127716983));
#37139=CARTESIAN_POINT('Ctrl Pts',(-2.28984180579737,4.55213374662856,2.72281316722323));
#37140=CARTESIAN_POINT('Ctrl Pts',(-4.18818875799412,2.90247688538309,2.80218505727664));
#37141=CARTESIAN_POINT('Ctrl Pts',(-5.06630219914209,0.545783079381991,
2.88155694733003));
#37142=CARTESIAN_POINT('Ctrl Pts',(-4.71027563864874,-1.94386227668626,
2.96092883738345));
#37143=CARTESIAN_POINT('Ctrl Pts',(-3.20683635859883,-3.95998708481986,
3.04030072743684));
#37144=CARTESIAN_POINT('Ctrl Pts',(-0.922218839806132,-5.01146780437411,
3.11967261749025));
#37145=CARTESIAN_POINT('Ctrl Pts',(1.58704914706656,-4.84216605947864,3.19904450754365));
#37146=CARTESIAN_POINT('Ctrl Pts',(3.70971547458753,-3.49332338044696,3.27841639759706));
#37147=CARTESIAN_POINT('Ctrl Pts',(4.92870332381492,-1.29351485827855,3.35778828765046));
#37148=CARTESIAN_POINT('Ctrl Pts',(4.94706995286075,1.22139102021994,3.43716017770387));
#37149=CARTESIAN_POINT('Ctrl Pts',(3.76034129154331,3.43876874969603,3.51653206775727));
#37150=CARTESIAN_POINT('Ctrl Pts',(1.65760181498019,4.81847002333168,3.59590395781068));
#37151=CARTESIAN_POINT('Ctrl Pts',(-0.848925794672718,5.02440266478622,
3.67527584786407));
#37152=CARTESIAN_POINT('Ctrl Pts',(-3.14865695980872,4.00640193842551,3.75464773791748));
#37153=CARTESIAN_POINT('Ctrl Pts',(-4.68138225896931,2.01245056788461,3.83401962797088));
#37154=CARTESIAN_POINT('Ctrl Pts',(-5.07373320190881,-0.471729306509208,
3.91339151802429));
#37155=CARTESIAN_POINT('Ctrl Pts',(-4.23013396738131,-2.84099696599249,
3.99276340807769));
#37156=CARTESIAN_POINT('Ctrl Pts',(-2.3560834616424,-4.51820405300012,4.0721352981311));
#37157=CARTESIAN_POINT('Ctrl Pts',(0.0919037602502722,-5.09478663357196,
4.1515071881845));
#37158=CARTESIAN_POINT('Ctrl Pts',(2.51750342957152,-4.43029046732459,4.2308790782379));
#37159=CARTESIAN_POINT('Ctrl Pts',(4.32984483584847,-2.6865853495186,4.3102509682913));
#37160=CARTESIAN_POINT('Ctrl Pts',(5.08744562406172,-0.288433987225658,
4.38962285834471));
#37161=CARTESIAN_POINT('Ctrl Pts',(4.60575591912341,2.17997925591765,4.46899474839811));
#37162=CARTESIAN_POINT('Ctrl Pts',(3.00211426695445,4.11735437762165,4.54836663845152));
#37163=CARTESIAN_POINT('Ctrl Pts',(0.667164224422586,5.05175108654635,4.62773852850492));
#37164=CARTESIAN_POINT('Ctrl Pts',(-1.83030554643563,4.75555241264972,4.70711041855833));
#37165=CARTESIAN_POINT('Ctrl Pts',(-3.88191693749475,3.30091169726834,4.78648230861172));
#37166=CARTESIAN_POINT('Ctrl Pts',(-4.98790195505755,1.04217619887652,4.86585419866514));
#37167=CARTESIAN_POINT('Ctrl Pts',(-4.87884509690204,-1.47043111474375,
4.94522608871853));
#37168=CARTESIAN_POINT('Ctrl Pts',(-3.58131237228163,-3.62484466355651,
5.02459797877194));
#37169=CARTESIAN_POINT('Ctrl Pts',(-1.4113798808739,-4.89625407578446,5.10396986882534));
#37170=CARTESIAN_POINT('Ctrl Pts',(1.10236162547835,-4.97494683282589,5.18334175887874));
#37171=CARTESIAN_POINT('Ctrl Pts',(3.34757027990012,-3.84175355324895,5.26271364893216));
#37172=CARTESIAN_POINT('Ctrl Pts',(4.77731822385938,-1.77271761167783,5.34208553898555));
#37173=CARTESIAN_POINT('Ctrl Pts',(5.04332202290099,0.728148416254135,5.42145742903896));
#37174=CARTESIAN_POINT('Ctrl Pts',(4.0807837403679,3.05163910171577,5.50082931909235));
#37175=CARTESIAN_POINT('Ctrl Pts',(2.12417557134277,4.63175725668802,5.58020120914577));
#37176=CARTESIAN_POINT('Ctrl Pts',(-0.349877065078572,5.08358959615188,
5.65957309919917));
#37177=CARTESIAN_POINT('Ctrl Pts',(-2.73870042288654,4.29707076232783,5.73894498925257));
#37178=CARTESIAN_POINT('Ctrl Pts',(-4.46038241968988,2.46379500220554,5.81831687930597));
#37179=CARTESIAN_POINT('Ctrl Pts',(-5.09552513194581,0.0303442330637155,
5.89768876935938));
#37180=CARTESIAN_POINT('Ctrl Pts',(-4.48940920081331,-2.41049832408661,
5.97706065941278));
#37181=CARTESIAN_POINT('Ctrl Pts',(-2.78968312550141,-4.26414882503699,
6.05643254946618));
#37182=CARTESIAN_POINT('Ctrl Pts',(-0.410396415676208,-5.07906211074168,
6.13580443951959));
#37183=CARTESIAN_POINT('Ctrl Pts',(2.06886195261065,-4.65672710858298,6.21517632957299));
#37184=CARTESIAN_POINT('Ctrl Pts',(4.04415012858982,-3.10002369026409,6.2945482196264));
#37185=CARTESIAN_POINT('Ctrl Pts',(5.03429228481897,-0.788161362782912,
6.37392010967979));
#37186=CARTESIAN_POINT('Ctrl Pts',(4.79809198368318,1.7156953281066,6.45329199973321));
#37187=CARTESIAN_POINT('Ctrl Pts',(3.39308709571864,3.80161243469653,6.5326638897866));
#37188=CARTESIAN_POINT('Ctrl Pts',(1.16153370170793,4.96146516692078,6.61203577984001));
#37189=CARTESIAN_POINT('Ctrl Pts',(-1.35296673102758,4.91271596650001,6.69140766989341));
#37190=CARTESIAN_POINT('Ctrl Pts',(-3.53788746282585,3.66724003075218,6.77077955994682));
#37191=CARTESIAN_POINT('Ctrl Pts',(-4.8609866396608,1.52843254081124,6.85015145000022));
#37192=CARTESIAN_POINT('Ctrl Pts',(-4.99996023068582,-0.982697732943262,
6.92952334005363));
#37193=CARTESIAN_POINT('Ctrl Pts',(-3.92095457674001,-3.25444501411732,
7.00889523010702));
#37194=CARTESIAN_POINT('Ctrl Pts',(-1.8868130667861,-4.73341669344426,7.08826712016043));
#37195=CARTESIAN_POINT('Ctrl Pts',(0.606951929847044,-5.05933854348832,
7.16763901021384));
#37196=CARTESIAN_POINT('Ctrl Pts',(2.95286477983474,-4.15281672299454,7.24701090026724));
#37197=CARTESIAN_POINT('Ctrl Pts',(4.57946630551004,-2.23467794088318,7.32638279032065));
#37198=CARTESIAN_POINT('Ctrl Pts',(5.0905199756398,0.227823441251604,7.40575468037404));
#37199=CARTESIAN_POINT('Ctrl Pts',(4.36153424737857,2.63482753737611,7.48512657042746));
#37200=CARTESIAN_POINT('Ctrl Pts',(2.57008843054822,4.39999347748764,7.56449846048085));
#37201=CARTESIAN_POINT('Ctrl Pts',(0.152574760830579,5.09333074570355,7.64387035053426));
#37202=CARTESIAN_POINT('Ctrl Pts',(-2.3021057829069,4.54594391816246,7.72324224058766));
#37203=CARTESIAN_POINT('Ctrl Pts',(-4.19599845355297,2.89117521443317,7.80261413064106));
#37204=CARTESIAN_POINT('Ctrl Pts',(-5.06775518859857,0.532122627975753,
7.88198602069447));
#37205=CARTESIAN_POINT('Ctrl Pts',(-4.70501797698741,-1.95655385282311,
7.96135791074787));
#37206=CARTESIAN_POINT('Ctrl Pts',(-3.19614880056275,-3.96861814583273,
8.04072980080128));
#37207=CARTESIAN_POINT('Ctrl Pts',(-0.908704850876407,-5.01393584290478,
8.12010169085468));
#37208=CARTESIAN_POINT('Ctrl Pts',(1.60009758909935,-4.83786986680398,8.19947358090808));
#37209=CARTESIAN_POINT('Ctrl Pts',(3.71911979812647,-3.48330949959307,8.27884547096148));
#37210=CARTESIAN_POINT('Ctrl Pts',(4.93217265646204,-1.28022264845606,8.3582173610149));
#37211=CARTESIAN_POINT('Ctrl Pts',(4.94375917286243,1.23472360612009,8.43758925106829));
#37212=CARTESIAN_POINT('Ctrl Pts',(3.75105689757885,3.4488939232597,8.5169611411217));
#37213=CARTESIAN_POINT('Ctrl Pts',(1.64460546486869,4.82292131469047,8.5963330311751));
#37214=CARTESIAN_POINT('Ctrl Pts',(-0.862468218811062,5.02209574921791,
8.67570492122851));
#37215=CARTESIAN_POINT('Ctrl Pts',(-3.15944655342946,3.99789877545622,8.75507681128191));
#37216=CARTESIAN_POINT('Ctrl Pts',(-4.68679070094874,1.99982250919225,8.83444870133531));
#37217=CARTESIAN_POINT('Ctrl Pts',(-5.07244300775217,-0.485406093778898,
8.91382059138872));
#37218=CARTESIAN_POINT('Ctrl Pts',(-4.22245942552934,-2.85239084673368,
8.99319248144211));
#37219=CARTESIAN_POINT('Ctrl Pts',(-2.34389407350296,-4.52453950308418,
9.07256437149552));
#37220=CARTESIAN_POINT('Ctrl Pts',(0.105638686707185,-5.09452035138171,
9.15193626154893));
#37221=CARTESIAN_POINT('Ctrl Pts',(2.52943809666274,-4.42348731861218,9.23130815160232));
#37222=CARTESIAN_POINT('Ctrl Pts',(4.33707198508751,-2.67490256625183,9.31068004165574));
#37223=CARTESIAN_POINT('Ctrl Pts',(5.08820473789098,-0.274717469548947,
9.39005193170913));
#37224=CARTESIAN_POINT('Ctrl Pts',(4.59986207909436,2.19238819465928,9.46942382176255));
#37225=CARTESIAN_POINT('Ctrl Pts',(2.99100319945234,4.12543294741746,9.54879571181595));
#37226=CARTESIAN_POINT('Ctrl Pts',(0.653542560897033,5.05353136567566,9.62816760186935));
#37227=CARTESIAN_POINT('Ctrl Pts',(-1.84311959890086,4.75060072905723,9.70753949192275));
#37228=CARTESIAN_POINT('Ctrl Pts',(-3.89080190408257,3.29043427011681,9.78691138197615));
#37229=CARTESIAN_POINT('Ctrl Pts',(-4.99069347757367,1.02872530622863,9.86628327202957));
#37230=CARTESIAN_POINT('Ctrl Pts',(-4.87486316664046,-1.48357886521197,
9.94565516208295));
#37231=CARTESIAN_POINT('Ctrl Pts',(-3.57152697864026,-3.63448650893304,
10.0250270521364));
#37232=CARTESIAN_POINT('Ctrl Pts',(-1.39817472408419,-4.90004128387748,
10.1043989421898));
#37233=CARTESIAN_POINT('Ctrl Pts',(1.11576979845155,-4.9719568481268,10.1837708322432));
#37234=CARTESIAN_POINT('Ctrl Pts',(3.35791526779908,-3.83271472941224,10.2631427222966));
#37235=CARTESIAN_POINT('Ctrl Pts',(4.7820800105301,-1.75983178618299,10.34251461235));
#37236=CARTESIAN_POINT('Ctrl Pts',(5.04134064765054,0.741742284838825,10.4218865024034));
#37237=CARTESIAN_POINT('Ctrl Pts',(4.07254186182158,3.0626295770926,10.5012583924568));
#37238=CARTESIAN_POINT('Ctrl Pts',(2.11168089287137,4.63746708338223,10.5806302825102));
#37239=CARTESIAN_POINT('Ctrl Pts',(-0.363580867455945,5.08262787301918,
10.6600021725636));
#37240=CARTESIAN_POINT('Ctrl Pts',(-2.75027513324356,4.28967176299466,10.739374062617));
#37241=CARTESIAN_POINT('Ctrl Pts',(-4.46700846420381,2.45176110653202,10.8187459526704));
#37242=CARTESIAN_POINT('Ctrl Pts',(-5.09558842083953,0.0166068713993523,
10.8981178427238));
#37243=CARTESIAN_POINT('Ctrl Pts',(-4.48289431705241,-2.42259276084751,
10.9774897327772));
#37244=CARTESIAN_POINT('Ctrl Pts',(-2.77817708034959,-4.27165415887005,
11.0568616228306));
#37245=CARTESIAN_POINT('Ctrl Pts',(-0.396702056264276,-5.08015005893795,
11.136233512884));
#37246=CARTESIAN_POINT('Ctrl Pts',(2.0814087106419,-4.65113264937,11.2156054029374));
#37247=CARTESIAN_POINT('Ctrl Pts',(4.05249292275577,-3.08910962152302,11.2949772929908));
#37248=CARTESIAN_POINT('Ctrl Pts',(5.03639882892726,-0.774586327501172,
11.3743491830442));
#37249=CARTESIAN_POINT('Ctrl Pts',(4.79344912825178,1.7286244813822,11.4537210730976));
#37250=CARTESIAN_POINT('Ctrl Pts',(3.38282583005384,3.81074619284624,11.533092963151));
#37251=CARTESIAN_POINT('Ctrl Pts',(1.14815364741277,4.96457856667656,11.6124648532044));
#37252=CARTESIAN_POINT('Ctrl Pts',(-1.36620622234309,4.90905059057276,11.6918367432579));
#37253=CARTESIAN_POINT('Ctrl Pts',(-3.54776128038234,3.65768875660455,11.7712086333112));
#37254=CARTESIAN_POINT('Ctrl Pts',(-4.86508954335683,1.51532203768426,11.8505805233647));
#37255=CARTESIAN_POINT('Ctrl Pts',(-4.99729276226266,-0.9961737755075,11.9299524134181));
#37256=CARTESIAN_POINT('Ctrl Pts',(-3.91216652560121,-3.26500386197887,
12.0093243034715));
#37257=CARTESIAN_POINT('Ctrl Pts',(-1.87404518273703,-4.73848623463566,
12.0886961935249));
#37258=CARTESIAN_POINT('Ctrl Pts',(0.620589418513222,-5.05768384899659,
12.1680680835782));
#37259=CARTESIAN_POINT('Ctrl Pts',(2.96404981106505,-4.14484087273527,12.2474399736317));
#37260=CARTESIAN_POINT('Ctrl Pts',(4.58547423045439,-2.2223238343253,12.3268118636851));
#37261=CARTESIAN_POINT('Ctrl Pts',(5.08988727708011,0.241546371095948,12.4061837537385));
#37262=CARTESIAN_POINT('Ctrl Pts',(4.3544150492835,2.64657641517207,12.4855556437919));
#37263=CARTESIAN_POINT('Ctrl Pts',(2.55821695381563,4.40690630260979,12.5649275338453));
#37264=CARTESIAN_POINT('Ctrl Pts',(0.138842870915485,5.09372356925339,12.6442994238987));
#37265=CARTESIAN_POINT('Ctrl Pts',(-2.3143530280162,4.53972104919276,12.7236713139521));
#37266=CARTESIAN_POINT('Ctrl Pts',(-4.20377765205669,2.87985253005087,12.8030432040055));
#37267=CARTESIAN_POINT('Ctrl Pts',(-5.06917134496016,0.518458309034014,
12.8824150940589));
#37268=CARTESIAN_POINT('Ctrl Pts',(-4.69972611865178,-1.9692312084755,12.9617869841123));
#37269=CARTESIAN_POINT('Ctrl Pts',(-3.18543801250715,-3.97722036241972,
13.0411588741657));
#37270=CARTESIAN_POINT('Ctrl Pts',(-0.895184257363228,-5.01636743950647,
13.1205307642191));
#37271=CARTESIAN_POINT('Ctrl Pts',(1.61313440141763,-4.83353851187042,13.1999026542725));
#37272=CARTESIAN_POINT('Ctrl Pts',(3.72849709062559,-3.47327030159879,13.2792745443259));
#37273=CARTESIAN_POINT('Ctrl Pts',(4.93560614144549,-1.26692113381109,13.3586464343793));
#37274=CARTESIAN_POINT('Ctrl Pts',(4.94041246098816,1.24804721789062,13.4380183244327));
#37275=CARTESIAN_POINT('Ctrl Pts',(3.74174524045162,3.45899402981983,13.5173902144861));
#37276=CARTESIAN_POINT('Ctrl Pts',(1.63159716155366,4.82733755243838,13.5967621045395));
#37277=CARTESIAN_POINT('Ctrl Pts',(-0.87600437441973,5.01975233241333,13.6761339945929));
#37278=CARTESIAN_POINT('Ctrl Pts',(-3.17021318378723,3.98936655524573,13.7555058846463));
#37279=CARTESIAN_POINT('Ctrl Pts',(-4.69216507873203,1.98717991553337,13.8348777746998));
#37280=CARTESIAN_POINT('Ctrl Pts',(-5.07111594642896,-0.499079353054812,
13.9142496647532));
#37281=CARTESIAN_POINT('Ctrl Pts',(-4.21475419430051,-2.86376399593225,
13.9936215548066));
#37282=CARTESIAN_POINT('Ctrl Pts',(-2.33168764964064,-4.53084206823465,
14.07299344486));
#37283=CARTESIAN_POINT('Ctrl Pts',(0.119372845368581,-5.09421704156391,
14.1523653349133));
#37284=CARTESIAN_POINT('Ctrl Pts',(2.54135437947334,-4.4166520194264,14.2317372249668));
#37285=CARTESIAN_POINT('Ctrl Pts',(4.34426761193091,-2.66320034145004,14.3111091150202));
#37286=CARTESIAN_POINT('Ctrl Pts',(5.08892686999541,-0.260998955190403,
14.3904810050736));
#37287=CARTESIAN_POINT('Ctrl Pts',(4.59393480667753,2.20478119884224,14.469852895127));
#37288=CARTESIAN_POINT('Ctrl Pts',(2.97987039295526,4.13348153303728,14.5492247851804));
#37289=CARTESIAN_POINT('Ctrl Pts',(0.639916147340316,5.05527491509065,14.6285966752338));
#37290=CARTESIAN_POINT('Ctrl Pts',(-1.85592025533638,4.74561451748915,14.7079685652872));
#37291=CARTESIAN_POINT('Ctrl Pts',(-3.89965859182293,3.27993292766684,14.7873404553406));
#37292=CARTESIAN_POINT('Ctrl Pts',(-4.99344872708928,1.01526693667329,14.866712345394));
#37293=CARTESIAN_POINT('Ctrl Pts',(-4.87084580524798,-1.49671583283861,
14.9460842354474));
#37294=CARTESIAN_POINT('Ctrl Pts',(-3.56171562668257,-3.64410193839537,
15.0254561255008));
#37295=CARTESIAN_POINT('Ctrl Pts',(-1.38495940518108,-4.90379287784181,
15.1048280155542));
#37296=CARTESIAN_POINT('Ctrl Pts',(1.12916986186683,-4.9689307266074,15.1841999056076));
#37297=CARTESIAN_POINT('Ctrl Pts',(3.36823584993909,-3.82364804891307,15.263571795661));
#37298=CARTESIAN_POINT('Ctrl Pts',(4.78680704042976,-1.74693317000493,15.3429436857144));
#37299=CARTESIAN_POINT('Ctrl Pts',(5.0393226312895,0.755330762345426,15.4223155757678));
#37300=CARTESIAN_POINT('Ctrl Pts',(4.06427038351844,3.07359779288479,15.5016874658212));
#37301=CARTESIAN_POINT('Ctrl Pts',(2.09917086643239,4.64314320437064,15.5810593558746));
#37302=CARTESIAN_POINT('Ctrl Pts',(-0.377282027281083,5.08162920869508,
15.660431245928));
#37303=CARTESIAN_POINT('Ctrl Pts',(-2.76182985424771,4.28224158577663,15.7398031359814));
#37304=CARTESIAN_POINT('Ctrl Pts',(-4.47360204192776,2.43970939114443,15.8191750260348));
#37305=CARTESIAN_POINT('Ctrl Pts',(-5.09561467434161,0.00286938903366673,
15.8985469160882));
#37306=CARTESIAN_POINT('Ctrl Pts',(-4.47634685104277,-2.43466958989267,
15.9779188061416));
#37307=CARTESIAN_POINT('Ctrl Pts',(-2.76665084304587,-4.27912844577413,
16.0572906961951));
#37308=CARTESIAN_POINT('Ctrl Pts',(-0.383004813579153,-5.08120108394907,
16.1366625862484));
#37309=CARTESIAN_POINT('Ctrl Pts',(2.09394034074345,-4.64550438513334,16.2160344763019));
#37310=CARTESIAN_POINT('Ctrl Pts',(4.06080626285358,-3.07817310072693,16.2954063663552));
#37311=CARTESIAN_POINT('Ctrl Pts',(5.03846876789878,-0.761005662445124,
16.3747782564087));
#37312=CARTESIAN_POINT('Ctrl Pts',(4.7887714333112,1.74154107082836,16.4541501464621));
#37313=CARTESIAN_POINT('Ctrl Pts',(3.37253997777685,3.81985225393751,16.5335220365155));
#37314=CARTESIAN_POINT('Ctrl Pts',(1.13476524781198,4.96765588336339,16.6128939265689));
#37315=CARTESIAN_POINT('Ctrl Pts',(-1.37943578318358,4.90534953479992,16.6922658166222));
#37316=CARTESIAN_POINT('Ctrl Pts',(-3.5576093137008,3.64811089835147,16.7716377066757));
#37317=CARTESIAN_POINT('Ctrl Pts',(-4.86915708441607,1.50220052016076,16.851009596729));
#37318=CARTESIAN_POINT('Ctrl Pts',(-4.99458897767399,-1.00964257616395,
16.9303814867825));
#37319=CARTESIAN_POINT('Ctrl Pts',(-3.90335003127183,-3.2755389823738,17.0097533768359));
#37320=CARTESIAN_POINT('Ctrl Pts',(-1.8612636949986,-4.74352133023597,17.0891252668893));
#37321=CARTESIAN_POINT('Ctrl Pts',(0.634222428965914,-5.05599240530682,
17.1684971569427));
#37322=CARTESIAN_POINT('Ctrl Pts',(2.9752132381933,-4.13683487704247,17.2478690469961));
#37323=CARTESIAN_POINT('Ctrl Pts',(4.59144894277892,-2.20995361377096,17.3272409370495));
#37324=CARTESIAN_POINT('Ctrl Pts',(5.08921736705481,0.255267617363485,17.4066128271029));
#37325=CARTESIAN_POINT('Ctrl Pts',(4.34726461344772,2.65830592133578,17.4859847171563));
#37326=CARTESIAN_POINT('Ctrl Pts',(2.54632610813648,4.41378735452059,17.5653566072097));
#37327=CARTESIAN_POINT('Ctrl Pts',(0.125111436169681,5.09407888617233,17.6447284972631));
#37328=CARTESIAN_POINT('Ctrl Pts',(-2.32658621700147,4.53346610033861,17.7241003873165));
#37329=CARTESIAN_POINT('Ctrl Pts',(-4.21152107628919,2.8685071860873,17.8034722773699));
#37330=CARTESIAN_POINT('Ctrl Pts',(-5.07056051563183,0.504793485523745,
17.8828441674233));
#37331=CARTESIAN_POINT('Ctrl Pts',(-4.69438148876582,-1.98190041394314,
17.9622160574767));
#37332=CARTESIAN_POINT('Ctrl Pts',(-3.1747392180444,-3.9857820361196,18.0415879475301));
#37333=CARTESIAN_POINT('Ctrl Pts',(-0.881590795203727,-5.01878454751455,
18.1209598375835));
#37334=CARTESIAN_POINT('Ctrl Pts',(1.62603418385021,-4.82913054051801,18.2003317276369));
#37335=CARTESIAN_POINT('Ctrl Pts',(3.73808388472066,-3.46328419200805,18.2797036176903));
#37336=CARTESIAN_POINT('Ctrl Pts',(4.93855701420293,-1.25346250930793,18.3590755077438));
#37337=CARTESIAN_POINT('Ctrl Pts',(4.93787328845974,1.26108254025623,18.4384473977971));
#37338=CARTESIAN_POINT('Ctrl Pts',(3.73081451079157,3.46959580775143,18.5178192878506));
#37339=CARTESIAN_POINT('Ctrl Pts',(1.62157688245111,4.83072732396141,18.597191177904));
#37340=CARTESIAN_POINT('Ctrl Pts',(-0.895150293053049,5.01921699961797,
18.6765630679574));
#37341=CARTESIAN_POINT('Ctrl Pts',(-3.17074515011531,3.97754537770249,18.7559349580108));
#37342=CARTESIAN_POINT('Ctrl Pts',(-5.22808970274021,1.31272284990122,18.8617641447486));
#37343=CARTESIAN_POINT('Ctrl Pts',(-4.77339715849023,-3.25411141853201,
18.994050628171));
#37344=CARTESIAN_POINT('Ctrl Pts',(0.152720854580862,-5.77834717219764,
19.1527944082778));
#37345=CARTESIAN_POINT('Ctrl Pts',(4.93271294602037,-3.00474199436408,19.3115381883846));
#37346=CARTESIAN_POINT('Ctrl Pts',(5.20235975367847,2.51303602329821,19.4702819684914));
#37347=CARTESIAN_POINT('Ctrl Pts',(0.709818611660393,5.73400533709388,19.6290257485982));
#37348=CARTESIAN_POINT('Ctrl Pts',(-4.43131449514935,3.70671199728522,19.787769528705));
#37349=CARTESIAN_POINT('Ctrl Pts',(-5.51805139390214,-1.71188403765749,
19.9465133088118));
#37350=CARTESIAN_POINT('Ctrl Pts',(-1.55524717023727,-5.56394358573197,
20.1052570889187));
#37351=CARTESIAN_POINT('Ctrl Pts',(3.83058845612614,-4.32541925679744,20.2640008690254));
#37352=CARTESIAN_POINT('Ctrl Pts',(5.71123844601177,0.87272703286029,20.4227446491323));
#37353=CARTESIAN_POINT('Ctrl Pts',(2.36591519662234,5.26902047281308,20.581488429239));
#37354=CARTESIAN_POINT('Ctrl Pts',(-3.14459942082001,4.85016640791291,20.7402322093459));
#37355=CARTESIAN_POINT('Ctrl Pts',(-5.77704085522352,-0.0189872057270379,
20.8989759894526));
#37356=CARTESIAN_POINT('Ctrl Pts',(-3.56709774791074,-4.0412840629435,21.031262472875));
#37357=CARTESIAN_POINT('Ctrl Pts',(-0.362731338653644,-5.07374792580599,
21.1370916596129));
#37358=CARTESIAN_POINT('Ctrl Pts',(2.10287077052077,-4.64454172754387,21.2164635496663));
#37359=CARTESIAN_POINT('Ctrl Pts',(4.07100210770441,-3.06469899064061,21.2958354397197));
#37360=CARTESIAN_POINT('Ctrl Pts',(5.03948789886561,-0.748754766453301,
21.3752073297731));
#37361=CARTESIAN_POINT('Ctrl Pts',(4.78459624359497,1.75515257798294,21.4545792198265));
#37362=CARTESIAN_POINT('Ctrl Pts',(3.36194502775863,3.82855576883798,21.5339511098799));
#37363=CARTESIAN_POINT('Ctrl Pts',(1.12151932172619,4.97089558679479,21.6133229999333));
#37364=CARTESIAN_POINT('Ctrl Pts',(-1.39273514199732,4.9015077036213,21.6926948899867));
#37365=CARTESIAN_POINT('Ctrl Pts',(-3.56738921282951,3.63856219800436,21.7720667800401));
#37366=CARTESIAN_POINT('Ctrl Pts',(-4.87321162956223,1.48903860109202,21.8514386700935));
#37367=CARTESIAN_POINT('Ctrl Pts',(-4.99183702504821,-1.02308842639,21.9308105601469));
#37368=CARTESIAN_POINT('Ctrl Pts',(-3.89451146459856,-3.28605855970678,
22.0101824502003));
#37369=CARTESIAN_POINT('Ctrl Pts',(-1.84846531944319,-4.74851758083281,
22.0895543402537));
#37370=CARTESIAN_POINT('Ctrl Pts',(0.647849003889951,-5.05426651218743,
22.1689262303072));
#37371=CARTESIAN_POINT('Ctrl Pts',(2.98635609589609,-4.12879762624803,22.2482981203605));
#37372=CARTESIAN_POINT('Ctrl Pts',(4.59738955946421,-2.19756790530644,22.3276700104139));
#37373=CARTESIAN_POINT('Ctrl Pts',(5.08851116459638,0.268987208844064,22.4070419004674));
#37374=CARTESIAN_POINT('Ctrl Pts',(4.34008162116472,2.67001619606227,22.4864137905207));
#37375=CARTESIAN_POINT('Ctrl Pts',(2.53441837980377,4.4206359096037,22.5657856805742));
#37376=CARTESIAN_POINT('Ctrl Pts',(0.11137612465092,5.09439809707615,22.6451575706275));
#37377=CARTESIAN_POINT('Ctrl Pts',(-2.3387969457162,4.52717639800266,22.724529460681));
#37378=CARTESIAN_POINT('Ctrl Pts',(-4.2192443428605,2.85714443596456,22.8039013507343));
#37379=CARTESIAN_POINT('Ctrl Pts',(-5.07189311172227,0.491118473430054,
22.8832732407878));
#37380=CARTESIAN_POINT('Ctrl Pts',(-4.6890399691108,-1.99454289389497,22.9626451308412));
#37381=CARTESIAN_POINT('Ctrl Pts',(-3.1639470562758,-3.99433801030587,23.0420170208946));
#37382=CARTESIAN_POINT('Ctrl Pts',(-0.868123650568842,-5.02112123762457,
23.121388910948));
#37383=CARTESIAN_POINT('Ctrl Pts',(1.63917275843702,-4.82477044080721,23.2007608010014));
#37384=CARTESIAN_POINT('Ctrl Pts',(3.74717030983928,-3.45311624655406,23.2801326910548));
#37385=CARTESIAN_POINT('Ctrl Pts',(4.94236546898948,-1.24029057666132,23.3595045811082));
#37386=CARTESIAN_POINT('Ctrl Pts',(4.93361133910258,1.27466713166923,23.4388764711616));
#37387=CARTESIAN_POINT('Ctrl Pts',(3.72304040765536,3.47911874852391,23.518248361215));
#37388=CARTESIAN_POINT('Ctrl Pts',(1.60554507356429,4.83606473894047,23.5976202512684));
#37389=CARTESIAN_POINT('Ctrl Pts',(-0.903057486554317,5.01495606350285,
23.6769921413218));
#37390=CARTESIAN_POINT('Ctrl Pts',(-3.19167724187396,3.97221519135782,23.7563640313752));
#37391=CARTESIAN_POINT('Ctrl Pts',(-4.70281148570869,1.96185149097637,23.8357359214286));
#37392=CARTESIAN_POINT('Ctrl Pts',(-5.06835126113314,-0.526414890137771,
23.915107811482));
#37393=CARTESIAN_POINT('Ctrl Pts',(-4.1992518879446,-2.88644776920571,23.9944797015354));
#37394=CARTESIAN_POINT('Ctrl Pts',(-2.30722404974247,-4.54334836074326,
24.0738515915888));
#37395=CARTESIAN_POINT('Ctrl Pts',(0.1468384600249,-5.09349934813251,24.1532234816422));
#37396=CARTESIAN_POINT('Ctrl Pts',(2.56513144595071,-4.40288516858744,24.2325953716957));
#37397=CARTESIAN_POINT('Ctrl Pts',(4.35856408946553,-2.63973790759483,24.311967261749));
#37398=CARTESIAN_POINT('Ctrl Pts',(5.09026016830426,-0.23355633527326,24.3913391518024));
#37399=CARTESIAN_POINT('Ctrl Pts',(4.58198013724401,2.22951904335289,24.4707110418559));
#37400=CARTESIAN_POINT('Ctrl Pts',(2.95753988679205,4.1494885179749,24.5500829319092));
#37401=CARTESIAN_POINT('Ctrl Pts',(0.612649466321058,5.05865177435533,24.6294548219626));
#37402=CARTESIAN_POINT('Ctrl Pts',(-1.88148100806917,4.73553865563851,24.7088267120161));
#37403=CARTESIAN_POINT('Ctrl Pts',(-3.91728687348126,3.25885880234522,24.7881986020694));
#37404=CARTESIAN_POINT('Ctrl Pts',(-4.99885032728078,0.988328158162253,
24.8675704921229));
#37405=CARTESIAN_POINT('Ctrl Pts',(-4.86270490612224,-1.5229570377218,24.9469423821763));
#37406=CARTESIAN_POINT('Ctrl Pts',(-3.54201533324704,-3.66325327022505,
25.0263142722297));
#37407=CARTESIAN_POINT('Ctrl Pts',(-1.3584986653108,-4.91118911457504,25.1056861622831));
#37408=CARTESIAN_POINT('Ctrl Pts',(1.15594527050936,-4.96277016134726,25.1850580523365));
#37409=CARTESIAN_POINT('Ctrl Pts',(3.38880349707489,-3.80543138172069,25.2644299423899));
#37410=CARTESIAN_POINT('Ctrl Pts',(4.79615669274227,-1.72109794068643,25.3438018324433));
#37411=CARTESIAN_POINT('Ctrl Pts',(5.0351767341704,0.782491149113306,25.4231737224967));
#37412=CARTESIAN_POINT('Ctrl Pts',(4.04763886832931,3.09546712700384,25.5025456125501));
#37413=CARTESIAN_POINT('Ctrl Pts',(2.07410513345989,4.65439416445651,25.5819175026035));
#37414=CARTESIAN_POINT('Ctrl Pts',(-0.404676020966502,5.07952108577436,
25.6612893926569));
#37415=CARTESIAN_POINT('Ctrl Pts',(-2.78487899242069,4.26728791392678,25.7406612827102));
#37416=CARTESIAN_POINT('Ctrl Pts',(-4.48669160554627,2.41555285172821,25.8200331727637));
#37417=CARTESIAN_POINT('Ctrl Pts',(-5.09555607468418,-0.0246055384158182,
25.8994050628171));
#37418=CARTESIAN_POINT('Ctrl Pts',(-4.46315436285108,-2.45877007386518,
25.9787769528705));
#37419=CARTESIAN_POINT('Ctrl Pts',(-2.74353812725205,-4.29398366171623,
26.0581488429239));
#37420=CARTESIAN_POINT('Ctrl Pts',(-0.355602076573053,-5.0831923341448,
26.1375207329773));
#37421=CARTESIAN_POINT('Ctrl Pts',(2.11895785284724,-4.63414660543109,26.2168926230307));
#37422=CARTESIAN_POINT('Ctrl Pts',(4.07734433954763,-3.05623302114393,26.2962645130841));
#37423=CARTESIAN_POINT('Ctrl Pts',(5.04249877018284,-0.733827837763115,
26.3756364031375));
#37424=CARTESIAN_POINT('Ctrl Pts',(4.77931166178323,1.76733618259643,26.4550082931909));
#37425=CARTESIAN_POINT('Ctrl Pts',(3.3518948114001,3.83798102080776,26.5343801832444));
#37426=CARTESIAN_POINT('Ctrl Pts',(1.10796380425329,4.97370217757719,26.6137520732977));
#37427=CARTESIAN_POINT('Ctrl Pts',(-1.40586473317334,4.89784049299189,26.6931239633511));
#37428=CARTESIAN_POINT('Ctrl Pts',(-3.57722773342779,3.62887570549981,26.7724958534045));
#37429=CARTESIAN_POINT('Ctrl Pts',(-4.87718597587851,1.47592482852807,26.851867743458));
#37430=CARTESIAN_POINT('Ctrl Pts',(-4.98907251007324,-1.0365580697689,26.9312396335114));
#37431=CARTESIAN_POINT('Ctrl Pts',(-3.88563202393884,-3.29653771665249,
27.0106115235647));
#37432=CARTESIAN_POINT('Ctrl Pts',(-1.83566017747357,-4.75348807252204,
27.0899834136182));
#37433=CARTESIAN_POINT('Ctrl Pts',(0.661474425059423,-5.05249925559262,
27.1693553036715));
#37434=CARTESIAN_POINT('Ctrl Pts',(2.99747532179674,-4.12073280351822,27.248727193725));
#37435=CARTESIAN_POINT('Ctrl Pts',(4.60329786494346,-2.18516496159412,27.3280990837784));
#37436=CARTESIAN_POINT('Ctrl Pts',(5.08776723741692,0.282704228193704,27.4074709738318));
#37437=CARTESIAN_POINT('Ctrl Pts',(4.33286777243738,2.68170729374875,27.4868428638852));
#37438=CARTESIAN_POINT('Ctrl Pts',(2.5224913087322,4.42745239840498,27.5662147539386));
#37439=CARTESIAN_POINT('Ctrl Pts',(0.0976415456597213,5.09467989880942,
27.6455866439919));
#37440=CARTESIAN_POINT('Ctrl Pts',(-2.35099348180958,4.52085465274658,27.7249585340454));
#37441=CARTESIAN_POINT('Ctrl Pts',(-4.22693170094588,2.84575922001675,27.8043304240988));
#37442=CARTESIAN_POINT('Ctrl Pts',(-5.07319871388641,0.477443140272041,
27.8837023141522));
#37443=CARTESIAN_POINT('Ctrl Pts',(-4.68364574945911,-2.00717703164051,
27.9630742042056));
#37444=CARTESIAN_POINT('Ctrl Pts',(-3.15316704753758,-4.00285332145644,
28.042446094259));
#37445=CARTESIAN_POINT('Ctrl Pts',(-0.854583832252744,-5.02344340233109,
28.1218179843124));
#37446=CARTESIAN_POINT('Ctrl Pts',(1.65217411297962,-4.82033378960126,28.2011898743658));
#37447=CARTESIAN_POINT('Ctrl Pts',(3.75646610131553,-3.44300153535241,28.2805617644192));
#37448=CARTESIAN_POINT('Ctrl Pts',(4.94569126216762,-1.22696172804632,28.3599336544726));
#37449=CARTESIAN_POINT('Ctrl Pts',(4.93015697865761,1.28796324037807,28.439305544526));
#37450=CARTESIAN_POINT('Ctrl Pts',(3.71364736786401,3.48914321430466,28.5186774345794));
#37451=CARTESIAN_POINT('Ctrl Pts',(1.59250147827778,4.84037562431415,28.5980493246328));
#37452=CARTESIAN_POINT('Ctrl Pts',(-0.916574246474672,5.01250324623047,
28.6774212146862));
#37453=CARTESIAN_POINT('Ctrl Pts',(-3.20237451358863,3.96359617235279,28.7567931047396));
#37454=CARTESIAN_POINT('Ctrl Pts',(-4.70808343752814,1.94916584416126,28.836164994793));
#37455=CARTESIAN_POINT('Ctrl Pts',(-5.0669136572517,-0.540076969262536,
28.9155368848465));
#37456=CARTESIAN_POINT('Ctrl Pts',(-4.19145492549188,-2.89775822841407,
28.9949087748998));
#37457=CARTESIAN_POINT('Ctrl Pts',(-2.29496705151034,-4.54955199720298,
29.0742806649532));
#37458=CARTESIAN_POINT('Ctrl Pts',(0.160569716395729,-5.09308496973575,
29.1536525550067));
#37459=CARTESIAN_POINT('Ctrl Pts',(2.57699205680278,-4.39595371699326,29.23302444506));
#37460=CARTESIAN_POINT('Ctrl Pts',(4.36566483624787,-2.62797786906977,29.3123963351135));
#37461=CARTESIAN_POINT('Ctrl Pts',(5.09087132481821,-0.219832429171176,
29.3917682251668));
#37462=CARTESIAN_POINT('Ctrl Pts',(4.57595282711536,2.24186370388268,29.4711401152203));
#37463=CARTESIAN_POINT('Ctrl Pts',(2.94634234942697,4.15744680095185,29.5505120052737));
#37464=CARTESIAN_POINT('Ctrl Pts',(0.599009397036387,5.06028505966152,29.6298838953271));
#37465=CARTESIAN_POINT('Ctrl Pts',(-1.89424091858745,4.73044907858869,29.7092557853805));
#37466=CARTESIAN_POINT('Ctrl Pts',(-3.92605833927458,3.24828617264307,29.7886276754339));
#37467=CARTESIAN_POINT('Ctrl Pts',(-5.00149663869715,0.974847945001076,
29.8679995654873));
#37468=CARTESIAN_POINT('Ctrl Pts',(-4.85858142755809,-1.53606108425386,
29.9473714555407));
#37469=CARTESIAN_POINT('Ctrl Pts',(-3.53212653495348,-3.67278903339805,
30.026743345594));
#37470=CARTESIAN_POINT('Ctrl Pts',(-1.34525343666372,-4.91483370358714,
30.1061152356475));
#37471=CARTESIAN_POINT('Ctrl Pts',(1.16932042112941,-4.95963576238229,30.1854871257009));
#37472=CARTESIAN_POINT('Ctrl Pts',(3.39905041258226,-3.79628152742866,30.2648590157543));
#37473=CARTESIAN_POINT('Ctrl Pts',(4.80077924720052,-1.70816151532001,30.3442309058077));
#37474=CARTESIAN_POINT('Ctrl Pts',(5.03304888354535,0.796062860969203,30.4236027958611));
#37475=CARTESIAN_POINT('Ctrl Pts',(4.03927895232327,3.10636808638158,30.5029746859145));
#37476=CARTESIAN_POINT('Ctrl Pts',(2.06154960910751,4.65996892178051,30.5823465759679));
#37477=CARTESIAN_POINT('Ctrl Pts',(-0.418368655724119,5.07841164249995,
30.6617184660213));
#37478=CARTESIAN_POINT('Ctrl Pts',(-2.79637324206467,4.25976452797996,30.7410903560747));
#37479=CARTESIAN_POINT('Ctrl Pts',(-4.49318749630546,2.4034482032729,30.8204622461281));
#37480=CARTESIAN_POINT('Ctrl Pts',(-5.09547122194811,-0.0383427838090456,
30.8998341361815));
#37481=CARTESIAN_POINT('Ctrl Pts',(-4.45650943655845,-2.47079355362547,
30.9792060262349));
#37482=CARTESIAN_POINT('Ctrl Pts',(-2.73195181673944,-4.3013644827875,31.0585779162883));
#37483=CARTESIAN_POINT('Ctrl Pts',(-0.341896781435476,-5.08413254485124,
31.1379498063417));
#37484=CARTESIAN_POINT('Ctrl Pts',(2.13144355305047,-4.62841717252575,31.2173216963952));
#37485=CARTESIAN_POINT('Ctrl Pts',(4.08556895588362,-3.04522962180058,31.2966935864485));
#37486=CARTESIAN_POINT('Ctrl Pts',(5.04445880431697,-0.720230875706232,
31.376065476502));
#37487=CARTESIAN_POINT('Ctrl Pts',(4.77452965373889,1.78021451750611,31.4554373665553));
#37488=CARTESIAN_POINT('Ctrl Pts',(3.34153564775218,3.84700359469197,31.5348092566088));
#37489=CARTESIAN_POINT('Ctrl Pts',(1.09455095433672,4.97667111140894,31.6141811466621));
#37490=CARTESIAN_POINT('Ctrl Pts',(-1.41906392880775,4.89403256106132,31.6935530367156));
#37491=CARTESIAN_POINT('Ctrl Pts',(-3.58699797993935,3.61921851159646,31.772924926769));
#37492=CARTESIAN_POINT('Ctrl Pts',(-4.88114726284307,1.46277084371106,31.8522968168224));
#37493=CARTESIAN_POINT('Ctrl Pts',(-4.98625987675445,-1.05000456391402,
31.9316687068758));
#37494=CARTESIAN_POINT('Ctrl Pts',(-3.87673062158748,-3.30700118391536,
32.0110405969292));
#37495=CARTESIAN_POINT('Ctrl Pts',(-1.82283836799946,-4.75841963543788,
32.0904124869826));
#37496=CARTESIAN_POINT('Ctrl Pts',(0.675093277248947,-5.0506975963509,32.169784377036));
#37497=CARTESIAN_POINT('Ctrl Pts',(3.00857369445308,-4.11263680232238,32.2491562670894));
#37498=CARTESIAN_POINT('Ctrl Pts',(4.60917221905339,-2.17274678641531,32.3285281571428));
#37499=CARTESIAN_POINT('Ctrl Pts',(5.08698659332197,0.296419537369132,32.4079000471962));
#37500=CARTESIAN_POINT('Ctrl Pts',(4.32562229331115,2.69337871796399,32.4872719372496));
#37501=CARTESIAN_POINT('Ctrl Pts',(2.51054597725224,4.43423680455544,32.566643827303));
#37502=CARTESIAN_POINT('Ctrl Pts',(0.0839062181339619,5.09492462057391,
32.6460157173564));
#37503=CARTESIAN_POINT('Ctrl Pts',(-2.3631729099985,4.51450007644488,32.7253876074099));
#37504=CARTESIAN_POINT('Ctrl Pts',(-4.23458834804982,2.8343533063703,32.8047594974632));
#37505=CARTESIAN_POINT('Ctrl Pts',(-5.07446743761851,0.463764344598583,
32.8841313875167));
#37506=CARTESIAN_POINT('Ctrl Pts',(-4.67821749152652,-2.01979658499237,
32.96350327757));
#37507=CARTESIAN_POINT('Ctrl Pts',(-3.14236411955747,-4.01133953722311,
33.0428751676235));
#37508=CARTESIAN_POINT('Ctrl Pts',(-0.841037803569241,-5.02572905713579,
33.1222470576768));
#37509=CARTESIAN_POINT('Ctrl Pts',(1.6651634597629,-4.81586210299279,33.2016189477303));
#37510=CARTESIAN_POINT('Ctrl Pts',(3.76573459007359,-3.43286180029067,33.2809908377836));
#37511=CARTESIAN_POINT('Ctrl Pts',(4.94898110955447,-1.21362396154845,33.3603627278371));
#37512=CARTESIAN_POINT('Ctrl Pts',(4.92666678513176,1.3012499879159,33.4397346178904));
#37513=CARTESIAN_POINT('Ctrl Pts',(3.70422733684289,3.49914232059194,33.5191065079439));
#37514=CARTESIAN_POINT('Ctrl Pts',(1.5794463084672,4.8446513291919,33.5984783979973));
#37515=CARTESIAN_POINT('Ctrl Pts',(-0.930084344605925,5.01001399745455,
33.6778502880506));
#37516=CARTESIAN_POINT('Ctrl Pts',(-3.21304851003985,3.95494834541518,33.7572221781041));
#37517=CARTESIAN_POINT('Ctrl Pts',(-4.71332117039034,1.93646603056234,33.8365940681574));
#37518=CARTESIAN_POINT('Ctrl Pts',(-5.06543922639319,-0.553735123040657,
33.9159659582109));
#37519=CARTESIAN_POINT('Ctrl Pts',(-4.18362749900617,-2.90904762634284,
33.9953378482642));
#37520=CARTESIAN_POINT('Ctrl Pts',(-2.28269337316369,-4.55572256693558,
34.0747097383177));
#37521=CARTESIAN_POINT('Ctrl Pts',(0.174299805725373,-5.0926335741437,34.154081628371));
#37522=CARTESIAN_POINT('Ctrl Pts',(2.58883393774586,-4.38899031504365,34.2334535184245));
#37523=CARTESIAN_POINT('Ctrl Pts',(4.37273385281817,-2.61619873006421,34.3128254084779));
#37524=CARTESIAN_POINT('Ctrl Pts',(5.09144548022617,-0.206106925298799,
34.3921972985313));
#37525=CARTESIAN_POINT('Ctrl Pts',(4.56989225837449,2.25419207025942,34.4715691885847));
#37526=CARTESIAN_POINT('Ctrl Pts',(2.93512339766776,4.16537486707196,34.5509410786381));
#37527=CARTESIAN_POINT('Ctrl Pts',(0.585364974074578,5.06188156616671,34.6303129686915));
#37528=CARTESIAN_POINT('Ctrl Pts',(-1.9069870615198,4.72532512002801,34.7096848587449));
#37529=CARTESIAN_POINT('Ctrl Pts',(-3.93480126997218,3.23768993398022,34.7890567487983));
#37530=CARTESIAN_POINT('Ctrl Pts',(-5.00410659859424,0.961360646519953,
34.8684286388517));
#37531=CARTESIAN_POINT('Ctrl Pts',(-4.85442263620079,-1.54915396649689,
34.9478005289051));
#37532=CARTESIAN_POINT('Ctrl Pts',(-3.52221206471105,-3.68229810226921,
35.0271724189585));
#37533=CARTESIAN_POINT('Ctrl Pts',(-1.33199843054191,-4.91844257095733,
35.1065443090119));
#37534=CARTESIAN_POINT('Ctrl Pts',(1.1826870729787,-4.95646531614826,35.1859161990653));
#37535=CARTESIAN_POINT('Ctrl Pts',(3.40927262335516,-3.78710408127537,35.2652880891187));
#37536=CARTESIAN_POINT('Ctrl Pts',(4.80536690897926,-1.69521267481654,35.3446599791721));
#37537=CARTESIAN_POINT('Ctrl Pts',(5.03088445207529,0.809628786938043,35.4240318692255));
#37538=CARTESIAN_POINT('Ctrl Pts',(4.0308896783196,3.11724646827744,35.503403759279));
#37539=CARTESIAN_POINT('Ctrl Pts',(2.04897910114821,4.66550980985245,35.5827756493324));
#37540=CARTESIAN_POINT('Ctrl Pts',(-0.432058249724576,5.0772652886782,35.6621475393857));
#37541=CARTESIAN_POINT('Ctrl Pts',(-2.80784716730917,4.25221018151802,35.7415194294392));
#37542=CARTESIAN_POINT('Ctrl Pts',(-4.49965073000152,2.39132608624762,35.8208913194925));
#37543=CARTESIAN_POINT('Ctrl Pts',(-5.09534933467344,-0.052079750522149,
35.9002632095459));
#37544=CARTESIAN_POINT('Ctrl Pts',(-4.4498321197834,-2.48279907534128,35.9796350995994));
#37545=CARTESIAN_POINT('Ctrl Pts',(-2.72034565005043,-4.30871404098988,
36.0590069896527));
#37546=CARTESIAN_POINT('Ctrl Pts',(-0.328189001348134,-5.08503580343008,
36.1383788797062));
#37547=CARTESIAN_POINT('Ctrl Pts',(2.14391376164854,-4.62265409969052,36.2177507697596));
#37548=CARTESIAN_POINT('Ctrl Pts',(4.0937638777802,-3.03420408933768,36.2971226598129));
#37549=CARTESIAN_POINT('Ctrl Pts',(5.0463821746773,-0.706628678919033,36.3764945498664));
#37550=CARTESIAN_POINT('Ctrl Pts',(4.76971294380048,1.79307991358828,36.4558664399198));
#37551=CARTESIAN_POINT('Ctrl Pts',(3.33115219739438,3.85599820806056,36.5352383299732));
#37552=CARTESIAN_POINT('Ctrl Pts',(1.08113014908331,4.97960387415652,36.6146102200266));
#37553=CARTESIAN_POINT('Ctrl Pts',(-1.4322528105034,4.89018905867418,36.69398211008));
#37554=CARTESIAN_POINT('Ctrl Pts',(-3.59674215568932,3.60953501274872,36.7733540001334));
#37555=CARTESIAN_POINT('Ctrl Pts',(-4.88507307300309,1.44960622728788,36.8527258901868));
#37556=CARTESIAN_POINT('Ctrl Pts',(-4.98341100265913,-1.06344342649134,
36.9320977802402));
#37557=CARTESIAN_POINT('Ctrl Pts',(-3.86780104266052,-3.31744061546937,
37.0114696702936));
#37558=CARTESIAN_POINT('Ctrl Pts',(-1.81000330990226,-4.76331661354924,
37.090841560347));
#37559=CARTESIAN_POINT('Ctrl Pts',(0.688707222773825,-5.04885922799112,
37.1702134504005));
#37560=CARTESIAN_POINT('Ctrl Pts',(3.0196502004098,-4.10451090995456,37.2495853404537));
#37561=CARTESIAN_POINT('Ctrl Pts',(4.61501307310836,-2.16031281943414,37.3289572305073));
#37562=CARTESIAN_POINT('Ctrl Pts',(5.08616897635574,0.310132692129688,37.4083291205606));
#37563=CARTESIAN_POINT('Ctrl Pts',(4.31834537500717,2.70503056635669,37.4877010106141));
#37564=CARTESIAN_POINT('Ctrl Pts',(2.49858239880182,4.44098898210481,37.5670729006674));
#37565=CARTESIAN_POINT('Ctrl Pts',(0.0701702807674692,5.09513231177087,
37.6464447907209));
#37566=CARTESIAN_POINT('Ctrl Pts',(-2.37533516234416,4.50811268818063,37.7258166807742));
#37567=CARTESIAN_POINT('Ctrl Pts',(-4.2422142176209,2.82292679227449,37.8051885708277));
#37568=CARTESIAN_POINT('Ctrl Pts',(-5.07569927947281,0.450082178237795,
37.884560460881));
#37569=CARTESIAN_POINT('Ctrl Pts',(-4.67275523170413,-2.03240145822491,
37.9639323509345));
#37570=CARTESIAN_POINT('Ctrl Pts',(-3.13153835248091,-4.01979659801907,
38.0433042409878));
#37571=CARTESIAN_POINT('Ctrl Pts',(-0.827485662097561,-5.02797818437316,
38.1226761310413));
#37572=CARTESIAN_POINT('Ctrl Pts',(1.6781407038918,-4.81135541393667,38.2020480210947));
#37573=CARTESIAN_POINT('Ctrl Pts',(3.77497570905148,-3.42269711502072,38.281419911148));
#37574=CARTESIAN_POINT('Ctrl Pts',(4.95223498699472,-1.20027737376265,38.3607918012015));
#37575=CARTESIAN_POINT('Ctrl Pts',(4.92314078418044,1.31452727683269,38.4401636912548));
#37576=CARTESIAN_POINT('Ctrl Pts',(3.69478038260533,3.50911599649374,38.5195355813083));
#37577=CARTESIAN_POINT('Ctrl Pts',(1.56637965982565,4.8488918190669,38.5989074713616));
#37578=CARTESIAN_POINT('Ctrl Pts',(-0.943587684251231,5.00748834177839,
38.6782793614151));
#37579=CARTESIAN_POINT('Ctrl Pts',(-3.22369915083517,3.94627176108658,38.7576512514684));
#37580=CARTESIAN_POINT('Ctrl Pts',(-4.71852465152966,1.92375216574096,38.8370231415219));
#37581=CARTESIAN_POINT('Ctrl Pts',(-5.06392796926474,-0.567389296122155,
38.9163950315753));
#37582=CARTESIAN_POINT('Ctrl Pts',(-4.17576968427578,-2.92031579800749,
38.9957669216287));
#37583=CARTESIAN_POINT('Ctrl Pts',(-2.27040306822808,-4.56186018168572,
39.0751388116821));
#37584=CARTESIAN_POINT('Ctrl Pts',(0.188028560849278,-5.0921448689568,39.1545107017355));
#37585=CARTESIAN_POINT('Ctrl Pts',(2.60065712992459,-4.38199557165452,39.2338825917889));
#37586=CARTESIAN_POINT('Ctrl Pts',(4.37977084759398,-2.60439952199669,39.3132544818424));
#37587=CARTESIAN_POINT('Ctrl Pts',(5.091983083909,-0.192381913948899,39.3926263718957));
#37588=CARTESIAN_POINT('Ctrl Pts',(4.56379761866661,2.26650781142318,39.4719982619492));
#37589=CARTESIAN_POINT('Ctrl Pts',(2.92388473013463,4.17326556172555,39.5513701520025));
#37590=CARTESIAN_POINT('Ctrl Pts',(0.571713243107522,5.06345468357226,39.6307420420559));
#37591=CARTESIAN_POINT('Ctrl Pts',(-1.91971357759784,4.72014150668349,39.7101139321093));
#37592=CARTESIAN_POINT('Ctrl Pts',(-3.94352649879586,3.22711800485078,39.7894858221628));
#37593=CARTESIAN_POINT('Ctrl Pts',(-5.00665954563271,0.947775616877117,
39.8688577122161));
#37594=CARTESIAN_POINT('Ctrl Pts',(-4.85026808817391,-1.56206090154421,
39.9482296022695));
#37595=CARTESIAN_POINT('Ctrl Pts',(-3.51219281059473,-3.69213734276829,
40.027601492323));
#37596=CARTESIAN_POINT('Ctrl Pts',(-2.05001543279097,-4.51147638686035,
40.0805160856919));
#37597=CARTESIAN_POINT('Ctrl Pts',(-1.2650852794273,-4.72177922709094,40.1069733823764));
#37598=CARTESIAN_POINT('Ctrl Pts',(-3.8562705385024,3.29705846079174,-0.320920147129055));
#37599=CARTESIAN_POINT('Ctrl Pts',(-4.40436067122819,2.6560070944272,-0.294462850444587));
#37600=CARTESIAN_POINT('Ctrl Pts',(-5.17416686787623,1.09598291074317,-0.241548257075651));
#37601=CARTESIAN_POINT('Ctrl Pts',(-5.06779668194698,-1.512680812799,-0.162176367022247));
#37602=CARTESIAN_POINT('Ctrl Pts',(-3.72722085031348,-3.75211381890485,
-0.0828044769688437));
#37603=CARTESIAN_POINT('Ctrl Pts',(-1.47855208449991,-5.07791790908896,
-0.00343258691543986));
#37604=CARTESIAN_POINT('Ctrl Pts',(1.1302101318597,-5.16655447652177,0.0759393031379633));
#37605=CARTESIAN_POINT('Ctrl Pts',(3.46369715057722,-3.99673439595713,0.155311193191368));
#37606=CARTESIAN_POINT('Ctrl Pts',(4.95341325213432,-1.85326330477546,0.23468308324477));
#37607=CARTESIAN_POINT('Ctrl Pts',(5.23650047694814,0.741629311098527,0.314054973298175));
#37608=CARTESIAN_POINT('Ctrl Pts',(4.24398161873799,3.15587819282154,0.393426863351577));
#37609=CARTESIAN_POINT('Ctrl Pts',(2.21764149317933,4.80135391043019,0.472798753404982));
#37610=CARTESIAN_POINT('Ctrl Pts',(-0.348912918530393,5.27723479734493,
0.552170643458385));
#37611=CARTESIAN_POINT('Ctrl Pts',(-2.83047200092439,4.46759066254957,0.631542533511789));
#37612=CARTESIAN_POINT('Ctrl Pts',(-4.62253485344812,2.56965255248809,0.710914423565193));
#37613=CARTESIAN_POINT('Ctrl Pts',(-5.28855819093304,0.045752121671659,
0.790286313618596));
#37614=CARTESIAN_POINT('Ctrl Pts',(-4.66630059499956,-2.48929308216644,
0.869658203672));
#37615=CARTESIAN_POINT('Ctrl Pts',(-2.90734243084918,-4.4179521825598,0.949030093725403));
#37616=CARTESIAN_POINT('Ctrl Pts',(-0.440162123945536,-5.27040781417518,
1.02840198377881));
#37617=CARTESIAN_POINT('Ctrl Pts',(2.1342407222512,-4.83900381899044,1.10777387383221));
#37618=CARTESIAN_POINT('Ctrl Pts',(4.18874724188064,-3.228829177505,1.18714576388562));
#37619=CARTESIAN_POINT('Ctrl Pts',(5.22288421068343,-0.832118909543204,
1.26651765393902));
#37620=CARTESIAN_POINT('Ctrl Pts',(4.98473814342391,1.76729369047769,1.34588954399242));
#37621=CARTESIAN_POINT('Ctrl Pts',(3.53232089954478,3.93619745533352,1.42526143404583));
#37622=CARTESIAN_POINT('Ctrl Pts',(1.21943810235538,5.14625223481536,1.50463332409923));
#37623=CARTESIAN_POINT('Ctrl Pts',(-1.39049711694202,5.10269135980955,1.58400521415263));
#37624=CARTESIAN_POINT('Ctrl Pts',(-3.66171031660135,3.81612616476449,1.66337710420604));
#37625=CARTESIAN_POINT('Ctrl Pts',(-5.04093898807,1.59996108251987,1.74274899425944));
#37626=CARTESIAN_POINT('Ctrl Pts',(-5.19220608004013,-1.00595097780601,
1.82212088431284));
#37627=CARTESIAN_POINT('Ctrl Pts',(-4.07866326363067,-3.3668156066614,1.90149277436625));
#37628=CARTESIAN_POINT('Ctrl Pts',(-1.97156710418735,-4.90753140600723,
1.98086466441965));
#37629=CARTESIAN_POINT('Ctrl Pts',(0.61579843785608,-5.25278341751101,2.06023655447306));
#37630=CARTESIAN_POINT('Ctrl Pts',(3.0531568434793,-4.31846901533485,2.13960844452646));
#37631=CARTESIAN_POINT('Ctrl Pts',(4.74677300008174,-2.3321851197991,2.21898033457986));
#37632=CARTESIAN_POINT('Ctrl Pts',(5.28408576066664,0.222213908719184,2.29835222463327));
#37633=CARTESIAN_POINT('Ctrl Pts',(4.53420692607935,2.72248212093367,2.37772411468667));
#37634=CARTESIAN_POINT('Ctrl Pts',(2.67980532059554,4.5595597146017,2.45709600474007));
#37635=CARTESIAN_POINT('Ctrl Pts',(0.172609070663326,5.28593865420646,2.53646789479348));
#37636=CARTESIAN_POINT('Ctrl Pts',(-2.37663436681889,4.72467463787357,2.61583978484688));
#37637=CARTESIAN_POINT('Ctrl Pts',(-4.34693493313492,3.01249033764445,2.69521167490029));
#37638=CARTESIAN_POINT('Ctrl Pts',(-5.25833177151656,0.56647005919948,2.77458356495369));
#37639=CARTESIAN_POINT('Ctrl Pts',(-4.88881062947673,-2.01754107180632,
2.85395545500709));
#37640=CARTESIAN_POINT('Ctrl Pts',(-3.32838603929513,-4.11008366347149,
2.93332734506049));
#37641=CARTESIAN_POINT('Ctrl Pts',(-0.957173977198773,-5.20141897223089,
3.0126992351139));
#37642=CARTESIAN_POINT('Ctrl Pts',(1.64720354707453,-5.02570013250045,3.0920711251673));
#37643=CARTESIAN_POINT('Ctrl Pts',(3.85032593330369,-3.62573186469146,3.1714430152207));
#37644=CARTESIAN_POINT('Ctrl Pts',(5.11551744473197,-1.342543340065,3.25081490527411));
#37645=CARTESIAN_POINT('Ctrl Pts',(5.13458022962935,1.26768577053204,3.33018679532751));
#37646=CARTESIAN_POINT('Ctrl Pts',(3.90287063578958,3.56910943340232,3.40955868538091));
#37647=CARTESIAN_POINT('Ctrl Pts',(1.7204303939291,5.00110593838552,3.48893057543432));
#37648=CARTESIAN_POINT('Ctrl Pts',(-0.881102883784432,5.21484410653825,
3.56830246548772));
#37649=CARTESIAN_POINT('Ctrl Pts',(-3.26800144929621,4.15825779319991,3.64767435554113));
#37650=CARTESIAN_POINT('Ctrl Pts',(-4.85882209535798,2.08872908558557,3.72704624559453));
#37651=CARTESIAN_POINT('Ctrl Pts',(-5.2660444338108,-0.489609403954008,
3.80641813564793));
#37652=CARTESIAN_POINT('Ctrl Pts',(-4.39047000437897,-2.94868012642242,
3.88579002570134));
#37653=CARTESIAN_POINT('Ctrl Pts',(-2.44538680002092,-4.68945889688708,
3.96516191575474));
#37654=CARTESIAN_POINT('Ctrl Pts',(0.0953872160503347,-5.28789586001125,
4.04453380580815));
#37655=CARTESIAN_POINT('Ctrl Pts',(2.61292511742776,-4.59821309619564,4.12390569586154));
#37656=CARTESIAN_POINT('Ctrl Pts',(4.49396024381142,-2.78841580011883,4.20327758591496));
#37657=CARTESIAN_POINT('Ctrl Pts',(5.28027660201492,-0.299366587186749,
4.28264947596836));
#37658=CARTESIAN_POINT('Ctrl Pts',(4.78032926766157,2.26260766374733,4.36202136602176));
#37659=CARTESIAN_POINT('Ctrl Pts',(3.11590430478523,4.27341569598967,4.44139325607517));
#37660=CARTESIAN_POINT('Ctrl Pts',(0.692451950200399,5.24322912373411,4.52076514612856));
#37661=CARTESIAN_POINT('Ctrl Pts',(-1.89968016673685,4.93580354262775,4.60013703618198));
#37662=CARTESIAN_POINT('Ctrl Pts',(-4.02905439992773,3.42602714375309,4.67950892623537));
#37663=CARTESIAN_POINT('Ctrl Pts',(-5.17695989945686,1.08167811604265,4.75888081628878));
#37664=CARTESIAN_POINT('Ctrl Pts',(-5.06376942648468,-1.5261653064819,4.83825270634218));
#37665=CARTESIAN_POINT('Ctrl Pts',(-3.71705592968434,-3.76223823845706,
4.91762459639559));
#37666=CARTESIAN_POINT('Ctrl Pts',(-1.46487583597662,-5.08183826311717,
4.996996486449));
#37667=CARTESIAN_POINT('Ctrl Pts',(1.14414476892732,-5.16351373534013,5.07636837650239));
#37668=CARTESIAN_POINT('Ctrl Pts',(3.47445424064207,-3.98736869087803,5.15574026655581));
#37669=CARTESIAN_POINT('Ctrl Pts',(4.95839434991041,-1.83990945920892,5.2351121566092));
#37670=CARTESIAN_POINT('Ctrl Pts',(5.23448057076031,0.75574764415296,5.31448404666261));
#37671=CARTESIAN_POINT('Ctrl Pts',(4.23545891089922,3.1673062942182,5.39385593671601));
#37672=CARTESIAN_POINT('Ctrl Pts',(2.20468883537238,4.80731614172549,5.47322782676942));
#37673=CARTESIAN_POINT('Ctrl Pts',(-0.363138560455233,5.27627441792221,
5.55259971682281));
#37674=CARTESIAN_POINT('Ctrl Pts',(-2.84250620674952,4.45994392474844,5.63197160687622));
#37675=CARTESIAN_POINT('Ctrl Pts',(-4.62944563286038,2.55718096342436,5.71134349692963));
#37676=CARTESIAN_POINT('Ctrl Pts',(-5.28866234991055,0.0314943796341776,
5.79071538698302));
#37677=CARTESIAN_POINT('Ctrl Pts',(-4.65957262477808,-2.50186416532327,
5.87008727703643));
#37678=CARTESIAN_POINT('Ctrl Pts',(-2.89542132203872,-4.42577413739037,
5.94945916708984));
#37679=CARTESIAN_POINT('Ctrl Pts',(-0.425951794157121,-5.27157532587407,
6.02883105714324));
#37680=CARTESIAN_POINT('Ctrl Pts',(2.14727864795285,-4.8332324334089,6.10820294719664));
#37681=CARTESIAN_POINT('Ctrl Pts',(4.19743676434218,-3.21752481834385,6.18757483725004));
#37682=CARTESIAN_POINT('Ctrl Pts',(5.22510857580644,-0.81803527940062,6.26694672730345));
#37683=CARTESIAN_POINT('Ctrl Pts',(4.97995550378589,1.78072584291422,6.34631861735685));
#37684=CARTESIAN_POINT('Ctrl Pts',(3.52169629398765,3.94570609146495,6.42569050741027));
#37685=CARTESIAN_POINT('Ctrl Pts',(1.20555966211655,5.14952106980711,6.50506239746365));
#37686=CARTESIAN_POINT('Ctrl Pts',(-1.40424863498509,5.09892411381582,6.58443428751707));
#37687=CARTESIAN_POINT('Ctrl Pts',(-3.67198507285601,3.80624052997609,6.66380617757046));
#37688=CARTESIAN_POINT('Ctrl Pts',(-5.04523407478029,1.58636517800468,6.74317806762388));
#37689=CARTESIAN_POINT('Ctrl Pts',(-5.1894752235243,-1.01994521996889,6.82254995767727));
#37690=CARTESIAN_POINT('Ctrl Pts',(-4.06957169452636,-3.37779921996849,
6.90192184773068));
#37691=CARTESIAN_POINT('Ctrl Pts',(-1.95832950858598,-4.91282880661553,
6.98129373778407));
#37692=CARTESIAN_POINT('Ctrl Pts',(0.629957410957137,-5.25110417033315,
7.06066562783749));
#37693=CARTESIAN_POINT('Ctrl Pts',(3.06478809957816,-4.31022218127953,7.14003751789089));
#37694=CARTESIAN_POINT('Ctrl Pts',(4.75304319093534,-2.31937960938119,7.21940940794429));
#37695=CARTESIAN_POINT('Ctrl Pts',(5.28346748166331,0.236458701502723,7.2987812979977));
#37696=CARTESIAN_POINT('Ctrl Pts',(4.52685078861501,2.73469619609302,7.37815318805109));
#37697=CARTESIAN_POINT('Ctrl Pts',(2.66750326347436,4.56676775046241,7.45752507810451));
#37698=CARTESIAN_POINT('Ctrl Pts',(0.158357847769689,5.28638478918814,7.5368969681579));
#37699=CARTESIAN_POINT('Ctrl Pts',(-2.38936318913255,4.71825019448189,7.61626885821132));
#37700=CARTESIAN_POINT('Ctrl Pts',(-4.3550406419278,3.0007602960695,7.69564074826471));
#37701=CARTESIAN_POINT('Ctrl Pts',(-5.25983983406839,0.552291831604834,
7.77501263831812));
#37702=CARTESIAN_POINT('Ctrl Pts',(-4.88335368508791,-2.03071370056153,
7.85438452837152));
#37703=CARTESIAN_POINT('Ctrl Pts',(-3.31729338754006,-4.11904187017964,
7.93375641842492));
#37704=CARTESIAN_POINT('Ctrl Pts',(-0.943147763491834,-5.20398055756651,
8.01312830847834));
#37705=CARTESIAN_POINT('Ctrl Pts',(1.66074656812082,-5.02124109994579,8.09250019853171));
#37706=CARTESIAN_POINT('Ctrl Pts',(3.86008671173945,-3.61533842470695,8.17187208858515));
#37707=CARTESIAN_POINT('Ctrl Pts',(5.11911827653537,-1.32874731162534,8.25124397863853));
#37708=CARTESIAN_POINT('Ctrl Pts',(5.13114396014337,1.28152370543593,8.33061586869195));
#37709=CARTESIAN_POINT('Ctrl Pts',(3.89323433265495,3.57961838445758,8.40998775874535));
#37710=CARTESIAN_POINT('Ctrl Pts',(1.70694143925982,5.00572594837628,8.48935964879875));
#37711=CARTESIAN_POINT('Ctrl Pts',(-0.895158610488236,5.21244975125697,
8.56873153885215));
#37712=CARTESIAN_POINT('Ctrl Pts',(-3.27920000412133,4.14943233229326,8.64810342890557));
#37713=CARTESIAN_POINT('Ctrl Pts',(-4.86443553513654,2.0756223817956,8.72747531895896));
#37714=CARTESIAN_POINT('Ctrl Pts',(-5.26470533703792,-0.503804586595236,
8.80684720901237));
#37715=CARTESIAN_POINT('Ctrl Pts',(-4.38250457206448,-2.96050587284403,
8.88621909906576));
#37716=CARTESIAN_POINT('Ctrl Pts',(-2.43273539384546,-4.69603448143659,
8.96559098911917));
#37717=CARTESIAN_POINT('Ctrl Pts',(0.109642741545844,-5.28761948484726,
9.04496287917257));
#37718=CARTESIAN_POINT('Ctrl Pts',(2.62531214778668,-4.59115208569632,9.12433476922599));
#37719=CARTESIAN_POINT('Ctrl Pts',(4.50146132585655,-2.77629020081255,9.20370665927937));
#37720=CARTESIAN_POINT('Ctrl Pts',(5.28106448876342,-0.285130168224959,
9.28307854933281));
#37721=CARTESIAN_POINT('Ctrl Pts',(4.77421203164548,2.27548694221733,9.36245043938617));
#37722=CARTESIAN_POINT('Ctrl Pts',(3.10437209115777,4.28180047024037,9.44182232943961));
#37723=CARTESIAN_POINT('Ctrl Pts',(0.67831398067512,5.24507688131743,9.52119421949299));
#37724=CARTESIAN_POINT('Ctrl Pts',(-1.91297991407746,4.93066417388633,9.6005661095464));
#37725=CARTESIAN_POINT('Ctrl Pts',(-4.03827613607002,3.41515258753654,9.6799379995998));
#37726=CARTESIAN_POINT('Ctrl Pts',(-5.1798572298885,1.06771739017486,9.75930988965322));
#37727=CARTESIAN_POINT('Ctrl Pts',(-5.05963656792565,-1.53981140008104,
9.8386817797066));
#37728=CARTESIAN_POINT('Ctrl Pts',(-3.70689963733171,-3.77224554159189,
9.91805366976003));
#37729=CARTESIAN_POINT('Ctrl Pts',(-1.45117016016697,-5.08576901889487,
9.99742555981341));
#37730=CARTESIAN_POINT('Ctrl Pts',(1.1580611559038,-5.16041042035386,10.0767974498668));
#37731=CARTESIAN_POINT('Ctrl Pts',(3.48519133772131,-3.97798726578937,10.1561693399202));
#37732=CARTESIAN_POINT('Ctrl Pts',(4.96333662401008,-1.82653521840402,10.2355412299736));
#37733=CARTESIAN_POINT('Ctrl Pts',(5.23242409484924,0.769856765217389,10.314913120027));
#37734=CARTESIAN_POINT('Ctrl Pts',(4.22690463795744,3.1787133448809,10.3942850100804));
#37735=CARTESIAN_POINT('Ctrl Pts',(2.1917205673539,4.81324238969408,10.4736569001339));
#37736=CARTESIAN_POINT('Ctrl Pts',(-0.377361782165876,5.27527624230907,
10.5530287901872));
#37737=CARTESIAN_POINT('Ctrl Pts',(-2.85451963682615,4.45226447892349,10.6324006802407));
#37738=CARTESIAN_POINT('Ctrl Pts',(-4.63632282632763,2.54469094339242,10.711772570294));
#37739=CARTESIAN_POINT('Ctrl Pts',(-5.28872803766221,0.0172363266288179,
10.7911444603475));
#37740=CARTESIAN_POINT('Ctrl Pts',(-4.65281080542322,-2.5144170211496,10.8705163504009));
#37741=CARTESIAN_POINT('Ctrl Pts',(-2.88347915980519,-4.43356394814365,
10.9498882404543));
#37742=CARTESIAN_POINT('Ctrl Pts',(-0.411738373331464,-5.27270451089727,
11.0292601305077));
#37743=CARTESIAN_POINT('Ctrl Pts',(2.16030096951836,-4.82742592572977,11.1086320205611));
#37744=CARTESIAN_POINT('Ctrl Pts',(4.20609577793862,-3.20619707038057,11.1880039106145));
#37745=CARTESIAN_POINT('Ctrl Pts',(5.22729496488813,-0.803945705483474,
11.2673758006679));
#37746=CARTESIAN_POINT('Ctrl Pts',(4.975136668812,1.79414505376576,11.3467476907213));
#37747=CARTESIAN_POINT('Ctrl Pts',(3.51104609249152,3.95518604919035,11.4261195807747));
#37748=CARTESIAN_POINT('Ctrl Pts',(1.19167245960881,5.152752477688,11.5054914708281));
#37749=CARTESIAN_POINT('Ctrl Pts',(-1.41798994671238,5.09511980804502,11.5848633608815));
#37750=CARTESIAN_POINT('Ctrl Pts',(-3.68223314068194,3.79632723101863,11.6642352509349));
#37751=CARTESIAN_POINT('Ctrl Pts',(-5.04949249206616,1.57275774354392,11.7436071409883));
#37752=CARTESIAN_POINT('Ctrl Pts',(-5.18670664924514,-1.03393204901786,
11.8229790310417));
#37753=CARTESIAN_POINT('Ctrl Pts',(-4.06045054724843,-3.38875828300867,
11.9023509210951));
#37754=CARTESIAN_POINT('Ctrl Pts',(-1.94507767959685,-4.91809050014781,
11.9817228111485));
#37755=CARTESIAN_POINT('Ctrl Pts',(0.644111805448097,-5.24938675745961,
12.0610947012019));
#37756=CARTESIAN_POINT('Ctrl Pts',(3.0763970804032,-4.30194401997477,12.1404665912553));
#37757=CARTESIAN_POINT('Ctrl Pts',(4.7592788360615,-2.30655724141565,12.2198384813087));
#37758=CARTESIAN_POINT('Ctrl Pts',(5.28281080174027,0.250701775674464,12.2992103713621));
#37759=CARTESIAN_POINT('Ctrl Pts',(4.51946174941847,2.74689039512926,12.3785822614155));
#37760=CARTESIAN_POINT('Ctrl Pts',(2.6551818185972,4.57394259446934,12.4579541514689));
#37761=CARTESIAN_POINT('Ctrl Pts',(0.144105473910954,5.28679250204684,12.5373260415223));
#37762=CARTESIAN_POINT('Ctrl Pts',(-2.40207464524796,4.7117914582425,12.6166979315757));
#37763=CARTESIAN_POINT('Ctrl Pts',(-4.36311469772651,2.98900844458373,12.6960698216291));
#37764=CARTESIAN_POINT('Ctrl Pts',(-5.26130966742946,0.538109589882336,
12.7754417116825));
#37765=CARTESIAN_POINT('Ctrl Pts',(-4.87786124785798,-2.043871569829,12.854813601736));
#37766=CARTESIAN_POINT('Ctrl Pts',(-3.30617662527107,-4.12797013916298,
12.9341854917893));
#37767=CARTESIAN_POINT('Ctrl Pts',(-0.929114694865931,-5.20650431970379,
13.0135573818428));
#37768=CARTESIAN_POINT('Ctrl Pts',(1.67427751864803,-5.01674557236658,13.0929292718962));
#37769=CARTESIAN_POINT('Ctrl Pts',(3.86981943456978,-3.60491870797887,13.1723011619496));
#37770=CARTESIAN_POINT('Ctrl Pts',(5.12268190193035,-1.31494162567972,13.251673052003));
#37771=CARTESIAN_POINT('Ctrl Pts',(5.12767039684476,1.29535232606109,13.3310449420564));
#37772=CARTESIAN_POINT('Ctrl Pts',(3.8835697329937,3.59010131838716,13.4104168321098));
#37773=CARTESIAN_POINT('Ctrl Pts',(1.69344007832116,5.01030957610862,13.4897887221632));
#37774=CARTESIAN_POINT('Ctrl Pts',(-0.909207831064397,5.21001751122212,
13.5691606122166));
#37775=CARTESIAN_POINT('Ctrl Pts',(-3.29037472530003,4.14057671278008,13.64853250227));
#37776=CARTESIAN_POINT('Ctrl Pts',(-4.87001361957351,2.06250059211591,13.7279043923234));
#37777=CARTESIAN_POINT('Ctrl Pts',(-5.26332797571119,-0.517996107520081,
13.8072762823768));
#37778=CARTESIAN_POINT('Ctrl Pts',(-4.37450728714447,-2.97231010192914,
13.8866481724302));
#37779=CARTESIAN_POINT('Ctrl Pts',(-2.420066306237,-4.70257593460501,13.9660200624836));
#37780=CARTESIAN_POINT('Ctrl Pts',(0.123897470143854,-5.28730467858643,
14.045391952537));
#37781=CARTESIAN_POINT('Ctrl Pts',(2.63768009704007,-4.58405770611459,14.1247638425904));
#37782=CARTESIAN_POINT('Ctrl Pts',(4.50892969070322,-2.76414442307289,14.2041357326438));
#37783=CARTESIAN_POINT('Ctrl Pts',(5.28181399205766,-0.270891676900501,
14.2835076226972));
#37784=CARTESIAN_POINT('Ctrl Pts',(4.7680600960438,2.28834968215629,14.3628795127506));
#37785=CARTESIAN_POINT('Ctrl Pts',(3.09281731455568,4.29015412381589,14.442251402804));
#37786=CARTESIAN_POINT('Ctrl Pts',(0.664171081076821,5.24688651700904,14.5216232928574));
#37787=CARTESIAN_POINT('Ctrl Pts',(-1.92626575763464,4.9254889684451,14.6009951829108));
#37788=CARTESIAN_POINT('Ctrl Pts',(-4.04746852150321,3.4042532095528,14.6803670729642));
#37789=CARTESIAN_POINT('Ctrl Pts',(-5.1827169124532,1.05374890400015,14.7597389630177));
#37790=CARTESIAN_POINT('Ctrl Pts',(-5.05546693527891,-1.55344630213332,
14.839110853071));
#37791=CARTESIAN_POINT('Ctrl Pts',(-3.69671640275692,-3.78222542756219,
14.9184827431245));
#37792=CARTESIAN_POINT('Ctrl Pts',(-1.43745393706629,-5.08966281065088,
14.9978546331779));
#37793=CARTESIAN_POINT('Ctrl Pts',(1.17196912594334,-5.15726959884254,15.0772265232312));
#37794=CARTESIAN_POINT('Ctrl Pts',(3.49590310398282,-3.96857692817882,15.1565984132847));
#37795=CARTESIAN_POINT('Ctrl Pts',(4.96824282394235,-1.81314770210679,15.2359703033381));
#37796=CARTESIAN_POINT('Ctrl Pts',(5.23032958900857,0.783960290864088,15.3153421933915));
#37797=CARTESIAN_POINT('Ctrl Pts',(4.21831964333036,3.19009729224721,15.3947140834449));
#37798=CARTESIAN_POINT('Ctrl Pts',(2.17873636962922,4.81913365439941,15.4740859734983));
#37799=CARTESIAN_POINT('Ctrl Pts',(-0.391582261162836,5.27423972531144,
15.5534578635517));
#37800=CARTESIAN_POINT('Ctrl Pts',(-2.86651231988745,4.44455267346898,15.6328297536051));
#37801=CARTESIAN_POINT('Ctrl Pts',(-4.64316632240643,2.53218242822043,15.7122016436585));
#37802=CARTESIAN_POINT('Ctrl Pts',(-5.28875528625864,0.00297814834715876,
15.7915735337119));
#37803=CARTESIAN_POINT('Ctrl Pts',(-4.64601516884489,-2.52695160186966,
15.8709454237653));
#37804=CARTESIAN_POINT('Ctrl Pts',(-2.87151604007055,-4.44132153518687,
15.9503173138187));
#37805=CARTESIAN_POINT('Ctrl Pts',(-0.397521959947054,-5.27379537322474,
16.0296892038721));
#37806=CARTESIAN_POINT('Ctrl Pts',(2.1733075897557,-4.82158433170501,16.1090610939255));
#37807=CARTESIAN_POINT('Ctrl Pts',(4.21472422106055,-3.1948460193553,16.1884329839789));
#37808=CARTESIAN_POINT('Ctrl Pts',(5.22944336137754,-0.789850288404984,
16.2678048740323));
#37809=CARTESIAN_POINT('Ctrl Pts',(4.97028167379658,1.80755122457726,16.3471767640857));
#37810=CARTESIAN_POINT('Ctrl Pts',(3.50037037246945,3.9646372600474,16.4265486541391));
#37811=CARTESIAN_POINT('Ctrl Pts',(1.17777659548083,5.15594643483254,16.5059205441925));
#37812=CARTESIAN_POINT('Ctrl Pts',(-1.43172095156687,5.09127847004474,16.5852924342459));
#37813=CARTESIAN_POINT('Ctrl Pts',(-3.69245444696213,3.78638634033038,16.6646643242993));
#37814=CARTESIAN_POINT('Ctrl Pts',(-5.05371420635461,1.5591388772047,16.7440362143527));
#37815=CARTESIAN_POINT('Ctrl Pts',(-5.18390038229795,-1.04791136166686,
16.8234081044061));
#37816=CARTESIAN_POINT('Ctrl Pts',(-4.05129987868913,-3.39969271923294,
16.9027799944595));
#37817=CARTESIAN_POINT('Ctrl Pts',(-1.93181173129365,-4.9233164424874,16.9821518845129));
#37818=CARTESIAN_POINT('Ctrl Pts',(0.658261551986501,-5.24763120247215,
17.0615237745663));
#37819=CARTESIAN_POINT('Ctrl Pts',(3.08798363825942,-4.29363457062506,17.1408956646198));
#37820=CARTESIAN_POINT('Ctrl Pts',(4.76548000969996,-2.29371814868002,17.2202675546731));
#37821=CARTESIAN_POINT('Ctrl Pts',(5.28211549991427,0.264943102456271,17.2996394447266));
#37822=CARTESIAN_POINT('Ctrl Pts',(4.51204028846775,2.7590644882845,17.3790113347799));
#37823=CARTESIAN_POINT('Ctrl Pts',(2.64284027062647,4.58108446095533,17.4583832248334));
#37824=CARTESIAN_POINT('Ctrl Pts',(0.129853572473924,5.28716128664959,17.5377551148867));
#37825=CARTESIAN_POINT('Ctrl Pts',(-2.41477151246584,4.70529942618515,17.6171270049402));
#37826=CARTESIAN_POINT('Ctrl Pts',(-4.37115162329109,2.9772330746438,17.6964988949936));
#37827=CARTESIAN_POINT('Ctrl Pts',(-5.2627514922539,0.523926824466488,17.775870785047));
#37828=CARTESIAN_POINT('Ctrl Pts',(-4.87231403886184,-2.05702097999283,
17.8552426751004));
#37829=CARTESIAN_POINT('Ctrl Pts',(-3.29507231119166,-4.13685632854999,
17.9346145651538));
#37830=CARTESIAN_POINT('Ctrl Pts',(-0.915005995631555,-5.20901304408194,
18.0139864552072));
#37831=CARTESIAN_POINT('Ctrl Pts',(1.68766624540468,-5.01217052435341,18.0933583452606));
#37832=CARTESIAN_POINT('Ctrl Pts',(3.8797695997979,-3.59455409188004,18.172730235314));
#37833=CARTESIAN_POINT('Ctrl Pts',(5.12574462250332,-1.30097287489382,18.2521021253674));
#37834=CARTESIAN_POINT('Ctrl Pts',(5.12503498129813,1.3088817301615,18.3314740154208));
#37835=CARTESIAN_POINT('Ctrl Pts',(3.87222469260764,3.60110493868871,18.4108459054742));
#37836=CARTESIAN_POINT('Ctrl Pts',(1.68303999757325,5.01382783115876,18.4902177955276));
#37837=CARTESIAN_POINT('Ctrl Pts',(-0.929079443196312,5.2094618875472,18.569589685581));
#37838=CARTESIAN_POINT('Ctrl Pts',(-3.29092685490746,4.12830747359753,18.6489615756344));
#37839=CARTESIAN_POINT('Ctrl Pts',(-5.42625155540715,1.36247937795741,18.7547907623723));
#37840=CARTESIAN_POINT('Ctrl Pts',(-4.95432466322409,-3.37745298000962,
18.8870772457946));
#37841=CARTESIAN_POINT('Ctrl Pts',(0.158509478955228,-5.99736559883162,
19.0458210259014));
#37842=CARTESIAN_POINT('Ctrl Pts',(5.11967904485094,-3.11863163173532,19.2045648060083));
#37843=CARTESIAN_POINT('Ctrl Pts',(5.39954635636598,2.60828838171404,19.363308586115));
#37844=CARTESIAN_POINT('Ctrl Pts',(0.736723079475925,5.95134306184737,19.5220523662219));
#37845=CARTESIAN_POINT('Ctrl Pts',(-4.59927593805429,3.84720861430001,19.6807961463287));
#37846=CARTESIAN_POINT('Ctrl Pts',(-5.72720375155086,-1.77677009197966,
19.8395399264355));
#37847=CARTESIAN_POINT('Ctrl Pts',(-1.61419617037545,-5.77483540889735,
19.9982837065423));
#37848=CARTESIAN_POINT('Ctrl Pts',(3.97578039972893,-4.48936692070975,20.1570274866491));
#37849=CARTESIAN_POINT('Ctrl Pts',(5.92771323046147,0.905806267444479,20.3157712667559));
#37850=CARTESIAN_POINT('Ctrl Pts',(2.45559119020176,5.46873373673919,20.4745150468627));
#37851=CARTESIAN_POINT('Ctrl Pts',(-3.26379011618977,5.03400372054189,20.6332588269695));
#37852=CARTESIAN_POINT('Ctrl Pts',(-5.99600976813329,-0.0197068834827358,
20.7920026070763));
#37853=CARTESIAN_POINT('Ctrl Pts',(-3.70230252414087,-4.19446206534972,
20.9242890904987));
#37854=CARTESIAN_POINT('Ctrl Pts',(-0.376480053418488,-5.26605971579228,
21.0301182772365));
#37855=CARTESIAN_POINT('Ctrl Pts',(2.18257651229242,-4.8205851862161,21.10949016729));
#37856=CARTESIAN_POINT('Ctrl Pts',(4.22530652207796,-3.18086119603153,21.1888620573433));
#37857=CARTESIAN_POINT('Ctrl Pts',(5.23050112077121,-0.777135043026565,
21.2682339473968));
#37858=CARTESIAN_POINT('Ctrl Pts',(4.96594823061178,1.82167865277159,21.3476058374501));
#37859=CARTESIAN_POINT('Ctrl Pts',(3.48937383888172,3.97367066688458,21.4269777275036));
#37860=CARTESIAN_POINT('Ctrl Pts',(1.16402860508423,5.15930893371516,21.5063496175569));
#37861=CARTESIAN_POINT('Ctrl Pts',(-1.44552439996815,5.08729102078623,21.5857215076104));
#37862=CARTESIAN_POINT('Ctrl Pts',(-3.70260503654192,3.77647571272897,21.6650933976637));
#37863=CARTESIAN_POINT('Ctrl Pts',(-5.057922432142,1.54547807796832,21.7444652877172));
#37864=CARTESIAN_POINT('Ctrl Pts',(-5.18104412158608,-1.06186685398839,
21.8238371777705));
#37865=CARTESIAN_POINT('Ctrl Pts',(-4.04212630117128,-3.41061102326193,
21.903209067824));
#37866=CARTESIAN_POINT('Ctrl Pts',(-1.91852825506946,-4.92850206746972,
21.9825809578774));
#37867=CARTESIAN_POINT('Ctrl Pts',(0.672404619068471,-5.245839892308,22.0619528479308));
#37868=CARTESIAN_POINT('Ctrl Pts',(3.09954884704109,-4.28529268150223,22.1413247379842));
#37869=CARTESIAN_POINT('Ctrl Pts',(4.77164579536192,-2.28086298099128,22.2206966280376));
#37870=CARTESIAN_POINT('Ctrl Pts',(5.28138253005217,0.279182711729235,22.300068518091));
#37871=CARTESIAN_POINT('Ctrl Pts',(4.50458503707303,2.77121862106756,22.3794404081444));
#37872=CARTESIAN_POINT('Ctrl Pts',(2.63048120009391,4.58819259887664,22.4588122981978));
#37873=CARTESIAN_POINT('Ctrl Pts',(0.115597647321455,5.28749259670008,22.5381841882512));
#37874=CARTESIAN_POINT('Ctrl Pts',(-2.42744506809483,4.69877132337436,22.6175560783046));
#37875=CARTESIAN_POINT('Ctrl Pts',(-4.37916762715256,2.96543963879382,22.696927968358));
#37876=CARTESIAN_POINT('Ctrl Pts',(-5.26413459813381,0.509733484286287,
22.7762998584114));
#37877=CARTESIAN_POINT('Ctrl Pts',(-4.86677005798463,-2.07014265165558,
22.8556717484648));
#37878=CARTESIAN_POINT('Ctrl Pts',(-3.28387109087741,-4.14573660239302,
22.9350436385182));
#37879=CARTESIAN_POINT('Ctrl Pts',(-0.901028401772815,-5.21143830245831,
23.0144155285717));
#37880=CARTESIAN_POINT('Ctrl Pts',(1.70130281532621,-5.00764516247504,23.093787418625));
#37881=CARTESIAN_POINT('Ctrl Pts',(3.88920043041414,-3.58400074773866,23.1731593086785));
#37882=CARTESIAN_POINT('Ctrl Pts',(5.12969743029434,-1.28730168253193,23.2525311987318));
#37883=CARTESIAN_POINT('Ctrl Pts',(5.12061148999571,1.32298122241883,23.3319030887853));
#37884=CARTESIAN_POINT('Ctrl Pts',(3.86415592530766,3.6109888303426,23.4112749788386));
#37885=CARTESIAN_POINT('Ctrl Pts',(1.66640053022393,5.01936755177924,23.4906468688921));
#37886=CARTESIAN_POINT('Ctrl Pts',(-0.937286345425383,5.20503944789203,
23.5700187589454));
#37887=CARTESIAN_POINT('Ctrl Pts',(-3.31265234202061,4.12277525560054,23.6493906489989));
#37888=CARTESIAN_POINT('Ctrl Pts',(-4.88106356050821,2.03621213668325,23.7287625390522));
#37889=CARTESIAN_POINT('Ctrl Pts',(-5.26045849971908,-0.546367751667005,
23.8081344291057));
#37890=CARTESIAN_POINT('Ctrl Pts',(-4.35841739221935,-2.99585366506712,
23.887506319159));
#37891=CARTESIAN_POINT('Ctrl Pts',(-2.3946754551717,-4.71555625687105,23.9668782092125));
#37892=CARTESIAN_POINT('Ctrl Pts',(0.152404122233421,-5.28655978220554,
24.0462500992659));
#37893=CARTESIAN_POINT('Ctrl Pts',(2.66235839280233,-4.56976904619763,24.1256219893193));
#37894=CARTESIAN_POINT('Ctrl Pts',(4.52376805191542,-2.73979268554746,24.2049938793727));
#37895=CARTESIAN_POINT('Ctrl Pts',(5.28319782677237,-0.242408891126616,
24.2843657694261));
#37896=CARTESIAN_POINT('Ctrl Pts',(4.75565230518779,2.3140251726099,24.3637376594795));
#37897=CARTESIAN_POINT('Ctrl Pts',(3.0696404085172,4.30676782630642,24.4431095495329));
#37898=CARTESIAN_POINT('Ctrl Pts',(0.635870902865647,5.25039137038364,24.5224814395863));
#37899=CARTESIAN_POINT('Ctrl Pts',(-1.95279534724764,4.9150311981795,24.6018533296397));
#37900=CARTESIAN_POINT('Ctrl Pts',(-4.06576497321052,3.38238030533593,24.6812252196931));
#37901=CARTESIAN_POINT('Ctrl Pts',(-5.18832325111748,1.02578905688434,24.7605971097465));
#37902=CARTESIAN_POINT('Ctrl Pts',(-5.04701746921096,-1.58068213527875,
24.8399689997999));
#37903=CARTESIAN_POINT('Ctrl Pts',(-3.67626940318832,-3.80210265806849,
24.9193408898533));
#37904=CARTESIAN_POINT('Ctrl Pts',(-1.40999024783327,-5.09733938916421,
24.9987127799067));
#37905=CARTESIAN_POINT('Ctrl Pts',(1.19975941093347,-5.1508755278289,25.0780846699601));
#37906=CARTESIAN_POINT('Ctrl Pts',(3.51725033281924,-3.94966978918403,25.1574565600135));
#37907=CARTESIAN_POINT('Ctrl Pts',(4.97794685893178,-1.7863332323397,25.2368284500669));
#37908=CARTESIAN_POINT('Ctrl Pts',(5.226026548707,0.812150145920977,25.3162003401203));
#37909=CARTESIAN_POINT('Ctrl Pts',(4.20105773883081,3.21279554629917,25.3955722301737));
#37910=CARTESIAN_POINT('Ctrl Pts',(2.15272056265901,4.83081106300121,25.4749441202272));
#37911=CARTESIAN_POINT('Ctrl Pts',(-0.420014577610356,5.27205169757513,
25.5543160102805));
#37912=CARTESIAN_POINT('Ctrl Pts',(-2.89043509646038,4.42903220810823,25.6336879003339));
#37913=CARTESIAN_POINT('Ctrl Pts',(-4.65675202368223,2.50711027624266,25.7130597903873));
#37914=CARTESIAN_POINT('Ctrl Pts',(-5.28869446548081,-0.0255381695211706,
25.7924316804408));
#37915=CARTESIAN_POINT('Ctrl Pts',(-4.63232264181493,-2.55196557371741,
25.8718035704942));
#37916=CARTESIAN_POINT('Ctrl Pts',(-2.84752727607513,-4.45673981283608,
25.9511754605475));
#37917=CARTESIAN_POINT('Ctrl Pts',(-0.369080568778156,-5.27586209837409,
26.030547350601));
#37918=CARTESIAN_POINT('Ctrl Pts',(2.19927334812716,-4.80979605467087,26.1099192406543));
#37919=CARTESIAN_POINT('Ctrl Pts',(4.23188914543768,-3.17207433835284,26.1892911307078));
#37920=CARTESIAN_POINT('Ctrl Pts',(5.23362611404738,-0.761642334479479,
26.2686630207611));
#37921=CARTESIAN_POINT('Ctrl Pts',(4.96046334571002,1.83432405620638,26.3480349108146));
#37922=CARTESIAN_POINT('Ctrl Pts',(3.47894268615705,3.98345316700778,26.427406800868));
#37923=CARTESIAN_POINT('Ctrl Pts',(1.14995928876529,5.16222190355009,26.5067786909214));
#37924=CARTESIAN_POINT('Ctrl Pts',(-1.45915164597797,5.08348481077201,26.5861505809748));
#37925=CARTESIAN_POINT('Ctrl Pts',(-3.71281646953845,3.76642207019263,26.6655224710282));
#37926=CARTESIAN_POINT('Ctrl Pts',(-5.06204741929919,1.53186725014815,26.7448943610816));
#37927=CARTESIAN_POINT('Ctrl Pts',(-5.17817482237054,-1.07584704130177,
26.824266251135));
#37928=CARTESIAN_POINT('Ctrl Pts',(-4.032910300408,-3.42148737483758,26.9036381411884));
#37929=CARTESIAN_POINT('Ctrl Pts',(-1.90523775596165,-4.93366095719681,
26.9830100312419));
#37930=CARTESIAN_POINT('Ctrl Pts',(0.686546488664775,-5.24400565085624,
27.0623819212952));
#37931=CARTESIAN_POINT('Ctrl Pts',(3.11108952829732,-4.27692217537667,27.1417538113486));
#37932=CARTESIAN_POINT('Ctrl Pts',(4.77777804511651,-2.267989924782,27.221125701402));
#37933=CARTESIAN_POINT('Ctrl Pts',(5.28061040557762,0.293419651379019,27.3004975914554));
#37934=CARTESIAN_POINT('Ctrl Pts',(4.49709775967288,2.7833528499375,27.3798694815089));
#37935=CARTESIAN_POINT('Ctrl Pts',(2.61810205366886,4.59526745509821,27.4592413715622));
#37936=CARTESIAN_POINT('Ctrl Pts',(0.101342482461748,5.28778507964899,27.5386132616156));
#37937=CARTESIAN_POINT('Ctrl Pts',(-2.44010389315526,4.69220996311103,27.617985151669));
#37938=CARTESIAN_POINT('Ctrl Pts',(-4.38714636147802,2.95362288558985,27.6973570417224));
#37939=CARTESIAN_POINT('Ctrl Pts',(-5.26548968692851,0.495539810872365,
27.7767289317758));
#37940=CARTESIAN_POINT('Ctrl Pts',(-4.86117137960698,-2.08325566491491,
27.8561008218293));
#37941=CARTESIAN_POINT('Ctrl Pts',(-3.27268248423349,-4.15457467193712,
27.9354727118826));
#37942=CARTESIAN_POINT('Ctrl Pts',(-0.886975379660524,-5.21384848487045,
28.0148446019361));
#37943=CARTESIAN_POINT('Ctrl Pts',(1.71479696411104,-5.00304034754724,28.0942164919895));
#37944=CARTESIAN_POINT('Ctrl Pts',(3.89884856306386,-3.57350265560346,28.1735883820429));
#37945=CARTESIAN_POINT('Ctrl Pts',(5.1331492820092,-1.27346762656861,28.2529602720963));
#37946=CARTESIAN_POINT('Ctrl Pts',(5.11702619789033,1.3367812975255,28.3323321621497));
#37947=CARTESIAN_POINT('Ctrl Pts',(3.85440685831077,3.62139325645763,28.4117040522031));
#37948=CARTESIAN_POINT('Ctrl Pts',(1.6528625396316,5.02384183393471,28.4910759422564));
#37949=CARTESIAN_POINT('Ctrl Pts',(-0.951315435152638,5.20249366075061,
28.5704478323099));
#37950=CARTESIAN_POINT('Ctrl Pts',(-3.32375507563475,4.11382954733206,28.6498197223633));
#37951=CARTESIAN_POINT('Ctrl Pts',(-4.8865353366993,2.02304566199065,28.7291916124167));
#37952=CARTESIAN_POINT('Ctrl Pts',(-5.25896640590637,-0.560547668676075,
28.8085635024701));
#37953=CARTESIAN_POINT('Ctrl Pts',(-4.35032489915935,-3.00759282800452,
28.8879353925235));
#37954=CARTESIAN_POINT('Ctrl Pts',(-2.38195387625792,-4.72199503162487,
28.9673072825769));
#37955=CARTESIAN_POINT('Ctrl Pts',(0.166655838534471,-5.28612969750008,
29.0466791726303));
#37956=CARTESIAN_POINT('Ctrl Pts',(2.67466855994625,-4.56257486971391,29.1260510626837));
#37957=CARTESIAN_POINT('Ctrl Pts',(4.53113794043359,-2.72758690275364,29.2054229527372));
#37958=CARTESIAN_POINT('Ctrl Pts',(5.28383214813505,-0.228164803693758,
29.2847948427905));
#37959=CARTESIAN_POINT('Ctrl Pts',(4.74939654011487,2.32683773651173,29.3641667328439));
#37960=CARTESIAN_POINT('Ctrl Pts',(3.05801844753361,4.31502775447088,29.4435386228973));
#37961=CARTESIAN_POINT('Ctrl Pts',(0.621713829942241,5.25208656259286,29.5229105129507));
#37962=CARTESIAN_POINT('Ctrl Pts',(-1.96603890048284,4.90974870936366,29.6022824030042));
#37963=CARTESIAN_POINT('Ctrl Pts',(-4.07486890650364,3.37140693807791,29.6816542930575));
#37964=CARTESIAN_POINT('Ctrl Pts',(-5.19106986646947,1.01179789915904,29.7610261831109));
#37965=CARTESIAN_POINT('Ctrl Pts',(-5.04273769720158,-1.59428286841832,
29.8403980731643));
#37966=CARTESIAN_POINT('Ctrl Pts',(-3.66600578680595,-3.81199985813419,
29.9197699632177));
#37967=CARTESIAN_POINT('Ctrl Pts',(-1.39624298131062,-5.10112212012718,
29.9991418532712));
#37968=CARTESIAN_POINT('Ctrl Pts',(1.21364152390063,-5.1476223247995,30.0785137433246));
#37969=CARTESIAN_POINT('Ctrl Pts',(3.52788564023963,-3.94017312521939,30.157885633378));
#37970=CARTESIAN_POINT('Ctrl Pts',(4.98274462345863,-1.7729064737611,30.2372575234313));
#37971=CARTESIAN_POINT('Ctrl Pts',(5.22381804552127,0.826236270443475,30.3166294134848));
#37972=CARTESIAN_POINT('Ctrl Pts',(4.19238095442003,3.22410968801099,30.3960013035382));
#37973=CARTESIAN_POINT('Ctrl Pts',(2.13968914249988,4.83659712202475,30.4753731935916));
#37974=CARTESIAN_POINT('Ctrl Pts',(-0.434226208411599,5.27090020273941,
30.554745083645));
#37975=CARTESIAN_POINT('Ctrl Pts',(-2.90236501609743,4.4212236610065,30.6341169736984));
#37976=CARTESIAN_POINT('Ctrl Pts',(-4.66349413013793,2.49454682166501,30.7134888637518));
#37977=CARTESIAN_POINT('Ctrl Pts',(-5.28860639654603,-0.0397961018483339,
30.7928607538052));
#37978=CARTESIAN_POINT('Ctrl Pts',(-4.62542585088724,-2.56444478303865,
30.8722326438586));
#37979=CARTESIAN_POINT('Ctrl Pts',(-2.83550180615875,-4.46440039138299,
30.951604533912));
#37980=CARTESIAN_POINT('Ctrl Pts',(-0.354855797726762,-5.27683794616905,
31.0309764239654));
#37981=CARTESIAN_POINT('Ctrl Pts',(2.21223229757146,-4.80384945735102,31.1103483140188));
#37982=CARTESIAN_POINT('Ctrl Pts',(4.24042550187443,-3.16065387386267,31.1897202040722));
#37983=CARTESIAN_POINT('Ctrl Pts',(5.23566043994338,-0.747530002690045,
31.2690920941256));
#37984=CARTESIAN_POINT('Ctrl Pts',(4.95550008377996,1.84769052250822,31.348463984179));
#37985=CARTESIAN_POINT('Ctrl Pts',(3.46819087602115,3.99281772621712,31.4278358742324));
#37986=CARTESIAN_POINT('Ctrl Pts',(1.13603804757386,5.16530336977167,31.5072077642858));
#37987=CARTESIAN_POINT('Ctrl Pts',(-1.47285113468488,5.07953254565492,31.5865796543392));
#37988=CARTESIAN_POINT('Ctrl Pts',(-3.72295704063504,3.75639883677117,31.6659515443926));
#37989=CARTESIAN_POINT('Ctrl Pts',(-5.06615885211213,1.51821468589782,31.745323434446));
#37990=CARTESIAN_POINT('Ctrl Pts',(-5.17525558096714,-1.08980320194903,
31.8246953244994));
#37991=CARTESIAN_POINT('Ctrl Pts',(-4.02367150553249,-3.43234744203962,
31.9040672145529));
#37992=CARTESIAN_POINT('Ctrl Pts',(-1.89192995759591,-4.93877944262154,
31.9834391046062));
#37993=CARTESIAN_POINT('Ctrl Pts',(0.70068154029511,-5.24213570278371,32.0628109946597));
#37994=CARTESIAN_POINT('Ctrl Pts',(3.12260856590247,-4.26851930901834,32.142182884713));
#37995=CARTESIAN_POINT('Ctrl Pts',(4.78387505663285,-2.25510105978337,32.2215547747665));
#37996=CARTESIAN_POINT('Ctrl Pts',(5.27980017249531,0.307654816033343,32.3009266648198));
#37997=CARTESIAN_POINT('Ctrl Pts',(4.48957765297736,2.79546665964672,32.3802985548733));
#37998=CARTESIAN_POINT('Ctrl Pts',(2.60570395470567,4.60230901263064,32.4596704449267));
#37999=CARTESIAN_POINT('Ctrl Pts',(0.0870865406955613,5.28803907717593,
32.5390423349801));
#38000=CARTESIAN_POINT('Ctrl Pts',(-2.45274496186521,4.68561452739711,32.6184142250335));
#38001=CARTESIAN_POINT('Ctrl Pts',(-4.39509322077448,2.94178465017617,32.6977861150869));
#38002=CARTESIAN_POINT('Ctrl Pts',(-5.26680649947691,0.48134254370224,32.7771580051403));
#38003=CARTESIAN_POINT('Ctrl Pts',(-4.85553737278523,-2.09635354098391,
32.8565298951937));
#38004=CARTESIAN_POINT('Ctrl Pts',(-3.26147008963279,-4.16338254328624,
32.9359017852471));
#38005=CARTESIAN_POINT('Ctrl Pts',(-0.8729159117874,-5.21622077353502,33.0152736753005));
#38006=CARTESIAN_POINT('Ctrl Pts',(1.72827865000283,-4.99839916925953,33.0946455653539));
#38007=CARTESIAN_POINT('Ctrl Pts',(3.9084683581323,-3.5629785911213,33.1740174554073));
#38008=CARTESIAN_POINT('Ctrl Pts',(5.13656382546866,-1.25962431470524,33.2533893454607));
#38009=CARTESIAN_POINT('Ctrl Pts',(5.11340371451205,1.35057165664188,33.3327612355141));
#38010=CARTESIAN_POINT('Ctrl Pts',(3.84462977702742,3.63177136187071,33.4121331255675));
#38011=CARTESIAN_POINT('Ctrl Pts',(1.63931253580255,5.02827960213734,33.4915050156209));
#38012=CARTESIAN_POINT('Ctrl Pts',(-0.965337610587002,5.19991006123145,
33.5708769056743));
#38013=CARTESIAN_POINT('Ctrl Pts',(-3.33483365177614,4.1048539392153,33.6502487957277));
#38014=CARTESIAN_POINT('Ctrl Pts',(-4.89197159692173,2.00986448354636,33.7296206857811));
#38015=CARTESIAN_POINT('Ctrl Pts',(-5.25743608925264,-0.574723511554913,
33.8089925758345));
#38016=CARTESIAN_POINT('Ctrl Pts',(-4.34220078737896,-3.01931013137032,
33.888364465888));
#38017=CARTESIAN_POINT('Ctrl Pts',(-2.36921498499824,-4.72839948631349,
33.9677363559413));
#38018=CARTESIAN_POINT('Ctrl Pts',(0.18090634355963,-5.28566119252548,34.0471082459947));
#38019=CARTESIAN_POINT('Ctrl Pts',(2.68695928725581,-4.55534753185087,34.1264801360481));
#38020=CARTESIAN_POINT('Ctrl Pts',(4.53847489605999,-2.71536129550809,34.2058520261016));
#38021=CARTESIAN_POINT('Ctrl Pts',(5.28442806592769,-0.21391905792982,34.2852239161549));
#38022=CARTESIAN_POINT('Ctrl Pts',(4.74310625581857,2.3396333886583,34.3645958062084));
#38023=CARTESIAN_POINT('Ctrl Pts',(3.04637426047967,4.32325632045994,34.4439676962618));
#38024=CARTESIAN_POINT('Ctrl Pts',(0.607552238322964,5.25374358196314,34.5233395863151));
#38025=CARTESIAN_POINT('Ctrl Pts',(-1.97926816429518,4.90443053586424,34.6027114763686));
#38026=CARTESIAN_POINT('Ctrl Pts',(-4.08394322312674,3.36040906700167,34.6820833664219));
#38027=CARTESIAN_POINT('Ctrl Pts',(-5.19377875245966,0.997799387556786,
34.7614552564754));
#38028=CARTESIAN_POINT('Ctrl Pts',(-5.03842127392763,-1.60787201410546,
34.8408271465287));
#38029=CARTESIAN_POINT('Ctrl Pts',(-3.65571552542313,-3.82186935209593,
34.9201990365822));
#38030=CARTESIAN_POINT('Ctrl Pts',(-1.38248556671468,-5.10486777548014,
34.9995709266355));
#38031=CARTESIAN_POINT('Ctrl Pts',(1.22751481596557,-5.14433170819057,35.078942816689));
#38032=CARTESIAN_POINT('Ctrl Pts',(3.53849530653457,-3.93064782357091,35.1583147067423));
#38033=CARTESIAN_POINT('Ctrl Pts',(4.98750617275828,-1.75946682947078,35.2376865967958));
#38034=CARTESIAN_POINT('Ctrl Pts',(5.22157157495577,0.840316389774704,35.3170584868492));
#38035=CARTESIAN_POINT('Ctrl Pts',(4.18367369924664,3.23540039647985,35.3964303769026));
#38036=CARTESIAN_POINT('Ctrl Pts',(2.12664217080567,4.8423480280398,35.4758022669559));
#38037=CARTESIAN_POINT('Ctrl Pts',(-0.448434683200953,5.2697103983248,35.5551741570095));
#38038=CARTESIAN_POINT('Ctrl Pts',(-2.91427384097317,4.41338297988397,35.6345460470627));
#38039=CARTESIAN_POINT('Ctrl Pts',(-4.67020234172003,2.48196523640092,35.7139179371163));
#38040=CARTESIAN_POINT('Ctrl Pts',(-5.28847988934142,-0.0540537449324728,
35.7932898271696));
#38041=CARTESIAN_POINT('Ctrl Pts',(-4.61849544177097,-2.57690535364626,
35.872661717223));
#38042=CARTESIAN_POINT('Ctrl Pts',(-2.82345572745135,-4.47202852209511,
35.9520336072764));
#38043=CARTESIAN_POINT('Ctrl Pts',(-0.340628447537815,-5.27777544122882,
36.0314054973298));
#38044=CARTESIAN_POINT('Ctrl Pts',(2.22517516822766,-4.79786794503694,36.1107773873833));
#38045=CARTESIAN_POINT('Ctrl Pts',(4.2489310383545,-3.14921043733466,36.1901492774366));
#38046=CARTESIAN_POINT('Ctrl Pts',(5.23765671238758,-0.733412237756749,
36.2695211674901));
#38047=CARTESIAN_POINT('Ctrl Pts',(4.95050080463952,1.8610435595583,36.3488930575434));
#38048=CARTESIAN_POINT('Ctrl Pts',(3.45741385862894,4.002153265115,36.4282649475969));
#38049=CARTESIAN_POINT('Ctrl Pts',(1.12210854951209,5.16834729390565,36.5076368376502));
#38050=CARTESIAN_POINT('Ctrl Pts',(-1.4865399185207,5.07554336184357,36.5870087277037));
#38051=CARTESIAN_POINT('Ctrl Pts',(-3.73307055280216,3.74634830136112,36.666380617757));
#38052=CARTESIAN_POINT('Ctrl Pts',(-5.07023346343257,1.50455108706837,36.7457525078105));
#38053=CARTESIAN_POINT('Ctrl Pts',(-5.17229872514219,-1.10375144176689,
36.8251243978638));
#38054=CARTESIAN_POINT('Ctrl Pts',(-4.01440346609619,-3.44318256250012,
36.9044962879173));
#38055=CARTESIAN_POINT('Ctrl Pts',(-1.87860840844056,-4.94386203236358,
36.9838681779707));
#38056=CARTESIAN_POINT('Ctrl Pts',(0.71481149928202,-5.24022765419639,37.0632400680241));
#38057=CARTESIAN_POINT('Ctrl Pts',(3.13410490798792,-4.26008541851396,37.1426119580775));
#38058=CARTESIAN_POINT('Ctrl Pts',(4.78993729833158,-2.24219580442096,37.2219838481309));
#38059=CARTESIAN_POINT('Ctrl Pts',(5.27895156514787,0.321887744613352,37.3013557381843));
#38060=CARTESIAN_POINT('Ctrl Pts',(4.48202491545551,2.80756015154514,37.3807276282377));
#38061=CARTESIAN_POINT('Ctrl Pts',(2.59328691715162,4.6093171199916,37.4600995182911));
#38062=CARTESIAN_POINT('Ctrl Pts',(0.0728299659736646,5.28825464055466,
37.5394714083445));
#38063=CARTESIAN_POINT('Ctrl Pts',(-2.46536820371075,4.67898503603898,37.6188432983979));
#38064=CARTESIAN_POINT('Ctrl Pts',(-4.40300813596802,2.92992503348812,37.6982151884513));
#38065=CARTESIAN_POINT('Ctrl Pts',(-5.26808503220261,0.467141778084607,
37.7775870785047));
#38066=CARTESIAN_POINT('Ctrl Pts',(-4.84986807528987,-2.10943618050861,
37.8569589685581));
#38067=CARTESIAN_POINT('Ctrl Pts',(-3.2502339902585,-4.17216015459505,37.9363308586115));
#38068=CARTESIAN_POINT('Ctrl Pts',(-0.858850099431265,-5.21855515011692,
38.0157027486649));
#38069=CARTESIAN_POINT('Ctrl Pts',(1.74174777450972,-4.99372166181591,38.0950746387183));
#38070=CARTESIAN_POINT('Ctrl Pts',(3.91805974601555,-3.55242863073569,38.1744465287717));
#38071=CARTESIAN_POINT('Ctrl Pts',(5.13994103560184,-1.24577184719802,38.2538184188251));
#38072=CARTESIAN_POINT('Ctrl Pts',(5.10974406648872,1.36435219862427,38.3331903088785));
#38073=CARTESIAN_POINT('Ctrl Pts',(3.83482475204887,3.64212307300276,38.4125621989319));
#38074=CARTESIAN_POINT('Ctrl Pts',(1.62575061805696,5.03268082057242,38.4919340889853));
#38075=CARTESIAN_POINT('Ctrl Pts',(-0.979352771366501,5.19728867487039,
38.5713059790387));
#38076=CARTESIAN_POINT('Ctrl Pts',(-3.3458879870052,4.09584848370752,38.6506778690921));
#38077=CARTESIAN_POINT('Ctrl Pts',(-4.89737230716795,1.99666872129193,38.7300497591456));
#38078=CARTESIAN_POINT('Ctrl Pts',(-5.2558675504918,-0.588895222855594,
38.809421649199));
#38079=CARTESIAN_POINT('Ctrl Pts',(-4.33404513553914,-3.03100540392653,
38.8887935392523));
#38080=CARTESIAN_POINT('Ctrl Pts',(-2.35645883694701,-4.73476973691708,
38.9681654293058));
#38081=CARTESIAN_POINT('Ctrl Pts',(0.195155463808245,-5.28515396379923,
39.0475373193592));
#38082=CARTESIAN_POINT('Ctrl Pts',(2.69923061743519,-4.54808766460433,39.1269092094126));
#38083=CARTESIAN_POINT('Ctrl Pts',(4.5457786161602,-2.70311485851688,39.2062810994659));
#38084=CARTESIAN_POINT('Ctrl Pts',(5.28498604656423,-0.199673823356607,
39.2856529895194));
#38085=CARTESIAN_POINT('Ctrl Pts',(4.73678060915317,2.35241593705468,39.3650248795727));
#38086=CARTESIAN_POINT('Ctrl Pts',(3.03470961035893,4.33144609848054,39.4443967696262));
#38087=CARTESIAN_POINT('Ctrl Pts',(0.593383061700927,5.25537632570972,39.5237686596795));
#38088=CARTESIAN_POINT('Ctrl Pts',(-1.99247705733066,4.8990504464678,39.603140549733));
#38089=CARTESIAN_POINT('Ctrl Pts',(-4.09299916691649,3.34943642687039,39.6825124397864));
#38090=CARTESIAN_POINT('Ctrl Pts',(-5.19642846461573,0.983699440459269,
39.7618843298398));
#38091=CARTESIAN_POINT('Ctrl Pts',(-5.03410925482033,-1.62126816458454,
39.8412562198932));
#38092=CARTESIAN_POINT('Ctrl Pts',(-3.6453165085118,-3.83208153227987,39.9206281099466));
#38093=CARTESIAN_POINT('Ctrl Pts',(-2.12771778283764,-4.68247622999901,
39.9735427033155));
#38094=CARTESIAN_POINT('Ctrl Pts',(-1.31303618635638,-4.90075024188325,
40.));
#38095=CARTESIAN_POINT('Ctrl Pts',(-3.43378788736187,2.93584158412999,-1.38777878078145E-15));
#38096=CARTESIAN_POINT('Ctrl Pts',(-3.5274298169339,2.83894612463338,-1.38777878078145E-15));
#38097=CARTESIAN_POINT('Ctrl Pts',(-3.61644080326455,2.73799316940158,-1.70682494898246E-15));
#38098=CARTESIAN_POINT('Ctrl Pts',(-3.70070760607863,2.63340714286309,-1.68962066560141E-15));
#38099=CARTESIAN_POINT('Ctrl Pts',(-3.78643913867677,2.52700319677679,-1.67211733650556E-15));
#38100=CARTESIAN_POINT('Ctrl Pts',(-3.86726060843671,2.41683829132909,-1.52825423918462E-15));
#38101=CARTESIAN_POINT('Ctrl Pts',(-3.9430233259709,2.30331415642333,-1.42247325030098E-15));
#38102=CARTESIAN_POINT('Ctrl Pts',(-4.01958942326278,2.18858622372678,-1.31557057111923E-15));
#38103=CARTESIAN_POINT('Ctrl Pts',(-4.09098941448581,2.07042685422507,-1.45703061823736E-15));
#38104=CARTESIAN_POINT('Ctrl Pts',(-4.15703260143776,1.94921318851517,-1.40165656858926E-15));
#38105=CARTESIAN_POINT('Ctrl Pts',(-4.22276474819078,1.82857039656885,-1.34654331125317E-15));
#38106=CARTESIAN_POINT('Ctrl Pts',(-4.28319084758819,1.70490133278768,-1.76868280947178E-15));
#38107=CARTESIAN_POINT('Ctrl Pts',(-4.33807945470206,1.57855051046471,-1.88044024795886E-15));
#38108=CARTESIAN_POINT('Ctrl Pts',(-4.35502796120398,1.53953589802935,-1.91494871469599E-15));
#38109=CARTESIAN_POINT('Ctrl Pts',(-4.37144815676901,1.50026543549027,-1.30689270547165E-15));
#38110=CARTESIAN_POINT('Ctrl Pts',(-4.38733228779962,1.46074889051522,-1.32532873564628E-15));
#38111=CARTESIAN_POINT('Ctrl Pts',(-4.39376253093777,1.44475173009898,-1.33279204328941E-15));
#38112=CARTESIAN_POINT('Ctrl Pts',(-4.40010357988131,1.42871748389362,-1.28259685789569E-15));
#38113=CARTESIAN_POINT('Ctrl Pts',(-4.4063520165592,1.41265478977856,-1.29063426612674E-15));
#38114=CARTESIAN_POINT('Ctrl Pts',(-4.45729152748394,1.28170591015729,-1.35615811881152E-15));
#38115=CARTESIAN_POINT('Ctrl Pts',(-4.50214144181921,1.14871482526442,-2.13815754900839E-15));
#38116=CARTESIAN_POINT('Ctrl Pts',(-4.54074327371246,1.0140904790896,-2.05391259555654E-15));
#38117=CARTESIAN_POINT('Ctrl Pts',(-4.54547345988333,0.997593898764086,
-2.0435893985931E-15));
#38118=CARTESIAN_POINT('Ctrl Pts',(-4.55010977859188,0.981072752949281,
-1.00791691148873E-15));
#38119=CARTESIAN_POINT('Ctrl Pts',(-4.55465189605181,0.964527761093366,
-1.01307850997046E-15));
#38120=CARTESIAN_POINT('Ctrl Pts',(-4.59134817932549,0.830858891175244,
-1.05169067743968E-15));
#38121=CARTESIAN_POINT('Ctrl Pts',(-4.62189967399316,0.695635489793831,
-1.41485248297211E-15));
#38122=CARTESIAN_POINT('Ctrl Pts',(-4.64637428491341,0.559286455771474,
-1.36002320516582E-15));
#38123=CARTESIAN_POINT('Ctrl Pts',(-4.67110897469857,0.42148851201501,-1.30461128535625E-15));
#38124=CARTESIAN_POINT('Ctrl Pts',(-4.68963709540601,0.282540149701787,
-1.43104411647104E-15));
#38125=CARTESIAN_POINT('Ctrl Pts',(-4.70197867697062,0.142866308633218,
-1.36002320516582E-15));
#38126=CARTESIAN_POINT('Ctrl Pts',(-4.71314718957453,0.0164684846393732,
-1.29575284087739E-15));
#38127=CARTESIAN_POINT('Ctrl Pts',(-4.71924875509872,-0.110524098082,-1.66579323769632E-15));
#38128=CARTESIAN_POINT('Ctrl Pts',(-4.72026194547141,-0.237801095913712,
-1.67921232474555E-15));
#38129=CARTESIAN_POINT('Ctrl Pts',(-4.72045200129662,-0.261675913030809,
-1.68172949795545E-15));
#38130=CARTESIAN_POINT('Ctrl Pts',(-4.72046291446759,-0.285560737563283,
-9.9370225703457E-16));
#38131=CARTESIAN_POINT('Ctrl Pts',(-4.72029440609211,-0.309453515786201,
-9.71445146547012E-16));
#38132=CARTESIAN_POINT('Ctrl Pts',(-4.72016631155934,-0.327616021086772,
-9.54526022139039E-16));
#38133=CARTESIAN_POINT('Ctrl Pts',(-4.7199344986873,-0.345781850732525,
-1.1165476318937E-15));
#38134=CARTESIAN_POINT('Ctrl Pts',(-4.7195992402228,-0.363937763232007,
-1.12410081243297E-15));
#38135=CARTESIAN_POINT('Ctrl Pts',(-4.7169715342115,-0.506241106673104,
-1.18330151878048E-15));
#38136=CARTESIAN_POINT('Ctrl Pts',(-4.70799214533038,-0.648137600560786,
-1.67849620506959E-15));
#38137=CARTESIAN_POINT('Ctrl Pts',(-4.69273559502703,-0.789185289486343,
-1.60982338570648E-15));
#38138=CARTESIAN_POINT('Ctrl Pts',(-4.67736001919945,-0.931333376259461,
-1.5406148083796E-15));
#38139=CARTESIAN_POINT('Ctrl Pts',(-4.65560906635571,-1.07262015451611,
-1.29947818212301E-15));
#38140=CARTESIAN_POINT('Ctrl Pts',(-4.62750766548139,-1.21260443247969,
-1.38777878078145E-15));
#38141=CARTESIAN_POINT('Ctrl Pts',(-4.61688292082861,-1.26553052023664,
-1.42116399590398E-15));
#38142=CARTESIAN_POINT('Ctrl Pts',(-4.60534985624838,-1.31827046839259,
-1.10373700911438E-15));
#38143=CARTESIAN_POINT('Ctrl Pts',(-4.59290787692679,-1.37080047994465,
-1.0547118733939E-15));
#38144=CARTESIAN_POINT('Ctrl Pts',(-4.56011975477607,-1.50923186540429,
-9.25516823562078E-16));
#38145=CARTESIAN_POINT('Ctrl Pts',(-4.52102317103095,-1.64620611480812,
-1.41788356490645E-15));
#38146=CARTESIAN_POINT('Ctrl Pts',(-4.47583839059365,-1.78136570298785,
-1.36002320516582E-15));
#38147=CARTESIAN_POINT('Ctrl Pts',(-4.44941052359499,-1.86041841908909,
-1.32618159130998E-15));
#38148=CARTESIAN_POINT('Ctrl Pts',(-4.42089896739826,-1.93885019183042,
-1.30868430769761E-15));
#38149=CARTESIAN_POINT('Ctrl Pts',(-4.3903399301827,-2.01658705378289,-1.30451205393456E-15));
#38150=CARTESIAN_POINT('Ctrl Pts',(-4.37718466105246,-2.05005176450371,
-1.30271595280921E-15));
#38151=CARTESIAN_POINT('Ctrl Pts',(-4.36364988420426,-2.08338766611273,
-1.16152748166208E-15));
#38152=CARTESIAN_POINT('Ctrl Pts',(-4.3497381750326,-2.11658871139626,-1.13797860024079E-15));
#38153=CARTESIAN_POINT('Ctrl Pts',(-4.34244585283277,-2.13399223217085,
-1.12563460794976E-15));
#38154=CARTESIAN_POINT('Ctrl Pts',(-4.33504992528714,-2.15135862906508,
-1.92978013206096E-15));
#38155=CARTESIAN_POINT('Ctrl Pts',(-4.32755662758879,-2.16867384922929,
-1.9151347174784E-15));
#38156=CARTESIAN_POINT('Ctrl Pts',(-4.2701680431329,-2.30128515265925,-1.80297053483165E-15));
#38157=CARTESIAN_POINT('Ctrl Pts',(-4.20699158680529,-2.43109046195038,
-1.71043044263751E-15));
#38158=CARTESIAN_POINT('Ctrl Pts',(-4.13831811099888,-2.55774085897211,
-1.72084568816899E-15));
#38159=CARTESIAN_POINT('Ctrl Pts',(-4.0690864175418,-2.68542074352523,-1.73134559482798E-15));
#38160=CARTESIAN_POINT('Ctrl Pts',(-3.99426770892291,-2.80989493979695,
-1.80815084065395E-15));
#38161=CARTESIAN_POINT('Ctrl Pts',(-3.91410750939009,-2.93079631633735,
-1.80411241501588E-15));
#38162=CARTESIAN_POINT('Ctrl Pts',(-3.83416065570548,-3.05137591465264,
-1.8000847376213E-15));
#38163=CARTESIAN_POINT('Ctrl Pts',(-3.74890035710146,-3.16840239753955,
-1.26386791065628E-15));
#38164=CARTESIAN_POINT('Ctrl Pts',(-3.6585229556131,-3.28149127673775,-1.27675647831893E-15));
#38165=CARTESIAN_POINT('Ctrl Pts',(-3.59945026249498,-3.35540870018578,
-1.2851807347119E-15));
#38166=CARTESIAN_POINT('Ctrl Pts',(-3.5381904788592,-3.42764345712454,-1.45186396209174E-15));
#38167=CARTESIAN_POINT('Ctrl Pts',(-3.47478854700661,-3.49808125449704,
-1.41553435639707E-15));
#38168=CARTESIAN_POINT('Ctrl Pts',(-3.4391425896078,-3.5376829298883,-1.39540507371065E-15));
#38169=CARTESIAN_POINT('Ctrl Pts',(-3.40281937333393,-3.57671648450509,
-1.55816047969468E-15));
#38170=CARTESIAN_POINT('Ctrl Pts',(-3.36583573983685,-3.61517046963578,
-1.55431223447522E-15));
#38171=CARTESIAN_POINT('Ctrl Pts',(-3.34056943595204,-3.64144128139824,
-1.55168320849956E-15));
#38172=CARTESIAN_POINT('Ctrl Pts',(-3.31499488246685,-3.66744157776442,
-1.71311115652187E-15));
#38173=CARTESIAN_POINT('Ctrl Pts',(-3.28911728144163,-3.6931675174981,-1.69309011255336E-15));
#38174=CARTESIAN_POINT('Ctrl Pts',(-3.27259035745335,-3.70959758186502,
-1.68030352265613E-15));
#38175=CARTESIAN_POINT('Ctrl Pts',(-3.25594506354961,-3.7259104717157,-1.35072386705874E-15));
#38176=CARTESIAN_POINT('Ctrl Pts',(-3.23918904311522,-3.74209965697934,
-1.36002320516582E-15));
#38177=CARTESIAN_POINT('Ctrl Pts',(-3.13422859724164,-3.84350942251737,
-1.41827466635674E-15));
#38178=CARTESIAN_POINT('Ctrl Pts',(-3.02485537861799,-3.94013896638234,
-1.29586046630586E-15));
#38179=CARTESIAN_POINT('Ctrl Pts',(-2.91147703861897,-4.03180594754837,
-1.33226762955019E-15));
#38180=CARTESIAN_POINT('Ctrl Pts',(-2.80007805253152,-4.12187261071949,
-1.36803919819172E-15));
#38181=CARTESIAN_POINT('Ctrl Pts',(-2.68481190070853,-4.20714879945784,
-1.75330405072015E-15));
#38182=CARTESIAN_POINT('Ctrl Pts',(-2.5660285220091,-4.28743071443088,-1.77635683940025E-15));
#38183=CARTESIAN_POINT('Ctrl Pts',(-2.51557747120272,-4.32152897813987,
-1.78614808650622E-15));
#38184=CARTESIAN_POINT('Ctrl Pts',(-2.46449152304015,-4.35472587736193,
-1.31186991621621E-15));
#38185=CARTESIAN_POINT('Ctrl Pts',(-2.41279587231268,-4.38700384624999,
-1.27675647831893E-15));
#38186=CARTESIAN_POINT('Ctrl Pts',(-2.38543234505614,-4.40408921163422,
-1.2581702432788E-15));
#38187=CARTESIAN_POINT('Ctrl Pts',(-2.35789457340209,-4.42091901104391,
-1.50863034215941E-15));
#38188=CARTESIAN_POINT('Ctrl Pts',(-2.3302097471481,-4.43747675896359,-1.49880108324396E-15));
#38189=CARTESIAN_POINT('Ctrl Pts',(-2.2023530709709,-4.51394531233533,-1.45340667250483E-15));
#38190=CARTESIAN_POINT('Ctrl Pts',(-2.07127177001784,-4.58467311410489,
-7.9672741319199E-16));
#38191=CARTESIAN_POINT('Ctrl Pts',(-1.93736496285559,-4.64944928440847,
-4.9960036108132E-16));
#38192=CARTESIAN_POINT('Ctrl Pts',(-1.80364190208402,-4.71413656910759,
-2.02881025535331E-16));
#38193=CARTESIAN_POINT('Ctrl Pts',(-1.66710043882179,-4.77288900981815,
-3.16087603122754E-17));
#38194=CARTESIAN_POINT('Ctrl Pts',(-1.52810715957136,-4.82545526764581,
-5.55111512312578E-17));
#38195=CARTESIAN_POINT('Ctrl Pts',(-1.49120032503771,-4.83941316683462,
-6.1857944337824E-17));
#38196=CARTESIAN_POINT('Ctrl Pts',(-1.4541204835251,-4.85293465562285,3.75650465851052E-17));
#38197=CARTESIAN_POINT('Ctrl Pts',(-1.41687422066829,-4.86601447289862,
5.55111512312578E-17));
#38198=CARTESIAN_POINT('Ctrl Pts',(-1.38244754401982,-4.87810413251642,
1.27205291019773E-16));
#38199=CARTESIAN_POINT('Ctrl Pts',(-1.3478786871628,-4.88981645711078,2.24269765851654E-16));
#38200=CARTESIAN_POINT('Ctrl Pts',(-1.31317395760259,-4.90115117757553,
2.22044604925031E-16));
#38201=CARTESIAN_POINT('Ctrl Pts',(4.51755838390264,-0.00010457874560596,
1.61258330249198));
#38202=CARTESIAN_POINT('Ctrl Pts',(4.51776153214983,-0.238054206488734,
1.60420146868401));
#38203=CARTESIAN_POINT('Ctrl Pts',(4.49928771368086,-0.475972597056525,
1.59581963487604));
#38204=CARTESIAN_POINT('Ctrl Pts',(4.46186317968569,-0.710871726876144,
1.58743780106807));
#38205=CARTESIAN_POINT('Ctrl Pts',(4.34373246725773,-1.45233190264972,1.5609805043836));
#38206=CARTESIAN_POINT('Ctrl Pts',(4.03678590132105,-2.16370961033161,1.53452320769914));
#38207=CARTESIAN_POINT('Ctrl Pts',(3.57840923518442,-2.75835983566981,1.50806591101467));
#38208=CARTESIAN_POINT('Ctrl Pts',(3.1200325690478,-3.353010061008,1.4816086143302));
#38209=CARTESIAN_POINT('Ctrl Pts',(2.51022580271121,-3.8309328040025,1.45515131764573));
#38210=CARTESIAN_POINT('Ctrl Pts',(1.82326272299592,-4.13391759737134,1.42869402096126));
#38211=CARTESIAN_POINT('Ctrl Pts',(1.13629964328063,-4.43690239074017,1.4022367242768));
#38212=CARTESIAN_POINT('Ctrl Pts',(0.372180250186614,-4.56494923448333,
1.37577942759233));
#38213=CARTESIAN_POINT('Ctrl Pts',(-0.37602655530059,-4.50246217629702,
1.34932213090786));
#38214=CARTESIAN_POINT('Ctrl Pts',(-1.1242333607878,-4.4399751181107,1.32286483422339));
#38215=CARTESIAN_POINT('Ctrl Pts',(-1.85652757866819,-4.18695415799491,
1.29640753753892));
#38216=CARTESIAN_POINT('Ctrl Pts',(-2.48371659230757,-3.77421694705552,
1.26995024085446));
#38217=CARTESIAN_POINT('Ctrl Pts',(-3.11090560594693,-3.36147973611613,
1.24349294416999));
#38218=CARTESIAN_POINT('Ctrl Pts',(-3.63298941534527,-2.78902627435314,
1.21703564748552));
#38219=CARTESIAN_POINT('Ctrl Pts',(-3.98637877398998,-2.12658080103894,
1.19057835080105));
#38220=CARTESIAN_POINT('Ctrl Pts',(-4.3397681326347,-1.46413532772474,1.16412105411659));
#38221=CARTESIAN_POINT('Ctrl Pts',(-4.52446304052578,-0.711697842859317,
1.13766375743212));
#38222=CARTESIAN_POINT('Ctrl Pts',(-4.51796789313228,0.039085678406338,
1.11120646074765));
#38223=CARTESIAN_POINT('Ctrl Pts',(-4.51147274573878,0.789869199671988,
1.08474916406318));
#38224=CARTESIAN_POINT('Ctrl Pts',(-4.3137875430607,1.53899875733787,1.05829186737871));
#38225=CARTESIAN_POINT('Ctrl Pts',(-3.94899006576281,2.19523105353949,1.03183457069425));
#38226=CARTESIAN_POINT('Ctrl Pts',(-3.58419258846491,2.85146334974111,1.00537727400978));
#38227=CARTESIAN_POINT('Ctrl Pts',(-3.0522828365472,3.41479838447846,0.97891997732531));
#38228=CARTESIAN_POINT('Ctrl Pts',(-2.4180469390755,3.81662285121812,0.952462680640842));
#38229=CARTESIAN_POINT('Ctrl Pts',(-1.78381104160379,4.21844731795778,0.926005383956374));
#38230=CARTESIAN_POINT('Ctrl Pts',(-1.0472489985781,4.45876121669975,0.899548087271906));
#38231=CARTESIAN_POINT('Ctrl Pts',(-0.298073044029486,4.50829405706007,
0.873090790587439));
#38232=CARTESIAN_POINT('Ctrl Pts',(0.451102910519128,4.55782689742038,0.846633493902971));
#38233=CARTESIAN_POINT('Ctrl Pts',(1.21289277659066,4.41657867939905,0.820176197218503));
#38234=CARTESIAN_POINT('Ctrl Pts',(1.89451099954032,4.10175426806438,0.793718900534035));
#38235=CARTESIAN_POINT('Ctrl Pts',(2.57612922248998,3.7869298567297,0.767261603849567));
#38236=CARTESIAN_POINT('Ctrl Pts',(3.17757580231775,3.29852925208169,0.740804307165098));
#38237=CARTESIAN_POINT('Ctrl Pts',(3.6255959515189,2.69603724086577,0.71434701048063));
#38238=CARTESIAN_POINT('Ctrl Pts',(4.07361610072004,2.09354522964985,0.687889713796163));
#38239=CARTESIAN_POINT('Ctrl Pts',(4.36820981929455,1.37696181186601,0.661432417111696));
#38240=CARTESIAN_POINT('Ctrl Pts',(4.47349452055126,0.633569578843809,0.634975120427228));
#38241=CARTESIAN_POINT('Ctrl Pts',(4.50319667153093,0.423849191372714,0.627511181115478));
#38242=CARTESIAN_POINT('Ctrl Pts',(4.51783217716753,0.211995155346536,0.620047241803728));
#38243=CARTESIAN_POINT('Ctrl Pts',(4.51763087883895,0.00011359767064345,
0.612583302491977));
#38244=CARTESIAN_POINT('Ctrl Pts',(1.3130361863565,-4.90075024188322,0.));
#38245=CARTESIAN_POINT('Ctrl Pts',(2.12771778283771,-4.68247622999897,0.0264572966844678));
#38246=CARTESIAN_POINT('Ctrl Pts',(3.64531650851188,-3.8320815322798,0.0793718900534037));
#38247=CARTESIAN_POINT('Ctrl Pts',(5.03410925482037,-1.62126816458446,0.158743780106807));
#38248=CARTESIAN_POINT('Ctrl Pts',(5.19642846461569,0.98369944045933,0.238115670160212));
#38249=CARTESIAN_POINT('Ctrl Pts',(4.09299916691648,3.34943642687043,0.317487560213614));
#38250=CARTESIAN_POINT('Ctrl Pts',(1.99247705733062,4.89905044646781,0.396859450267019));
#38251=CARTESIAN_POINT('Ctrl Pts',(-0.593383061700938,5.2553763257097,0.476231340320422));
#38252=CARTESIAN_POINT('Ctrl Pts',(-3.03470961035893,4.33144609848054,0.555603230373826));
#38253=CARTESIAN_POINT('Ctrl Pts',(-4.73678060915323,2.35241593705463,0.634975120427228));
#38254=CARTESIAN_POINT('Ctrl Pts',(-5.28498604656423,-0.199673823356779,
0.714347010480634));
#38255=CARTESIAN_POINT('Ctrl Pts',(-4.5457786161601,-2.703114858517,0.793718900534037));
#38256=CARTESIAN_POINT('Ctrl Pts',(-2.69923061743508,-4.5480876646044,0.87309079058744));
#38257=CARTESIAN_POINT('Ctrl Pts',(-0.195155463808127,-5.28515396379925,
0.952462680640845));
#38258=CARTESIAN_POINT('Ctrl Pts',(2.35645883694709,-4.73476973691702,1.03183457069425));
#38259=CARTESIAN_POINT('Ctrl Pts',(4.33404513553918,-3.03100540392648,1.11120646074765));
#38260=CARTESIAN_POINT('Ctrl Pts',(5.25586755049182,-0.58889522285553,1.19057835080105));
#38261=CARTESIAN_POINT('Ctrl Pts',(4.89737230716791,1.99666872129196,1.26995024085446));
#38262=CARTESIAN_POINT('Ctrl Pts',(3.34588798700519,4.09584848370755,1.34932213090786));
#38263=CARTESIAN_POINT('Ctrl Pts',(0.979352771366438,5.19728867487042,1.42869402096127));
#38264=CARTESIAN_POINT('Ctrl Pts',(-1.6257506180571,5.03268082057239,1.50806591101467));
#38265=CARTESIAN_POINT('Ctrl Pts',(-3.83482475204895,3.64212307300266,1.58743780106807));
#38266=CARTESIAN_POINT('Ctrl Pts',(-5.10974406648874,1.36435219862418,1.66680969112148));
#38267=CARTESIAN_POINT('Ctrl Pts',(-5.13994103560183,-1.2457718471981,1.74618158117488));
#38268=CARTESIAN_POINT('Ctrl Pts',(-3.91805974601548,-3.55242863073578,
1.82555347122828));
#38269=CARTESIAN_POINT('Ctrl Pts',(-1.74174777450957,-4.99372166181597,
1.90492536128169));
#38270=CARTESIAN_POINT('Ctrl Pts',(0.858850099431454,-5.21855515011689,
1.98429725133509));
#38271=CARTESIAN_POINT('Ctrl Pts',(3.25023399025869,-4.17216015459491,2.0636691413885));
#38272=CARTESIAN_POINT('Ctrl Pts',(4.84986807528995,-2.10943618050841,2.1430410314419));
#38273=CARTESIAN_POINT('Ctrl Pts',(5.26808503220259,0.467141778084788,2.22241292149531));
#38274=CARTESIAN_POINT('Ctrl Pts',(4.40300813596794,2.92992503348825,2.3017848115487));
#38275=CARTESIAN_POINT('Ctrl Pts',(2.46536820371062,4.67898503603904,2.38115670160211));
#38276=CARTESIAN_POINT('Ctrl Pts',(-0.0728299659737919,5.28825464055465,
2.46052859165552));
#38277=CARTESIAN_POINT('Ctrl Pts',(-2.59328691715172,4.60931711999155,2.53990048170891));
#38278=CARTESIAN_POINT('Ctrl Pts',(-4.4820249154556,2.80756015154502,2.61927237176233));
#38279=CARTESIAN_POINT('Ctrl Pts',(-5.27895156514789,0.321887744613165,
2.69864426181572));
#38280=CARTESIAN_POINT('Ctrl Pts',(-4.7899372983315,-2.2421958044211,2.77801615186913));
#38281=CARTESIAN_POINT('Ctrl Pts',(-3.13410490798781,-4.26008541851404,
2.85738804192253));
#38282=CARTESIAN_POINT('Ctrl Pts',(-0.714811499281904,-5.2402276541964,
2.93675993197593));
#38283=CARTESIAN_POINT('Ctrl Pts',(1.8786084084407,-4.94386203236353,3.01613182202934));
#38284=CARTESIAN_POINT('Ctrl Pts',(4.01440346609632,-3.44318256249998,3.09550371208274));
#38285=CARTESIAN_POINT('Ctrl Pts',(5.17229872514222,-1.10375144176671,3.17487560213615));
#38286=CARTESIAN_POINT('Ctrl Pts',(5.07023346343252,1.50455108706853,3.25424749218955));
#38287=CARTESIAN_POINT('Ctrl Pts',(3.73307055280206,3.74634830136122,3.33361938224296));
#38288=CARTESIAN_POINT('Ctrl Pts',(1.48653991852054,5.07554336184363,3.41299127229636));
#38289=CARTESIAN_POINT('Ctrl Pts',(-1.12210854951228,5.16834729390561,3.49236316234976));
#38290=CARTESIAN_POINT('Ctrl Pts',(-3.45741385862906,4.00215326511488,3.57173505240317));
#38291=CARTESIAN_POINT('Ctrl Pts',(-4.95050080463958,1.86104355955814,3.65110694245657));
#38292=CARTESIAN_POINT('Ctrl Pts',(-5.23765671238755,-0.733412237756895,
3.73047883250997));
#38293=CARTESIAN_POINT('Ctrl Pts',(-4.24893103835441,-3.14921043733482,
3.80985072256337));
#38294=CARTESIAN_POINT('Ctrl Pts',(-2.22517516822744,-4.79786794503704,
3.88922261261678));
#38295=CARTESIAN_POINT('Ctrl Pts',(0.340628447538026,-5.2777754412288,3.96859450267018));
#38296=CARTESIAN_POINT('Ctrl Pts',(2.82345572745151,-4.472028522095,4.04796639272359));
#38297=CARTESIAN_POINT('Ctrl Pts',(4.61849544177105,-2.57690535364612,4.12733828277699));
#38298=CARTESIAN_POINT('Ctrl Pts',(5.28847988934143,-0.0540537449322821,
4.2067101728304));
#38299=CARTESIAN_POINT('Ctrl Pts',(4.67020234171992,2.48196523640112,4.2860820628838));
#38300=CARTESIAN_POINT('Ctrl Pts',(2.91427384097298,4.41338297988409,4.36545395293721));
#38301=CARTESIAN_POINT('Ctrl Pts',(0.44843468320075,5.26971039832481,4.44482584299061));
#38302=CARTESIAN_POINT('Ctrl Pts',(-2.12664217080585,4.84234802803972,4.52419773304401));
#38303=CARTESIAN_POINT('Ctrl Pts',(-4.18367369924674,3.23540039647972,4.60356962309741));
#38304=CARTESIAN_POINT('Ctrl Pts',(-5.22157157495578,0.840316389774564,
4.68294151315082));
#38305=CARTESIAN_POINT('Ctrl Pts',(-4.98750617275825,-1.75946682947089,
4.76231340320422));
#38306=CARTESIAN_POINT('Ctrl Pts',(-3.53849530653447,-3.93064782357102,
4.84168529325762));
#38307=CARTESIAN_POINT('Ctrl Pts',(-1.22751481596538,-5.14433170819062,
4.92105718331103));
#38308=CARTESIAN_POINT('Ctrl Pts',(1.3824855667149,-5.10486777548008,5.00042907336443));
#38309=CARTESIAN_POINT('Ctrl Pts',(3.65571552542333,-3.82186935209575,5.07980096341784));
#38310=CARTESIAN_POINT('Ctrl Pts',(5.03842127392769,-1.60787201410522,5.15917285347124));
#38311=CARTESIAN_POINT('Ctrl Pts',(5.1937787524596,0.997799387556994,5.23854474352464));
#38312=CARTESIAN_POINT('Ctrl Pts',(4.08394322312664,3.36040906700182,5.31791663357805));
#38313=CARTESIAN_POINT('Ctrl Pts',(1.979268164295,4.90443053586431,5.39728852363145));
#38314=CARTESIAN_POINT('Ctrl Pts',(-0.607552238323124,5.25374358196311,
5.47666041368485));
#38315=CARTESIAN_POINT('Ctrl Pts',(-3.04637426047979,4.32325632045987,5.55603230373826));
#38316=CARTESIAN_POINT('Ctrl Pts',(-4.74310625581864,2.33963338865815,5.63540419379165));
#38317=CARTESIAN_POINT('Ctrl Pts',(-5.28442806592769,-0.213919057930008,
5.71477608384507));
#38318=CARTESIAN_POINT('Ctrl Pts',(-4.53847489605989,-2.71536129550824,
5.79414797389846));
#38319=CARTESIAN_POINT('Ctrl Pts',(-2.68695928725567,-4.55534753185094,
5.87351986395187));
#38320=CARTESIAN_POINT('Ctrl Pts',(-0.180906343559476,-5.28566119252549,
5.95289175400528));
#38321=CARTESIAN_POINT('Ctrl Pts',(2.36921498499841,-4.72839948631341,6.03226364405867));
#38322=CARTESIAN_POINT('Ctrl Pts',(4.3422007873791,-3.01931013137013,6.1116355341121));
#38323=CARTESIAN_POINT('Ctrl Pts',(5.25743608925265,-0.574723511554695,
6.19100742416548));
#38324=CARTESIAN_POINT('Ctrl Pts',(4.89197159692165,2.00986448354653,6.2703793142189));
#38325=CARTESIAN_POINT('Ctrl Pts',(3.33483365177601,4.10485393921541,6.34975120427228));
#38326=CARTESIAN_POINT('Ctrl Pts',(0.96533761058682,5.19991006123149,6.42912309432572));
#38327=CARTESIAN_POINT('Ctrl Pts',(-1.63931253580277,5.02827960213728,6.50849498437909));
#38328=CARTESIAN_POINT('Ctrl Pts',(-3.84462977702757,3.63177136187054,6.58786687443252));
#38329=CARTESIAN_POINT('Ctrl Pts',(-5.11340371451209,1.35057165664169,6.6672387644859));
#38330=CARTESIAN_POINT('Ctrl Pts',(-5.13656382546863,-1.25962431470543,
6.74661065453933));
#38331=CARTESIAN_POINT('Ctrl Pts',(-3.90846835813217,-3.56297859112141,
6.82598254459271));
#38332=CARTESIAN_POINT('Ctrl Pts',(-1.72827865000271,-4.99839916925957,
6.90535443464612));
#38333=CARTESIAN_POINT('Ctrl Pts',(0.872915911787522,-5.21622077353501,
6.98472632469953));
#38334=CARTESIAN_POINT('Ctrl Pts',(3.26147008963291,-4.16338254328616,7.06409821475292));
#38335=CARTESIAN_POINT('Ctrl Pts',(4.85553737278532,-2.09635354098373,7.14347010480633));
#38336=CARTESIAN_POINT('Ctrl Pts',(5.26680649947689,0.481342543702463,7.22284199485974));
#38337=CARTESIAN_POINT('Ctrl Pts',(4.39509322077433,2.9417846501764,7.30221388491313));
#38338=CARTESIAN_POINT('Ctrl Pts',(2.45274496186498,4.68561452739722,7.38158577496654));
#38339=CARTESIAN_POINT('Ctrl Pts',(-0.0870865406957981,5.28803907717593,
7.46095766501995));
#38340=CARTESIAN_POINT('Ctrl Pts',(-2.60570395470586,4.60230901263053,7.54032955507335));
#38341=CARTESIAN_POINT('Ctrl Pts',(-4.48957765297745,2.79546665964655,7.61970144512676));
#38342=CARTESIAN_POINT('Ctrl Pts',(-5.27980017249532,0.307654816033177,
7.69907333518014));
#38343=CARTESIAN_POINT('Ctrl Pts',(-4.78387505663278,-2.25510105978351,
7.77844522523357));
#38344=CARTESIAN_POINT('Ctrl Pts',(-3.12260856590233,-4.26851930901846,
7.85781711528695));
#38345=CARTESIAN_POINT('Ctrl Pts',(-0.70068154029489,-5.24213570278374,
7.93718900534038));
#38346=CARTESIAN_POINT('Ctrl Pts',(1.8919299575961,-4.93877944262147,8.01656089539376));
#38347=CARTESIAN_POINT('Ctrl Pts',(4.02367150553262,-3.43234744203947,8.09593278544719));
#38348=CARTESIAN_POINT('Ctrl Pts',(5.1752555809672,-1.08980320194883,8.17530467550057));
#38349=CARTESIAN_POINT('Ctrl Pts',(5.06615885211206,1.51821468589804,8.25467656555398));
#38350=CARTESIAN_POINT('Ctrl Pts',(3.72295704063487,3.75639883677136,8.33404845560738));
#38351=CARTESIAN_POINT('Ctrl Pts',(1.47285113468463,5.07953254565499,8.41342034566079));
#38352=CARTESIAN_POINT('Ctrl Pts',(-1.1360380475741,5.16530336977162,8.49279223571419));
#38353=CARTESIAN_POINT('Ctrl Pts',(-3.46819087602133,3.99281772621695,8.57216412576759));
#38354=CARTESIAN_POINT('Ctrl Pts',(-4.95550008378004,1.84769052250801,8.651536015821));
#38355=CARTESIAN_POINT('Ctrl Pts',(-5.23566043994335,-0.74753000269027,
8.7309079058744));
#38356=CARTESIAN_POINT('Ctrl Pts',(-4.24042550187429,-3.16065387386283,
8.81027979592781));
#38357=CARTESIAN_POINT('Ctrl Pts',(-2.21223229757129,-4.8038494573511,8.88965168598121));
#38358=CARTESIAN_POINT('Ctrl Pts',(0.354855797726969,-5.27683794616905,
8.96902357603462));
#38359=CARTESIAN_POINT('Ctrl Pts',(2.83550180615889,-4.46440039138287,9.04839546608801));
#38360=CARTESIAN_POINT('Ctrl Pts',(4.6254258508873,-2.56444478303851,9.12776735614143));
#38361=CARTESIAN_POINT('Ctrl Pts',(5.28860639654605,-0.0397961018481786,
9.20713924619482));
#38362=CARTESIAN_POINT('Ctrl Pts',(4.66349413013784,2.49454682166519,9.28651113624823));
#38363=CARTESIAN_POINT('Ctrl Pts',(2.90236501609723,4.42122366100663,9.36588302630163));
#38364=CARTESIAN_POINT('Ctrl Pts',(0.434226208411351,5.27090020273944,9.44525491635504));
#38365=CARTESIAN_POINT('Ctrl Pts',(-2.13968914250016,4.83659712202464,9.52462680640844));
#38366=CARTESIAN_POINT('Ctrl Pts',(-4.1923809544202,3.22410968801074,9.60399869646184));
#38367=CARTESIAN_POINT('Ctrl Pts',(-5.22381804552131,0.826236270443201,
9.68337058651526));
#38368=CARTESIAN_POINT('Ctrl Pts',(-4.98274462345855,-1.77290647376134,
9.76274247656865));
#38369=CARTESIAN_POINT('Ctrl Pts',(-3.52788564023945,-3.94017312521954,
9.84211436662205));
#38370=CARTESIAN_POINT('Ctrl Pts',(-1.21364152390043,-5.14762232479954,
9.92148625667546));
#38371=CARTESIAN_POINT('Ctrl Pts',(1.39624298131078,-5.10112212012714,10.0008581467289));
#38372=CARTESIAN_POINT('Ctrl Pts',(3.66600578680612,-3.81199985813406,10.0802300367823));
#38373=CARTESIAN_POINT('Ctrl Pts',(5.04273769720163,-1.5942828684181,10.1596019268357));
#38374=CARTESIAN_POINT('Ctrl Pts',(5.19106986646944,1.01179789915923,10.2389738168891));
#38375=CARTESIAN_POINT('Ctrl Pts',(4.07486890650351,3.37140693807807,10.3183457069425));
#38376=CARTESIAN_POINT('Ctrl Pts',(1.96603890048266,4.90974870936374,10.3977175969959));
#38377=CARTESIAN_POINT('Ctrl Pts',(-0.621713829942471,5.25208656259283,
10.4770894870493));
#38378=CARTESIAN_POINT('Ctrl Pts',(-3.05801844753381,4.31502775447074,10.5564613771027));
#38379=CARTESIAN_POINT('Ctrl Pts',(-4.74939654011498,2.32683773651149,10.6358332671561));
#38380=CARTESIAN_POINT('Ctrl Pts',(-5.28383214813503,-0.228164803694007,
10.7152051572095));
#38381=CARTESIAN_POINT('Ctrl Pts',(-4.53113794043347,-2.72758690275384,
10.7945770472629));
#38382=CARTESIAN_POINT('Ctrl Pts',(-2.67466855994604,-4.56257486971405,
10.8739489373163));
#38383=CARTESIAN_POINT('Ctrl Pts',(-0.166655838534166,-5.2861296975001,
10.9533208273697));
#38384=CARTESIAN_POINT('Ctrl Pts',(2.38195387625819,-4.72199503162473,11.0326927174231));
#38385=CARTESIAN_POINT('Ctrl Pts',(4.3503248991595,-3.00759282800428,11.1120646074765));
#38386=CARTESIAN_POINT('Ctrl Pts',(5.2589664059064,-0.560547668675828,11.1914364975299));
#38387=CARTESIAN_POINT('Ctrl Pts',(4.8865353366992,2.02304566199086,11.2708083875833));
#38388=CARTESIAN_POINT('Ctrl Pts',(3.32375507563458,4.11382954733217,11.3501802776367));
#38389=CARTESIAN_POINT('Ctrl Pts',(0.951315435152466,5.20249366075065,11.4295521676901));
#38390=CARTESIAN_POINT('Ctrl Pts',(-1.6528625396318,5.02384183393465,11.5089240577436));
#38391=CARTESIAN_POINT('Ctrl Pts',(-3.85440685831092,3.62139325645746,11.5882959477969));
#38392=CARTESIAN_POINT('Ctrl Pts',(-5.11702619789041,1.33678129752526,11.6676678378503));
#38393=CARTESIAN_POINT('Ctrl Pts',(-5.13314928200913,-1.27346762656892,
11.7470397279037));
#38394=CARTESIAN_POINT('Ctrl Pts',(-3.89884856306365,-3.57350265560368,
11.8264116179572));
#38395=CARTESIAN_POINT('Ctrl Pts',(-1.71479696411077,-5.00304034754732,
11.9057835080105));
#38396=CARTESIAN_POINT('Ctrl Pts',(0.886975379660772,-5.21384848487043,
11.985155398064));
#38397=CARTESIAN_POINT('Ctrl Pts',(3.27268248423369,-4.15457467193696,12.0645272881174));
#38398=CARTESIAN_POINT('Ctrl Pts',(4.86117137960707,-2.08325566491467,12.1438991781708));
#38399=CARTESIAN_POINT('Ctrl Pts',(5.26548968692849,0.495539810872594,12.2232710682242));
#38400=CARTESIAN_POINT('Ctrl Pts',(4.38714636147788,2.95362288559007,12.3026429582776));
#38401=CARTESIAN_POINT('Ctrl Pts',(2.44010389315499,4.69220996311119,12.382014848331));
#38402=CARTESIAN_POINT('Ctrl Pts',(-0.101342482462103,5.28778507964898,
12.4613867383844));
#38403=CARTESIAN_POINT('Ctrl Pts',(-2.61810205366918,4.59526745509803,12.5407586284378));
#38404=CARTESIAN_POINT('Ctrl Pts',(-4.49709775967304,2.78335284993721,12.6201305184912));
#38405=CARTESIAN_POINT('Ctrl Pts',(-5.28061040557763,0.293419651378745,
12.6995024085446));
#38406=CARTESIAN_POINT('Ctrl Pts',(-4.7777780451164,-2.26798992478223,12.778874298598));
#38407=CARTESIAN_POINT('Ctrl Pts',(-3.11108952829712,-4.27692217537683,
12.8582461886514));
#38408=CARTESIAN_POINT('Ctrl Pts',(-0.686546488664521,-5.24400565085626,
12.9376180787048));
#38409=CARTESIAN_POINT('Ctrl Pts',(1.90523775596186,-4.93366095719673,13.0169899687582));
#38410=CARTESIAN_POINT('Ctrl Pts',(4.03291030040817,-3.42148737483739,13.0963618588116));
#38411=CARTESIAN_POINT('Ctrl Pts',(5.17817482237061,-1.07584704130148,13.175733748865));
#38412=CARTESIAN_POINT('Ctrl Pts',(5.06204741929909,1.53186725014844,13.2551056389184));
#38413=CARTESIAN_POINT('Ctrl Pts',(3.71281646953824,3.76642207019282,13.3344775289718));
#38414=CARTESIAN_POINT('Ctrl Pts',(1.45915164597774,5.08348481077208,13.4138494190252));
#38415=CARTESIAN_POINT('Ctrl Pts',(-1.14995928876559,5.16222190355004,13.4932213090786));
#38416=CARTESIAN_POINT('Ctrl Pts',(-3.47894268615732,3.98345316700755,13.572593199132));
#38417=CARTESIAN_POINT('Ctrl Pts',(-4.96046334571011,1.83432405620607,13.6519650891854));
#38418=CARTESIAN_POINT('Ctrl Pts',(-5.23362611404733,-0.761642334479749,
13.7313369792388));
#38419=CARTESIAN_POINT('Ctrl Pts',(-4.23188914543755,-3.17207433835303,
13.8107088692922));
#38420=CARTESIAN_POINT('Ctrl Pts',(-2.19927334812693,-4.80979605467098,
13.8900807593456));
#38421=CARTESIAN_POINT('Ctrl Pts',(0.369080568778457,-5.27586209837409,
13.9694526493991));
#38422=CARTESIAN_POINT('Ctrl Pts',(2.84752727607539,-4.45673981283591,14.0488245394524));
#38423=CARTESIAN_POINT('Ctrl Pts',(4.63232264181505,-2.55196557371717,14.1281964295059));
#38424=CARTESIAN_POINT('Ctrl Pts',(5.28869446548083,-0.0255381695209159,
14.2075683195592));
#38425=CARTESIAN_POINT('Ctrl Pts',(4.65675202368211,2.50711027624288,14.2869402096127));
#38426=CARTESIAN_POINT('Ctrl Pts',(2.89043509646017,4.42903220810837,14.3663120996661));
#38427=CARTESIAN_POINT('Ctrl Pts',(0.420014577610126,5.27205169757513,14.4456839897195));
#38428=CARTESIAN_POINT('Ctrl Pts',(-2.15272056265924,4.83081106300113,14.5250558797729));
#38429=CARTESIAN_POINT('Ctrl Pts',(-4.201057738831,3.21279554629894,14.6044277698263));
#38430=CARTESIAN_POINT('Ctrl Pts',(-5.22602654870706,0.81215014592063,14.6837996598797));
#38431=CARTESIAN_POINT('Ctrl Pts',(-4.97794685893165,-1.78633323234006,
14.7631715499331));
#38432=CARTESIAN_POINT('Ctrl Pts',(-3.51725033281897,-3.94966978918425,
14.8425434399865));
#38433=CARTESIAN_POINT('Ctrl Pts',(-1.19975941093315,-5.15087552782897,
14.9219153300399));
#38434=CARTESIAN_POINT('Ctrl Pts',(1.40999024783357,-5.09733938916413,15.0012872200933));
#38435=CARTESIAN_POINT('Ctrl Pts',(3.67626940318851,-3.8021026580683,15.0806591101467));
#38436=CARTESIAN_POINT('Ctrl Pts',(5.04701746921103,-1.5806821352785,15.1600310002001));
#38437=CARTESIAN_POINT('Ctrl Pts',(5.18832325111744,1.02578905688456,15.2394028902535));
#38438=CARTESIAN_POINT('Ctrl Pts',(4.06576497321036,3.38238030533612,15.3187747803069));
#38439=CARTESIAN_POINT('Ctrl Pts',(1.95279534724736,4.91503119817963,15.3981466703603));
#38440=CARTESIAN_POINT('Ctrl Pts',(-0.635870902865948,5.2503913703836,15.4775185604137));
#38441=CARTESIAN_POINT('Ctrl Pts',(-3.06964040851742,4.30676782630626,15.5568904504671));
#38442=CARTESIAN_POINT('Ctrl Pts',(-4.75565230518791,2.31402517260967,15.6362623405205));
#38443=CARTESIAN_POINT('Ctrl Pts',(-5.28319782677237,-0.24240889112691,
15.7156342305739));
#38444=CARTESIAN_POINT('Ctrl Pts',(-4.52376805191524,-2.73979268554778,
15.7950061206273));
#38445=CARTESIAN_POINT('Ctrl Pts',(-2.66235839280204,-4.56976904619777,
15.8743780106807));
#38446=CARTESIAN_POINT('Ctrl Pts',(-0.15240412223312,-5.28655978220556,
15.9537499007341));
#38447=CARTESIAN_POINT('Ctrl Pts',(2.39467545517194,-4.71555625687092,16.0331217907875));
#38448=CARTESIAN_POINT('Ctrl Pts',(4.35841739221953,-2.99585366506689,16.112493680841));
#38449=CARTESIAN_POINT('Ctrl Pts',(5.26045849971912,-0.546367751666672,
16.1918655708943));
#38450=CARTESIAN_POINT('Ctrl Pts',(4.88106356050808,2.03621213668353,16.2712374609478));
#38451=CARTESIAN_POINT('Ctrl Pts',(3.31265234202039,4.12277525560071,16.3506093510011));
#38452=CARTESIAN_POINT('Ctrl Pts',(0.937286345425132,5.20503944789207,16.4299812410546));
#38453=CARTESIAN_POINT('Ctrl Pts',(-1.66640053022416,5.01936755177917,16.509353131108));
#38454=CARTESIAN_POINT('Ctrl Pts',(-3.86415592530783,3.6109888303424,16.5887250211614));
#38455=CARTESIAN_POINT('Ctrl Pts',(-5.12061148999576,1.32298122241861,16.6680969112148));
#38456=CARTESIAN_POINT('Ctrl Pts',(-5.1296974302943,-1.28730168253218,16.7474688012682));
#38457=CARTESIAN_POINT('Ctrl Pts',(-3.88920043041393,-3.58400074773889,
16.8268406913216));
#38458=CARTESIAN_POINT('Ctrl Pts',(-1.70130281532588,-5.00764516247516,
16.906212581375));
#38459=CARTESIAN_POINT('Ctrl Pts',(0.90102840177319,-5.21143830245825,16.9855844714284));
#38460=CARTESIAN_POINT('Ctrl Pts',(3.28387109087768,-4.1457366023928,17.0649563614818));
#38461=CARTESIAN_POINT('Ctrl Pts',(4.86677005798476,-2.07014265165526,17.1443282515352));
#38462=CARTESIAN_POINT('Ctrl Pts',(5.26413459813378,0.50973348428664,17.2237001415886));
#38463=CARTESIAN_POINT('Ctrl Pts',(4.37916762715237,2.96543963879408,17.303072031642));
#38464=CARTESIAN_POINT('Ctrl Pts',(2.42744506809458,4.69877132337447,17.3824439216954));
#38465=CARTESIAN_POINT('Ctrl Pts',(-0.115597647321682,5.28749259670007,
17.4618158117488));
#38466=CARTESIAN_POINT('Ctrl Pts',(-2.63048120009413,4.58819259887652,17.5411877018022));
#38467=CARTESIAN_POINT('Ctrl Pts',(-4.5045850370732,2.7712186210673,17.6205595918556));
#38468=CARTESIAN_POINT('Ctrl Pts',(-5.28138253005218,0.27918271172893,17.699931481909));
#38469=CARTESIAN_POINT('Ctrl Pts',(-4.77164579536179,-2.28086298099153,
17.7793033719624));
#38470=CARTESIAN_POINT('Ctrl Pts',(-3.09954884704088,-4.28529268150238,
17.8586752620158));
#38471=CARTESIAN_POINT('Ctrl Pts',(-0.672404619068171,-5.24583989230806,
17.9380471520692));
#38472=CARTESIAN_POINT('Ctrl Pts',(1.91852825506979,-4.9285020674696,18.0174190421226));
#38473=CARTESIAN_POINT('Ctrl Pts',(4.04212630117149,-3.41061102326166,18.096790932176));
#38474=CARTESIAN_POINT('Ctrl Pts',(5.18104412158612,-1.06186685398811,18.1761628222294));
#38475=CARTESIAN_POINT('Ctrl Pts',(5.05792243214194,1.54547807796858,18.2555347122829));
#38476=CARTESIAN_POINT('Ctrl Pts',(3.70260503654169,3.77647571272922,18.3349066023362));
#38477=CARTESIAN_POINT('Ctrl Pts',(1.44552439996779,5.08729102078633,18.4142784923897));
#38478=CARTESIAN_POINT('Ctrl Pts',(-1.16402860508455,5.15930893371508,18.4936503824431));
#38479=CARTESIAN_POINT('Ctrl Pts',(-3.48937383888192,3.97367066688439,18.5730222724965));
#38480=CARTESIAN_POINT('Ctrl Pts',(-4.96594823061187,1.82167865277138,18.6523941625499));
#38481=CARTESIAN_POINT('Ctrl Pts',(-5.23050112077116,-0.77713504302674,
18.7317660526033));
#38482=CARTESIAN_POINT('Ctrl Pts',(-4.22530652207786,-3.18086119603167,
18.8111379426567));
#38483=CARTESIAN_POINT('Ctrl Pts',(-2.18257651229225,-4.82058518621618,
18.8905098327101));
#38484=CARTESIAN_POINT('Ctrl Pts',(0.37648005341871,-5.26605971579227,18.9698817227635));
#38485=CARTESIAN_POINT('Ctrl Pts',(3.70230252414111,-4.19446206534953,19.0757109095013));
#38486=CARTESIAN_POINT('Ctrl Pts',(5.99600976813328,-0.0197068834824163,
19.2079973929237));
#38487=CARTESIAN_POINT('Ctrl Pts',(3.26379011618947,5.03400372054209,19.3667411730305));
#38488=CARTESIAN_POINT('Ctrl Pts',(-2.45559119020206,5.46873373673905,19.5254849531373));
#38489=CARTESIAN_POINT('Ctrl Pts',(-5.92771323046149,0.905806267444168,
19.6842287332441));
#38490=CARTESIAN_POINT('Ctrl Pts',(-3.97578039972873,-4.48936692070992,
19.8429725133509));
#38491=CARTESIAN_POINT('Ctrl Pts',(1.61419617037569,-5.77483540889728,20.0017162934577));
#38492=CARTESIAN_POINT('Ctrl Pts',(5.72720375155094,-1.77677009197941,20.1604600735645));
#38493=CARTESIAN_POINT('Ctrl Pts',(4.59927593805412,3.84720861430021,20.3192038536713));
#38494=CARTESIAN_POINT('Ctrl Pts',(-0.73672307947618,5.95134306184733,20.4779476337782));
#38495=CARTESIAN_POINT('Ctrl Pts',(-5.3995463563661,2.60828838171381,20.6366914138849));
#38496=CARTESIAN_POINT('Ctrl Pts',(-5.1196790448508,-3.11863163173554,20.7954351939918));
#38497=CARTESIAN_POINT('Ctrl Pts',(-0.158509478954971,-5.99736559883163,
20.9541789740985));
#38498=CARTESIAN_POINT('Ctrl Pts',(4.95432466322423,-3.37745298000941,21.1129227542054));
#38499=CARTESIAN_POINT('Ctrl Pts',(5.4262515554071,1.3624793779577,21.2452092376277));
#38500=CARTESIAN_POINT('Ctrl Pts',(3.29092685490723,4.12830747359771,21.3510384243656));
#38501=CARTESIAN_POINT('Ctrl Pts',(0.929079443196039,5.20946188754723,21.430410314419));
#38502=CARTESIAN_POINT('Ctrl Pts',(-1.68303999757346,5.01382783115869,21.5097822044724));
#38503=CARTESIAN_POINT('Ctrl Pts',(-3.8722246926078,3.60110493868854,21.5891540945258));
#38504=CARTESIAN_POINT('Ctrl Pts',(-5.12503498129818,1.30888173016128,21.6685259845792));
#38505=CARTESIAN_POINT('Ctrl Pts',(-5.12574462250326,-1.300972874894,21.7478978746326));
#38506=CARTESIAN_POINT('Ctrl Pts',(-3.87976959979778,-3.59455409188016,
21.827269764686));
#38507=CARTESIAN_POINT('Ctrl Pts',(-1.68766624540451,-5.01217052435348,
21.9066416547394));
#38508=CARTESIAN_POINT('Ctrl Pts',(0.915005995631755,-5.2090130440819,21.9860135447928));
#38509=CARTESIAN_POINT('Ctrl Pts',(3.29507231119182,-4.13685632854986,22.0653854348462));
#38510=CARTESIAN_POINT('Ctrl Pts',(4.87231403886192,-2.05702097999265,22.1447573248996));
#38511=CARTESIAN_POINT('Ctrl Pts',(5.26275149225388,0.523926824466718,22.2241292149531));
#38512=CARTESIAN_POINT('Ctrl Pts',(4.37115162329097,2.97723307464397,22.3035011050064));
#38513=CARTESIAN_POINT('Ctrl Pts',(2.4147715124657,4.70529942618521,22.3828729950599));
#38514=CARTESIAN_POINT('Ctrl Pts',(-0.129853572474074,5.28716128664959,
22.4622448851132));
#38515=CARTESIAN_POINT('Ctrl Pts',(-2.64284027062663,4.58108446095525,22.5416167751666));
#38516=CARTESIAN_POINT('Ctrl Pts',(-4.51204028846786,2.7590644882843,22.62098866522));
#38517=CARTESIAN_POINT('Ctrl Pts',(-5.28211549991429,0.264943102456049,
22.7003605552734));
#38518=CARTESIAN_POINT('Ctrl Pts',(-4.76548000969985,-2.2937181486802,22.7797324453269));
#38519=CARTESIAN_POINT('Ctrl Pts',(-3.08798363825926,-4.29363457062517,
22.8591043353802));
#38520=CARTESIAN_POINT('Ctrl Pts',(-0.658261551986295,-5.24763120247219,
22.9384762254337));
#38521=CARTESIAN_POINT('Ctrl Pts',(1.93181173129385,-4.92331644248731,23.017848115487));
#38522=CARTESIAN_POINT('Ctrl Pts',(4.05129987868926,-3.39969271923279,23.0972200055405));
#38523=CARTESIAN_POINT('Ctrl Pts',(5.18390038229797,-1.0479113616667,23.1765918955939));
#38524=CARTESIAN_POINT('Ctrl Pts',(5.05371420635457,1.55913887720483,23.2559637856473));
#38525=CARTESIAN_POINT('Ctrl Pts',(3.69245444696201,3.78638634033052,23.3353356757007));
#38526=CARTESIAN_POINT('Ctrl Pts',(1.43172095156667,5.09127847004479,23.4147075657541));
#38527=CARTESIAN_POINT('Ctrl Pts',(-1.17777659548102,5.1559464348325,23.4940794558075));
#38528=CARTESIAN_POINT('Ctrl Pts',(-3.50037037246962,3.96463726004727,23.5734513458609));
#38529=CARTESIAN_POINT('Ctrl Pts',(-4.97028167379665,1.80755122457705,23.6528232359143));
#38530=CARTESIAN_POINT('Ctrl Pts',(-5.22944336137752,-0.789850288405212,
23.7321951259677));
#38531=CARTESIAN_POINT('Ctrl Pts',(-4.21472422106041,-3.19484601935549,
23.8115670160211));
#38532=CARTESIAN_POINT('Ctrl Pts',(-2.17330758975551,-4.82158433170509,
23.8909389060745));
#38533=CARTESIAN_POINT('Ctrl Pts',(0.397521959947206,-5.27379537322471,
23.9703107961279));
#38534=CARTESIAN_POINT('Ctrl Pts',(2.87151604007067,-4.4413215351868,24.0496826861813));
#38535=CARTESIAN_POINT('Ctrl Pts',(4.64601516884499,-2.5269516018695,24.1290545762347));
#38536=CARTESIAN_POINT('Ctrl Pts',(5.28875528625864,0.00297814834736192,
24.2084264662881));
#38537=CARTESIAN_POINT('Ctrl Pts',(4.64316632240633,2.53218242822061,24.2877983563415));
#38538=CARTESIAN_POINT('Ctrl Pts',(2.86651231988729,4.4445526734691,24.3671702463949));
#38539=CARTESIAN_POINT('Ctrl Pts',(0.391582261162602,5.27423972531146,24.4465421364484));
#38540=CARTESIAN_POINT('Ctrl Pts',(-2.1787363696294,4.81913365439931,24.5259140265017));
#38541=CARTESIAN_POINT('Ctrl Pts',(-4.21831964333045,3.19009729224708,24.6052859165552));
#38542=CARTESIAN_POINT('Ctrl Pts',(-5.23032958900859,0.783960290863936,
24.6846578066085));
#38543=CARTESIAN_POINT('Ctrl Pts',(-4.9682428239423,-1.81314770210696,24.764029696662));
#38544=CARTESIAN_POINT('Ctrl Pts',(-3.49590310398264,-3.96857692817898,
24.8434015867153));
#38545=CARTESIAN_POINT('Ctrl Pts',(-1.17196912594307,-5.15726959884261,
24.9227734767688));
#38546=CARTESIAN_POINT('Ctrl Pts',(1.43745393706658,-5.08966281065081,25.0021453668222));
#38547=CARTESIAN_POINT('Ctrl Pts',(3.69671640275713,-3.78222542756197,25.0815172568756));
#38548=CARTESIAN_POINT('Ctrl Pts',(5.05546693527898,-1.55344630213307,25.160889146929));
#38549=CARTESIAN_POINT('Ctrl Pts',(5.18271691245315,1.05374890400037,25.2402610369824));
#38550=CARTESIAN_POINT('Ctrl Pts',(4.04746852150308,3.40425320955296,25.3196329270358));
#38551=CARTESIAN_POINT('Ctrl Pts',(1.92626575763449,4.92548896844514,25.3990048170892));
#38552=CARTESIAN_POINT('Ctrl Pts',(-0.664171081076968,5.24688651700902,
25.4783767071426));
#38553=CARTESIAN_POINT('Ctrl Pts',(-3.09281731455583,4.2901541238158,25.5577485971959));
#38554=CARTESIAN_POINT('Ctrl Pts',(-4.76806009604388,2.2883496821561,25.6371204872494));
#38555=CARTESIAN_POINT('Ctrl Pts',(-5.28181399205765,-0.2708916769007,25.7164923773028));
#38556=CARTESIAN_POINT('Ctrl Pts',(-4.50892969070311,-2.76414442307307,
25.7958642673562));
#38557=CARTESIAN_POINT('Ctrl Pts',(-2.63768009703987,-4.58405770611471,
25.8752361574096));
#38558=CARTESIAN_POINT('Ctrl Pts',(-0.123897470143628,-5.28730467858643,
25.9546080474629));
#38559=CARTESIAN_POINT('Ctrl Pts',(2.42006630623721,-4.70257593460492,26.0339799375165));
#38560=CARTESIAN_POINT('Ctrl Pts',(4.37450728714461,-2.97231010192892,26.1133518275698));
#38561=CARTESIAN_POINT('Ctrl Pts',(5.26332797571122,-0.517996107519831,
26.1927237176232));
#38562=CARTESIAN_POINT('Ctrl Pts',(4.8700136195734,2.06250059211614,26.2720956076766));
#38563=CARTESIAN_POINT('Ctrl Pts',(3.29037472529985,4.14057671278022,26.35146749773));
#38564=CARTESIAN_POINT('Ctrl Pts',(0.909207831064193,5.21001751122215,26.4308393877834));
#38565=CARTESIAN_POINT('Ctrl Pts',(-1.69344007832135,5.01030957610855,26.5102112778369));
#38566=CARTESIAN_POINT('Ctrl Pts',(-3.88356973299385,3.59010131838702,26.5895831678902));
#38567=CARTESIAN_POINT('Ctrl Pts',(-5.12767039684481,1.29535232606086,26.6689550579437));
#38568=CARTESIAN_POINT('Ctrl Pts',(-5.12268190193029,-1.31494162567991,
26.748326947997));
#38569=CARTESIAN_POINT('Ctrl Pts',(-3.86981943456965,-3.604918707979,26.8276988380504));
#38570=CARTESIAN_POINT('Ctrl Pts',(-1.67427751864785,-5.01674557236666,
26.9070707281038));
#38571=CARTESIAN_POINT('Ctrl Pts',(0.929114694866165,-5.20650431970375,
26.9864426181573));
#38572=CARTESIAN_POINT('Ctrl Pts',(3.30617662527125,-4.12797013916282,27.0658145082107));
#38573=CARTESIAN_POINT('Ctrl Pts',(4.8778612478581,-2.04387156982875,27.145186398264));
#38574=CARTESIAN_POINT('Ctrl Pts',(5.26130966742943,0.538109589882639,27.2245582883175));
#38575=CARTESIAN_POINT('Ctrl Pts',(4.36311469772634,2.98900844458398,27.3039301783709));
#38576=CARTESIAN_POINT('Ctrl Pts',(2.40207464524773,4.7117914582426,27.3833020684242));
#38577=CARTESIAN_POINT('Ctrl Pts',(-0.144105473911181,5.28679250204684,
27.4626739584777));
#38578=CARTESIAN_POINT('Ctrl Pts',(-2.65518181859737,4.57394259446923,27.542045848531));
#38579=CARTESIAN_POINT('Ctrl Pts',(-4.51946174941854,2.74689039512913,27.6214177385845));
#38580=CARTESIAN_POINT('Ctrl Pts',(-5.28281080174027,0.25070177567431,27.7007896286378));
#38581=CARTESIAN_POINT('Ctrl Pts',(-4.75927883606144,-2.30655724141581,
27.7801615186913));
#38582=CARTESIAN_POINT('Ctrl Pts',(-3.07639708040302,-4.30194401997489,
27.8595334087447));
#38583=CARTESIAN_POINT('Ctrl Pts',(-0.644111805447875,-5.24938675745965,
27.9389052987981));
#38584=CARTESIAN_POINT('Ctrl Pts',(1.94507767959709,-4.91809050014772,28.0182771888515));
#38585=CARTESIAN_POINT('Ctrl Pts',(4.06045054724861,-3.38875828300845,28.0976490789049));
#38586=CARTESIAN_POINT('Ctrl Pts',(5.18670664924518,-1.03393204901761,28.1770209689583));
#38587=CARTESIAN_POINT('Ctrl Pts',(5.0494924920661,1.57275774354414,28.2563928590118));
#38588=CARTESIAN_POINT('Ctrl Pts',(3.68223314068176,3.79632723101881,28.3357647490651));
#38589=CARTESIAN_POINT('Ctrl Pts',(1.41798994671214,5.09511980804509,28.4151366391186));
#38590=CARTESIAN_POINT('Ctrl Pts',(-1.19167245960906,5.15275247768794,28.4945085291719));
#38591=CARTESIAN_POINT('Ctrl Pts',(-3.51104609249168,3.9551860491902,28.5738804192253));
#38592=CARTESIAN_POINT('Ctrl Pts',(-4.97513666881207,1.79414505376557,28.6532523092787));
#38593=CARTESIAN_POINT('Ctrl Pts',(-5.22729496488809,-0.803945705483672,
28.7326241993322));
#38594=CARTESIAN_POINT('Ctrl Pts',(-4.2060957779385,-3.20619707038074,28.8119960893855));
#38595=CARTESIAN_POINT('Ctrl Pts',(-2.16030096951815,-4.82742592572986,
28.891367979439));
#38596=CARTESIAN_POINT('Ctrl Pts',(0.41173837333167,-5.27270451089724,28.9707398694923));
#38597=CARTESIAN_POINT('Ctrl Pts',(2.88347915980534,-4.43356394814356,29.0501117595458));
#38598=CARTESIAN_POINT('Ctrl Pts',(4.65281080542333,-2.51441702114943,29.1294836495991));
#38599=CARTESIAN_POINT('Ctrl Pts',(5.28872803766221,0.0172363266290461,
29.2088555396526));
#38600=CARTESIAN_POINT('Ctrl Pts',(4.6363228263275,2.54469094339263,29.2882274297059));
#38601=CARTESIAN_POINT('Ctrl Pts',(2.85451963682592,4.45226447892365,29.3675993197594));
#38602=CARTESIAN_POINT('Ctrl Pts',(0.377361782165573,5.2752762423091,29.4469712098127));
#38603=CARTESIAN_POINT('Ctrl Pts',(-2.19172056735417,4.81324238969394,29.5263430998662));
#38604=CARTESIAN_POINT('Ctrl Pts',(-4.22690463795758,3.17871334488069,29.6057149899195));
#38605=CARTESIAN_POINT('Ctrl Pts',(-5.23242409484928,0.769856765217166,
29.6850868799731));
#38606=CARTESIAN_POINT('Ctrl Pts',(-4.96333662400999,-1.82653521840426,
29.7644587700263));
#38607=CARTESIAN_POINT('Ctrl Pts',(-3.48519133772112,-3.97798726578954,
29.8438306600798));
#38608=CARTESIAN_POINT('Ctrl Pts',(-1.15806115590354,-5.16041042035391,
29.9232025501331));
#38609=CARTESIAN_POINT('Ctrl Pts',(1.45117016016719,-5.08576901889481,30.0025744401866));
#38610=CARTESIAN_POINT('Ctrl Pts',(3.70689963733188,-3.77224554159173,30.08194633024));
#38611=CARTESIAN_POINT('Ctrl Pts',(5.05963656792573,-1.53981140008078,30.1613182202934));
#38612=CARTESIAN_POINT('Ctrl Pts',(5.17985722988845,1.06771739017516,30.2406901103468));
#38613=CARTESIAN_POINT('Ctrl Pts',(4.0382761360698,3.41515258753676,30.3200620004003));
#38614=CARTESIAN_POINT('Ctrl Pts',(1.91297991407722,4.93066417388641,30.3994338904535));
#38615=CARTESIAN_POINT('Ctrl Pts',(-0.678313980675348,5.24507688131741,
30.4788057805071));
#38616=CARTESIAN_POINT('Ctrl Pts',(-3.10437209115798,4.28180047024023,30.5581776705604));
#38617=CARTESIAN_POINT('Ctrl Pts',(-4.77421203164559,2.2754869422171,30.6375495606138));
#38618=CARTESIAN_POINT('Ctrl Pts',(-5.28106448876339,-0.285130168225216,
30.7169214506672));
#38619=CARTESIAN_POINT('Ctrl Pts',(-4.50146132585641,-2.77629020081278,
30.7962933407206));
#38620=CARTESIAN_POINT('Ctrl Pts',(-2.62531214778642,-4.59115208569648,
30.8756652307741));
#38621=CARTESIAN_POINT('Ctrl Pts',(-0.109642741545517,-5.28761948484725,
30.9550371208274));
#38622=CARTESIAN_POINT('Ctrl Pts',(2.43273539384572,-4.69603448143646,31.0344090108809));
#38623=CARTESIAN_POINT('Ctrl Pts',(4.38250457206463,-2.96050587284378,31.1137809009342));
#38624=CARTESIAN_POINT('Ctrl Pts',(5.26470533703794,-0.503804586594991,
31.1931527909877));
#38625=CARTESIAN_POINT('Ctrl Pts',(4.86443553513645,2.07562238179582,31.272524681041));
#38626=CARTESIAN_POINT('Ctrl Pts',(3.27920000412114,4.14943233229341,31.3518965710945));
#38627=CARTESIAN_POINT('Ctrl Pts',(0.895158610487983,5.21244975125701,31.4312684611478));
#38628=CARTESIAN_POINT('Ctrl Pts',(-1.70694143926006,5.00572594837619,31.5106403512013));
#38629=CARTESIAN_POINT('Ctrl Pts',(-3.89323433265515,3.57961838445739,31.5900122412546));
#38630=CARTESIAN_POINT('Ctrl Pts',(-5.13114396014345,1.28152370543563,31.6693841313081));
#38631=CARTESIAN_POINT('Ctrl Pts',(-5.11911827653528,-1.32874731162563,
31.7487560213615));
#38632=CARTESIAN_POINT('Ctrl Pts',(-3.86008671173927,-3.61533842470713,
31.8281279114149));
#38633=CARTESIAN_POINT('Ctrl Pts',(-1.6607465681206,-5.02124109994587,31.9074998014683));
#38634=CARTESIAN_POINT('Ctrl Pts',(0.943147763492109,-5.20398055756647,
31.9868716915216));
#38635=CARTESIAN_POINT('Ctrl Pts',(3.31729338754031,-4.11904187017945,32.0662435815751));
#38636=CARTESIAN_POINT('Ctrl Pts',(4.88335368508803,-2.03071370056122,32.1456154716285));
#38637=CARTESIAN_POINT('Ctrl Pts',(5.25983983406835,0.552291831605133,32.2249873616819));
#38638=CARTESIAN_POINT('Ctrl Pts',(4.35504064192764,3.00076029606972,32.3043592517354));
#38639=CARTESIAN_POINT('Ctrl Pts',(2.3893631891323,4.71825019448202,32.3837311417886));
#38640=CARTESIAN_POINT('Ctrl Pts',(-0.158357847769981,5.28638478918814,
32.4631030318421));
#38641=CARTESIAN_POINT('Ctrl Pts',(-2.66750326347463,4.56676775046226,32.5424749218955));
#38642=CARTESIAN_POINT('Ctrl Pts',(-4.52685078861515,2.73469619609277,32.6218468119489));
#38643=CARTESIAN_POINT('Ctrl Pts',(-5.28346748166331,0.23645870150246,32.7012187020024));
#38644=CARTESIAN_POINT('Ctrl Pts',(-4.75304319093522,-2.31937960938145,
32.7805905920557));
#38645=CARTESIAN_POINT('Ctrl Pts',(-3.06478809957792,-4.3102221812797,32.8599624821091));
#38646=CARTESIAN_POINT('Ctrl Pts',(-0.629957410956834,-5.25110417033318,
32.9393343721625));
#38647=CARTESIAN_POINT('Ctrl Pts',(1.95832950858626,-4.91282880661543,33.0187062622159));
#38648=CARTESIAN_POINT('Ctrl Pts',(4.06957169452659,-3.37779921996823,33.0980781522693));
#38649=CARTESIAN_POINT('Ctrl Pts',(5.18947522352436,-1.01994521996853,33.1774500423228));
#38650=CARTESIAN_POINT('Ctrl Pts',(5.04523407478018,1.586365178005,33.2568219323761));
#38651=CARTESIAN_POINT('Ctrl Pts',(3.67198507285579,3.80624052997629,33.3361938224296));
#38652=CARTESIAN_POINT('Ctrl Pts',(1.40424863498483,5.09892411381589,33.4155657124829));
#38653=CARTESIAN_POINT('Ctrl Pts',(-1.20555966211678,5.14952106980705,33.4949376025364));
#38654=CARTESIAN_POINT('Ctrl Pts',(-3.52169629398785,3.94570609146478,33.5743094925897));
#38655=CARTESIAN_POINT('Ctrl Pts',(-4.979955503786,1.78072584291395,33.6536813826432));
#38656=CARTESIAN_POINT('Ctrl Pts',(-5.22510857580638,-0.818035279400921,
33.7330532726965));
#38657=CARTESIAN_POINT('Ctrl Pts',(-4.19743676434199,-3.2175248183441,33.81242516275));
#38658=CARTESIAN_POINT('Ctrl Pts',(-2.14727864795256,-4.83323243340904,
33.8917970528034));
#38659=CARTESIAN_POINT('Ctrl Pts',(0.425951794157462,-5.27157532587404,
33.9711689428568));
#38660=CARTESIAN_POINT('Ctrl Pts',(2.89542132203897,-4.4257741373902,34.0505408329101));
#38661=CARTESIAN_POINT('Ctrl Pts',(4.6595726247782,-2.50186416532303,34.1299127229636));
#38662=CARTESIAN_POINT('Ctrl Pts',(5.28866234991056,0.0314943796344648,
34.209284613017));
#38663=CARTESIAN_POINT('Ctrl Pts',(4.62944563286023,2.55718096342464,34.2886565030704));
#38664=CARTESIAN_POINT('Ctrl Pts',(2.84250620674923,4.45994392474861,34.3680283931238));
#38665=CARTESIAN_POINT('Ctrl Pts',(0.363138560454883,5.27627441792225,34.4474002831772));
#38666=CARTESIAN_POINT('Ctrl Pts',(-2.20468883537271,4.80731614172534,34.5267721732306));
#38667=CARTESIAN_POINT('Ctrl Pts',(-4.23545891089946,3.1673062942179,34.606144063284));
#38668=CARTESIAN_POINT('Ctrl Pts',(-5.23448057076036,0.755747644152594,
34.6855159533374));
#38669=CARTESIAN_POINT('Ctrl Pts',(-4.95839434991029,-1.83990945920924,
34.7648878433908));
#38670=CARTESIAN_POINT('Ctrl Pts',(-3.47445424064183,-3.98736869087822,
34.8442597334442));
#38671=CARTESIAN_POINT('Ctrl Pts',(-1.14414476892706,-5.16351373534018,
34.9236316234976));
#38672=CARTESIAN_POINT('Ctrl Pts',(1.4648758359769,-5.0818382631171,35.003003513551));
#38673=CARTESIAN_POINT('Ctrl Pts',(3.71705592968454,-3.76223823845686,35.0823754036044));
#38674=CARTESIAN_POINT('Ctrl Pts',(5.06376942648477,-1.52616530648161,35.1617472936578));
#38675=CARTESIAN_POINT('Ctrl Pts',(5.1769598994568,1.08167811604296,35.2411191837112));
#38676=CARTESIAN_POINT('Ctrl Pts',(4.02905439992751,3.42602714375337,35.3204910737646));
#38677=CARTESIAN_POINT('Ctrl Pts',(1.8996801667365,4.93580354262787,35.3998629638181));
#38678=CARTESIAN_POINT('Ctrl Pts',(-0.69245195020073,5.24322912373406,35.4792348538714));
#38679=CARTESIAN_POINT('Ctrl Pts',(-3.11590430478548,4.27341569598948,35.5586067439249));
#38680=CARTESIAN_POINT('Ctrl Pts',(-4.78032926766171,2.26260766374704,35.6379786339782));
#38681=CARTESIAN_POINT('Ctrl Pts',(-5.28027660201491,-0.299366587187078,
35.7173505240316));
#38682=CARTESIAN_POINT('Ctrl Pts',(-4.49396024381123,-2.78841580011912,
35.7967224140851));
#38683=CARTESIAN_POINT('Ctrl Pts',(-2.61292511742748,-4.59821309619579,
35.8760943041384));
#38684=CARTESIAN_POINT('Ctrl Pts',(-0.0953872160500441,-5.28789586001125,
35.9554661941919));
#38685=CARTESIAN_POINT('Ctrl Pts',(2.4453868000212,-4.68945889688694,36.0348380842453));
#38686=CARTESIAN_POINT('Ctrl Pts',(4.39047000437915,-2.94868012642215,36.1142099742987));
#38687=CARTESIAN_POINT('Ctrl Pts',(5.26604443381084,-0.489609403953667,
36.1935818643521));
#38688=CARTESIAN_POINT('Ctrl Pts',(4.85882209535785,2.08872908558584,36.2729537544055));
#38689=CARTESIAN_POINT('Ctrl Pts',(3.26800144929601,4.15825779320007,36.3523256444589));
#38690=CARTESIAN_POINT('Ctrl Pts',(0.881102883784141,5.2148441065383,36.4316975345123));
#38691=CARTESIAN_POINT('Ctrl Pts',(-1.72043039392939,5.00110593838543,36.5110694245656));
#38692=CARTESIAN_POINT('Ctrl Pts',(-3.90287063578981,3.56910943340206,36.5904413146191));
#38693=CARTESIAN_POINT('Ctrl Pts',(-5.13458022962944,1.26768577053169,36.6698132046725));
#38694=CARTESIAN_POINT('Ctrl Pts',(-5.11551744473188,-1.34254334006536,
36.7491850947259));
#38695=CARTESIAN_POINT('Ctrl Pts',(-3.85032593330342,-3.62573186469175,
36.8285569847793));
#38696=CARTESIAN_POINT('Ctrl Pts',(-1.64720354707418,-5.02570013250056,
36.9079288748327));
#38697=CARTESIAN_POINT('Ctrl Pts',(0.957173977199105,-5.20141897223083,
36.9873007648861));
#38698=CARTESIAN_POINT('Ctrl Pts',(3.32838603929536,-4.11008366347129,37.0666726549395));
#38699=CARTESIAN_POINT('Ctrl Pts',(4.88881062947681,-2.01754107180608,37.1460445449929));
#38700=CARTESIAN_POINT('Ctrl Pts',(5.25833177151655,0.566470059199757,37.2254164350463));
#38701=CARTESIAN_POINT('Ctrl Pts',(4.34693493313475,3.01249033764469,37.3047883250998));
#38702=CARTESIAN_POINT('Ctrl Pts',(2.37663436681862,4.72467463787371,37.3841602151531));
#38703=CARTESIAN_POINT('Ctrl Pts',(-0.17260907066365,5.28593865420645,37.4635321052065));
#38704=CARTESIAN_POINT('Ctrl Pts',(-2.67980532059584,4.55955971460153,37.54290399526));
#38705=CARTESIAN_POINT('Ctrl Pts',(-4.53420692607955,2.72248212093334,37.6222758853133));
#38706=CARTESIAN_POINT('Ctrl Pts',(-5.28408576066665,0.222213908718847,
37.7016477753668));
#38707=CARTESIAN_POINT('Ctrl Pts',(-4.74677300008161,-2.33218511979937,
37.7810196654201));
#38708=CARTESIAN_POINT('Ctrl Pts',(-3.05315684347904,-4.31846901533503,
37.8603915554736));
#38709=CARTESIAN_POINT('Ctrl Pts',(-0.615798437855754,-5.25278341751105,
37.9397634455269));
#38710=CARTESIAN_POINT('Ctrl Pts',(1.97156710418767,-4.90753140600709,38.0191353355804));
#38711=CARTESIAN_POINT('Ctrl Pts',(4.07866326363087,-3.36681560666115,38.0985072256337));
#38712=CARTESIAN_POINT('Ctrl Pts',(5.19220608004019,-1.00595097780572,38.1778791156872));
#38713=CARTESIAN_POINT('Ctrl Pts',(5.04093898806991,1.59996108252017,38.2572510057405));
#38714=CARTESIAN_POINT('Ctrl Pts',(3.66171031660113,3.81612616476472,38.336622895794));
#38715=CARTESIAN_POINT('Ctrl Pts',(1.39049711694169,5.10269135980963,38.4159947858473));
#38716=CARTESIAN_POINT('Ctrl Pts',(-1.21943810235573,5.14625223481529,38.4953666759008));
#38717=CARTESIAN_POINT('Ctrl Pts',(-3.53232089954511,3.93619745533324,38.5747385659542));
#38718=CARTESIAN_POINT('Ctrl Pts',(-4.98473814342406,1.76729369047725,38.6541104560076));
#38719=CARTESIAN_POINT('Ctrl Pts',(-5.22288421068334,-0.832118909543577,
38.733482346061));
#38720=CARTESIAN_POINT('Ctrl Pts',(-4.18874724188046,-3.22882917750522,
38.8128542361144));
#38721=CARTESIAN_POINT('Ctrl Pts',(-2.13424072225093,-4.83900381899058,
38.8922261261678));
#38722=CARTESIAN_POINT('Ctrl Pts',(0.440162123945958,-5.27040781417516,
38.9715980162212));
#38723=CARTESIAN_POINT('Ctrl Pts',(2.90734243084964,-4.41795218255951,39.0509699062746));
#38724=CARTESIAN_POINT('Ctrl Pts',(4.66630059499982,-2.48929308216594,39.130341796328));
#38725=CARTESIAN_POINT('Ctrl Pts',(5.288558190933,0.0457521216721363,39.2097136863814));
#38726=CARTESIAN_POINT('Ctrl Pts',(4.62253485344793,2.56965255248844,39.2890855764349));
#38727=CARTESIAN_POINT('Ctrl Pts',(2.83047200092405,4.46759066254981,39.3684574664882));
#38728=CARTESIAN_POINT('Ctrl Pts',(0.34891291852996,5.27723479734496,39.4478293565417));
#38729=CARTESIAN_POINT('Ctrl Pts',(-2.21764149317963,4.80135391043001,39.527201246595));
#38730=CARTESIAN_POINT('Ctrl Pts',(-4.24398161873814,3.15587819282133,39.6065731366485));
#38731=CARTESIAN_POINT('Ctrl Pts',(-5.23650047694821,0.74162931109825,39.6859450267018));
#38732=CARTESIAN_POINT('Ctrl Pts',(-4.9534132521342,-1.85326330477585,39.7653169167553));
#38733=CARTESIAN_POINT('Ctrl Pts',(-3.46369715057683,-3.99673439595749,
39.8446888068086));
#38734=CARTESIAN_POINT('Ctrl Pts',(-1.13021013185916,-5.16655447652188,
39.9240606968621));
#38735=CARTESIAN_POINT('Ctrl Pts',(1.47855208450035,-5.0779179090888,40.0034325869154));
#38736=CARTESIAN_POINT('Ctrl Pts',(3.72722085031374,-3.75211381890458,40.0828044769689));
#38737=CARTESIAN_POINT('Ctrl Pts',(5.06779668194711,-1.51268081279862,40.1621763670222));
#38738=CARTESIAN_POINT('Ctrl Pts',(5.17416686787614,1.09598291074358,40.2415482570757));
#38739=CARTESIAN_POINT('Ctrl Pts',(4.40436067122798,2.65600709442752,40.2944628504446));
#38740=CARTESIAN_POINT('Ctrl Pts',(3.85627053850219,3.29705846079199,40.3209201471291));
#38741=CARTESIAN_POINT('Ctrl Pts',(1.26508527942741,-4.72177922709091,-0.106973382376351));
#38742=CARTESIAN_POINT('Ctrl Pts',(2.05001543279104,-4.51147638686031,-0.0805160856918833));
#38743=CARTESIAN_POINT('Ctrl Pts',(3.5121928105948,-3.69213734276823,-0.0276014923229477));
#38744=CARTESIAN_POINT('Ctrl Pts',(4.85026808817394,-1.56206090154413,0.0517703977304561));
#38745=CARTESIAN_POINT('Ctrl Pts',(5.00665954563268,0.947775616877177,0.13114228778386));
#38746=CARTESIAN_POINT('Ctrl Pts',(3.94352649879584,3.22711800485082,0.210514177837264));
#38747=CARTESIAN_POINT('Ctrl Pts',(1.91971357759781,4.72014150668349,0.289886067890667));
#38748=CARTESIAN_POINT('Ctrl Pts',(-0.571713243107534,5.06345468357225,
0.369257957944071));
#38749=CARTESIAN_POINT('Ctrl Pts',(-2.92388473013463,4.17326556172555,0.448629847997474));
#38750=CARTESIAN_POINT('Ctrl Pts',(-4.56379761866667,2.26650781142313,0.528001738050878));
#38751=CARTESIAN_POINT('Ctrl Pts',(-5.091983083909,-0.192381913949067,0.607373628104282));
#38752=CARTESIAN_POINT('Ctrl Pts',(-4.37977084759389,-2.6043995219968,0.686745518157685));
#38753=CARTESIAN_POINT('Ctrl Pts',(-2.60065712992448,-4.3819955716546,0.766117408211089));
#38754=CARTESIAN_POINT('Ctrl Pts',(-0.188028560849166,-5.09214486895681,
0.845489298264494));
#38755=CARTESIAN_POINT('Ctrl Pts',(2.27040306822816,-4.56186018168567,0.924861188317896));
#38756=CARTESIAN_POINT('Ctrl Pts',(4.17576968427582,-2.92031579800744,1.0042330783713));
#38757=CARTESIAN_POINT('Ctrl Pts',(5.06392796926476,-0.567389296122094,
1.0836049684247));
#38758=CARTESIAN_POINT('Ctrl Pts',(4.71852465152963,1.92375216574099,1.16297685847811));
#38759=CARTESIAN_POINT('Ctrl Pts',(3.22369915083516,3.94627176108661,1.24234874853151));
#38760=CARTESIAN_POINT('Ctrl Pts',(0.943587684251177,5.00748834177841,1.32172063858492));
#38761=CARTESIAN_POINT('Ctrl Pts',(-1.5663796598258,4.84889181906687,1.40109252863832));
#38762=CARTESIAN_POINT('Ctrl Pts',(-3.69478038260539,3.50911599649364,1.48046441869172));
#38763=CARTESIAN_POINT('Ctrl Pts',(-4.92314078418047,1.3145272768326,1.55983630874512));
#38764=CARTESIAN_POINT('Ctrl Pts',(-4.9522349869947,-1.20027737376273,1.63920819879853));
#38765=CARTESIAN_POINT('Ctrl Pts',(-3.77497570905141,-3.4226971150208,1.71858008885193));
#38766=CARTESIAN_POINT('Ctrl Pts',(-1.67814070389166,-4.81135541393673,
1.79795197890534));
#38767=CARTESIAN_POINT('Ctrl Pts',(0.827485662097738,-5.02797818437314,
1.87732386895874));
#38768=CARTESIAN_POINT('Ctrl Pts',(3.13153835248109,-4.01979659801894,1.95669575901214));
#38769=CARTESIAN_POINT('Ctrl Pts',(4.6727552317042,-2.03240145822472,2.03606764906555));
#38770=CARTESIAN_POINT('Ctrl Pts',(5.07569927947279,0.450082178237972,2.11543953911895));
#38771=CARTESIAN_POINT('Ctrl Pts',(4.24221421762082,2.82292679227462,2.19481142917235));
#38772=CARTESIAN_POINT('Ctrl Pts',(2.37533516234403,4.50811268818069,2.27418331922576));
#38773=CARTESIAN_POINT('Ctrl Pts',(-0.0701702807675918,5.09513231177087,
2.35355520927916));
#38774=CARTESIAN_POINT('Ctrl Pts',(-2.49858239880191,4.44098898210475,2.43292709933257));
#38775=CARTESIAN_POINT('Ctrl Pts',(-4.31834537500726,2.70503056635658,2.51229898938597));
#38776=CARTESIAN_POINT('Ctrl Pts',(-5.08616897635574,0.310132692129504,
2.59167087943937));
#38777=CARTESIAN_POINT('Ctrl Pts',(-4.61501307310829,-2.16031281943427,
2.67104276949278));
#38778=CARTESIAN_POINT('Ctrl Pts',(-3.01965020040969,-4.10451090995464,
2.75041465954618));
#38779=CARTESIAN_POINT('Ctrl Pts',(-0.688707222773715,-5.04885922799114,
2.82978654959958));
#38780=CARTESIAN_POINT('Ctrl Pts',(1.8100033099024,-4.7633166135492,2.90915843965299));
#38781=CARTESIAN_POINT('Ctrl Pts',(3.86780104266064,-3.31744061546923,2.98853032970639));
#38782=CARTESIAN_POINT('Ctrl Pts',(4.98341100265916,-1.06344342649117,3.0679022197598));
#38783=CARTESIAN_POINT('Ctrl Pts',(4.88507307300304,1.44960622728803,3.1472741098132));
#38784=CARTESIAN_POINT('Ctrl Pts',(3.59674215568923,3.60953501274882,3.2266459998666));
#38785=CARTESIAN_POINT('Ctrl Pts',(1.43225281050325,4.89018905867422,3.30601788992001));
#38786=CARTESIAN_POINT('Ctrl Pts',(-1.0811301490835,4.97960387415649,3.38538977997341));
#38787=CARTESIAN_POINT('Ctrl Pts',(-3.3311521973945,3.85599820806045,3.46476167002682));
#38788=CARTESIAN_POINT('Ctrl Pts',(-4.76971294380054,1.79307991358813,3.54413356008021));
#38789=CARTESIAN_POINT('Ctrl Pts',(-5.04638217467727,-0.706628678919173,
3.62350545013362));
#38790=CARTESIAN_POINT('Ctrl Pts',(-4.09376387778011,-3.03420408933784,
3.70287734018702));
#38791=CARTESIAN_POINT('Ctrl Pts',(-2.14391376164834,-4.62265409969061,
3.78224923024043));
#38792=CARTESIAN_POINT('Ctrl Pts',(0.328189001348338,-5.08503580343006,
3.86162112029383));
#38793=CARTESIAN_POINT('Ctrl Pts',(2.72034565005059,-4.30871404098977,3.94099301034724));
#38794=CARTESIAN_POINT('Ctrl Pts',(4.44983211978348,-2.48279907534115,4.02036490040064));
#38795=CARTESIAN_POINT('Ctrl Pts',(5.09534933467345,-0.0520797505219637,
4.09973679045404));
#38796=CARTESIAN_POINT('Ctrl Pts',(4.49965073000142,2.39132608624781,4.17910868050745));
#38797=CARTESIAN_POINT('Ctrl Pts',(2.80784716730899,4.25221018151813,4.25848057056085));
#38798=CARTESIAN_POINT('Ctrl Pts',(0.432058249724383,5.07726528867822,4.33785246061425));
#38799=CARTESIAN_POINT('Ctrl Pts',(-2.04897910114838,4.66550980985238,4.41722435066766));
#38800=CARTESIAN_POINT('Ctrl Pts',(-4.03088967831969,3.1172464682773,4.49659624072106));
#38801=CARTESIAN_POINT('Ctrl Pts',(-5.0308844520753,0.809628786937908,4.57596813077447));
#38802=CARTESIAN_POINT('Ctrl Pts',(-4.80536690897923,-1.69521267481664,
4.65534002082787));
#38803=CARTESIAN_POINT('Ctrl Pts',(-3.40927262335505,-3.78710408127548,
4.73471191088127));
#38804=CARTESIAN_POINT('Ctrl Pts',(-1.18268707297853,-4.9564653161483,4.81408380093467));
#38805=CARTESIAN_POINT('Ctrl Pts',(1.33199843054213,-4.91844257095729,4.89345569098808));
#38806=CARTESIAN_POINT('Ctrl Pts',(3.52221206471124,-3.68229810226904,4.97282758104148));
#38807=CARTESIAN_POINT('Ctrl Pts',(4.85442263620086,-1.54915396649666,5.05219947109489));
#38808=CARTESIAN_POINT('Ctrl Pts',(5.00410659859419,0.961360646520152,5.13157136114829));
#38809=CARTESIAN_POINT('Ctrl Pts',(3.93480126997208,3.23768993398037,5.21094325120169));
#38810=CARTESIAN_POINT('Ctrl Pts',(1.90698706151963,4.72532512002807,5.2903151412551));
#38811=CARTESIAN_POINT('Ctrl Pts',(-0.585364974074726,5.06188156616668,
5.3696870313085));
#38812=CARTESIAN_POINT('Ctrl Pts',(-2.93512339766788,4.1653748670719,5.44905892136191));
#38813=CARTESIAN_POINT('Ctrl Pts',(-4.56989225837456,2.25419207025927,5.52843081141531));
#38814=CARTESIAN_POINT('Ctrl Pts',(-5.09144548022617,-0.206106925298976,
5.60780270146872));
#38815=CARTESIAN_POINT('Ctrl Pts',(-4.37273385281808,-2.61619873006436,
5.68717459152211));
#38816=CARTESIAN_POINT('Ctrl Pts',(-2.58883393774572,-4.38899031504372,
5.76654648157553));
#38817=CARTESIAN_POINT('Ctrl Pts',(-0.174299805725225,-5.09263357414371,
5.84591837162892));
#38818=CARTESIAN_POINT('Ctrl Pts',(2.28269337316386,-4.5557225669355,5.92529026168233));
#38819=CARTESIAN_POINT('Ctrl Pts',(4.18362749900631,-2.90904762634266,6.00466215173574));
#38820=CARTESIAN_POINT('Ctrl Pts',(5.0654392263932,-0.553735123040447,6.08403404178913));
#38821=CARTESIAN_POINT('Ctrl Pts',(4.71332117039027,1.9364660305625,6.16340593184254));
#38822=CARTESIAN_POINT('Ctrl Pts',(3.21304851003972,3.95494834541529,6.24277782189595));
#38823=CARTESIAN_POINT('Ctrl Pts',(0.93008434460575,5.01001399745458,6.32214971194934));
#38824=CARTESIAN_POINT('Ctrl Pts',(-1.57944630846742,4.84465132919185,6.40152160200275));
#38825=CARTESIAN_POINT('Ctrl Pts',(-3.70422733684302,3.49914232059178,6.48089349205615));
#38826=CARTESIAN_POINT('Ctrl Pts',(-4.92666678513181,1.30124998791572,6.56026538210956));
#38827=CARTESIAN_POINT('Ctrl Pts',(-4.94898110955443,-1.21362396154863,
6.63963727216295));
#38828=CARTESIAN_POINT('Ctrl Pts',(-3.76573459007348,-3.43286180029078,
6.71900916221637));
#38829=CARTESIAN_POINT('Ctrl Pts',(-1.66516345976277,-4.81586210299283,
6.79838105226976));
#38830=CARTESIAN_POINT('Ctrl Pts',(0.841037803569352,-5.02572905713577,
6.87775294232318));
#38831=CARTESIAN_POINT('Ctrl Pts',(3.14236411955759,-4.01133953722303,6.95712483237658));
#38832=CARTESIAN_POINT('Ctrl Pts',(4.6782174915266,-2.0197965849922,7.03649672242998));
#38833=CARTESIAN_POINT('Ctrl Pts',(5.0744674376185,0.463764344598802,7.11586861248339));
#38834=CARTESIAN_POINT('Ctrl Pts',(4.23458834804968,2.83435330637052,7.19524050253678));
#38835=CARTESIAN_POINT('Ctrl Pts',(2.36317290999828,4.51450007644499,7.2746123925902));
#38836=CARTESIAN_POINT('Ctrl Pts',(-0.0839062181341898,5.09492462057389,
7.35398428264359));
#38837=CARTESIAN_POINT('Ctrl Pts',(-2.51054597725242,4.43423680455535,7.433356172697));
#38838=CARTESIAN_POINT('Ctrl Pts',(-4.32562229331123,2.69337871796382,7.5127280627504));
#38839=CARTESIAN_POINT('Ctrl Pts',(-5.08698659332198,0.296419537368979,
7.5920999528038));
#38840=CARTESIAN_POINT('Ctrl Pts',(-4.60917221905333,-2.17274678641544,
7.67147184285721));
#38841=CARTESIAN_POINT('Ctrl Pts',(-3.00857369445294,-4.11263680232249,
7.75084373291061));
#38842=CARTESIAN_POINT('Ctrl Pts',(-0.675093277248738,-5.05069759635094,
7.83021562296402));
#38843=CARTESIAN_POINT('Ctrl Pts',(1.82283836799964,-4.7584196354378,7.90958751301742));
#38844=CARTESIAN_POINT('Ctrl Pts',(3.8767306215876,-3.30700118391521,7.98895940307083));
#38845=CARTESIAN_POINT('Ctrl Pts',(4.9862598767545,-1.05000456391383,8.06833129312422));
#38846=CARTESIAN_POINT('Ctrl Pts',(4.881147262843,1.46277084371127,8.14770318317763));
#38847=CARTESIAN_POINT('Ctrl Pts',(3.58699797993919,3.61921851159664,8.22707507323104));
#38848=CARTESIAN_POINT('Ctrl Pts',(1.41906392880751,4.89403256106139,8.30644696328444));
#38849=CARTESIAN_POINT('Ctrl Pts',(-1.09455095433695,4.97667111140887,8.38581885333784));
#38850=CARTESIAN_POINT('Ctrl Pts',(-3.34153564775234,3.84700359469183,8.46519074339125));
#38851=CARTESIAN_POINT('Ctrl Pts',(-4.77452965373897,1.7802145175059,8.54456263344465));
#38852=CARTESIAN_POINT('Ctrl Pts',(-5.04445880431694,-0.720230875706447,
8.62393452349805));
#38853=CARTESIAN_POINT('Ctrl Pts',(-4.08556895588349,-3.04522962180074,
8.70330641355146));
#38854=CARTESIAN_POINT('Ctrl Pts',(-2.1314435530503,-4.62841717252583,8.78267830360486));
#38855=CARTESIAN_POINT('Ctrl Pts',(0.341896781435676,-5.08413254485124,
8.86205019365827));
#38856=CARTESIAN_POINT('Ctrl Pts',(2.73195181673958,-4.30136448278739,8.94142208371167));
#38857=CARTESIAN_POINT('Ctrl Pts',(4.45650943655852,-2.47079355362535,9.02079397376506));
#38858=CARTESIAN_POINT('Ctrl Pts',(5.09547122194811,-0.0383427838088964,
9.10016586381848));
#38859=CARTESIAN_POINT('Ctrl Pts',(4.49318749630538,2.40344820327308,9.17953775387187));
#38860=CARTESIAN_POINT('Ctrl Pts',(2.79637324206448,4.25976452798008,9.25890964392529));
#38861=CARTESIAN_POINT('Ctrl Pts',(0.418368655723882,5.07841164249998,9.33828153397869));
#38862=CARTESIAN_POINT('Ctrl Pts',(-2.06154960910779,4.65996892178041,9.41765342403209));
#38863=CARTESIAN_POINT('Ctrl Pts',(-4.03927895232343,3.10636808638134,9.49702531408549));
#38864=CARTESIAN_POINT('Ctrl Pts',(-5.03304888354539,0.79606286096894,9.5763972041389));
#38865=CARTESIAN_POINT('Ctrl Pts',(-4.80077924720044,-1.70816151532024,
9.6557690941923));
#38866=CARTESIAN_POINT('Ctrl Pts',(-3.39905041258209,-3.7962815274288,9.7351409842457));
#38867=CARTESIAN_POINT('Ctrl Pts',(-1.16932042112922,-4.95963576238233,
9.81451287429911));
#38868=CARTESIAN_POINT('Ctrl Pts',(1.34525343666388,-4.91483370358709,9.89388476435251));
#38869=CARTESIAN_POINT('Ctrl Pts',(3.53212653495364,-3.67278903339792,9.97325665440591));
#38870=CARTESIAN_POINT('Ctrl Pts',(4.85858142755815,-1.53606108425365,10.0526285444593));
#38871=CARTESIAN_POINT('Ctrl Pts',(5.00149663869711,0.974847945001263,10.1320004345127));
#38872=CARTESIAN_POINT('Ctrl Pts',(3.92605833927446,3.24828617264322,10.2113723245661));
#38873=CARTESIAN_POINT('Ctrl Pts',(1.89424091858727,4.73044907858876,10.2907442146195));
#38874=CARTESIAN_POINT('Ctrl Pts',(-0.599009397036607,5.0602850596615,10.3701161046729));
#38875=CARTESIAN_POINT('Ctrl Pts',(-2.94634234942717,4.15744680095171,10.4494879947264));
#38876=CARTESIAN_POINT('Ctrl Pts',(-4.57595282711548,2.24186370388246,10.5288598847797));
#38877=CARTESIAN_POINT('Ctrl Pts',(-5.09087132481819,-0.219832429171425,
10.6082317748331));
#38878=CARTESIAN_POINT('Ctrl Pts',(-4.36566483624775,-2.62797786906995,
10.6876036648866));
#38879=CARTESIAN_POINT('Ctrl Pts',(-2.57699205680257,-4.39595371699339,
10.7669755549399));
#38880=CARTESIAN_POINT('Ctrl Pts',(-0.160569716395434,-5.09308496973576,
10.8463474449934));
#38881=CARTESIAN_POINT('Ctrl Pts',(2.2949670515106,-4.54955199720284,10.9257193350468));
#38882=CARTESIAN_POINT('Ctrl Pts',(4.19145492549203,-2.89775822841384,11.0050912251002));
#38883=CARTESIAN_POINT('Ctrl Pts',(5.06691365725173,-0.540076969262297,
11.0844631151535));
#38884=CARTESIAN_POINT('Ctrl Pts',(4.70808343752805,1.94916584416147,11.163835005207));
#38885=CARTESIAN_POINT('Ctrl Pts',(3.20237451358847,3.96359617235289,11.2432068952604));
#38886=CARTESIAN_POINT('Ctrl Pts',(0.916574246474504,5.01250324623051,11.3225787853138));
#38887=CARTESIAN_POINT('Ctrl Pts',(-1.59250147827797,4.84037562431409,11.4019506753672));
#38888=CARTESIAN_POINT('Ctrl Pts',(-3.71364736786416,3.4891432143045,11.4813225654206));
#38889=CARTESIAN_POINT('Ctrl Pts',(-4.93015697865768,1.28796324037784,11.560694455474));
#38890=CARTESIAN_POINT('Ctrl Pts',(-4.94569126216756,-1.22696172804661,
11.6400663455274));
#38891=CARTESIAN_POINT('Ctrl Pts',(-3.75646610131532,-3.44300153535262,
11.7194382355808));
#38892=CARTESIAN_POINT('Ctrl Pts',(-1.65217411297936,-4.82033378960134,
11.7988101256342));
#38893=CARTESIAN_POINT('Ctrl Pts',(0.854583832252985,-5.02344340233105,
11.8781820156876));
#38894=CARTESIAN_POINT('Ctrl Pts',(3.15316704753777,-4.00285332145629,11.957553905741));
#38895=CARTESIAN_POINT('Ctrl Pts',(4.6836457494592,-2.00717703164028,12.0369257957944));
#38896=CARTESIAN_POINT('Ctrl Pts',(5.07319871388639,0.477443140272258,12.1162976858478));
#38897=CARTESIAN_POINT('Ctrl Pts',(4.22693170094574,2.84575922001696,12.1956695759012));
#38898=CARTESIAN_POINT('Ctrl Pts',(2.35099348180933,4.52085465274672,12.2750414659546));
#38899=CARTESIAN_POINT('Ctrl Pts',(-0.0976415456600611,5.09467989880942,
12.354413356008));
#38900=CARTESIAN_POINT('Ctrl Pts',(-2.52249130873252,4.4274523984048,12.4337852460614));
#38901=CARTESIAN_POINT('Ctrl Pts',(-4.33286777243754,2.68170729374847,12.5131571361148));
#38902=CARTESIAN_POINT('Ctrl Pts',(-5.08776723741693,0.282704228193439,
12.5925290261682));
#38903=CARTESIAN_POINT('Ctrl Pts',(-4.60329786494335,-2.18516496159434,
12.6719009162216));
#38904=CARTESIAN_POINT('Ctrl Pts',(-2.99747532179655,-4.12073280351837,
12.751272806275));
#38905=CARTESIAN_POINT('Ctrl Pts',(-0.661474425059184,-5.05249925559264,
12.8306446963284));
#38906=CARTESIAN_POINT('Ctrl Pts',(1.83566017747378,-4.75348807252195,12.9100165863819));
#38907=CARTESIAN_POINT('Ctrl Pts',(3.885632023939,-3.29653771665232,12.9893884764353));
#38908=CARTESIAN_POINT('Ctrl Pts',(4.98907251007332,-1.03655806976862,13.0687603664887));
#38909=CARTESIAN_POINT('Ctrl Pts',(4.87718597587842,1.47592482852836,13.1481322565421));
#38910=CARTESIAN_POINT('Ctrl Pts',(3.5772277334276,3.62887570549998,13.2275041465955));
#38911=CARTESIAN_POINT('Ctrl Pts',(1.4058647331731,4.89784049299196,13.3068760366489));
#38912=CARTESIAN_POINT('Ctrl Pts',(-1.10796380425358,4.97370217757714,13.3862479267023));
#38913=CARTESIAN_POINT('Ctrl Pts',(-3.35189481140037,3.83798102080754,13.4656198167557));
#38914=CARTESIAN_POINT('Ctrl Pts',(-4.77931166178332,1.76733618259613,13.5449917068091));
#38915=CARTESIAN_POINT('Ctrl Pts',(-5.0424987701828,-0.733827837763376,
13.6243635968625));
#38916=CARTESIAN_POINT('Ctrl Pts',(-4.07734433954749,-3.0562330211441,13.7037354869159));
#38917=CARTESIAN_POINT('Ctrl Pts',(-2.11895785284703,-4.6341466054312,13.7831073769693));
#38918=CARTESIAN_POINT('Ctrl Pts',(0.355602076573349,-5.08319233414479,
13.8624792670227));
#38919=CARTESIAN_POINT('Ctrl Pts',(2.74353812725229,-4.29398366171607,13.9418511570761));
#38920=CARTESIAN_POINT('Ctrl Pts',(4.4631543628512,-2.45877007386494,14.0212230471295));
#38921=CARTESIAN_POINT('Ctrl Pts',(5.09555607468418,-0.024605538415575,
14.1005949371829));
#38922=CARTESIAN_POINT('Ctrl Pts',(4.48669160554615,2.41555285172843,14.1799668272363));
#38923=CARTESIAN_POINT('Ctrl Pts',(2.78487899242048,4.26728791392691,14.2593387172897));
#38924=CARTESIAN_POINT('Ctrl Pts',(0.404676020966283,5.07952108577437,14.3387106073431));
#38925=CARTESIAN_POINT('Ctrl Pts',(-2.07410513346011,4.65439416445642,14.4180824973965));
#38926=CARTESIAN_POINT('Ctrl Pts',(-4.0476388683295,3.09546712700361,14.4974543874499));
#38927=CARTESIAN_POINT('Ctrl Pts',(-5.03517673417046,0.782491149112972,
14.5768262775033));
#38928=CARTESIAN_POINT('Ctrl Pts',(-4.79615669274215,-1.72109794068678,
14.6561981675567));
#38929=CARTESIAN_POINT('Ctrl Pts',(-3.38880349707463,-3.80543138172091,
14.7355700576101));
#38930=CARTESIAN_POINT('Ctrl Pts',(-1.15594527050905,-4.96277016134733,
14.8149419476636));
#38931=CARTESIAN_POINT('Ctrl Pts',(1.35849866531108,-4.91118911457496,14.8943138377169));
#38932=CARTESIAN_POINT('Ctrl Pts',(3.54201533324722,-3.66325327022487,14.9736857277704));
#38933=CARTESIAN_POINT('Ctrl Pts',(4.86270490612231,-1.52295703772157,15.0530576178238));
#38934=CARTESIAN_POINT('Ctrl Pts',(4.99885032728073,0.988328158162469,15.1324295078772));
#38935=CARTESIAN_POINT('Ctrl Pts',(3.91728687348112,3.25885880234541,15.2118013979306));
#38936=CARTESIAN_POINT('Ctrl Pts',(1.8814810080689,4.73553865563863,15.291173287984));
#38937=CARTESIAN_POINT('Ctrl Pts',(-0.612649466321345,5.05865177435528,
15.3705451780374));
#38938=CARTESIAN_POINT('Ctrl Pts',(-2.95753988679226,4.14948851797474,15.4499170680908));
#38939=CARTESIAN_POINT('Ctrl Pts',(-4.58198013724412,2.22951904335266,15.5292889581442));
#38940=CARTESIAN_POINT('Ctrl Pts',(-5.09026016830427,-0.233556335273548,
15.6086608481976));
#38941=CARTESIAN_POINT('Ctrl Pts',(-4.35856408946536,-2.63973790759512,
15.688032738251));
#38942=CARTESIAN_POINT('Ctrl Pts',(-2.56513144595043,-4.40288516858759,
15.7674046283044));
#38943=CARTESIAN_POINT('Ctrl Pts',(-0.146838460024607,-5.09349934813251,
15.8467765183578));
#38944=CARTESIAN_POINT('Ctrl Pts',(2.3072240497427,-4.54334836074314,15.9261484084112));
#38945=CARTESIAN_POINT('Ctrl Pts',(4.19925188794477,-2.88644776920547,16.0055202984646));
#38946=CARTESIAN_POINT('Ctrl Pts',(5.06835126113318,-0.526414890137456,
16.084892188518));
#38947=CARTESIAN_POINT('Ctrl Pts',(4.70281148570858,1.96185149097663,16.1642640785714));
#38948=CARTESIAN_POINT('Ctrl Pts',(3.19167724187374,3.97221519135797,16.2436359686248));
#38949=CARTESIAN_POINT('Ctrl Pts',(0.90305748655408,5.01495606350291,16.3230078586782));
#38950=CARTESIAN_POINT('Ctrl Pts',(-1.60554507356452,4.83606473894038,16.4023797487316));
#38951=CARTESIAN_POINT('Ctrl Pts',(-3.72304040765551,3.47911874852373,16.481751638785));
#38952=CARTESIAN_POINT('Ctrl Pts',(-4.93361133910263,1.27466713166901,16.5611235288384));
#38953=CARTESIAN_POINT('Ctrl Pts',(-4.94236546898943,-1.24029057666156,
16.6404954188918));
#38954=CARTESIAN_POINT('Ctrl Pts',(-3.74717030983909,-3.45311624655429,
16.7198673089452));
#38955=CARTESIAN_POINT('Ctrl Pts',(-1.6391727584367,-4.82477044080732,16.7992391989986));
#38956=CARTESIAN_POINT('Ctrl Pts',(0.868123650569205,-5.02112123762451,
16.8786110890521));
#38957=CARTESIAN_POINT('Ctrl Pts',(3.16394705627606,-3.99433801030565,16.9579829791054));
#38958=CARTESIAN_POINT('Ctrl Pts',(4.68903996911093,-1.99454289389466,17.0373548691589));
#38959=CARTESIAN_POINT('Ctrl Pts',(5.07189311172224,0.491118473430398,17.1167267592122));
#38960=CARTESIAN_POINT('Ctrl Pts',(4.21924434286031,2.85714443596481,17.1960986492657));
#38961=CARTESIAN_POINT('Ctrl Pts',(2.33879694571596,4.52717639800277,17.275470539319));
#38962=CARTESIAN_POINT('Ctrl Pts',(-0.11137612465114,5.09439809707615,17.3548424293725));
#38963=CARTESIAN_POINT('Ctrl Pts',(-2.53441837980398,4.42063590960358,17.4342143194259));
#38964=CARTESIAN_POINT('Ctrl Pts',(-4.34008162116489,2.67001619606203,17.5135862094793));
#38965=CARTESIAN_POINT('Ctrl Pts',(-5.08851116459639,0.268987208843763,
17.5929580995327));
#38966=CARTESIAN_POINT('Ctrl Pts',(-4.59738955946409,-2.19756790530666,
17.6723299895861));
#38967=CARTESIAN_POINT('Ctrl Pts',(-2.98635609589589,-4.12879762624818,
17.7517018796395));
#38968=CARTESIAN_POINT('Ctrl Pts',(-0.647849003889666,-5.05426651218747,
17.8310737696929));
#38969=CARTESIAN_POINT('Ctrl Pts',(1.84846531944351,-4.7485175808327,17.9104456597463));
#38970=CARTESIAN_POINT('Ctrl Pts',(3.89451146459875,-3.28605855970652,17.9898175497997));
#38971=CARTESIAN_POINT('Ctrl Pts',(4.99183702504825,-1.02308842638974,18.0691894398531));
#38972=CARTESIAN_POINT('Ctrl Pts',(4.87321162956217,1.48903860109228,18.1485613299065));
#38973=CARTESIAN_POINT('Ctrl Pts',(3.5673892128293,3.63856219800459,18.2279332199599));
#38974=CARTESIAN_POINT('Ctrl Pts',(1.39273514199697,4.90150770362139,18.3073051100133));
#38975=CARTESIAN_POINT('Ctrl Pts',(-1.12151932172649,4.97089558679471,18.3866770000667));
#38976=CARTESIAN_POINT('Ctrl Pts',(-3.36194502775882,3.82855576883779,18.4660488901201));
#38977=CARTESIAN_POINT('Ctrl Pts',(-4.78459624359504,1.75515257798274,18.5454207801735));
#38978=CARTESIAN_POINT('Ctrl Pts',(-5.03948789886558,-0.748754766453475,
18.6247926702269));
#38979=CARTESIAN_POINT('Ctrl Pts',(-4.0710021077043,-3.06469899064074,18.7041645602803));
#38980=CARTESIAN_POINT('Ctrl Pts',(-2.10287077052062,-4.64454172754396,
18.7835364503337));
#38981=CARTESIAN_POINT('Ctrl Pts',(0.36273133865386,-5.07374792580598,18.8629083403871));
#38982=CARTESIAN_POINT('Ctrl Pts',(3.56709774791096,-4.04128406294332,18.968737527125));
#38983=CARTESIAN_POINT('Ctrl Pts',(5.77704085522352,-0.0189872057267309,
19.1010240105473));
#38984=CARTESIAN_POINT('Ctrl Pts',(3.14459942081972,4.8501664079131,19.2597677906541));
#38985=CARTESIAN_POINT('Ctrl Pts',(-2.36591519662263,5.26902047281295,19.418511570761));
#38986=CARTESIAN_POINT('Ctrl Pts',(-5.71123844601178,0.872727032859995,
19.5772553508678));
#38987=CARTESIAN_POINT('Ctrl Pts',(-3.83058845612596,-4.3254192567976,19.7359991309746));
#38988=CARTESIAN_POINT('Ctrl Pts',(1.55524717023751,-5.5639435857319,19.8947429110814));
#38989=CARTESIAN_POINT('Ctrl Pts',(5.51805139390222,-1.71188403765725,20.0534866911882));
#38990=CARTESIAN_POINT('Ctrl Pts',(4.43131449514919,3.70671199728542,20.212230471295));
#38991=CARTESIAN_POINT('Ctrl Pts',(-0.709818611660639,5.73400533709385,
20.3709742514018));
#38992=CARTESIAN_POINT('Ctrl Pts',(-5.20235975367858,2.51303602329798,20.5297180315086));
#38993=CARTESIAN_POINT('Ctrl Pts',(-4.93271294602024,-3.0047419943643,20.6884618116154));
#38994=CARTESIAN_POINT('Ctrl Pts',(-0.152720854580618,-5.77834717219765,
20.8472055917222));
#38995=CARTESIAN_POINT('Ctrl Pts',(4.77339715849037,-3.25411141853181,21.005949371829));
#38996=CARTESIAN_POINT('Ctrl Pts',(5.22808970274015,1.3127228499015,21.1382358552514));
#38997=CARTESIAN_POINT('Ctrl Pts',(3.1707451501151,3.97754537770267,21.2440650419892));
#38998=CARTESIAN_POINT('Ctrl Pts',(0.895150293052777,5.019216999618,21.3234369320426));
#38999=CARTESIAN_POINT('Ctrl Pts',(-1.62157688245131,4.83072732396133,21.402808822096));
#39000=CARTESIAN_POINT('Ctrl Pts',(-3.73081451079173,3.46959580775127,21.4821807121495));
#39001=CARTESIAN_POINT('Ctrl Pts',(-4.93787328845979,1.26108254025601,21.5615526022028));
#39002=CARTESIAN_POINT('Ctrl Pts',(-4.93855701420288,-1.25346250930809,
21.6409244922563));
#39003=CARTESIAN_POINT('Ctrl Pts',(-3.73808388472054,-3.46328419200818,
21.7202963823096));
#39004=CARTESIAN_POINT('Ctrl Pts',(-1.62603418385006,-4.82913054051807,
21.7996682723631));
#39005=CARTESIAN_POINT('Ctrl Pts',(0.881590795203928,-5.01878454751451,
21.8790401624164));
#39006=CARTESIAN_POINT('Ctrl Pts',(3.17473921804455,-3.98578203611947,21.9584120524699));
#39007=CARTESIAN_POINT('Ctrl Pts',(4.69438148876591,-1.98190041394297,22.0377839425233));
#39008=CARTESIAN_POINT('Ctrl Pts',(5.0705605156318,0.504793485523968,22.1171558325767));
#39009=CARTESIAN_POINT('Ctrl Pts',(4.21152107628908,2.86850718608746,22.1965277226301));
#39010=CARTESIAN_POINT('Ctrl Pts',(2.32658621700133,4.53346610033867,22.2758996126835));
#39011=CARTESIAN_POINT('Ctrl Pts',(-0.125111436169825,5.09407888617233,
22.3552715027369));
#39012=CARTESIAN_POINT('Ctrl Pts',(-2.54632610813663,4.41378735452051,22.4346433927903));
#39013=CARTESIAN_POINT('Ctrl Pts',(-4.34726461344783,2.6583059213356,22.5140152828437));
#39014=CARTESIAN_POINT('Ctrl Pts',(-5.08921736705482,0.255267617363269,
22.5933871728972));
#39015=CARTESIAN_POINT('Ctrl Pts',(-4.59144894277882,-2.20995361377114,
22.6727590629504));
#39016=CARTESIAN_POINT('Ctrl Pts',(-2.97521323819314,-4.13683487704257,
22.7521309530039));
#39017=CARTESIAN_POINT('Ctrl Pts',(-0.634222428965717,-5.05599240530685,
22.8315028430573));
#39018=CARTESIAN_POINT('Ctrl Pts',(1.8612636949988,-4.74352133023588,22.9108747331107));
#39019=CARTESIAN_POINT('Ctrl Pts',(3.90335003127195,-3.27553898237365,22.9902466231641));
#39020=CARTESIAN_POINT('Ctrl Pts',(4.99458897767401,-1.00964257616381,23.0696185132175));
#39021=CARTESIAN_POINT('Ctrl Pts',(4.86915708441603,1.5022005201609,23.1489904032709));
#39022=CARTESIAN_POINT('Ctrl Pts',(3.55760931370069,3.6481108983516,23.2283622933243));
#39023=CARTESIAN_POINT('Ctrl Pts',(1.37943578318338,4.90534953479997,23.3077341833777));
#39024=CARTESIAN_POINT('Ctrl Pts',(-1.13476524781216,4.96765588336336,23.3871060734311));
#39025=CARTESIAN_POINT('Ctrl Pts',(-3.37253997777701,3.81985225393738,23.4664779634845));
#39026=CARTESIAN_POINT('Ctrl Pts',(-4.78877143331127,1.74154107082816,23.545849853538));
#39027=CARTESIAN_POINT('Ctrl Pts',(-5.03846876789875,-0.76100566244534,
23.6252217435914));
#39028=CARTESIAN_POINT('Ctrl Pts',(-4.06080626285345,-3.07817310072711,
23.7045936336447));
#39029=CARTESIAN_POINT('Ctrl Pts',(-2.09394034074327,-4.64550438513341,
23.7839655236982));
#39030=CARTESIAN_POINT('Ctrl Pts',(0.383004813579298,-5.08120108394905,
23.8633374137515));
#39031=CARTESIAN_POINT('Ctrl Pts',(2.76665084304599,-4.27912844577405,23.942709303805));
#39032=CARTESIAN_POINT('Ctrl Pts',(4.47634685104287,-2.43466958989253,24.0220811938583));
#39033=CARTESIAN_POINT('Ctrl Pts',(5.0956146743416,0.00286938903386649,
24.1014530839118));
#39034=CARTESIAN_POINT('Ctrl Pts',(4.47360204192767,2.4397093911446,24.1808249739652));
#39035=CARTESIAN_POINT('Ctrl Pts',(2.76182985424755,4.28224158577674,24.2601968640186));
#39036=CARTESIAN_POINT('Ctrl Pts',(0.377282027280861,5.08162920869509,24.339568754072));
#39037=CARTESIAN_POINT('Ctrl Pts',(-2.09917086643256,4.64314320437055,24.4189406441253));
#39038=CARTESIAN_POINT('Ctrl Pts',(-4.06427038351852,3.07359779288466,24.4983125341788));
#39039=CARTESIAN_POINT('Ctrl Pts',(-5.03932263128953,0.755330762345285,
24.5776844242322));
#39040=CARTESIAN_POINT('Ctrl Pts',(-4.78680704042971,-1.74693317000509,
24.6570563142856));
#39041=CARTESIAN_POINT('Ctrl Pts',(-3.36823584993892,-3.82364804891321,
24.736428204339));
#39042=CARTESIAN_POINT('Ctrl Pts',(-1.12916986186658,-4.96893072660747,
24.8158000943924));
#39043=CARTESIAN_POINT('Ctrl Pts',(1.38495940518137,-4.90379287784174,24.8951719844458));
#39044=CARTESIAN_POINT('Ctrl Pts',(3.56171562668277,-3.64410193839515,24.9745438744992));
#39045=CARTESIAN_POINT('Ctrl Pts',(4.87084580524804,-1.49671583283838,25.0539157645526));
#39046=CARTESIAN_POINT('Ctrl Pts',(4.99344872708924,1.01526693667351,25.133287654606));
#39047=CARTESIAN_POINT('Ctrl Pts',(3.8996585918228,3.27993292766699,25.2126595446594));
#39048=CARTESIAN_POINT('Ctrl Pts',(1.85592025533624,4.7456145174892,25.2920314347128));
#39049=CARTESIAN_POINT('Ctrl Pts',(-0.639916147340462,5.05527491509063,
25.3714033247662));
#39050=CARTESIAN_POINT('Ctrl Pts',(-2.9798703929554,4.13348153303719,25.4507752148196));
#39051=CARTESIAN_POINT('Ctrl Pts',(-4.59393480667762,2.20478119884206,25.5301471048731));
#39052=CARTESIAN_POINT('Ctrl Pts',(-5.08892686999539,-0.260998955190596,
25.6095189949264));
#39053=CARTESIAN_POINT('Ctrl Pts',(-4.34426761193083,-2.66320034145021,
25.6888908849798));
#39054=CARTESIAN_POINT('Ctrl Pts',(-2.54135437947314,-4.41665201942651,
25.7682627750333));
#39055=CARTESIAN_POINT('Ctrl Pts',(-0.119372845368366,-5.09421704156391,
25.8476346650866));
#39056=CARTESIAN_POINT('Ctrl Pts',(2.33168764964084,-4.53084206823456,25.9270065551401));
#39057=CARTESIAN_POINT('Ctrl Pts',(4.21475419430065,-2.86376399593205,26.0063784451934));
#39058=CARTESIAN_POINT('Ctrl Pts',(5.07111594642898,-0.49907935305457,26.0857503352469));
#39059=CARTESIAN_POINT('Ctrl Pts',(4.69216507873193,1.98717991553359,26.1651222253003));
#39060=CARTESIAN_POINT('Ctrl Pts',(3.17021318378706,3.98936655524586,26.2444941153537));
#39061=CARTESIAN_POINT('Ctrl Pts',(0.876004374419533,5.01975233241337,26.3238660054071));
#39062=CARTESIAN_POINT('Ctrl Pts',(-1.63159716155383,4.82733755243831,26.4032378954604));
#39063=CARTESIAN_POINT('Ctrl Pts',(-3.74174524045176,3.4589940298197,26.4826097855139));
#39064=CARTESIAN_POINT('Ctrl Pts',(-4.94041246098821,1.2480472178904,26.5619816755672));
#39065=CARTESIAN_POINT('Ctrl Pts',(-4.93560614144543,-1.26692113381128,
26.6413535656207));
#39066=CARTESIAN_POINT('Ctrl Pts',(-3.72849709062547,-3.4732703015989,26.7207254556741));
#39067=CARTESIAN_POINT('Ctrl Pts',(-1.61313440141745,-4.8335385118705,26.8000973457275));
#39068=CARTESIAN_POINT('Ctrl Pts',(0.895184257363441,-5.01636743950643,
26.8794692357809));
#39069=CARTESIAN_POINT('Ctrl Pts',(3.18543801250735,-3.97722036241957,26.9588411258343));
#39070=CARTESIAN_POINT('Ctrl Pts',(4.69972611865188,-1.96923120847525,27.0382130158877));
#39071=CARTESIAN_POINT('Ctrl Pts',(5.06917134496014,0.51845830903431,27.1175849059411));
#39072=CARTESIAN_POINT('Ctrl Pts',(4.20377765205651,2.8798525300511,27.1969567959945));
#39073=CARTESIAN_POINT('Ctrl Pts',(2.31435302801598,4.53972104919287,27.2763286860479));
#39074=CARTESIAN_POINT('Ctrl Pts',(-0.138842870915707,5.09372356925338,
27.3557005761014));
#39075=CARTESIAN_POINT('Ctrl Pts',(-2.5582169538158,4.40690630260968,27.4350724661547));
#39076=CARTESIAN_POINT('Ctrl Pts',(-4.35441504928357,2.64657641517193,27.5144443562082));
#39077=CARTESIAN_POINT('Ctrl Pts',(-5.08988727708012,0.241546371095803,
27.5938162462615));
#39078=CARTESIAN_POINT('Ctrl Pts',(-4.58547423045432,-2.22232383432546,
27.6731881363149));
#39079=CARTESIAN_POINT('Ctrl Pts',(-2.96404981106488,-4.14484087273538,
27.7525600263683));
#39080=CARTESIAN_POINT('Ctrl Pts',(-0.620589418513009,-5.05768384899663,
27.8319319164217));
#39081=CARTESIAN_POINT('Ctrl Pts',(1.87404518273727,-4.73848623463559,27.9113038064751));
#39082=CARTESIAN_POINT('Ctrl Pts',(3.91216652560138,-3.26500386197866,27.9906756965286));
#39083=CARTESIAN_POINT('Ctrl Pts',(4.9972927622627,-0.99617377550726,28.0700475865819));
#39084=CARTESIAN_POINT('Ctrl Pts',(4.86508954335677,1.51532203768447,28.1494194766354));
#39085=CARTESIAN_POINT('Ctrl Pts',(3.54776128038217,3.65768875660473,28.2287913666887));
#39086=CARTESIAN_POINT('Ctrl Pts',(1.36620622234286,4.90905059057282,28.3081632567422));
#39087=CARTESIAN_POINT('Ctrl Pts',(-1.148153647413,4.96457856667651,28.3875351467955));
#39088=CARTESIAN_POINT('Ctrl Pts',(-3.382825830054,3.81074619284609,28.466907036849));
#39089=CARTESIAN_POINT('Ctrl Pts',(-4.79344912825184,1.72862448138202,28.5462789269024));
#39090=CARTESIAN_POINT('Ctrl Pts',(-5.03639882892723,-0.774586327501372,
28.6256508169557));
#39091=CARTESIAN_POINT('Ctrl Pts',(-4.05249292275565,-3.08910962152317,
28.7050227070092));
#39092=CARTESIAN_POINT('Ctrl Pts',(-2.0814087106417,-4.65113264937009,28.7843945970626));
#39093=CARTESIAN_POINT('Ctrl Pts',(0.39670205626447,-5.08015005893792,28.863766487116));
#39094=CARTESIAN_POINT('Ctrl Pts',(2.77817708034974,-4.27165415886996,28.9431383771694));
#39095=CARTESIAN_POINT('Ctrl Pts',(4.48289431705251,-2.42259276084734,29.0225102672228));
#39096=CARTESIAN_POINT('Ctrl Pts',(5.09558842083954,0.016606871399571,29.1018821572762));
#39097=CARTESIAN_POINT('Ctrl Pts',(4.46700846420369,2.45176110653224,29.1812540473296));
#39098=CARTESIAN_POINT('Ctrl Pts',(2.75027513324334,4.28967176299481,29.260625937383));
#39099=CARTESIAN_POINT('Ctrl Pts',(0.363580867455653,5.08262787301922,29.3399978274364));
#39100=CARTESIAN_POINT('Ctrl Pts',(-2.11168089287163,4.6374670833821,29.4193697174898));
#39101=CARTESIAN_POINT('Ctrl Pts',(-4.07254186182172,3.0626295770924,29.4987416075432));
#39102=CARTESIAN_POINT('Ctrl Pts',(-5.04134064765058,0.741742284838609,
29.5781134975966));
#39103=CARTESIAN_POINT('Ctrl Pts',(-4.78208001053002,-1.75983178618322,
29.6574853876501));
#39104=CARTESIAN_POINT('Ctrl Pts',(-3.35791526779889,-3.8327147294124,29.7368572777034));
#39105=CARTESIAN_POINT('Ctrl Pts',(-1.11576979845131,-4.97195684812685,
29.8162291677569));
#39106=CARTESIAN_POINT('Ctrl Pts',(1.3981747240844,-4.90004128387741,29.8956010578102));
#39107=CARTESIAN_POINT('Ctrl Pts',(3.57152697864042,-3.63448650893289,29.9749729478637));
#39108=CARTESIAN_POINT('Ctrl Pts',(4.87486316664055,-1.48357886521172,30.054344837917));
#39109=CARTESIAN_POINT('Ctrl Pts',(4.99069347757362,1.02872530622892,30.1337167279705));
#39110=CARTESIAN_POINT('Ctrl Pts',(3.89080190408237,3.29043427011703,30.2130886180238));
#39111=CARTESIAN_POINT('Ctrl Pts',(1.84311959890063,4.75060072905731,30.2924605080773));
#39112=CARTESIAN_POINT('Ctrl Pts',(-0.653542560897256,5.05353136567563,
30.3718323981307));
#39113=CARTESIAN_POINT('Ctrl Pts',(-2.99100319945254,4.12543294741732,30.4512042881841));
#39114=CARTESIAN_POINT('Ctrl Pts',(-4.59986207909447,2.19238819465906,30.5305761782375));
#39115=CARTESIAN_POINT('Ctrl Pts',(-5.08820473789096,-0.274717469549192,
30.6099480682909));
#39116=CARTESIAN_POINT('Ctrl Pts',(-4.33707198508738,-2.67490256625206,
30.6893199583443));
#39117=CARTESIAN_POINT('Ctrl Pts',(-2.52943809666249,-4.42348731861233,
30.7686918483976));
#39118=CARTESIAN_POINT('Ctrl Pts',(-0.10563868670687,-5.09452035138171,
30.8480637384511));
#39119=CARTESIAN_POINT('Ctrl Pts',(2.34389407350322,-4.52453950308404,30.9274356285044));
#39120=CARTESIAN_POINT('Ctrl Pts',(4.22245942552948,-2.85239084673345,31.006807518558));
#39121=CARTESIAN_POINT('Ctrl Pts',(5.07244300775219,-0.485406093778655,
31.0861794086112));
#39122=CARTESIAN_POINT('Ctrl Pts',(4.68679070094865,1.99982250919246,31.1655512986648));
#39123=CARTESIAN_POINT('Ctrl Pts',(3.15944655342927,3.99789877545637,31.2449231887181));
#39124=CARTESIAN_POINT('Ctrl Pts',(0.862468218810821,5.02209574921795,31.3242950787715));
#39125=CARTESIAN_POINT('Ctrl Pts',(-1.64460546486892,4.82292131469039,31.4036669688249));
#39126=CARTESIAN_POINT('Ctrl Pts',(-3.75105689757904,3.44889392325951,31.4830388588783));
#39127=CARTESIAN_POINT('Ctrl Pts',(-4.94375917286251,1.23472360611981,31.5624107489317));
#39128=CARTESIAN_POINT('Ctrl Pts',(-4.93217265646195,-1.28022264845634,
31.6417826389851));
#39129=CARTESIAN_POINT('Ctrl Pts',(-3.7191197981263,-3.48330949959324,31.7211545290385));
#39130=CARTESIAN_POINT('Ctrl Pts',(-1.60009758909914,-4.83786986680406,
31.8005264190919));
#39131=CARTESIAN_POINT('Ctrl Pts',(0.908704850876668,-5.01393584290474,
31.8798983091453));
#39132=CARTESIAN_POINT('Ctrl Pts',(3.196148800563,-3.96861814583255,31.9592701991988));
#39133=CARTESIAN_POINT('Ctrl Pts',(4.70501797698753,-1.9565538528228,32.0386420892521));
#39134=CARTESIAN_POINT('Ctrl Pts',(5.06775518859854,0.532122627976042,32.1180139793055));
#39135=CARTESIAN_POINT('Ctrl Pts',(4.19599845355282,2.89117521443338,32.1973858693589));
#39136=CARTESIAN_POINT('Ctrl Pts',(2.30210578290666,4.54594391816259,32.2767577594124));
#39137=CARTESIAN_POINT('Ctrl Pts',(-0.152574760830862,5.09333074570355,
32.3561296494657));
#39138=CARTESIAN_POINT('Ctrl Pts',(-2.57008843054848,4.39999347748749,32.4355015395192));
#39139=CARTESIAN_POINT('Ctrl Pts',(-4.3615342473787,2.63482753737587,32.5148734295725));
#39140=CARTESIAN_POINT('Ctrl Pts',(-5.09051997563981,0.227823441251348,
32.594245319626));
#39141=CARTESIAN_POINT('Ctrl Pts',(-4.57946630550992,-2.23467794088343,
32.6736172096794));
#39142=CARTESIAN_POINT('Ctrl Pts',(-2.95286477983452,-4.1528167229947,32.7529890997328));
#39143=CARTESIAN_POINT('Ctrl Pts',(-0.60695192984675,-5.05933854348835,
32.8323609897862));
#39144=CARTESIAN_POINT('Ctrl Pts',(1.88681306678638,-4.73341669344416,32.9117328798396));
#39145=CARTESIAN_POINT('Ctrl Pts',(3.92095457674023,-3.25444501411708,32.991104769893));
#39146=CARTESIAN_POINT('Ctrl Pts',(4.99996023068588,-0.982697732942914,
33.0704766599464));
#39147=CARTESIAN_POINT('Ctrl Pts',(4.8609866396607,1.52843254081155,33.1498485499997));
#39148=CARTESIAN_POINT('Ctrl Pts',(3.53788746282564,3.66724003075238,33.2292204400532));
#39149=CARTESIAN_POINT('Ctrl Pts',(1.35296673102733,4.91271596650007,33.3085923301066));
#39150=CARTESIAN_POINT('Ctrl Pts',(-1.16153370170815,4.96146516692072,33.38796422016));
#39151=CARTESIAN_POINT('Ctrl Pts',(-3.39308709571883,3.80161243469636,33.4673361102134));
#39152=CARTESIAN_POINT('Ctrl Pts',(-4.79809198368328,1.71569532810634,33.5467080002668));
#39153=CARTESIAN_POINT('Ctrl Pts',(-5.03429228481892,-0.788161362783202,
33.6260798903202));
#39154=CARTESIAN_POINT('Ctrl Pts',(-4.04415012858963,-3.10002369026433,
33.7054517803737));
#39155=CARTESIAN_POINT('Ctrl Pts',(-2.06886195261037,-4.65672710858312,
33.784823670427));
#39156=CARTESIAN_POINT('Ctrl Pts',(0.41039641567654,-5.07906211074165,33.8641955604805));
#39157=CARTESIAN_POINT('Ctrl Pts',(2.78968312550164,-4.26414882503682,33.9435674505338));
#39158=CARTESIAN_POINT('Ctrl Pts',(4.48940920081343,-2.41049832408638,34.0229393405872));
#39159=CARTESIAN_POINT('Ctrl Pts',(5.09552513194581,0.0303442330639926,
34.1023112306406));
#39160=CARTESIAN_POINT('Ctrl Pts',(4.46038241968974,2.46379500220581,34.181683120694));
#39161=CARTESIAN_POINT('Ctrl Pts',(2.73870042288625,4.29707076232801,34.2610550107475));
#39162=CARTESIAN_POINT('Ctrl Pts',(0.349877065078239,5.0835895961519,34.3404269008008));
#39163=CARTESIAN_POINT('Ctrl Pts',(-2.1241755713431,4.63175725668789,34.4197987908543));
#39164=CARTESIAN_POINT('Ctrl Pts',(-4.08078374036812,3.05163910171546,34.4991706809076));
#39165=CARTESIAN_POINT('Ctrl Pts',(-5.04332202290104,0.728148416253786,
34.5785425709611));
#39166=CARTESIAN_POINT('Ctrl Pts',(-4.77731822385925,-1.77271761167814,
34.6579144610144));
#39167=CARTESIAN_POINT('Ctrl Pts',(-3.3475702798999,-3.84175355324914,34.7372863510679));
#39168=CARTESIAN_POINT('Ctrl Pts',(-1.10236162547809,-4.97494683282594,
34.8166582411212));
#39169=CARTESIAN_POINT('Ctrl Pts',(1.41137988087415,-4.8962540757844,34.8960301311747));
#39170=CARTESIAN_POINT('Ctrl Pts',(3.58131237228184,-3.62484466355631,34.9754020212281));
#39171=CARTESIAN_POINT('Ctrl Pts',(4.87884509690211,-1.47043111474347,35.0547739112815));
#39172=CARTESIAN_POINT('Ctrl Pts',(4.98790195505749,1.04217619887681,35.1341458013349));
#39173=CARTESIAN_POINT('Ctrl Pts',(3.88191693749454,3.3009116972686,35.2135176913883));
#39174=CARTESIAN_POINT('Ctrl Pts',(1.8303055464353,4.75555241264984,35.2928895814417));
#39175=CARTESIAN_POINT('Ctrl Pts',(-0.667164224422912,5.05175108654629,
35.3722614714951));
#39176=CARTESIAN_POINT('Ctrl Pts',(-3.00211426695468,4.11735437762148,35.4516333615485));
#39177=CARTESIAN_POINT('Ctrl Pts',(-4.60575591912355,2.17997925591738,35.5310052516019));
#39178=CARTESIAN_POINT('Ctrl Pts',(-5.08744562406171,-0.288433987225976,
35.6103771416553));
#39179=CARTESIAN_POINT('Ctrl Pts',(-4.32984483584829,-2.68658534951887,
35.6897490317088));
#39180=CARTESIAN_POINT('Ctrl Pts',(-2.51750342957125,-4.43029046732475,
35.7691209217621));
#39181=CARTESIAN_POINT('Ctrl Pts',(-0.0919037602499935,-5.09478663357195,
35.8484928118156));
#39182=CARTESIAN_POINT('Ctrl Pts',(2.35608346164268,-4.51820405299999,35.9278647018689));
#39183=CARTESIAN_POINT('Ctrl Pts',(4.23013396738149,-2.84099696599223,36.0072365919223));
#39184=CARTESIAN_POINT('Ctrl Pts',(5.07373320190884,-0.471729306508876,
36.0866084819757));
#39185=CARTESIAN_POINT('Ctrl Pts',(4.68138225896918,2.01245056788487,36.1659803720291));
#39186=CARTESIAN_POINT('Ctrl Pts',(3.14865695980852,4.00640193842567,36.2453522620825));
#39187=CARTESIAN_POINT('Ctrl Pts',(0.84892579467244,5.02440266478627,36.3247241521359));
#39188=CARTESIAN_POINT('Ctrl Pts',(-1.65760181498048,4.81847002333159,36.4040960421893));
#39189=CARTESIAN_POINT('Ctrl Pts',(-3.76034129154353,3.43876874969578,36.4834679322427));
#39190=CARTESIAN_POINT('Ctrl Pts',(-4.94706995286084,1.22139102021962,36.5628398222961));
#39191=CARTESIAN_POINT('Ctrl Pts',(-4.92870332381484,-1.2935148582789,36.6422117123495));
#39192=CARTESIAN_POINT('Ctrl Pts',(-3.70971547458727,-3.49332338044723,
36.721583602403));
#39193=CARTESIAN_POINT('Ctrl Pts',(-1.58704914706622,-4.84216605947875,
36.8009554924563));
#39194=CARTESIAN_POINT('Ctrl Pts',(0.922218839806455,-5.01146780437405,
36.8803273825098));
#39195=CARTESIAN_POINT('Ctrl Pts',(3.20683635859905,-3.95998708481968,36.9596992725631));
#39196=CARTESIAN_POINT('Ctrl Pts',(4.71027563864883,-1.94386227668601,37.0390711626166));
#39197=CARTESIAN_POINT('Ctrl Pts',(5.06630219914206,0.545783079382256,37.1184430526699));
#39198=CARTESIAN_POINT('Ctrl Pts',(4.18818875799396,2.90247688538333,37.1978149427234));
#39199=CARTESIAN_POINT('Ctrl Pts',(2.28984180579711,4.55213374662869,37.2771868327768));
#39200=CARTESIAN_POINT('Ctrl Pts',(-0.1663055418131,5.0929009031723,37.3565587228302));
#39201=CARTESIAN_POINT('Ctrl Pts',(-2.58194122754862,4.39304867264833,37.4359306128836));
#39202=CARTESIAN_POINT('Ctrl Pts',(-4.36862174528344,2.62305950931498,37.515302502937));
#39203=CARTESIAN_POINT('Ctrl Pts',(-5.09111567564704,0.214098855557291,
37.5946743929904));
#39204=CARTESIAN_POINT('Ctrl Pts',(-4.57342509641719,-2.24701580551625,
37.6740462830439));
#39205=CARTESIAN_POINT('Ctrl Pts',(-2.94165828680345,-4.16076239004767,
37.7534181730971));
#39206=CARTESIAN_POINT('Ctrl Pts',(-0.593310029777194,-5.06095646606148,
37.8327900631507));
#39207=CARTESIAN_POINT('Ctrl Pts',(1.89956723723832,-4.72831274916718,37.912161953204));
#39208=CARTESIAN_POINT('Ctrl Pts',(3.92971412987383,-3.2438625125424,37.9915338432574));
#39209=CARTESIAN_POINT('Ctrl Pts',(5.00259135876467,-0.969214547985126,
38.0709057333108));
#39210=CARTESIAN_POINT('Ctrl Pts',(4.85684840567486,1.54153193505625,38.1502776233642));
#39211=CARTESIAN_POINT('Ctrl Pts',(3.52798793147795,3.67676465100168,38.2296495134176));
#39212=CARTESIAN_POINT('Ctrl Pts',(1.3397174061215,4.91634563604017,38.309021403471));
#39213=CARTESIAN_POINT('Ctrl Pts',(-1.17490531372475,4.95831570685867,38.3883932935245));
#39214=CARTESIAN_POINT('Ctrl Pts',(-3.40332370018554,3.79245104545026,38.4677651835778));
#39215=CARTESIAN_POINT('Ctrl Pts',(-4.80269996560014,1.70275370586069,38.5471370736313));
#39216=CARTESIAN_POINT('Ctrl Pts',(-5.03214915152033,-0.801730671351773,
38.6265089636846));
#39217=CARTESIAN_POINT('Ctrl Pts',(-4.03577793971505,-3.11091522434137,
38.705880853738));
#39218=CARTESIAN_POINT('Ctrl Pts',(-2.05630016029208,-4.6622877283261,38.7852527437914));
#39219=CARTESIAN_POINT('Ctrl Pts',(0.424087796933226,-5.0779372355256,38.8646246338449));
#39220=CARTESIAN_POINT('Ctrl Pts',(2.80116888608276,-4.2566125209993,38.9439965238982));
#39221=CARTESIAN_POINT('Ctrl Pts',(4.49589147158116,-2.39838632564053,39.0233684139517));
#39222=CARTESIAN_POINT('Ctrl Pts',(5.09542477676094,0.0440812951169324,
39.1027403040051));
#39223=CARTESIAN_POINT('Ctrl Pts',(4.45372401575944,2.47581113999364,39.1821121940585));
#39224=CARTESIAN_POINT('Ctrl Pts',(2.72710569549243,4.30443824810521,39.2614840841118));
#39225=CARTESIAN_POINT('Ctrl Pts',(0.336170930870647,5.08451490337722,39.3408559741653));
#39226=CARTESIAN_POINT('Ctrl Pts',(-2.1366552096739,4.62601276074587,39.4202278642187));
#39227=CARTESIAN_POINT('Ctrl Pts',(-4.08899520654064,3.04062834435872,39.4995997542721));
#39228=CARTESIAN_POINT('Ctrl Pts',(-5.04526816392185,0.714545672092809,
39.5789716443255));
#39229=CARTESIAN_POINT('Ctrl Pts',(-4.77251903131803,-1.78558378675053,
39.6583435343789));
#39230=CARTESIAN_POINT('Ctrl Pts',(-3.33720602914116,-3.85077723115716,
39.7377154244323));
#39231=CARTESIAN_POINT('Ctrl Pts',(-1.08893586889047,-4.97787652885981,
39.8170873144857));
#39232=CARTESIAN_POINT('Ctrl Pts',(1.42455668503583,-4.8924768895782,39.8964592045391));
#39233=CARTESIAN_POINT('Ctrl Pts',(3.59110607910284,-3.61508997874913,39.9758310945925));
#39234=CARTESIAN_POINT('Ctrl Pts',(4.88272528059762,-1.45743906270703,40.0552029846459));
#39235=CARTESIAN_POINT('Ctrl Pts',(4.98521092249161,1.05595859527154,40.1345748746994));
#39236=CARTESIAN_POINT('Ctrl Pts',(4.2435173595031,2.5590120913109,40.1874894680683));
#39237=CARTESIAN_POINT('Ctrl Pts',(3.71544298812202,3.17665283523806,40.2139467647527));
#39238=CARTESIAN_POINT('Ctrl Pts',(1.21713437249832,-4.5428082122986,-0.213946764752702));
#39239=CARTESIAN_POINT('Ctrl Pts',(1.97231308274437,-4.34047654372165,-0.187489468068234));
#39240=CARTESIAN_POINT('Ctrl Pts',(3.37906911267772,-3.55219315325666,-0.134574874699299));
#39241=CARTESIAN_POINT('Ctrl Pts',(4.66642692152752,-1.5028536385038,-0.055202984645895));
#39242=CARTESIAN_POINT('Ctrl Pts',(4.81689062664967,0.911851793295018,0.0241689054075086));
#39243=CARTESIAN_POINT('Ctrl Pts',(3.79405383067521,3.10479958283122,0.103540795460912));
#39244=CARTESIAN_POINT('Ctrl Pts',(1.84695009786499,4.54123256689918,0.182912685514316));
#39245=CARTESIAN_POINT('Ctrl Pts',(-0.550043424514128,4.8715330414348,0.26228457556772));
#39246=CARTESIAN_POINT('Ctrl Pts',(-2.81305984991034,4.01508502497055,0.341656465621123));
#39247=CARTESIAN_POINT('Ctrl Pts',(-4.39081462818011,2.18059968579164,0.421028355674527));
#39248=CARTESIAN_POINT('Ctrl Pts',(-4.89898012125377,-0.18509000454136,
0.500400245727931));
#39249=CARTESIAN_POINT('Ctrl Pts',(-4.21376307902768,-2.5056841854766,0.579772135781334));
#39250=CARTESIAN_POINT('Ctrl Pts',(-2.50208364241389,-4.21590347870479,
0.659144025834738));
#39251=CARTESIAN_POINT('Ctrl Pts',(-0.180901657890204,-4.89913577411436,
0.738515915888141));
#39252=CARTESIAN_POINT('Ctrl Pts',(2.18434729950923,-4.38895062645432,0.817887805941546));
#39253=CARTESIAN_POINT('Ctrl Pts',(4.01749423301245,-2.8096261920884,0.897259695994948));
#39254=CARTESIAN_POINT('Ctrl Pts',(4.87198838803769,-0.545883369388664,
0.976631586048353));
#39255=CARTESIAN_POINT('Ctrl Pts',(4.53967699589134,1.85083561019003,1.05600347610176));
#39256=CARTESIAN_POINT('Ctrl Pts',(3.10151031466513,3.79669503846566,1.13537536615516));
#39257=CARTESIAN_POINT('Ctrl Pts',(0.907822597135906,4.81768800868641,1.21474725620856));
#39258=CARTESIAN_POINT('Ctrl Pts',(-1.50700870159448,4.66510281756135,1.29411914626197));
#39259=CARTESIAN_POINT('Ctrl Pts',(-3.55473601316185,3.37610891998462,1.37349103631537));
#39260=CARTESIAN_POINT('Ctrl Pts',(-4.73653750187219,1.26470235504102,1.45286292636877));
#39261=CARTESIAN_POINT('Ctrl Pts',(-4.76452893838759,-1.15478290032736,
1.53223481642218));
#39262=CARTESIAN_POINT('Ctrl Pts',(-3.63189167208734,-3.29296559930584,
1.61160670647558));
#39263=CARTESIAN_POINT('Ctrl Pts',(-1.61453363327375,-4.62898916605748,
1.69097859652899));
#39264=CARTESIAN_POINT('Ctrl Pts',(0.796121224764031,-4.8374012186294,1.77035048658239));
#39265=CARTESIAN_POINT('Ctrl Pts',(3.01284271470348,-3.86743304144296,1.8497223766358));
#39266=CARTESIAN_POINT('Ctrl Pts',(4.49564238811846,-1.95536673594104,1.92909426668919));
#39267=CARTESIAN_POINT('Ctrl Pts',(4.88331352674298,0.433022578391154,2.0084661567426));
#39268=CARTESIAN_POINT('Ctrl Pts',(4.08142029927371,2.71592855106099,2.087838046796));
#39269=CARTESIAN_POINT('Ctrl Pts',(2.28530212097744,4.33724034032234,2.16720993684941));
#39270=CARTESIAN_POINT('Ctrl Pts',(-0.067510595561391,4.90200998298708,
2.24658182690281));
#39271=CARTESIAN_POINT('Ctrl Pts',(-2.4038778804521,4.27266084421796,2.32595371695622));
#39272=CARTESIAN_POINT('Ctrl Pts',(-4.15466583455893,2.60250098116813,2.40532560700962));
#39273=CARTESIAN_POINT('Ctrl Pts',(-4.8933863875636,0.298377639645852,2.48469749706302));
#39274=CARTESIAN_POINT('Ctrl Pts',(-4.44008884788507,-2.07842983444745,
2.56406938711643));
#39275=CARTESIAN_POINT('Ctrl Pts',(-2.90519549283157,-3.94893640139523,
2.64344127716983));
#39276=CARTESIAN_POINT('Ctrl Pts',(-0.662602946265526,-4.85749080178588,
2.72281316722323));
#39277=CARTESIAN_POINT('Ctrl Pts',(1.7413982113641,-4.58277119473486,2.80218505727664));
#39278=CARTESIAN_POINT('Ctrl Pts',(3.72119861922498,-3.19169866843848,2.88155694733003));
#39279=CARTESIAN_POINT('Ctrl Pts',(4.79452328017608,-1.02313541121562,2.96092883738345));
#39280=CARTESIAN_POINT('Ctrl Pts',(4.69991268257356,1.39466136750753,3.04030072743684));
#39281=CARTESIAN_POINT('Ctrl Pts',(3.46041375857639,3.47272172413642,3.11967261749026));
#39282=CARTESIAN_POINT('Ctrl Pts',(1.37796570248595,4.70483475550482,3.19904450754365));
#39283=CARTESIAN_POINT('Ctrl Pts',(-1.04015174865471,4.79086045440737,3.27841639759706));
#39284=CARTESIAN_POINT('Ctrl Pts',(-3.20489053615995,3.70984315100601,3.35778828765046));
#39285=CARTESIAN_POINT('Ctrl Pts',(-4.5889250829615,1.72511626761812,3.43716017770387));
#39286=CARTESIAN_POINT('Ctrl Pts',(-4.85510763696699,-0.679845120081458,
3.51653206775727));
#39287=CARTESIAN_POINT('Ctrl Pts',(-3.9385967172058,-2.91919774134084,3.59590395781068));
#39288=CARTESIAN_POINT('Ctrl Pts',(-2.06265235506924,-4.44744025434419,
3.67527584786408));
#39289=CARTESIAN_POINT('Ctrl Pts',(0.315749555158651,-4.89229616563132,
3.75464773791748));
#39290=CARTESIAN_POINT('Ctrl Pts',(2.61723557264967,-4.14539955988454,3.83401962797088));
#39291=CARTESIAN_POINT('Ctrl Pts',(4.2811687977959,-2.38869279703619,3.91339151802429));
#39292=CARTESIAN_POINT('Ctrl Pts',(4.90221878000547,-0.0501057561116431,
3.99276340807769));
#39293=CARTESIAN_POINT('Ctrl Pts',(4.32909911828292,2.3006869360945,4.0721352981311));
#39294=CARTESIAN_POINT('Ctrl Pts',(2.701420493645,4.09103738315217,4.1515071881845));
#39295=CARTESIAN_POINT('Ctrl Pts',(0.415681816248014,4.88482017903163,4.2308790782379));
#39296=CARTESIAN_POINT('Ctrl Pts',(-1.97131603149091,4.48867159166503,4.31025096829131));
#39297=CARTESIAN_POINT('Ctrl Pts',(-3.87810565739265,2.9990925400749,4.38962285834471));
#39298=CARTESIAN_POINT('Ctrl Pts',(-4.84019732919483,0.778941184101248,
4.46899474839812));
#39299=CARTESIAN_POINT('Ctrl Pts',(-4.62322764520021,-1.63095852016239,
4.54836663845152));
#39300=CARTESIAN_POINT('Ctrl Pts',(-3.28004994017564,-3.64356033897994,
4.62773852850492));
#39301=CARTESIAN_POINT('Ctrl Pts',(-1.13785932999167,-4.76859892410598,
4.70711041855833));
#39302=CARTESIAN_POINT('Ctrl Pts',(1.28151129436936,-4.73201736643448,4.78648230861172));
#39303=CARTESIAN_POINT('Ctrl Pts',(3.38870860399915,-3.54272685244233,4.86585419866514));
#39304=CARTESIAN_POINT('Ctrl Pts',(4.67042399847401,-1.4904359188881,4.94522608871853));
#39305=CARTESIAN_POINT('Ctrl Pts',(4.81443444472878,0.924921905483315,5.02459797877194));
#39306=CARTESIAN_POINT('Ctrl Pts',(3.78565931681752,3.1149708009589,5.10396986882535));
#39307=CARTESIAN_POINT('Ctrl Pts',(1.83470595874426,4.54621970419184,5.18334175887875));
#39308=CARTESIAN_POINT('Ctrl Pts',(-0.563177709826337,4.87001955037026,
5.26271364893215));
#39309=CARTESIAN_POINT('Ctrl Pts',(-2.82387253485596,4.00749341368393,5.34208553898556));
#39310=CARTESIAN_POINT('Ctrl Pts',(-4.39667826093048,2.1687507518604,5.42145742903895));
#39311=CARTESIAN_POINT('Ctrl Pts',(-4.89846289452463,-0.198294792667946,
5.50082931909237));
#39312=CARTESIAN_POINT('Ctrl Pts',(-4.20699280957627,-2.51703616462048,
5.58020120914576));
#39313=CARTESIAN_POINT('Ctrl Pts',(-2.49070858823577,-4.2226330982365,5.65957309919917));
#39314=CARTESIAN_POINT('Ctrl Pts',(-0.16769326789098,-4.89960595576194,
5.73894498925257));
#39315=CARTESIAN_POINT('Ctrl Pts',(2.19617176132931,-4.38304564755759,5.81831687930597));
#39316=CARTESIAN_POINT('Ctrl Pts',(4.0250542106335,-2.7987851213152,5.89768876935939));
#39317=CARTESIAN_POINT('Ctrl Pts',(4.87344236353376,-0.532746734526196,
5.97706065941277));
#39318=CARTESIAN_POINT('Ctrl Pts',(4.53467074385888,1.86306757757847,6.05643254946619));
#39319=CARTESIAN_POINT('Ctrl Pts',(3.09126336830344,3.80504275161517,6.13580443951959));
#39320=CARTESIAN_POINT('Ctrl Pts',(0.894831078624676,4.82011793367768,6.215176329573));
#39321=CARTESIAN_POINT('Ctrl Pts',(-1.51958008113206,4.6610230562464,6.2945482196264));
#39322=CARTESIAN_POINT('Ctrl Pts',(-3.56382489665849,3.36651327931302,6.3739201096798));
#39323=CARTESIAN_POINT('Ctrl Pts',(-4.73992985575151,1.25192831918974,6.45329199973321));
#39324=CARTESIAN_POINT('Ctrl Pts',(-4.76139839364024,-1.16762360839183,
6.53266388978661));
#39325=CARTESIAN_POINT('Ctrl Pts',(-3.62300082201479,-3.30274500946015,
6.61203577984002));
#39326=CARTESIAN_POINT('Ctrl Pts',(-1.60204826952283,-4.63332503672608,
6.69140766989341));
#39327=CARTESIAN_POINT('Ctrl Pts',(0.809159695351183,-4.83523734073654,
6.77077955994682));
#39328=CARTESIAN_POINT('Ctrl Pts',(3.02325814948227,-3.8592965311599,6.85015145000022));
#39329=CARTESIAN_POINT('Ctrl Pts',(4.50089761026788,-1.94323962900068,6.92952334005363));
#39330=CARTESIAN_POINT('Ctrl Pts',(4.8821283757601,0.446186145495144,7.00889523010703));
#39331=CARTESIAN_POINT('Ctrl Pts',(4.07408347532503,2.72692196256463,7.08826712016044));
#39332=CARTESIAN_POINT('Ctrl Pts',(2.27360085813158,4.34338562549276,7.16763901021384));
#39333=CARTESIAN_POINT('Ctrl Pts',(-0.0807258955725768,4.90181016397186,
7.24701090026724));
#39334=CARTESIAN_POINT('Ctrl Pts',(-2.41538799979899,4.26616459648018,7.32638279032065));
#39335=CARTESIAN_POINT('Ctrl Pts',(-4.16166693364502,2.59129077628108,7.40575468037405));
#39336=CARTESIAN_POINT('Ctrl Pts',(-4.89417301414864,0.285184258704783,
7.48512657042745));
#39337=CARTESIAN_POINT('Ctrl Pts',(-4.43446938147388,-2.09039251304738,
7.56449846048085));
#39338=CARTESIAN_POINT('Ctrl Pts',(-2.89453882300355,-3.95675429562653,
7.64387035053426));
#39339=CARTESIAN_POINT('Ctrl Pts',(-0.649505014202585,-4.85925948991814,
7.72324224058766));
#39340=CARTESIAN_POINT('Ctrl Pts',(1.75374677840318,-4.57805982825413,7.80261413064107));
#39341=CARTESIAN_POINT('Ctrl Pts',(3.72978973764259,-3.18165492579096,7.88198602069447));
#39342=CARTESIAN_POINT('Ctrl Pts',(4.79726417254181,-1.01020592587881,7.96135791074788));
#39343=CARTESIAN_POINT('Ctrl Pts',(4.69613567357394,1.40732700152449,8.04072980080128));
#39344=CARTESIAN_POINT('Ctrl Pts',(3.45103891924351,3.48203818642192,8.12010169085468));
#39345=CARTESIAN_POINT('Ctrl Pts',(1.36527672293039,4.70853257646778,8.19947358090808));
#39346=CARTESIAN_POINT('Ctrl Pts',(-1.05306386109979,4.78803885304614,8.2788454709615));
#39347=CARTESIAN_POINT('Ctrl Pts',(-3.21488041948337,3.7011894631667,8.35821736101489));
#39348=CARTESIAN_POINT('Ctrl Pts',(-4.5935592236979,1.7127385125038,8.4375892510683));
#39349=CARTESIAN_POINT('Ctrl Pts',(-4.85325716869052,-0.692931748722623,
8.51696114112171));
#39350=CARTESIAN_POINT('Ctrl Pts',(-3.93071240989269,-2.92980536973865,
8.59633303117509));
#39351=CARTESIAN_POINT('Ctrl Pts',(-2.05065480852931,-4.45298488770055,
8.67570492122852));
#39352=CARTESIAN_POINT('Ctrl Pts',(0.328937765144378,-4.89142714353344,
8.7550768112819));
#39353=CARTESIAN_POINT('Ctrl Pts',(2.62840182732027,-4.1383285741919,8.83444870133532));
#39354=CARTESIAN_POINT('Ctrl Pts',(4.28759302222971,-2.37714232421218,8.91382059138872));
#39355=CARTESIAN_POINT('Ctrl Pts',(4.90233604735019,-0.0368894657696129,
8.99319248144213));
#39356=CARTESIAN_POINT('Ctrl Pts',(4.32288086247292,2.31234958488097,9.07256437149553));
#39357=CARTESIAN_POINT('Ctrl Pts',(2.69038146803174,4.09830539495352,9.15193626154892));
#39358=CARTESIAN_POINT('Ctrl Pts',(0.402511103036409,4.88592308226053,9.23130815160233));
#39359=CARTESIAN_POINT('Ctrl Pts',(-1.9834100757154,4.48334072153617,9.31068004165575));
#39360=CARTESIAN_POINT('Ctrl Pts',(-3.88617695022667,2.98862648475194,9.39005193170914));
#39361=CARTESIAN_POINT('Ctrl Pts',(-4.84227972156947,0.765889451494674,
9.46942382176256));
#39362=CARTESIAN_POINT('Ctrl Pts',(-4.61881387094234,-1.64341655687914,
9.54879571181594));
#39363=CARTESIAN_POINT('Ctrl Pts',(-3.27021518492473,-3.65238992963806,
9.62816760186936));
#39364=CARTESIAN_POINT('Ctrl Pts',(-1.124999318358,-4.77164919996512,9.70753949192275));
#39365=CARTESIAN_POINT('Ctrl Pts',(1.29426389201697,-4.72854528704705,9.78691138197616));
#39366=CARTESIAN_POINT('Ctrl Pts',(3.39824728310117,-3.53357820866179,9.86628327202957));
#39367=CARTESIAN_POINT('Ctrl Pts',(4.67442515791466,-1.4778393000892,9.94565516208296));
#39368=CARTESIAN_POINT('Ctrl Pts',(4.81192341092478,0.937897990843289,10.0250270521364));
#39369=CARTESIAN_POINT('Ctrl Pts',(3.7772477720454,3.12516540720838,10.1043989421898));
#39370=CARTESIAN_POINT('Ctrl Pts',(1.82244293669188,4.55114944781378,10.1837708322432));
#39371=CARTESIAN_POINT('Ctrl Pts',(-0.576304964130747,4.86848355673017,
10.2631427222966));
#39372=CARTESIAN_POINT('Ctrl Pts',(-2.83466625132052,3.99986584743267,10.34251461235));
#39373=CARTESIAN_POINT('Ctrl Pts',(-4.40250911411597,2.15688967125344,10.4218865024034));
#39374=CARTESIAN_POINT('Ctrl Pts',(-4.89791050150136,-0.211500054648842,
10.5012583924568));
#39375=CARTESIAN_POINT('Ctrl Pts',(-4.20019173206204,-2.52836883538606,
10.5806302825102));
#39376=CARTESIAN_POINT('Ctrl Pts',(-2.47931555365911,-4.22933256427274,
10.6600021725636));
#39377=CARTESIAN_POINT('Ctrl Pts',(-0.154483594256702,-4.90004024197143,
10.739374062617));
#39378=CARTESIAN_POINT('Ctrl Pts',(2.20798022676301,-4.37710896278096,10.8187459526704));
#39379=CARTESIAN_POINT('Ctrl Pts',(4.03258495182456,-2.7879236288234,10.8981178427238));
#39380=CARTESIAN_POINT('Ctrl Pts',(4.87486090859705,-0.519606269848766,
10.9774897327772));
#39381=CARTESIAN_POINT('Ctrl Pts',(4.52963153835691,1.87528602633207,11.0568616228306));
#39382=CARTESIAN_POINT('Ctrl Pts',(3.08099395154235,3.81336279737362,11.136233512884));
#39383=CARTESIAN_POINT('Ctrl Pts',(0.881833057796546,4.82251283171035,11.2156054029374));
#39384=CARTESIAN_POINT('Ctrl Pts',(-1.53214041692415,4.65690941469354,11.2949772929908));
#39385=CARTESIAN_POINT('Ctrl Pts',(-3.5728878774174,3.35689317215153,11.3743491830443));
#39386=CARTESIAN_POINT('Ctrl Pts',(-4.74328775942496,1.23914518323042,11.4537210730976));
#39387=CARTESIAN_POINT('Ctrl Pts',(-4.75823324232597,-1.1804558295243,11.533092963151));
#39388=CARTESIAN_POINT('Ctrl Pts',(-3.614083639567,-3.31250041510156,11.6124648532044));
#39389=CARTESIAN_POINT('Ctrl Pts',(-1.58955126184795,-4.63762723165536,
11.6918367432579));
#39390=CARTESIAN_POINT('Ctrl Pts',(0.822192284845203,-4.83303831979168,
11.7712086333112));
#39391=CARTESIAN_POINT('Ctrl Pts',(3.03365161084184,-3.85113197097562,11.8505805233647));
#39392=CARTESIAN_POINT('Ctrl Pts',(4.50612011931135,-1.9310983983659,11.9299524134181));
#39393=CARTESIAN_POINT('Ctrl Pts',(4.88090774084429,0.459346469671929,12.0093243034715));
#39394=CARTESIAN_POINT('Ctrl Pts',(4.06671704041361,2.73789555444384,12.0886961935249));
#39395=CARTESIAN_POINT('Ctrl Pts',(2.26188307046365,4.34949934238227,12.1680680835783));
#39396=CARTESIAN_POINT('Ctrl Pts',(-0.0939406088580155,4.90157471796985,
12.2474399736317));
#39397=CARTESIAN_POINT('Ctrl Pts',(-2.42688056379585,4.25963734171157,12.3268118636851));
#39398=CARTESIAN_POINT('Ctrl Pts',(-4.16863778520202,2.58006173755973,12.4061837537385));
#39399=CARTESIAN_POINT('Ctrl Pts',(-4.89492406925624,0.271988805008134,
12.4855556437919));
#39400=CARTESIAN_POINT('Ctrl Pts',(-4.4288176847703,-2.10233999840645,12.5649275338453));
#39401=CARTESIAN_POINT('Ctrl Pts',(-2.88386111529598,-3.96454343165991,
12.6442994238987));
#39402=CARTESIAN_POINT('Ctrl Pts',(-0.636402361453836,-4.86099286032903,
12.7236713139521));
#39403=CARTESIAN_POINT('Ctrl Pts',(1.76608259898569,-4.57331518784718,12.8030432040055));
#39404=CARTESIAN_POINT('Ctrl Pts',(3.73835374746984,-3.17158805846724,12.8824150940589));
#39405=CARTESIAN_POINT('Ctrl Pts',(4.79997019777602,-0.997269098235751,
12.9617869841123));
#39406=CARTESIAN_POINT('Ctrl Pts',(4.69232453245774,1.41998240690827,13.0411588741657));
#39407=CARTESIAN_POINT('Ctrl Pts',(3.44163899731696,3.49132934080715,13.1205307642191));
#39408=CARTESIAN_POINT('Ctrl Pts',(1.35257782036847,4.71219617521183,13.1999026542725));
#39409=CARTESIAN_POINT('Ctrl Pts',(-1.06596831974157,4.78518245160425,13.2792745443259));
#39410=CARTESIAN_POINT('Ctrl Pts',(-3.22484693664342,3.69250887460753,13.3586464343793));
#39411=CARTESIAN_POINT('Ctrl Pts',(-4.59815997785652,1.70034830898619,13.4380183244327));
#39412=CARTESIAN_POINT('Ctrl Pts',(-4.85137142631828,-0.706013341047003,
13.5173902144861));
#39413=CARTESIAN_POINT('Ctrl Pts',(-3.92279953365742,-2.94039170393519,
13.5967621045396));
#39414=CARTESIAN_POINT('Ctrl Pts',(-2.03864235756713,-4.45849715619141,
13.6761339945929));
#39415=CARTESIAN_POINT('Ctrl Pts',(0.342123584368241,-4.8905225699155,13.7555058846463));
#39416=CARTESIAN_POINT('Ctrl Pts',(2.63954897842921,-4.13122751059623,13.8348777746997));
#39417=CARTESIAN_POINT('Ctrl Pts',(4.29398608388735,-2.36557457401273,13.9142496647532));
#39418=CARTESIAN_POINT('Ctrl Pts',(4.90241768388754,-0.0236729073102294,
13.9936215548065));
#39419=CARTESIAN_POINT('Ctrl Pts',(4.31663118741021,2.32399542721397,14.07299344486));
#39420=CARTESIAN_POINT('Ctrl Pts',(2.67932288838078,4.10554361974547,14.1523653349134));
#39421=CARTESIAN_POINT('Ctrl Pts',(0.389337464322444,4.8869904739736,14.2317372249668));
#39422=CARTESIAN_POINT('Ctrl Pts',(-1.99548970426098,4.47797726591172,14.3111091150202));
#39423=CARTESIAN_POINT('Ctrl Pts',(-3.894219997828,2.97813870770829,14.3904810050736));
#39424=CARTESIAN_POINT('Ctrl Pts',(-4.84432691963384,0.752832152305313,
14.469852895127));
#39425=CARTESIAN_POINT('Ctrl Pts',(-4.61436652655265,-1.6558626490335,14.5492247851804));
#39426=CARTESIAN_POINT('Ctrl Pts',(-3.26035666133029,-3.66119297425757,
14.6285966752338));
#39427=CARTESIAN_POINT('Ctrl Pts',(-1.11213113008494,-4.77466479486569,
14.7079685652872));
#39428=CARTESIAN_POINT('Ctrl Pts',(1.30700708278859,-4.72503883998578,14.7873404553406));
#39429=CARTESIAN_POINT('Ctrl Pts',(3.40776126330594,-3.52440388238144,14.866712345394));
#39430=CARTESIAN_POINT('Ctrl Pts',(4.67839234303357,-1.46523194016464,14.9460842354474));
#39431=CARTESIAN_POINT('Ctrl Pts',(4.80937740344404,0.95086725944037,15.0254561255008));
#39432=CARTESIAN_POINT('Ctrl Pts',(3.76880877375186,3.13533729935469,15.1048280155542));
#39433=CARTESIAN_POINT('Ctrl Pts',(1.81016666889045,4.55604611309762,15.1841999056076));
#39434=CARTESIAN_POINT('Ctrl Pts',(-0.58942802977675,4.86691217832697,15.263571795661));
#39435=CARTESIAN_POINT('Ctrl Pts',(-2.84543936506709,3.99220920964323,15.3429436857144));
#39436=CARTESIAN_POINT('Ctrl Pts',(-4.40830796930035,2.14501291409566,15.4223155757678));
#39437=CARTESIAN_POINT('Ctrl Pts',(-4.89732250983615,-0.224703779420184,
15.5016874658212));
#39438=CARTESIAN_POINT('Ctrl Pts',(-4.19336012701549,-2.53968312964247,
15.5810593558746));
#39439=CARTESIAN_POINT('Ctrl Pts',(-2.46790449909881,-4.23600129097741,
15.6604312459281));
#39440=CARTESIAN_POINT('Ctrl Pts',(-0.141272797816101,-4.90043891405947,
15.7398031359814));
#39441=CARTESIAN_POINT('Ctrl Pts',(2.21977264431347,-4.37114046461536,15.8191750260349));
#39442=CARTESIAN_POINT('Ctrl Pts',(4.04008638367001,-2.77704187334405,15.8985469160882));
#39443=CARTESIAN_POINT('Ctrl Pts',(4.87624402254724,-0.50646202860824,15.9779188061417));
#39444=CARTESIAN_POINT('Ctrl Pts',(4.52455941090906,1.88749084526974,16.057290696195));
#39445=CARTESIAN_POINT('Ctrl Pts',(3.0707021417271,3.82165512711525,16.1366625862485));
#39446=CARTESIAN_POINT('Ctrl Pts',(0.868828627683026,4.82487267911372,16.2160344763019));
#39447=CARTESIAN_POINT('Ctrl Pts',(-1.54468961690488,4.65276192610161,16.2954063663553));
#39448=CARTESIAN_POINT('Ctrl Pts',(-3.58192489000319,3.34724866670505,16.3747782564087));
#39449=CARTESIAN_POINT('Ctrl Pts',(-4.74661118820951,1.22635304091943,16.4541501464621));
#39450=CARTESIAN_POINT('Ctrl Pts',(-4.75503350768456,-1.19327947079094,
16.5335220365155));
#39451=CARTESIAN_POINT('Ctrl Pts',(-3.60514018926425,-3.32223174536968,
16.6128939265689));
#39452=CARTESIAN_POINT('Ctrl Pts',(-1.57704270154751,-4.64189571913949,
16.6922658166223));
#39453=CARTESIAN_POINT('Ctrl Pts',(0.835218899365215,-4.83080417279076,
16.7716377066757));
#39454=CARTESIAN_POINT('Ctrl Pts',(3.04402302167444,-3.84293941821851,16.8510095967291));
#39455=CARTESIAN_POINT('Ctrl Pts',(4.5113098802371,-1.91894313613405,16.9303814867825));
#39456=CARTESIAN_POINT('Ctrl Pts',(4.87965162531072,0.47250346257415,17.0097533768359));
#39457=CARTESIAN_POINT('Ctrl Pts',(4.05932105856824,2.74884923313555,17.0891252668893));
#39458=CARTESIAN_POINT('Ctrl Pts',(2.25014882333735,4.35558147263106,17.1684971569427));
#39459=CARTESIAN_POINT('Ctrl Pts',(-0.107154601980602,4.90130359745223,
17.2478690469961));
#39460=CARTESIAN_POINT('Ctrl Pts',(-2.43835555951383,4.25307922033065,17.3272409370495));
#39461=CARTESIAN_POINT('Ctrl Pts',(-4.17557820525659,2.56881377105676,17.4066128271029));
#39462=CARTESIAN_POINT('Ctrl Pts',(-4.8956397991406,0.258791705958601,17.4859847171563));
#39463=CARTESIAN_POINT('Ctrl Pts',(-4.42313332356637,-2.11427282962181,
17.5653566072097));
#39464=CARTESIAN_POINT('Ctrl Pts',(-2.8731633447509,-3.97230257099397,17.6447284972631));
#39465=CARTESIAN_POINT('Ctrl Pts',(-0.623293388711154,-4.8626931320669,
17.7241003873165));
#39466=CARTESIAN_POINT('Ctrl Pts',(1.77840238381723,-4.56853309419578,17.8034722773699));
#39467=CARTESIAN_POINT('Ctrl Pts',(3.74689662802603,-3.1615060961514,17.8828441674233));
#39468=CARTESIAN_POINT('Ctrl Pts',(4.80262992851038,-0.984309998791364,
17.9622160574768));
#39469=CARTESIAN_POINT('Ctrl Pts',(4.6885008269824,1.43259912421597,18.0415879475301));
#39470=CARTESIAN_POINT('Ctrl Pts',(3.43217338911689,3.50064868327997,18.1209598375836));
#39471=CARTESIAN_POINT('Ctrl Pts',(1.33994588402617,4.71572438645645,18.2003317276369));
#39472=CARTESIAN_POINT('Ctrl Pts',(-1.07901003836845,4.78248223987434,18.2797036176904));
#39473=CARTESIAN_POINT('Ctrl Pts',(-3.23451621663571,3.68344087079119,18.3590755077438));
#39474=CARTESIAN_POINT('Ctrl Pts',(-4.60324425657823,1.68862650319409,18.4384473977972));
#39475=CARTESIAN_POINT('Ctrl Pts',(-4.84847467695998,-0.720374489880202,
18.5178192878506));
#39476=CARTESIAN_POINT('Ctrl Pts',(-3.91669769333075,-2.94853678524982,
18.597191177904));
#39477=CARTESIAN_POINT('Ctrl Pts',(-2.02316502874899,-4.46849826887172,
18.6765630679574));
#39478=CARTESIAN_POINT('Ctrl Pts',(0.348982623889014,-4.88143613581971,
18.7559349580108));
#39479=CARTESIAN_POINT('Ctrl Pts',(3.43189297168081,-3.8881060605371,18.8617641447486));
#39480=CARTESIAN_POINT('Ctrl Pts',(5.55807194231376,-0.0182675279710476,
18.994050628171));
#39481=CARTESIAN_POINT('Ctrl Pts',(3.02540872544997,4.66632909528411,19.1527944082778));
#39482=CARTESIAN_POINT('Ctrl Pts',(-2.2762392030432,5.06930720888685,19.3115381883846));
#39483=CARTESIAN_POINT('Ctrl Pts',(-5.49476366156208,0.839647798275813,
19.4702819684914));
#39484=CARTESIAN_POINT('Ctrl Pts',(-3.68539651252317,-4.16147159288528,
19.6290257485982));
#39485=CARTESIAN_POINT('Ctrl Pts',(1.49629817009931,-5.35305176256653,19.787769528705));
#39486=CARTESIAN_POINT('Ctrl Pts',(5.30889903625351,-1.64699798333508,19.9465133088118));
#39487=CARTESIAN_POINT('Ctrl Pts',(4.26335305224425,3.56621538027062,20.1052570889186));
#39488=CARTESIAN_POINT('Ctrl Pts',(-0.682914143845088,5.51666761234037,
20.2640008690254));
#39489=CARTESIAN_POINT('Ctrl Pts',(-5.00517315099108,2.41778366488215,20.4227446491323));
#39490=CARTESIAN_POINT('Ctrl Pts',(-4.74574684718966,-2.89085235699305,
20.581488429239));
#39491=CARTESIAN_POINT('Ctrl Pts',(-0.146932230206273,-5.55932874556366,
20.7402322093459));
#39492=CARTESIAN_POINT('Ctrl Pts',(4.59246965375652,-3.13076985705421,20.8989759894527));
#39493=CARTESIAN_POINT('Ctrl Pts',(5.0299278500732,1.2629663218453,21.031262472875));
#39494=CARTESIAN_POINT('Ctrl Pts',(3.05056344532296,3.82678328180762,21.1370916596129));
#39495=CARTESIAN_POINT('Ctrl Pts',(0.861221142909519,4.82897211168878,21.2164635496663));
#39496=CARTESIAN_POINT('Ctrl Pts',(-1.56011376732917,4.64762681676397,21.2958354397197));
#39497=CARTESIAN_POINT('Ctrl Pts',(-3.58940432897566,3.338086676814,21.3752073297731));
#39498=CARTESIAN_POINT('Ctrl Pts',(-4.75071159562141,1.21328335035074,21.4545792198265));
#39499=CARTESIAN_POINT('Ctrl Pts',(-4.75136940590249,-1.2059521437222,21.5339511098799));
#39500=CARTESIAN_POINT('Ctrl Pts',(-3.59639816964331,-3.33201429213618,
21.6133229999333));
#39501=CARTESIAN_POINT('Ctrl Pts',(-1.56440212229559,-4.64609055668268,
21.6926948899867));
#39502=CARTESIAN_POINT('Ctrl Pts',(0.848175594776096,-4.82855605094712,
21.7720667800401));
#39503=CARTESIAN_POINT('Ctrl Pts',(3.05440612489727,-3.83470774368908,21.8514386700935));
#39504=CARTESIAN_POINT('Ctrl Pts',(4.5164489386699,-1.90677984789329,21.9308105601469));
#39505=CARTESIAN_POINT('Ctrl Pts',(4.87836953900972,0.485660146581216,22.0101824502003));
#39506=CARTESIAN_POINT('Ctrl Pts',(4.0518905292872,2.75978129753096,22.0895543402537));
#39507=CARTESIAN_POINT('Ctrl Pts',(2.23840092153696,4.36163277449212,22.1689262303071));
#39508=CARTESIAN_POINT('Ctrl Pts',(-0.120369299865574,4.90099648569508,
22.2482981203605));
#39509=CARTESIAN_POINT('Ctrl Pts',(-2.44981194564663,4.24649024808576,22.327670010414));
#39510=CARTESIAN_POINT('Ctrl Pts',(-4.18248893842781,2.55754735438689,22.4070419004673));
#39511=CARTESIAN_POINT('Ctrl Pts',(-4.89631923419535,0.245592132270486,
22.4864137905208));
#39512=CARTESIAN_POINT('Ctrl Pts',(-4.41741787585779,-2.12618907886207,
22.5657856805741));
#39513=CARTESIAN_POINT('Ctrl Pts',(-2.86244283812702,-3.98003518345998,
22.6451575706276));
#39514=CARTESIAN_POINT('Ctrl Pts',(-0.610183305945143,-4.86435360814152,
22.724529460681));
#39515=CARTESIAN_POINT('Ctrl Pts',(1.79071565870375,-4.56372621798445,22.8039013507344));
#39516=CARTESIAN_POINT('Ctrl Pts',(3.75540018385464,-3.15138524551451,22.8832732407878));
#39517=CARTESIAN_POINT('Ctrl Pts',(4.80527757305005,-0.971373790660912,
22.9626451308412));
#39518=CARTESIAN_POINT('Ctrl Pts',(4.68459996247748,1.44526216311697,23.0420170208946));
#39519=CARTESIAN_POINT('Ctrl Pts',(3.42276418043937,3.50983545637268,23.121388910948));
#39520=CARTESIAN_POINT('Ctrl Pts',(1.3271506148001,4.71942059955514,23.2007608010014));
#39521=CARTESIAN_POINT('Ctrl Pts',(-1.09175390014331,4.7793653318942,23.2801326910548));
#39522=CARTESIAN_POINT('Ctrl Pts',(-3.2447095830844,3.67506724782751,23.3595045811082));
#39523=CARTESIAN_POINT('Ctrl Pts',(-4.60726119282589,1.67553091707926,23.4388764711616));
#39524=CARTESIAN_POINT('Ctrl Pts',(-4.84749417441997,-0.732161036485464,
23.518248361215));
#39525=CARTESIAN_POINT('Ctrl Pts',(-3.90688830464649,-2.96150018209874,
23.5976202512684));
#39526=CARTESIAN_POINT('Ctrl Pts',(-2.01457309173102,-4.46942443856173,
23.6769921413218));
#39527=CARTESIAN_POINT('Ctrl Pts',(0.368487667211392,-4.88860679467339,
23.7563640313752));
#39528=CARTESIAN_POINT('Ctrl Pts',(2.66178564602131,-4.1169353563613,23.8357359214286));
#39529=CARTESIAN_POINT('Ctrl Pts',(4.30667853324075,-2.34238757791555,23.915107811482));
#39530=CARTESIAN_POINT('Ctrl Pts',(4.90247406242456,0.00276062972037378,
23.9944797015354));
#39531=CARTESIAN_POINT('Ctrl Pts',(4.30403776144901,2.34723635406859,24.0738515915888));
#39532=CARTESIAN_POINT('Ctrl Pts',(2.65714738860781,4.1199304980844,24.1532234816422));
#39533=CARTESIAN_POINT('Ctrl Pts',(0.362981793399119,4.88901869207872,24.2325953716956));
#39534=CARTESIAN_POINT('Ctrl Pts',(-2.01960536323572,4.46715275434179,24.311967261749));
#39535=CARTESIAN_POINT('Ctrl Pts',(-3.9102211237066,2.95709829352223,24.3913391518025));
#39536=CARTESIAN_POINT('Ctrl Pts',(-4.84831567357046,0.726701233826634,
24.4707110418558));
#39537=CARTESIAN_POINT('Ctrl Pts',(-4.60537125691712,-1.68071863790322,
24.5500829319093));
#39538=CARTESIAN_POINT('Ctrl Pts',(-3.2405685958952,-3.67871916964745,24.6294548219626));
#39539=CARTESIAN_POINT('Ctrl Pts',(-1.08637059779009,-4.78059185437233,
24.7088267120161));
#39540=CARTESIAN_POINT('Ctrl Pts',(1.33246487329615,-4.71792294503267,24.7881986020694));
#39541=CARTESIAN_POINT('Ctrl Pts',(3.42671485060842,-3.50597844922833,24.8675704921229));
#39542=CARTESIAN_POINT('Ctrl Pts',(4.68622467521711,-1.43998536354369,24.9469423821763));
#39543=CARTESIAN_POINT('Ctrl Pts',(4.80418054172532,0.976784969346655,25.0263142722297));
#39544=CARTESIAN_POINT('Ctrl Pts',(3.75184866214253,3.15561264578101,25.105686162283));
#39545=CARTESIAN_POINT('Ctrl Pts',(1.785574753038,4.56574006653325,25.1850580523365));
#39546=CARTESIAN_POINT('Ctrl Pts',(-0.615661213603954,4.86366331317224,
25.2644299423898));
#39547=CARTESIAN_POINT('Ctrl Pts',(-2.86692347135497,3.97680894225859,25.3438018324433));
#39548=CARTESIAN_POINT('Ctrl Pts',(-4.41980951731136,2.12121271552801,25.4231737224967));
#39549=CARTESIAN_POINT('Ctrl Pts',(-4.89603974793313,-0.25110623348048,
25.5025456125501));
#39550=CARTESIAN_POINT('Ctrl Pts',(-4.17960553315853,-2.56225625982736,
25.5819175026035));
#39551=CARTESIAN_POINT('Ctrl Pts',(-2.44502866190641,-4.24924633273829,
25.6612893926569));
#39552=CARTESIAN_POINT('Ctrl Pts',(-0.114848220593104,-4.9011294045414,
25.7406612827103));
#39553=CARTESIAN_POINT('Ctrl Pts',(2.24330899304448,-4.35910820186418,25.8200331727637));
#39554=CARTESIAN_POINT('Ctrl Pts',(4.05500110145669,-2.75521788993518,25.8994050628171));
#39555=CARTESIAN_POINT('Ctrl Pts',(4.87890391714675,-0.480162598589303,
25.9787769528705));
#39556=CARTESIAN_POINT('Ctrl Pts',(4.51431653789045,1.91185923895103,26.0581488429239));
#39557=CARTESIAN_POINT('Ctrl Pts',(3.05005164227427,3.83815639771151,26.1375207329773));
#39558=CARTESIAN_POINT('Ctrl Pts',(0.842800917774871,4.82948715360457,26.2168926230307));
#39559=CARTESIAN_POINT('Ctrl Pts',(-1.56975424478632,4.64436552876808,26.2962645130841));
#39560=CARTESIAN_POINT('Ctrl Pts',(-3.59992074790968,3.32788674125238,26.3756364031376));
#39561=CARTESIAN_POINT('Ctrl Pts',(-4.7531545251316,1.20074210971995,26.4550082931909));
#39562=CARTESIAN_POINT('Ctrl Pts',(-4.74853038096058,-1.21890064194263,
26.5343801832443));
#39563=CARTESIAN_POINT('Ctrl Pts',(-3.58717474668129,-3.34162189521881,
26.6137520732977));
#39564=CARTESIAN_POINT('Ctrl Pts',(-1.55199128418706,-4.65033145137433,
26.6931239633511));
#39565=CARTESIAN_POINT('Ctrl Pts',(0.861253819860729,-4.82623055930912,
26.7724958534045));
#39566=CARTESIAN_POINT('Ctrl Pts',(3.06469939974342,-3.82647058567632,26.851867743458));
#39567=CARTESIAN_POINT('Ctrl Pts',(4.52159098944567,-1.89459084712176,26.9312396335114));
#39568=CARTESIAN_POINT('Ctrl Pts',(4.87703302249084,0.49880702818598,27.0106115235648));
#39569=CARTESIAN_POINT('Ctrl Pts',(4.0444406063867,2.77069661551822,27.0899834136182));
#39570=CARTESIAN_POINT('Ctrl Pts',(2.22663141078423,4.36765064014314,27.1693553036716));
#39571=CARTESIAN_POINT('Ctrl Pts',(-0.133580267920228,4.90065463645992,
27.248727193725));
#39572=CARTESIAN_POINT('Ctrl Pts',(-2.46125208903423,4.23987001075014,27.3280990837784));
#39573=CARTESIAN_POINT('Ctrl Pts',(-4.1893683491486,2.54626243521474,27.4074709738318));
#39574=CARTESIAN_POINT('Ctrl Pts',(-4.89696375241997,0.232390966517291,
27.4868428638852));
#39575=CARTESIAN_POINT('Ctrl Pts',(-4.41166962484721,-2.13809042723509,
27.5662147539386));
#39576=CARTESIAN_POINT('Ctrl Pts',(-2.85170254172674,-3.98773772549588,
27.645586643992));
#39577=CARTESIAN_POINT('Ctrl Pts',(-0.597067031578144,-4.8659809405336,
27.7249585340454));
#39578=CARTESIAN_POINT('Ctrl Pts',(1.80301268587744,-4.55888196912345,27.8043304240988));
#39579=CARTESIAN_POINT('Ctrl Pts',(3.76388250395415,-3.14124944094887,27.8837023141522));
#39580=CARTESIAN_POINT('Ctrl Pts',(4.80787887528022,-0.958415501996903,
27.9630742042056));
#39581=CARTESIAN_POINT('Ctrl Pts',(4.68068659464744,1.45788633182479,28.042446094259));
#39582=CARTESIAN_POINT('Ctrl Pts',(3.41328942008259,3.51905028219065,28.1218179843124));
#39583=CARTESIAN_POINT('Ctrl Pts',(1.31442249797358,4.72298137310056,28.2011898743658));
#39584=CARTESIAN_POINT('Ctrl Pts',(-1.10463483521695,4.77640465566507,28.2805617644192));
#39585=CARTESIAN_POINT('Ctrl Pts',(-3.25460556761632,3.66630633650198,28.3599336544726));
#39586=CARTESIAN_POINT('Ctrl Pts',(-4.6117615876916,1.66310390899846,28.439305544526));
#39587=CARTESIAN_POINT('Ctrl Pts',(-4.84550269296638,-0.745226949519058,
28.5186774345794));
#39588=CARTESIAN_POINT('Ctrl Pts',(-3.89889006757279,-2.97202217266562,
28.5980493246329));
#39589=CARTESIAN_POINT('Ctrl Pts',(-2.00251645176526,-4.4748393730103,28.6774212146862));
#39590=CARTESIAN_POINT('Ctrl Pts',(0.381665739197275,-4.88759560697863,
28.7567931047396));
#39591=CARTESIAN_POINT('Ctrl Pts',(2.67287500089413,-4.10974436959635,28.8361649947931));
#39592=CARTESIAN_POINT('Ctrl Pts',(4.31297782868169,-2.33076850054527,28.9155368848464));
#39593=CARTESIAN_POINT('Ctrl Pts',(4.90244880401687,0.015977416170102,28.9949087748999));
#39594=CARTESIAN_POINT('Ctrl Pts',(4.29769410207987,2.35883126967183,29.0742806649532));
#39595=CARTESIAN_POINT('Ctrl Pts',(2.64603062966077,4.12707904706596,29.1536525550067));
#39596=CARTESIAN_POINT('Ctrl Pts',(0.349799952745733,4.88997950372933,29.23302444506));
#39597=CARTESIAN_POINT('Ctrl Pts',(-2.03164121838909,4.46169177707024,29.3123963351135));
#39598=CARTESIAN_POINT('Ctrl Pts',(-3.91817908568586,2.94654580930412,29.3917682251669));
#39599=CARTESIAN_POINT('Ctrl Pts',(-4.85025720045188,0.71362780446005,29.4711401152203));
#39600=CARTESIAN_POINT('Ctrl Pts',(-4.60082339705005,-1.69312835396218,
29.5505120052737));
#39601=CARTESIAN_POINT('Ctrl Pts',(-3.23063919787666,-3.68744219303526,
29.6298838953271));
#39602=CARTESIAN_POINT('Ctrl Pts',(-1.07347844099907,-4.78350327589979,
29.7092557853805));
#39603=CARTESIAN_POINT('Ctrl Pts',(1.34517928800161,-4.71431354886002,29.7886276754339));
#39604=CARTESIAN_POINT('Ctrl Pts',(3.43615431994896,-3.49672747627405,29.8679995654873));
#39605=CARTESIAN_POINT('Ctrl Pts',(4.69008976535537,-1.42734633034267,29.9473714555407));
#39606=CARTESIAN_POINT('Ctrl Pts',(4.8015297252588,0.989733222282683,30.0267433455941));
#39607=CARTESIAN_POINT('Ctrl Pts',(3.74332767209493,3.16571595269729,30.1061152356475));
#39608=CARTESIAN_POINT('Ctrl Pts',(1.77325928372404,4.57053728422822,30.1854871257009));
#39609=CARTESIAN_POINT('Ctrl Pts',(-0.628771141119161,4.86198585003386,
30.2648590157543));
#39610=CARTESIAN_POINT('Ctrl Pts',(-2.8776343077471,3.9690654245944,30.3442309058078));
#39611=CARTESIAN_POINT('Ctrl Pts',(-4.42551212654334,2.10928944710103,30.4236027958611));
#39612=CARTESIAN_POINT('Ctrl Pts',(-4.89534498701853,-0.264304770873174,
30.5029746859146));
#39613=CARTESIAN_POINT('Ctrl Pts',(-4.17268264431835,-2.57351493169134,
30.5823465759679));
#39614=CARTESIAN_POINT('Ctrl Pts',(-2.43356404553856,-4.25582255152819,
30.6617184660214));
#39615=CARTESIAN_POINT('Ctrl Pts',(-0.101634631868219,-4.90142121791616,
30.7410903560747));
#39616=CARTESIAN_POINT('Ctrl Pts',(2.25505275316072,-4.35304452473163,30.8204622461282));
#39617=CARTESIAN_POINT('Ctrl Pts',(4.06241427899435,-2.74427582062311,30.8998341361815));
#39618=CARTESIAN_POINT('Ctrl Pts',(4.88018067846643,-0.467007600962325,
30.979206026235));
#39619=CARTESIAN_POINT('Ctrl Pts',(4.50914586676086,1.9240226365891,31.0585779162884));
#39620=CARTESIAN_POINT('Ctrl Pts',(3.0396931027374,3.84636521861933,31.1379498063418));
#39621=CARTESIAN_POINT('Ctrl Pts',(0.829777827133663,4.83174174717888,31.2173216963951));
#39622=CARTESIAN_POINT('Ctrl Pts',(-1.58226949047778,4.64011668100458,31.2966935864486));
#39623=CARTESIAN_POINT('Ctrl Pts',(-3.60887946250293,3.31816946206164,31.376065476502));
#39624=CARTESIAN_POINT('Ctrl Pts',(-4.75637438558157,1.18792350680397,31.4554373665554));
#39625=CARTESIAN_POINT('Ctrl Pts',(-4.74522703638862,-1.23169798528705,
31.5348092566087));
#39626=CARTESIAN_POINT('Ctrl Pts',(-3.57815288451333,-3.35128057447936,
31.6141811466622));
#39627=CARTESIAN_POINT('Ctrl Pts',(-1.53944861007768,-4.65449863366224,
31.6935530367156));
#39628=CARTESIAN_POINT('Ctrl Pts',(0.874261938261232,-4.823891128243,31.772924926769));
#39629=CARTESIAN_POINT('Ctrl Pts',(3.07500421358568,-3.81819442148565,31.8522968168224));
#39630=CARTESIAN_POINT('Ctrl Pts',(4.52668226888703,-1.88239400508438,31.9316687068758));
#39631=CARTESIAN_POINT('Ctrl Pts',(4.87567054312872,0.511953424346944,32.0110405969291));
#39632=CARTESIAN_POINT('Ctrl Pts',(4.036956265178,2.78159013279705,32.0904124869827));
#39633=CARTESIAN_POINT('Ctrl Pts',(2.21484837668102,4.37363764184315,32.169784377036));
#39634=CARTESIAN_POINT('Ctrl Pts',(-0.146791673891742,4.90027670221896,
32.2491562670894));
#39635=CARTESIAN_POINT('Ctrl Pts',(-2.47267359762233,4.23321920451271,32.3285281571428));
#39636=CARTESIAN_POINT('Ctrl Pts',(-4.19621770614226,2.53495887865897,32.4079000471962));
#39637=CARTESIAN_POINT('Ctrl Pts',(-4.89757246961631,0.219188181000233,
32.4872719372496));
#39638=CARTESIAN_POINT('Ctrl Pts',(-4.40588942008463,-2.1499762723854,32.566643827303));
#39639=CARTESIAN_POINT('Ctrl Pts',(-2.84094146009112,-3.99541126470971,
32.6460157173564));
#39640=CARTESIAN_POINT('Ctrl Pts',(-0.583946448736662,-4.86757291664353,
32.7253876074098));
#39641=CARTESIAN_POINT('Ctrl Pts',(1.81529662498649,-4.55400458027289,32.8047594974633));
#39642=CARTESIAN_POINT('Ctrl Pts',(3.77233745895388,-3.13109080826592,32.8841313875166));
#39643=CARTESIAN_POINT('Ctrl Pts',(4.81044523784739,-0.945450245917296,
32.96350327757));
#39644=CARTESIAN_POINT('Ctrl Pts',(4.67673920454123,1.4704999036181,33.0428751676234));
#39645=CARTESIAN_POINT('Ctrl Pts',(3.40378985279549,3.52823953152847,33.1222470576768));
#39646=CARTESIAN_POINT('Ctrl Pts',(1.30168482706983,4.72650781918426,33.2016189477302));
#39647=CARTESIAN_POINT('Ctrl Pts',(-1.11750774129953,4.7734092640344,33.2809908377837));
#39648=CARTESIAN_POINT('Ctrl Pts',(-3.2644778974498,3.65751877792795,33.360362727837));
#39649=CARTESIAN_POINT('Ctrl Pts',(-4.61622846358057,1.65066481329873,33.4397346178904));
#39650=CARTESIAN_POINT('Ctrl Pts',(-4.84347599383145,-0.75828744616548,
33.5191065079439));
#39651=CARTESIAN_POINT('Ctrl Pts',(-3.89086349283728,-2.98252256218456,
33.5984783979973));
#39652=CARTESIAN_POINT('Ctrl Pts',(-1.99044525726817,-4.4802217837572,33.6778502880507));
#39653=CARTESIAN_POINT('Ctrl Pts',(0.394841037195618,-4.88654889560926,
33.7572221781041));
#39654=CARTESIAN_POINT('Ctrl Pts',(2.68394492896431,-4.10252351268344,33.8365940681574));
#39655=CARTESIAN_POINT('Ctrl Pts',(4.31924577684866,-2.31913248284973,33.9159659582109));
#39656=CARTESIAN_POINT('Ctrl Pts',(4.90238791398107,0.029194086493524,33.9953378482642));
#39657=CARTESIAN_POINT('Ctrl Pts',(4.29131920651926,2.37040904098698,34.0747097383177));
#39658=CARTESIAN_POINT('Ctrl Pts',(2.63489463902328,4.13419759990741,34.1540816283711));
#39659=CARTESIAN_POINT('Ctrl Pts',(0.336615569701593,4.89090477438156,34.2334535184245));
#39660=CARTESIAN_POINT('Ctrl Pts',(-2.04366230731349,4.45619837165044,34.3128254084779));
#39661=CARTESIAN_POINT('Ctrl Pts',(-3.92610856983677,2.93597190921303,34.3921972985313));
#39662=CARTESIAN_POINT('Ctrl Pts',(-4.85216347504172,0.700549188354975,
34.4715691885847));
#39663=CARTESIAN_POINT('Ctrl Pts',(-4.59624209780822,-1.70552576414703,
34.5509410786381));
#39664=CARTESIAN_POINT('Ctrl Pts',(-3.22068631915797,-3.69613841562006,
34.6303129686915));
#39665=CARTESIAN_POINT('Ctrl Pts',(-1.06057848202912,-4.7863799303117,34.709684858745));
#39666=CARTESIAN_POINT('Ctrl Pts',(1.35788392577142,-4.71066988845169,34.7890567487982));
#39667=CARTESIAN_POINT('Ctrl Pts',(3.44556881487913,-3.48745108865577,34.8684286388518));
#39668=CARTESIAN_POINT('Ctrl Pts',(4.69392076731947,-1.41469692300534,34.9478005289051));
#39669=CARTESIAN_POINT('Ctrl Pts',(4.79884401065818,1.00267428171067,35.0271724189586));
#39670=CARTESIAN_POINT('Ctrl Pts',(3.73477947506157,3.17579625078383,35.1065443090119));
#39671=CARTESIAN_POINT('Ctrl Pts',(1.76093092613411,4.57530128267181,35.1859161990653));
#39672=CARTESIAN_POINT('Ctrl Pts',(-0.64187649864509,4.86027304935852,35.2652880891187));
#39673=CARTESIAN_POINT('Ctrl Pts',(-2.88832422912388,3.96129305925348,35.3446599791721));
#39674=CARTESIAN_POINT('Ctrl Pts',(-4.43118257058537,2.09735084808771,35.4240318692256));
#39675=CARTESIAN_POINT('Ctrl Pts',(-4.89461464610851,-0.277501387264873,
35.5034037592789));
#39676=CARTESIAN_POINT('Ctrl Pts',(-4.16572942788534,-2.58475489891863,
35.5827756493324));
#39677=CARTESIAN_POINT('Ctrl Pts',(-2.42208174171502,-4.2623678384537,35.6621475393857));
#39678=CARTESIAN_POINT('Ctrl Pts',(-0.0884203044499451,-4.90167740713266,
35.7415194294392));
#39679=CARTESIAN_POINT('Ctrl Pts',(2.26678012326416,-4.34694920911302,35.8208913194925));
#39680=CARTESIAN_POINT('Ctrl Pts',(4.06979793038381,-2.73331380556231,35.900263209546));
#39681=CARTESIAN_POINT('Ctrl Pts',(4.88142197000686,-0.453849209064084,
35.9796350995994));
#39682=CARTESIAN_POINT('Ctrl Pts',(4.50394242258051,1.9361720501839,36.0590069896528));
#39683=CARTESIAN_POINT('Ctrl Pts',(3.02931247032103,3.85454608365127,36.1383788797062));
#39684=CARTESIAN_POINT('Ctrl Pts',(0.816748705560739,4.83396122303424,36.2177507697595));
#39685=CARTESIAN_POINT('Ctrl Pts',(-1.59477323603157,4.63583410827775,36.297122659813));
#39686=CARTESIAN_POINT('Ctrl Pts',(-3.61781194729725,3.3084280659895,36.3764945498664));
#39687=CARTESIAN_POINT('Ctrl Pts',(-4.75955967609224,1.17509626990754,36.4558664399198));
#39688=CARTESIAN_POINT('Ctrl Pts',(-4.74188920289779,-1.24448637649244,
36.5352383299732));
#39689=CARTESIAN_POINT('Ctrl Pts',(-3.56910501587113,-3.36091489620272,
36.6146102200266));
#39690=CARTESIAN_POINT('Ctrl Pts',(-1.52689474705826,-4.65863198645693,
36.69398211008));
#39691=CARTESIAN_POINT('Ctrl Pts',(0.887263702413796,-4.82151663651726,
36.7733540001334));
#39692=CARTESIAN_POINT('Ctrl Pts',(3.08528667790275,-3.80989050616806,36.8527258901868));
#39693=CARTESIAN_POINT('Ctrl Pts',(4.53174064782084,-1.87018348156595,36.9320977802402));
#39694=CARTESIAN_POINT('Ctrl Pts',(4.87427262676759,0.525096099564754,37.0114696702936));
#39695=CARTESIAN_POINT('Ctrl Pts',(4.02944258285317,2.79246343312197,37.090841560347));
#39696=CARTESIAN_POINT('Ctrl Pts',(2.20304924477561,4.37959285538367,37.1702134504005));
#39697=CARTESIAN_POINT('Ctrl Pts',(-0.160002012962556,4.89986315213815,
37.2495853404538));
#39698=CARTESIAN_POINT('Ctrl Pts',(-2.48407713450139,4.22653763069513,37.3289572305073));
#39699=CARTESIAN_POINT('Ctrl Pts',(-4.20303656448734,2.52363689769662,37.4083291205606));
#39700=CARTESIAN_POINT('Ctrl Pts',(-4.89814559062741,0.20598380239574,37.4877010106141));
#39701=CARTESIAN_POINT('Ctrl Pts',(-4.40007719275278,-2.16184649123314,
37.5670729006674));
#39702=CARTESIAN_POINT('Ctrl Pts',(-2.83015973012786,-4.0030557647603,37.6464447907209));
#39703=CARTESIAN_POINT('Ctrl Pts',(-0.570821621698638,-4.86912951461192,
37.7258166807742));
#39704=CARTESIAN_POINT('Ctrl Pts',(1.82756737028896,-4.54909409232726,37.8051885708277));
#39705=CARTESIAN_POINT('Ctrl Pts',(3.78076499611679,-3.12090941842365,37.884560460881));
#39706=CARTESIAN_POINT('Ctrl Pts',(4.81297663748916,-0.932478118164531,
37.9639323509345));
#39707=CARTESIAN_POINT('Ctrl Pts',(4.6727578232798,1.48310278759233,38.0433042409879));
#39708=CARTESIAN_POINT('Ctrl Pts',(3.39426554635479,3.53740313723864,38.1226761310413));
#39709=CARTESIAN_POINT('Ctrl Pts',(1.2889376953013,4.72999991227071,38.2020480210947));
#39710=CARTESIAN_POINT('Ctrl Pts',(-1.13037252509376,4.77037917890205,38.2814199111481));
#39711=CARTESIAN_POINT('Ctrl Pts',(-3.27432650082598,3.64870463556727,38.3607918012015));
#39712=CARTESIAN_POINT('Ctrl Pts',(-4.62066178777622,1.63821372124413,38.4401636912549));
#39713=CARTESIAN_POINT('Ctrl Pts',(-4.84141409235733,-0.771342433159972,
38.5195355813083));
#39714=CARTESIAN_POINT('Ctrl Pts',(-3.88280863754963,-2.99300127117752,
38.5989074713617));
#39715=CARTESIAN_POINT('Ctrl Pts',(-1.97835959833324,-4.48557163766163,
38.6782793614151));
#39716=CARTESIAN_POINT('Ctrl Pts',(0.4080134699205,-4.88546665687603,38.7576512514685));
#39717=CARTESIAN_POINT('Ctrl Pts',(2.69499534131588,-4.09527285943909,38.8370231415219));
#39718=CARTESIAN_POINT('Ctrl Pts',(4.32548234816251,-2.30747956911512,38.9163950315754));
#39719=CARTESIAN_POINT('Ctrl Pts',(4.90229136258888,0.0424104685617285,
38.9957669216287));
#39720=CARTESIAN_POINT('Ctrl Pts',(4.28491317807095,2.38196972749885,39.0751388116822));
#39721=CARTESIAN_POINT('Ctrl Pts',(2.62373939006081,4.14128583366062,39.1545107017355));
#39722=CARTESIAN_POINT('Ctrl Pts',(0.323428943211332,4.89179500940948,39.233882591789));
#39723=CARTESIAN_POINT('Ctrl Pts',(-2.05566892616818,4.45067161106171,39.3132544818423));
#39724=CARTESIAN_POINT('Ctrl Pts',(-3.93400879434316,2.92537849589611,39.3926263718958));
#39725=CARTESIAN_POINT('Ctrl Pts',(-4.85403585089548,0.68746203308737,39.4719982619491));
#39726=CARTESIAN_POINT('Ctrl Pts',(-4.59162481050186,-1.71790426872522,
39.5513701520026));
#39727=CARTESIAN_POINT('Ctrl Pts',(-3.21071490770548,-3.70482006635682,
39.6307420420559));
#39728=CARTESIAN_POINT('Ctrl Pts',(-1.04766160592177,-4.78919858119775,
39.7101139321094));
#39729=CARTESIAN_POINT('Ctrl Pts',(1.37056128557131,-4.7070358700676,39.7894858221627));
#39730=CARTESIAN_POINT('Ctrl Pts',(3.45499130789194,-3.47806613859367,39.8688577122162));
#39731=CARTESIAN_POINT('Ctrl Pts',(4.69765387924814,-1.40219731261544,39.9482296022695));
#39732=CARTESIAN_POINT('Ctrl Pts',(4.79625497710706,1.0159342797995,40.027601492323));
#39733=CARTESIAN_POINT('Ctrl Pts',(4.08267404777822,2.46201708819427,40.0805160856919));
#39734=CARTESIAN_POINT('Ctrl Pts',(3.57461543774186,3.05624720968413,40.1069733823764));
#39735=CARTESIAN_POINT('Ctrl Pts',(1.16918346556923,-4.36383719750629,-0.320920147129053));
#39736=CARTESIAN_POINT('Ctrl Pts',(1.8946107326977,-4.16947670058299,-0.294462850444586));
#39737=CARTESIAN_POINT('Ctrl Pts',(3.24594541476064,-3.41224896374509,-0.24154825707565));
#39738=CARTESIAN_POINT('Ctrl Pts',(4.48258575488109,-1.44364637546346,-0.162176367022246));
#39739=CARTESIAN_POINT('Ctrl Pts',(4.62712170766666,0.875927969712858,-0.0828044769688426));
#39740=CARTESIAN_POINT('Ctrl Pts',(3.64458116255458,2.98248116081162,-0.00343258691543892));
#39741=CARTESIAN_POINT('Ctrl Pts',(1.77418661813218,4.36232362711486,0.0759393031379646));
#39742=CARTESIAN_POINT('Ctrl Pts',(-0.52837360592073,4.67961139929734,0.155311193191369));
#39743=CARTESIAN_POINT('Ctrl Pts',(-2.70223496968603,3.85690448821556,0.234683083244771));
#39744=CARTESIAN_POINT('Ctrl Pts',(-4.21783163769356,2.09469156016015,0.314054973298176));
#39745=CARTESIAN_POINT('Ctrl Pts',(-4.70597715859854,-0.177798095133649,
0.393426863351579));
#39746=CARTESIAN_POINT('Ctrl Pts',(-4.04775531046147,-2.4069688489564,0.472798753404983));
#39747=CARTESIAN_POINT('Ctrl Pts',(-2.40351015490329,-4.04981138575499,
0.552170643458387));
#39748=CARTESIAN_POINT('Ctrl Pts',(-0.173774754931243,-4.70612667927193,
0.631542533511791));
#39749=CARTESIAN_POINT('Ctrl Pts',(2.0982915307903,-4.21604107122297,0.710914423565194));
#39750=CARTESIAN_POINT('Ctrl Pts',(3.85921878174909,-2.69893658616936,0.790286313618597));
#39751=CARTESIAN_POINT('Ctrl Pts',(4.68004880681062,-0.524377442655228,
0.869658203672002));
#39752=CARTESIAN_POINT('Ctrl Pts',(4.36082934025305,1.77791905463906,0.949030093725404));
#39753=CARTESIAN_POINT('Ctrl Pts',(2.97932147849509,3.64711831584472,1.02840198377881));
#39754=CARTESIAN_POINT('Ctrl Pts',(0.872057510020645,4.62788767559441,1.10777387383221));
#39755=CARTESIAN_POINT('Ctrl Pts',(-1.44763774336318,4.48131381605584,1.18714576388562));
#39756=CARTESIAN_POINT('Ctrl Pts',(-3.4146916437183,3.2431018434756,1.26651765393902));
#39757=CARTESIAN_POINT('Ctrl Pts',(-4.54993421956391,1.21487743324944,1.34588954399242));
#39758=CARTESIAN_POINT('Ctrl Pts',(-4.57682288978047,-1.10928842689199,
1.42526143404583));
#39759=CARTESIAN_POINT('Ctrl Pts',(-3.48880763512327,-3.16323408359086,
1.50463332409923));
#39760=CARTESIAN_POINT('Ctrl Pts',(-1.55092656265583,-4.44662291817823,
1.58400521415264));
#39761=CARTESIAN_POINT('Ctrl Pts',(0.764756787430318,-4.64682425288564,
1.66337710420604));
#39762=CARTESIAN_POINT('Ctrl Pts',(2.89414707692588,-3.71506948486699,1.74274899425944));
#39763=CARTESIAN_POINT('Ctrl Pts',(4.31852954453272,-1.87833201365734,1.82212088431284));
#39764=CARTESIAN_POINT('Ctrl Pts',(4.69092777401317,0.415962978544339,1.90149277436625));
#39765=CARTESIAN_POINT('Ctrl Pts',(3.92062638092659,2.60893030984735,1.98086466441965));
#39766=CARTESIAN_POINT('Ctrl Pts',(2.19526907961086,4.166367992464,2.06023655447306));
#39767=CARTESIAN_POINT('Ctrl Pts',(-0.0648509103551908,4.70888765420329,
2.13960844452646));
#39768=CARTESIAN_POINT('Ctrl Pts',(-2.30917336210229,4.10433270633116,2.21898033457986));
#39769=CARTESIAN_POINT('Ctrl Pts',(-3.99098629411059,2.49997139597969,2.29835222463327));
#39770=CARTESIAN_POINT('Ctrl Pts',(-4.70060379877146,0.286622587162194,
2.37772411468667));
#39771=CARTESIAN_POINT('Ctrl Pts',(-4.26516462266185,-1.99654684946062,
2.45709600474007));
#39772=CARTESIAN_POINT('Ctrl Pts',(-2.79074078525346,-3.79336189283582,
2.53646789479348));
#39773=CARTESIAN_POINT('Ctrl Pts',(-0.636498669757338,-4.66612237558061,
2.61583978484688));
#39774=CARTESIAN_POINT('Ctrl Pts',(1.6727931128258,-4.40222577592052,2.69521167490029));
#39775=CARTESIAN_POINT('Ctrl Pts',(3.5745961957893,-3.06595672140773,2.77458356495369));
#39776=CARTESIAN_POINT('Ctrl Pts',(4.60563555769302,-0.982827395940078,
2.85395545500709));
#39777=CARTESIAN_POINT('Ctrl Pts',(4.51475229214408,1.33971650772703,2.9333273450605));
#39778=CARTESIAN_POINT('Ctrl Pts',(3.32408536146356,3.33590843552402,3.0126992351139));
#39779=CARTESIAN_POINT('Ctrl Pts',(1.32367859446866,4.51948045233543,3.0920711251673));
#39780=CARTESIAN_POINT('Ctrl Pts',(-0.99917334822593,4.60211703465825,3.17144301522071));
#39781=CARTESIAN_POINT('Ctrl Pts',(-3.07862887492539,3.56368809395157,3.25081490527411));
#39782=CARTESIAN_POINT('Ctrl Pts',(-4.40813722212245,1.65715262164811,3.33018679532752));
#39783=CARTESIAN_POINT('Ctrl Pts',(-4.66383309925671,-0.653061561243739,
3.40955868538092));
#39784=CARTESIAN_POINT('Ctrl Pts',(-3.7834295566315,-2.80419139334385,3.48893057543432));
#39785=CARTESIAN_POINT('Ctrl Pts',(-1.98139094849014,-4.27222640899777,
3.56830246548773));
#39786=CARTESIAN_POINT('Ctrl Pts',(0.303310108968963,-4.69955652783259,
3.64767435554113));
#39787=CARTESIAN_POINT('Ctrl Pts',(2.51412549524875,-3.98208507877931,3.72704624559453));
#39788=CARTESIAN_POINT('Ctrl Pts',(4.11250547580833,-2.29458651873122,3.80641813564794));
#39789=CARTESIAN_POINT('Ctrl Pts',(4.70908822533748,-0.0481317617013215,
3.88579002570134));
#39790=CARTESIAN_POINT('Ctrl Pts',(4.15854750656441,2.21004778594118,3.96516191575474));
#39791=CARTESIAN_POINT('Ctrl Pts',(2.59499381998102,3.92986458478622,4.04453380580815));
#39792=CARTESIAN_POINT('Ctrl Pts',(0.399305382771643,4.69237506938503,4.12390569586155));
#39793=CARTESIAN_POINT('Ctrl Pts',(-1.89365296183344,4.3118333734777,4.20327758591496));
#39794=CARTESIAN_POINT('Ctrl Pts',(-3.72532163646561,2.88093861187248,4.28264947596836));
#39795=CARTESIAN_POINT('Ctrl Pts',(-4.64951020631435,0.748253581264596,
4.36202136602176));
#39796=CARTESIAN_POINT('Ctrl Pts',(-4.44108838142119,-1.56670436550815,
4.44139325607517));
#39797=CARTESIAN_POINT('Ctrl Pts',(-3.15082725699623,-3.5000165966844,4.52076514612857));
#39798=CARTESIAN_POINT('Ctrl Pts',(-1.09303158700481,-4.58073253206366,
4.60013703618198));
#39799=CARTESIAN_POINT('Ctrl Pts',(1.23102415819659,-4.54559216191169,4.67950892623538));
#39800=CARTESIAN_POINT('Ctrl Pts',(3.25520514328707,-3.40315560261561,4.75888081628878));
#39801=CARTESIAN_POINT('Ctrl Pts',(4.48642536074717,-1.43171787127954,4.83825270634219));
#39802=CARTESIAN_POINT('Ctrl Pts',(4.62476229086337,0.888483164446475,4.91762459639559));
#39803=CARTESIAN_POINT('Ctrl Pts',(3.63651736366295,2.99225166793745,4.99699648644899));
#39804=CARTESIAN_POINT('Ctrl Pts',(1.76242485596889,4.36711428835561,5.0763683765024));
#39805=CARTESIAN_POINT('Ctrl Pts',(-0.540990445577951,4.67815753457383,
5.15574026655579));
#39806=CARTESIAN_POINT('Ctrl Pts',(-2.71262167204403,3.84961196029596,5.23511215660921));
#39807=CARTESIAN_POINT('Ctrl Pts',(-4.22346426348642,2.08330943346152,5.3144840466626));
#39808=CARTESIAN_POINT('Ctrl Pts',(-4.70548030882309,-0.190482660036918,
5.39385593671601));
#39809=CARTESIAN_POINT('Ctrl Pts',(-4.04125176633447,-2.41787359917659,
5.47322782676941));
#39810=CARTESIAN_POINT('Ctrl Pts',(-2.39258323872581,-4.05627588142928,
5.55259971682282));
#39811=CARTESIAN_POINT('Ctrl Pts',(-0.161086730056731,-4.70657833738016,
5.63197160687622));
#39812=CARTESIAN_POINT('Ctrl Pts',(2.10965014949475,-4.21036872817968,5.71134349692963));
#39813=CARTESIAN_POINT('Ctrl Pts',(3.86648092226071,-2.68852261628773,5.79071538698303));
#39814=CARTESIAN_POINT('Ctrl Pts',(4.68144550067431,-0.511758346011949,
5.87008727703643));
#39815=CARTESIAN_POINT('Ctrl Pts',(4.3560203173275,1.78966912459444,5.94945916708984));
#39816=CARTESIAN_POINT('Ctrl Pts',(2.96947822656715,3.65513715781504,6.02883105714324));
#39817=CARTESIAN_POINT('Ctrl Pts',(0.859577812643608,4.63022186990077,6.10820294719665));
#39818=CARTESIAN_POINT('Ctrl Pts',(-1.45971385379671,4.47739478330096,6.18757483725004));
#39819=CARTESIAN_POINT('Ctrl Pts',(-3.42342245647396,3.23388423803426,6.26694672730346));
#39820=CARTESIAN_POINT('Ctrl Pts',(-4.55319292637122,1.20260665046377,6.34631861735685));
#39821=CARTESIAN_POINT('Ctrl Pts',(-4.57381567772605,-1.12162325523503,
6.42569050741026));
#39822=CARTESIAN_POINT('Ctrl Pts',(-3.48026705395609,-3.17262821862952,
6.50506239746367));
#39823=CARTESIAN_POINT('Ctrl Pts',(-1.5389330792829,-4.45078797045933,6.58443428751706));
#39824=CARTESIAN_POINT('Ctrl Pts',(0.777281587133017,-4.64474562433731,
6.66380617757047));
#39825=CARTESIAN_POINT('Ctrl Pts',(2.90415217940695,-3.70725352509678,6.74317806762387));
#39826=CARTESIAN_POINT('Ctrl Pts',(4.32357772900916,-1.86668267300916,6.82254995767728));
#39827=CARTESIAN_POINT('Ctrl Pts',(4.68978931390171,0.428607946391479,6.90192184773068));
#39828=CARTESIAN_POINT('Ctrl Pts',(3.91357860260037,2.61949061875875,6.98129373778408));
#39829=CARTESIAN_POINT('Ctrl Pts',(2.18402880626489,4.17227117454053,7.06066562783749));
#39830=CARTESIAN_POINT('Ctrl Pts',(-0.0775455730109682,4.70869570736982,
7.14003751789088));
#39831=CARTESIAN_POINT('Ctrl Pts',(-2.32023002234555,4.09809238840499,7.2194094079443));
#39832=CARTESIAN_POINT('Ctrl Pts',(-3.9977115739788,2.48920283459836,7.29878129799769));
#39833=CARTESIAN_POINT('Ctrl Pts',(-4.70135943497531,0.273948980040579,
7.37815318805111));
#39834=CARTESIAN_POINT('Ctrl Pts',(-4.25976654389442,-2.00803823967931,
7.4575250781045));
#39835=CARTESIAN_POINT('Ctrl Pts',(-2.78050395155417,-3.80087178893057,
7.53689696815791));
#39836=CARTESIAN_POINT('Ctrl Pts',(-0.623916751156424,-4.66782138348534,
7.61626885821132));
#39837=CARTESIAN_POINT('Ctrl Pts',(1.68465518880672,-4.39770002107047,7.69564074826471));
#39838=CARTESIAN_POINT('Ctrl Pts',(3.58284885369757,-3.05630866766671,7.77501263831812));
#39839=CARTESIAN_POINT('Ctrl Pts',(4.6082684683291,-0.970407287843808,7.85438452837152));
#39840=CARTESIAN_POINT('Ctrl Pts',(4.51112408430488,1.35188315933773,7.93375641842493));
#39841=CARTESIAN_POINT('Ctrl Pts',(3.31507985854782,3.3448578612472,8.01312830847833));
#39842=CARTESIAN_POINT('Ctrl Pts',(1.31148951705327,4.52303259187419,8.09250019853174));
#39843=CARTESIAN_POINT('Ctrl Pts',(-1.01157676786264,4.5994065946834,8.17187208858514));
#39844=CARTESIAN_POINT('Ctrl Pts',(-3.08822519121439,3.55537533164157,8.25124397863854));
#39845=CARTESIAN_POINT('Ctrl Pts',(-4.41258879365683,1.64526250750169,8.33061586869195));
#39846=CARTESIAN_POINT('Ctrl Pts',(-4.66205553306411,-0.665632621738795,
8.40998775874535));
#39847=CARTESIAN_POINT('Ctrl Pts',(-3.77585586390188,-2.81438111767656,
8.48935964879875));
#39848=CARTESIAN_POINT('Ctrl Pts',(-1.96986606400833,-4.27755260287526,
8.56873153885216));
#39849=CARTESIAN_POINT('Ctrl Pts',(0.315978748853086,-4.69872174221563,
8.64810342890556));
#39850=CARTESIAN_POINT('Ctrl Pts',(2.52485183790096,-3.97529266559641,8.72747531895897));
#39851=CARTESIAN_POINT('Ctrl Pts',(4.11867660790092,-2.28349109479901,8.80684720901236));
#39852=CARTESIAN_POINT('Ctrl Pts',(4.70920087275226,-0.0354361477303297,
8.88621909906579));
#39853=CARTESIAN_POINT('Ctrl Pts',(4.15257422864046,2.22125096648886,8.96559098911916));
#39854=CARTESIAN_POINT('Ctrl Pts',(2.58438969399899,3.93684626192698,9.04496287917259));
#39855=CARTESIAN_POINT('Ctrl Pts',(0.386653550348944,4.69343452202107,9.12433476922598));
#39856=CARTESIAN_POINT('Ctrl Pts',(-1.90527054232303,4.30671252129195,9.20370665927939));
#39857=CARTESIAN_POINT('Ctrl Pts',(-3.7330749481299,2.87088488312254,9.28307854933279));
#39858=CARTESIAN_POINT('Ctrl Pts',(-4.65151055959357,0.735716042020416,
9.3624504393862));
#39859=CARTESIAN_POINT('Ctrl Pts',(-4.43684849468422,-1.57867159843805,
9.4418223294396));
#39860=CARTESIAN_POINT('Ctrl Pts',(-3.14137995726738,-3.50849833184732,
9.52119421949301));
#39861=CARTESIAN_POINT('Ctrl Pts',(-1.08067821558679,-4.58366263754791,
9.6005661095464));
#39862=CARTESIAN_POINT('Ctrl Pts',(1.24327434737007,-4.54225687050701,9.67993799959982));
#39863=CARTESIAN_POINT('Ctrl Pts',(3.26436803124868,-3.39436738392564,9.75930988965321));
#39864=CARTESIAN_POINT('Ctrl Pts',(4.49026888827119,-1.41961751592476,9.83868177970662));
#39865=CARTESIAN_POINT('Ctrl Pts',(4.62235018315245,0.900948036685318,9.91805366976003));
#39866=CARTESIAN_POINT('Ctrl Pts',(3.62843720481635,3.00204464177353,9.99742555981342));
#39867=CARTESIAN_POINT('Ctrl Pts',(1.7506449547965,4.37184981703879,10.0767974498668));
#39868=CARTESIAN_POINT('Ctrl Pts',(-0.553600531224886,4.67668205379884,
10.1561693399202));
#39869=CARTESIAN_POINT('Ctrl Pts',(-2.72299015321387,3.84228489391363,10.2355412299736));
#39870=CARTESIAN_POINT('Ctrl Pts',(-4.22906540111646,2.07191563862441,10.314913120027));
#39871=CARTESIAN_POINT('Ctrl Pts',(-4.70494967818453,-0.203167680126261,
10.3942850100804));
#39872=CARTESIAN_POINT('Ctrl Pts',(-4.03471862787632,-2.42875980170217,
10.4736569001339));
#39873=CARTESIAN_POINT('Ctrl Pts',(-2.38163905051565,-4.06271141155209,
10.5530287901872));
#39874=CARTESIAN_POINT('Ctrl Pts',(-0.148397472117971,-4.70699551420709,
10.6324006802407));
#39875=CARTESIAN_POINT('Ctrl Pts',(2.12099340201542,-4.20466592835908,10.7117725702941));
#39876=CARTESIAN_POINT('Ctrl Pts',(3.87371497815709,-2.67808902923296,10.7911444603475));
#39877=CARTESIAN_POINT('Ctrl Pts',(4.68280815994238,-0.499135570435235,
10.8705163504009));
#39878=CARTESIAN_POINT('Ctrl Pts',(4.35117963918574,1.80140620850268,10.9498882404543));
#39879=CARTESIAN_POINT('Ctrl Pts',(2.95961338949625,3.66312942239435,11.0292601305077));
#39880=CARTESIAN_POINT('Ctrl Pts',(0.847091869118581,4.6325224171902,11.1086320205611));
#39881=CARTESIAN_POINT('Ctrl Pts',(-1.47177935557031,4.47344320507298,11.1880039106145));
#39882=CARTESIAN_POINT('Ctrl Pts',(-3.43212838697064,3.22464312999856,11.2673758006679));
#39883=CARTESIAN_POINT('Ctrl Pts',(-4.55641854019224,1.19032712608301,11.3467476907213));
#39884=CARTESIAN_POINT('Ctrl Pts',(-4.5707752224844,-1.13394993100199,11.4261195807747));
#39885=CARTESIAN_POINT('Ctrl Pts',(-3.47170117781866,-3.1819992948505,11.5054914708281));
#39886=CARTESIAN_POINT('Ctrl Pts',(-1.52692841071655,-4.45492067370938,
11.5848633608815));
#39887=CARTESIAN_POINT('Ctrl Pts',(0.789800737437414,-4.64263323725232,
11.6642352509349));
#39888=CARTESIAN_POINT('Ctrl Pts',(2.91413617414593,-3.69941062049495,11.7436071409883));
#39889=CARTESIAN_POINT('Ctrl Pts',(4.32859448916348,-1.85501976509151,11.8229790310417));
#39890=CARTESIAN_POINT('Ctrl Pts',(4.68861676780219,0.441249799071602,11.9023509210951));
#39891=CARTESIAN_POINT('Ctrl Pts',(3.90650237988148,2.63003188887072,11.9817228111485));
#39892=CARTESIAN_POINT('Ctrl Pts',(2.17277265911798,4.17814403201782,12.0610947012019));
#39893=CARTESIAN_POINT('Ctrl Pts',(-0.0902396720559702,4.70846953713027,
12.1404665912553));
#39894=CARTESIAN_POINT('Ctrl Pts',(-2.33126981885919,4.09182228501836,12.2198384813087));
#39895=CARTESIAN_POINT('Ctrl Pts',(-4.00440779796651,2.47841618137099,12.2992103713621));
#39896=CARTESIAN_POINT('Ctrl Pts',(-4.70208090109554,0.261273381822832,
12.3785822614155));
#39897=CARTESIAN_POINT('Ctrl Pts',(-4.25433750459725,-2.01951503521857,
12.4579541514689));
#39898=CARTESIAN_POINT('Ctrl Pts',(-2.7702469087954,-3.80835405980145,12.5373260415224));
#39899=CARTESIAN_POINT('Ctrl Pts',(-0.611330297848498,-4.66948646506541,
12.6166979315757));
#39900=CARTESIAN_POINT('Ctrl Pts',(1.69650502049761,-4.3931423031724,12.6960698216292));
#39901=CARTESIAN_POINT('Ctrl Pts',(3.59107547100067,-3.04663840028217,12.7754417116826));
#39902=CARTESIAN_POINT('Ctrl Pts',(4.61086788547872,-0.957980126702884,
12.854813601736));
#39903=CARTESIAN_POINT('Ctrl Pts',(4.50746308903707,1.36403998528818,12.9341854917894));
#39904=CARTESIAN_POINT('Ctrl Pts',(3.30605026120632,3.35378297611432,13.0135573818428));
#39905=CARTESIAN_POINT('Ctrl Pts',(1.29929090756384,4.52655185743172,13.0929292718962));
#39906=CARTESIAN_POINT('Ctrl Pts',(-1.02397283522957,4.59666272563134,13.1723011619496));
#39907=CARTESIAN_POINT('Ctrl Pts',(-3.09779906188647,3.54703672840752,13.251673052003));
#39908=CARTESIAN_POINT('Ctrl Pts',(-4.41700829392973,1.63336043537625,13.3310449420564));
#39909=CARTESIAN_POINT('Ctrl Pts',(-4.66024408245374,-0.67819884433063,
13.4104168321098));
#39910=CARTESIAN_POINT('Ctrl Pts',(-3.76825472776737,-2.82455038672626,
13.4897887221632));
#39911=CARTESIAN_POINT('Ctrl Pts',(-1.95832686228722,-4.28284770695163,
13.5691606122166));
#39912=CARTESIAN_POINT('Ctrl Pts',(0.328645092163131,-4.69785280568621,
13.64853250227));
#39913=CARTESIAN_POINT('Ctrl Pts',(2.53555982960612,-3.96847135947639,13.7279043923234));
#39914=CARTESIAN_POINT('Ctrl Pts',(4.12481780492351,-2.2723790741605,13.8072762823768));
#39915=CARTESIAN_POINT('Ctrl Pts',(4.7092792930909,-0.0227402762048894,
13.8866481724302));
#39916=CARTESIAN_POINT('Ctrl Pts',(4.14657076927425,2.23243800269952,13.9660200624836));
#39917=CARTESIAN_POINT('Ctrl Pts',(2.57376678434109,3.94379932556401,14.045391952537));
#39918=CARTESIAN_POINT('Ctrl Pts',(0.373998907678603,4.69445986217284,14.1247638425904));
#39919=CARTESIAN_POINT('Ctrl Pts',(-1.91687427506185,4.30156036736702,14.2041357326438));
#39920=CARTESIAN_POINT('Ctrl Pts',(-3.7408011273265,2.86081028841297,14.2835076226972));
#39921=CARTESIAN_POINT('Ctrl Pts',(-4.65347710509724,0.723173155497658,
14.3628795127506));
#39922=CARTESIAN_POINT('Ctrl Pts',(-4.43257636036315,-1.59062735738022,
14.442251402804));
#39923=CARTESIAN_POINT('Ctrl Pts',(-3.13190982558595,-3.51695456679423,
14.5216232928574));
#39924=CARTESIAN_POINT('Ctrl Pts',(-1.06831698966085,-4.58655942838405,
14.6009951829108));
#39925=CARTESIAN_POINT('Ctrl Pts',(1.25551550026611,-4.53888856539661,14.6803670729642));
#39926=CARTESIAN_POINT('Ctrl Pts',(3.27350719336465,-3.38555449453801,14.7597389630177));
#39927=CARTESIAN_POINT('Ctrl Pts',(4.49407977994485,-1.40750684260771,14.839110853071));
#39928=CARTESIAN_POINT('Ctrl Pts',(4.61990447960734,0.913406360718275,14.9184827431245));
#39929=CARTESIAN_POINT('Ctrl Pts',(3.62033067402261,3.01181579636398,14.9978546331779));
#39930=CARTESIAN_POINT('Ctrl Pts',(1.73885232971199,4.37655357055661,15.0772265232313));
#39931=CARTESIAN_POINT('Ctrl Pts',(-0.566206593232149,4.67517258229866,
15.1565984132847));
#39932=CARTESIAN_POINT('Ctrl Pts',(-2.73333884334193,3.83492990131171,15.2359703033381));
#39933=CARTESIAN_POINT('Ctrl Pts',(-4.23463580135657,2.06050678483865,15.3153421933915));
#39934=CARTESIAN_POINT('Ctrl Pts',(-4.70438485136804,-0.21585122356682,
15.3947140834449));
#39935=CARTESIAN_POINT('Ctrl Pts',(-4.02815616456562,-2.43962835168982,
15.4740859734983));
#39936=CARTESIAN_POINT('Ctrl Pts',(-2.3706775522472,-4.06911741336723,15.5534578635517));
#39937=CARTESIAN_POINT('Ctrl Pts',(-0.135707135607595,-4.70737847998642,
15.6328297536051));
#39938=CARTESIAN_POINT('Ctrl Pts',(2.13232123888424,-4.19893256848759,15.7122016436585));
#39939=CARTESIAN_POINT('Ctrl Pts',(3.88092087939525,-2.66763597748263,15.7915735337119));
#39940=CARTESIAN_POINT('Ctrl Pts',(4.6841367839613,-0.486509167079024,15.8709454237653));
#39941=CARTESIAN_POINT('Ctrl Pts',(4.34630733610955,1.81313019956284,15.9503173138187));
#39942=CARTESIAN_POINT('Ctrl Pts',(2.94972704158046,3.67109506287253,16.0296892038721));
#39943=CARTESIAN_POINT('Ctrl Pts',(0.834599768811967,4.63478929472454,16.1090610939255));
#39944=CARTESIAN_POINT('Ctrl Pts',(-1.48383416024523,4.46945911326284,16.1884329839789));
#39945=CARTESIAN_POINT('Ctrl Pts',(-3.44080937235088,3.21537858488636,16.2678048740323));
#39946=CARTESIAN_POINT('Ctrl Pts',(-4.55961103731638,1.17803895016983,16.3471767640857));
#39947=CARTESIAN_POINT('Ctrl Pts',(-4.5677015463797,-1.14626836492032,16.4265486541391));
#39948=CARTESIAN_POINT('Ctrl Pts',(-3.4631100686894,-3.19134724418507,16.5059205441925));
#39949=CARTESIAN_POINT('Ctrl Pts',(-1.51491264465833,-4.45902099747165,
16.5852924342459));
#39950=CARTESIAN_POINT('Ctrl Pts',(0.802314148161232,-4.64048710795702,
16.6646643242993));
#39951=CARTESIAN_POINT('Ctrl Pts',(2.92409898707282,-3.69154082613136,16.7440362143527));
#39952=CARTESIAN_POINT('Ctrl Pts',(4.33357979136326,-1.84334337837345,16.8234081044061));
#39953=CARTESIAN_POINT('Ctrl Pts',(4.68741013889918,0.453888451717908,16.9027799944596));
#39954=CARTESIAN_POINT('Ctrl Pts',(3.89939777427618,2.64055403030628,16.9821518845129));
#39955=CARTESIAN_POINT('Ctrl Pts',(2.16150070095874,4.18398654725935,17.0615237745663));
#39956=CARTESIAN_POINT('Ctrl Pts',(-0.102933079310061,4.70820909782832,
17.1408956646198));
#39957=CARTESIAN_POINT('Ctrl Pts',(-2.34229273922368,4.08552253105771,17.2202675546731));
#39958=CARTESIAN_POINT('Ctrl Pts',(-4.01107478934828,2.46761134605149,17.2996394447266));
#39959=CARTESIAN_POINT('Ctrl Pts',(-4.70276843368481,0.248596203073432,
17.37901133478));
#39960=CARTESIAN_POINT('Ctrl Pts',(-4.24887708766866,-2.03097775393694,
17.4583832248334));
#39961=CARTESIAN_POINT('Ctrl Pts',(-2.75997059360591,-3.81580751573978,
17.5377551148868));
#39962=CARTESIAN_POINT('Ctrl Pts',(-0.598737773532647,-4.6711197519463,
17.6171270049402));
#39963=CARTESIAN_POINT('Ctrl Pts',(1.70833944819094,-4.38854860755889,17.6964988949936));
#39964=CARTESIAN_POINT('Ctrl Pts',(3.5992817914533,-3.03695363259626,17.775870785047));
#39965=CARTESIAN_POINT('Ctrl Pts',(4.61342283197251,-0.945531571192997,
17.8552426751004));
#39966=CARTESIAN_POINT('Ctrl Pts',(4.50379002440264,1.37615964733967,17.9346145651538));
#39967=CARTESIAN_POINT('Ctrl Pts',(3.29695756540449,3.36273516855535,18.0139864552072));
#39968=CARTESIAN_POINT('Ctrl Pts',(1.28715662605536,4.52994106929151,18.0933583452606));
#39969=CARTESIAN_POINT('Ctrl Pts',(-1.03650075501039,4.59406889295398,18.172730235314));
#39970=CARTESIAN_POINT('Ctrl Pts',(-3.10708740551261,3.53832597274458,18.2521021253674));
#39971=CARTESIAN_POINT('Ctrl Pts',(-4.42189226956141,1.62210042840545,18.3314740154208));
#39972=CARTESIAN_POINT('Ctrl Pts',(-4.65746145505438,-0.691994213306935,
18.4108459054742));
#39973=CARTESIAN_POINT('Ctrl Pts',(-3.7623932789572,-2.83237457985889,18.4902177955276));
#39974=CARTESIAN_POINT('Ctrl Pts',(-1.94345928697736,-4.29245481019949,
18.569589685581));
#39975=CARTESIAN_POINT('Ctrl Pts',(0.335233909124166,-4.68912434583344,
18.6489615756345));
#39976=CARTESIAN_POINT('Ctrl Pts',(3.29668819545067,-3.73492805813089,18.7547907623723));
#39977=CARTESIAN_POINT('Ctrl Pts',(5.339103029404,-0.0175478502153651,18.8870772457947));
#39978=CARTESIAN_POINT('Ctrl Pts',(2.90621803008022,4.48249178265512,19.0458210259014));
#39979=CARTESIAN_POINT('Ctrl Pts',(-2.18656320946377,4.86959394496076,19.2045648060083));
#39980=CARTESIAN_POINT('Ctrl Pts',(-5.27828887711238,0.806568563691633,
19.363308586115));
#39981=CARTESIAN_POINT('Ctrl Pts',(-3.54020456892039,-3.99752392897296,
19.5220523662219));
#39982=CARTESIAN_POINT('Ctrl Pts',(1.43734916996113,-5.14215993940115,19.6807961463287));
#39983=CARTESIAN_POINT('Ctrl Pts',(5.09974667860479,-1.58211192901293,19.8395399264355));
#39984=CARTESIAN_POINT('Ctrl Pts',(4.09539160933933,3.42571876325583,19.9982837065423));
#39985=CARTESIAN_POINT('Ctrl Pts',(-0.656009676029552,5.29932988758688,
20.1570274866491));
#39986=CARTESIAN_POINT('Ctrl Pts',(-4.80798654830356,2.32253130646633,20.3157712667559));
#39987=CARTESIAN_POINT('Ctrl Pts',(-4.5587807483591,-2.77696271962182,20.4745150468627));
#39988=CARTESIAN_POINT('Ctrl Pts',(-0.141143605831918,-5.34031031892967,
20.6332588269695));
#39989=CARTESIAN_POINT('Ctrl Pts',(4.41154214902265,-3.00742829557661,20.7920026070763));
#39990=CARTESIAN_POINT('Ctrl Pts',(4.83176599740626,1.2132097937891,20.9242890904987));
#39991=CARTESIAN_POINT('Ctrl Pts',(2.93038174053082,3.67602118591258,21.0301182772365));
#39992=CARTESIAN_POINT('Ctrl Pts',(0.82729199276626,4.63872722375956,21.1094901672899));
#39993=CARTESIAN_POINT('Ctrl Pts',(-1.49865065220701,4.46452630956661,21.1888620573433));
#39994=CARTESIAN_POINT('Ctrl Pts',(-3.44799414715959,3.20657754587673,21.2682339473967));
#39995=CARTESIAN_POINT('Ctrl Pts',(-4.56354990278301,1.16548416044547,21.3476058374502));
#39996=CARTESIAN_POINT('Ctrl Pts',(-4.56418179760212,-1.1584417781363,21.4269777275035));
#39997=CARTESIAN_POINT('Ctrl Pts',(-3.45471245456607,-3.20074439226419,
21.506349617557));
#39998=CARTESIAN_POINT('Ctrl Pts',(-1.50277006074114,-4.46305057284728,
21.5857215076104));
#39999=CARTESIAN_POINT('Ctrl Pts',(0.814760394348267,-4.63832755437973,
21.6650933976638));
#40000=CARTESIAN_POINT('Ctrl Pts',(2.93407303175,-3.6836334512587,21.7444652877172));
#40001=CARTESIAN_POINT('Ctrl Pts',(4.33851638857388,-1.83165928184362,21.8238371777706));
#40002=CARTESIAN_POINT('Ctrl Pts',(4.68617856238765,0.466526807638465,21.903209067824));
#40003=CARTESIAN_POINT('Ctrl Pts',(3.89225998228531,2.65105540897445,21.9825809578774));
#40004=CARTESIAN_POINT('Ctrl Pts',(2.1502156260726,4.18979944864558,22.0619528479308));
#40005=CARTESIAN_POINT('Ctrl Pts',(-0.115627163561327,4.70791408521783,
22.1413247379842));
#40006=CARTESIAN_POINT('Ctrl Pts',(-2.35329778315663,4.07919314165102,22.2206966280376));
#40007=CARTESIAN_POINT('Ctrl Pts',(-4.01771326340777,2.45678878743819,22.300068518091));
#40008=CARTESIAN_POINT('Ctrl Pts',(-4.7034211013359,0.235916647177708,22.3794404081444));
#40009=CARTESIAN_POINT('Ctrl Pts',(-4.24338680893675,-2.04242454395301,
22.4588122981978));
#40010=CARTESIAN_POINT('Ctrl Pts',(-2.74967243806091,-3.82323548987737,
22.5381841882512));
#40011=CARTESIAN_POINT('Ctrl Pts',(-0.586144182924564,-4.67271481097619,
22.6175560783046));
#40012=CARTESIAN_POINT('Ctrl Pts',(1.7201676224087,-4.38393110573301,22.696927968358));
#40013=CARTESIAN_POINT('Ctrl Pts',(3.60745033643733,-3.02723150865538,22.7762998584114));
#40014=CARTESIAN_POINT('Ctrl Pts',(4.61596616842609,-0.933105005158016,
22.8556717484649));
#40015=CARTESIAN_POINT('Ctrl Pts',(4.50004284053894,1.38832380607303,22.9350436385182));
#40016=CARTESIAN_POINT('Ctrl Pts',(3.28791904717806,3.37156001439376,23.0144155285717));
#40017=CARTESIAN_POINT('Ctrl Pts',(1.27486544641681,4.53349166431032,23.093787418625));
#40018=CARTESIAN_POINT('Ctrl Pts',(-1.04874255247445,4.59107478042505,23.1731593086785));
#40019=CARTESIAN_POINT('Ctrl Pts',(-3.11687918839179,3.53028224171763,23.2525311987318));
#40020=CARTESIAN_POINT('Ctrl Pts',(-4.42575095234051,1.60952076333037,23.3319030887853));
#40021=CARTESIAN_POINT('Ctrl Pts',(-4.6565195809412,-0.703316410525592,
23.4112749788386));
#40022=CARTESIAN_POINT('Ctrl Pts',(-3.75297034643954,-2.84482726347037,
23.4906468688921));
#40023=CARTESIAN_POINT('Ctrl Pts',(-1.93520584271877,-4.29334449199004,
23.5700187589454));
#40024=CARTESIAN_POINT('Ctrl Pts',(0.353970520843478,-4.69601250539774,
23.6493906489989));
#40025=CARTESIAN_POINT('Ctrl Pts',(2.55692044899663,-3.95474226694855,23.7287625390522));
#40026=CARTESIAN_POINT('Ctrl Pts',(4.13701021543862,-2.25010556593857,23.8081344291057));
#40027=CARTESIAN_POINT('Ctrl Pts',(4.70933345050753,0.00265187040687223,
23.887506319159));
#40028=CARTESIAN_POINT('Ctrl Pts',(4.13447348097035,2.25476331699259,23.9668782092125));
#40029=CARTESIAN_POINT('Ctrl Pts',(2.55246492296808,3.95761941039203,24.0462500992659));
#40030=CARTESIAN_POINT('Ctrl Pts',(0.348681559517371,4.69640817546236,24.1256219893193));
#40031=CARTESIAN_POINT('Ctrl Pts',(-1.94003986003887,4.29116230431301,24.2049938793727));
#40032=CARTESIAN_POINT('Ctrl Pts',(-3.75617186389469,2.84059879415982,24.2843657694261));
#40033=CARTESIAN_POINT('Ctrl Pts',(-4.65730871585138,0.698071705307978,
24.3637376594795));
#40034=CARTESIAN_POINT('Ctrl Pts',(-4.42393547340455,-1.61450410580135,
24.4431095495329));
#40035=CARTESIAN_POINT('Ctrl Pts',(-3.11290134185147,-3.5337902903817,24.5224814395863));
#40036=CARTESIAN_POINT('Ctrl Pts',(-1.0435713337136,-4.59225298213718,24.6018533296397));
#40037=CARTESIAN_POINT('Ctrl Pts',(1.27997034141094,-4.5320530122236,24.6812252196931));
#40038=CARTESIAN_POINT('Ctrl Pts',(3.29171407453406,-3.36785496006151,24.7605971097465));
#40039=CARTESIAN_POINT('Ctrl Pts',(4.50160354518617,-1.38325489424899,24.8399689997999));
#40040=CARTESIAN_POINT('Ctrl Pts',(4.61491235636141,0.938303002019797,24.9193408898533));
#40041=CARTESIAN_POINT('Ctrl Pts',(3.60403873246226,3.03129236389504,24.9987127799067));
#40042=CARTESIAN_POINT('Ctrl Pts',(1.71522925073975,4.3858656155773,25.0780846699601));
#40043=CARTESIAN_POINT('Ctrl Pts',(-0.591406279867446,4.67205171125385,
25.1574565600135));
#40044=CARTESIAN_POINT('Ctrl Pts',(-2.75397654975454,3.82013635147998,25.2368284500669));
#40045=CARTESIAN_POINT('Ctrl Pts',(-4.2456842279451,2.03764423221396,25.3162003401203));
#40046=CARTESIAN_POINT('Ctrl Pts',(-4.70315262587087,-0.24121351177037,
25.3955722301737));
#40047=CARTESIAN_POINT('Ctrl Pts',(-4.01494345438624,-2.4613121782045,25.4749441202271));
#40048=CARTESIAN_POINT('Ctrl Pts',(-2.34870294433969,-4.08184064605008,
25.5543160102806));
#40049=CARTESIAN_POINT('Ctrl Pts',(-0.110323595817837,-4.70804176751889,
25.6336879003339));
#40050=CARTESIAN_POINT('Ctrl Pts',(2.15493033644811,-4.1873743354938,25.7130597903874));
#40051=CARTESIAN_POINT('Ctrl Pts',(3.89524800861274,-2.64667178393831,25.7924316804407));
#40052=CARTESIAN_POINT('Ctrl Pts',(4.68669188786451,-0.461245844124039,
25.8718035704942));
#40053=CARTESIAN_POINT('Ctrl Pts',(4.33646799704899,1.83653856236848,25.9511754605475));
#40054=CARTESIAN_POINT('Ctrl Pts',(2.92989010076147,3.68694624017715,26.030547350601));
#40055=CARTESIAN_POINT('Ctrl Pts',(0.809597461130217,4.63922197479579,26.1099192406544));
#40056=CARTESIAN_POINT('Ctrl Pts',(-1.50791132801882,4.46139350509784,26.1892911307078));
#40057=CARTESIAN_POINT('Ctrl Pts',(-3.45809625536759,3.19677945268506,26.2686630207611));
#40058=CARTESIAN_POINT('Ctrl Pts',(-4.56589658927499,1.15343700154949,26.3480349108146));
#40059=CARTESIAN_POINT('Ctrl Pts',(-4.56145462047572,-1.170880150074,26.427406800868));
#40060=CARTESIAN_POINT('Ctrl Pts',(-3.44585240273711,-3.20997348883872,
26.5067786909214));
#40061=CARTESIAN_POINT('Ctrl Pts',(-1.49084816695666,-4.46712439087817,
26.5861505809748));
#40062=CARTESIAN_POINT('Ctrl Pts',(0.827323382358012,-4.6360936791118,26.6655224710282));
#40063=CARTESIAN_POINT('Ctrl Pts',(2.9439607869795,-3.67572080893307,26.7448943610816));
#40064=CARTESIAN_POINT('Ctrl Pts',(4.34345586023946,-1.81995048576826,26.824266251135));
#40065=CARTESIAN_POINT('Ctrl Pts',(4.68489470002155,0.479155747337646,26.9036381411885));
#40066=CARTESIAN_POINT('Ctrl Pts',(3.88510356071688,2.66154070098535,26.9830100312418));
#40067=CARTESIAN_POINT('Ctrl Pts',(2.13890979355249,4.1955802310934,27.0623819212952));
#40068=CARTESIAN_POINT('Ctrl Pts',(-0.128317664924755,4.70758570366646,
27.1417538113486));
#40069=CARTESIAN_POINT('Ctrl Pts',(-2.36428722425266,4.07283371889059,27.221125701402));
#40070=CARTESIAN_POINT('Ctrl Pts',(-4.02432164901364,2.44594845525754,27.3004975914554));
#40071=CARTESIAN_POINT('Ctrl Pts',(-4.70404022775981,0.223235561938782,
27.3798694815088));
#40072=CARTESIAN_POINT('Ctrl Pts',(-4.2378650192401,-2.05385702014473,27.4592413715622));
#40073=CARTESIAN_POINT('Ctrl Pts',(-2.73935527238859,-3.83063457825638,
27.5386132616157));
#40074=CARTESIAN_POINT('Ctrl Pts',(-0.573544644643281,-4.67427803207058,
27.617985151669));
#40075=CARTESIAN_POINT('Ctrl Pts',(1.73198018901762,-4.37927770361132,27.6973570417225));
#40076=CARTESIAN_POINT('Ctrl Pts',(3.61559848230692,-3.01749501991908,27.7767289317758));
#40077=CARTESIAN_POINT('Ctrl Pts',(4.61846498829774,-0.920657228486544,
27.8561008218292));
#40078=CARTESIAN_POINT('Ctrl Pts',(4.49628364593812,1.4004506259651,27.9354727118827));
#40079=CARTESIAN_POINT('Ctrl Pts',(3.278817559783,3.38041180777658,28.014844601936));
#40080=CARTESIAN_POINT('Ctrl Pts',(1.2626387736043,4.53691215562828,28.0942164919895));
#40081=CARTESIAN_POINT('Ctrl Pts',(-1.0611160230209,4.58823074465364,28.1735883820429));
#40082=CARTESIAN_POINT('Ctrl Pts',(-3.12638530517863,3.52186648015787,28.2529602720962));
#40083=CARTESIAN_POINT('Ctrl Pts',(-4.43007404713138,1.59758333661492,28.3323321621497));
#40084=CARTESIAN_POINT('Ctrl Pts',(-4.65460655700551,-0.715867571536754,
28.4117040522031));
#40085=CARTESIAN_POINT('Ctrl Pts',(-3.74528721238995,-2.85493472380806,
28.4910759422565));
#40086=CARTESIAN_POINT('Ctrl Pts',(-1.9236241928888,-4.29854609665053,28.5704478323099));
#40087=CARTESIAN_POINT('Ctrl Pts',(0.366629422130075,-4.69504115501931,
28.6498197223633));
#40088=CARTESIAN_POINT('Ctrl Pts',(2.56757292143854,-3.94783458032276,28.7291916124167));
#40089=CARTESIAN_POINT('Ctrl Pts',(4.14306134031087,-2.23894424024318,28.8085635024701));
#40090=CARTESIAN_POINT('Ctrl Pts',(4.70930918719419,0.0153479609406268,
28.8879353925235));
#40091=CARTESIAN_POINT('Ctrl Pts',(4.12837973995606,2.26590143281143,28.9673072825769));
#40092=CARTESIAN_POINT('Ctrl Pts',(2.54178612607819,3.96448633113712,29.0466791726303));
#40093=CARTESIAN_POINT('Ctrl Pts',(0.336019038035816,4.69733113443944,29.1260510626837));
#40094=CARTESIAN_POINT('Ctrl Pts',(-1.95160154390656,4.2859164707584,29.2054229527371));
#40095=CARTESIAN_POINT('Ctrl Pts',(-3.76381630954999,2.83046204151583,29.2847948427905));
#40096=CARTESIAN_POINT('Ctrl Pts',(-4.65917375325318,0.68551332408149,29.364166732844));
#40097=CARTESIAN_POINT('Ctrl Pts',(-4.41956678357008,-1.62642492174114,
29.4435386228973));
#40098=CARTESIAN_POINT('Ctrl Pts',(-3.10336312795443,-3.54216965665813,
29.5229105129507));
#40099=CARTESIAN_POINT('Ctrl Pts',(-1.03118708354684,-4.59504970367272,
29.6022824030041));
#40100=CARTESIAN_POINT('Ctrl Pts',(1.29218385191882,-4.52858581384264,29.6816542930575));
#40101=CARTESIAN_POINT('Ctrl Pts',(3.30078166125751,-3.3589684436152,29.761026183111));
#40102=CARTESIAN_POINT('Ctrl Pts',(4.50531636407018,-1.37111379547362,29.8403980731643));
#40103=CARTESIAN_POINT('Ctrl Pts',(4.61236597294397,0.950741138336453,29.9197699632178));
#40104=CARTESIAN_POINT('Ctrl Pts',(3.59585344010749,3.04099763527755,29.9991418532711));
#40105=CARTESIAN_POINT('Ctrl Pts',(1.70339896854746,4.39047383939912,30.0785137433246));
#40106=CARTESIAN_POINT('Ctrl Pts',(-0.603999721341074,4.67044033439209,
30.157885633378));
#40107=CARTESIAN_POINT('Ctrl Pts',(-2.76426541604165,3.81269790177148,30.2372575234314));
#40108=CARTESIAN_POINT('Ctrl Pts',(-4.25116217399222,2.02619069954299,30.3166294134847));
#40109=CARTESIAN_POINT('Ctrl Pts',(-4.70248523614609,-0.253892072197153,
30.3960013035382));
#40110=CARTESIAN_POINT('Ctrl Pts',(-4.00829330354932,-2.47212729713062,
30.4753731935915));
#40111=CARTESIAN_POINT('Ctrl Pts',(-2.33768999441463,-4.08815778444404,
30.554745083645));
#40112=CARTESIAN_POINT('Ctrl Pts',(-0.0976305770295779,-4.70832208445062,
30.6341169736984));
#40113=CARTESIAN_POINT('Ctrl Pts',(2.16621143281822,-4.18154954637921,30.7134888637517));
#40114=CARTESIAN_POINT('Ctrl Pts',(3.90236913245919,-2.63616079451278,30.7928607538052));
#40115=CARTESIAN_POINT('Ctrl Pts',(4.68791834918069,-0.448609108145992,
30.8722326438586));
#40116=CARTESIAN_POINT('Ctrl Pts',(4.33150103257305,1.84822276398574,30.951604533912));
#40117=CARTESIAN_POINT('Ctrl Pts',(2.91993965204555,3.69483166178228,31.0309764239654));
#40118=CARTESIAN_POINT('Ctrl Pts',(0.797087435456495,4.64138774513982,31.1103483140188));
#40119=CARTESIAN_POINT('Ctrl Pts',(-1.51993351608663,4.45731204731877,31.1897202040722));
#40120=CARTESIAN_POINT('Ctrl Pts',(-3.46670202742684,3.18744500086376,31.2690920941256));
#40121=CARTESIAN_POINT('Ctrl Pts',(-4.56898959830062,1.14112340748814,31.348463984179));
#40122=CARTESIAN_POINT('Ctrl Pts',(-4.5582814163153,-1.18317332211776,31.4278358742324));
#40123=CARTESIAN_POINT('Ctrl Pts',(-3.43718597090036,-3.21925164936547,
31.5072077642858));
#40124=CARTESIAN_POINT('Ctrl Pts',(-1.47879963105622,-4.47112740052042,
31.5865796543392));
#40125=CARTESIAN_POINT('Ctrl Pts',(0.839819025645787,-4.63384641358128,
31.6659515443926));
#40126=CARTESIAN_POINT('Ctrl Pts',(2.95385962660838,-3.66777069713875,31.745323434446));
#40127=CARTESIAN_POINT('Ctrl Pts',(4.34834656078651,-1.80823415734596,31.8246953244994));
#40128=CARTESIAN_POINT('Ctrl Pts',(4.68358589765892,0.491784220717852,31.9040672145528));
#40129=CARTESIAN_POINT('Ctrl Pts',(3.87791407680318,2.67200505116071,31.9834391046062));
#40130=CARTESIAN_POINT('Ctrl Pts',(2.12759097045539,4.20133136552371,32.0628109946597));
#40131=CARTESIAN_POINT('Ctrl Pts',(-0.141008586952624,4.70722265873437,
32.142182884713));
#40132=CARTESIAN_POINT('Ctrl Pts',(-2.37525876469618,4.06644493153793,32.2215547747665));
#40133=CARTESIAN_POINT('Ctrl Pts',(-4.03090116490581,2.43509021994207,32.3009266648198));
#40134=CARTESIAN_POINT('Ctrl Pts',(-4.7046249635928,0.21055292074912,32.3802985548733));
#40135=CARTESIAN_POINT('Ctrl Pts',(-4.23231253465933,-2.06527460388738,
32.4596704449267));
#40136=CARTESIAN_POINT('Ctrl Pts',(-2.72901814034772,-3.83800580642471,
32.5390423349801));
#40137=CARTESIAN_POINT('Ctrl Pts',(-0.560940967626579,-4.67580728979871,
32.6184142250335));
#40138=CARTESIAN_POINT('Ctrl Pts',(1.74378018318661,-4.37459246710163,32.6977861150869));
#40139=CARTESIAN_POINT('Ctrl Pts',(3.62372034116752,-3.00773660241476,32.7771580051403));
#40140=CARTESIAN_POINT('Ctrl Pts',(4.62093024500891,-0.90820275889168,32.8565298951936));
#40141=CARTESIAN_POINT('Ctrl Pts',(4.49249176942175,1.41256726642465,32.9359017852471));
#40142=CARTESIAN_POINT('Ctrl Pts',(3.26969224276534,3.38923903230456,33.0152736753005));
#40143=CARTESIAN_POINT('Ctrl Pts',(1.25040292311233,4.54029967186844,33.0946455653539));
#40144=CARTESIAN_POINT('Ctrl Pts',(-1.0734817808909,4.58535336114807,33.1740174554073));
#40145=CARTESIAN_POINT('Ctrl Pts',(-3.13586869918079,3.51342512115953,33.2533893454607));
#40146=CARTESIAN_POINT('Ctrl Pts',(-4.43436494347784,1.58563429849111,33.3327612355141));
#40147=CARTESIAN_POINT('Ctrl Pts',(-4.65265970284399,-0.728413529547759,
33.4121331255675));
#40148=CARTESIAN_POINT('Ctrl Pts',(-3.73757685708491,-2.8650214341048,33.4915050156209));
#40149=CARTESIAN_POINT('Ctrl Pts',(-1.91202856192598,-4.30371645893127,
33.5708769056743));
#40150=CARTESIAN_POINT('Ctrl Pts',(0.379285658714694,-4.69403568047687,
33.6502487957277));
#40151=CARTESIAN_POINT('Ctrl Pts',(2.57820673242699,-3.94089820033005,33.7296206857811));
#40152=CARTESIAN_POINT('Ctrl Pts',(4.14908235288389,-2.22776664161308,33.8089925758346));
#40153=CARTESIAN_POINT('Ctrl Pts',(4.70925069601633,0.0280439399230538,
33.8883644658879));
#40154=CARTESIAN_POINT('Ctrl Pts',(4.12225599334877,2.27702307976815,33.9677363559414));
#40155=CARTESIAN_POINT('Ctrl Pts',(2.53108885516031,3.9713244374868,34.0471082459947));
#40156=CARTESIAN_POINT('Ctrl Pts',(0.323354074324944,4.69821995261122,34.1264801360482));
#40157=CARTESIAN_POINT('Ctrl Pts',(-1.96314904328387,4.28063948661298,34.2058520261016));
#40158=CARTESIAN_POINT('Ctrl Pts',(-3.77143339930544,2.8203047167106,34.2852239161549));
#40159=CARTESIAN_POINT('Ctrl Pts',(-4.66100492718239,0.672949960456159,
34.3645958062084));
#40160=CARTESIAN_POINT('Ctrl Pts',(-4.41516597175719,-1.63833391661592,
34.4439676962618));
#40161=CARTESIAN_POINT('Ctrl Pts',(-3.09380235841604,-3.55052327799099,
34.5233395863151));
#40162=CARTESIAN_POINT('Ctrl Pts',(-1.01879533858015,-4.59781302779744,
34.6027114763686));
#40163=CARTESIAN_POINT('Ctrl Pts',(1.30438797066869,-4.52508570111899,34.6820833664219));
#40164=CARTESIAN_POINT('Ctrl Pts',(3.30982525747642,-3.35005751375522,34.7614552564754));
#40165=CARTESIAN_POINT('Ctrl Pts',(4.50899643773683,-1.3589627312672,34.8408271465288));
#40166=CARTESIAN_POINT('Ctrl Pts',(4.60978606625886,0.963172364544519,34.9201990365822));
#40167=CARTESIAN_POINT('Ctrl Pts',(3.58764201262861,3.05068080429907,34.9995709266356));
#40168=CARTESIAN_POINT('Ctrl Pts',(1.69155630583291,4.39505015269376,35.078942816689));
#40169=CARTESIAN_POINT('Ctrl Pts',(-0.616588772867267,4.66879501217076,
35.1583147067424));
#40170=CARTESIAN_POINT('Ctrl Pts',(-2.77453419129308,3.80523174088547,35.2376865967958));
#40171=CARTESIAN_POINT('Ctrl Pts',(-4.2566092220472,2.01472244025804,35.3170584868492));
#40172=CARTESIAN_POINT('Ctrl Pts',(-4.70178366815532,-0.266568787303772,
35.3964303769026));
#40173=CARTESIAN_POINT('Ctrl Pts',(-4.00161401992238,-2.48292444831838,
35.475802266956));
#40174=CARTESIAN_POINT('Ctrl Pts',(-2.3266600538588,-4.09444520958265,35.5551741570094));
#40175=CARTESIAN_POINT('Ctrl Pts',(-0.0849368486498902,-4.70856818069336,
35.6345460470628));
#40176=CARTESIAN_POINT('Ctrl Pts',(2.17747678488564,-4.17569436522607,35.7139179371162));
#40177=CARTESIAN_POINT('Ctrl Pts',(3.90946189338614,-2.62563064513239,35.7932898271696));
#40178=CARTESIAN_POINT('Ctrl Pts',(4.68911073810487,-0.435969111619298,
35.872661717223));
#40179=CARTESIAN_POINT('Ctrl Pts',(4.32650258619184,1.85989353248294,35.9520336072764));
#40180=CARTESIAN_POINT('Ctrl Pts',(2.90996798083354,3.70269022887686,36.0314054973299));
#40181=CARTESIAN_POINT('Ctrl Pts',(0.784571616449035,4.64351978128221,36.1107773873832));
#40182=CARTESIAN_POINT('Ctrl Pts',(-1.53194465708265,4.4531981932239,36.1901492774366));
#40183=CARTESIAN_POINT('Ctrl Pts',(-3.47528260305097,3.17808738228323,36.2695211674901));
#40184=CARTESIAN_POINT('Ctrl Pts',(-4.57204939932363,1.12880151959547,36.3488930575434));
#40185=CARTESIAN_POINT('Ctrl Pts',(-4.55507508198074,-1.19545789470598,
36.4282649475969));
#40186=CARTESIAN_POINT('Ctrl Pts',(-3.42849455715498,-3.2285064119582,36.5076368376502));
#40187=CARTESIAN_POINT('Ctrl Pts',(-1.4667403470503,-4.47509791343512,36.5870087277037));
#40188=CARTESIAN_POINT('Ctrl Pts',(0.852308565021146,-4.63156546866048,
36.6663806177571));
#40189=CARTESIAN_POINT('Ctrl Pts',(2.96373699720644,-3.65979392751645,36.7457525078104));
#40190=CARTESIAN_POINT('Ctrl Pts',(4.35320565699285,-1.79650468644589,36.8251243978639));
#40191=CARTESIAN_POINT('Ctrl Pts',(4.68224305439311,0.504409119747259,36.9044962879172));
#40192=CARTESIAN_POINT('Ctrl Pts',(3.87069640771237,2.68244998086059,36.9838681779707));
#40193=CARTESIAN_POINT('Ctrl Pts',(2.1162566837541,4.20705196413867,37.0632400680241));
#40194=CARTESIAN_POINT('Ctrl Pts',(-0.153698484112011,4.70682540110399,
37.1426119580775));
#40195=CARTESIAN_POINT('Ctrl Pts',(-2.38621304145417,4.06002658874194,37.2219838481309));
#40196=CARTESIAN_POINT('Ctrl Pts',(-4.03745138369124,2.42421428607825,37.3013557381843));
#40197=CARTESIAN_POINT('Ctrl Pts',(-4.7051755056078,0.197868749234187,37.3807276282377));
#40198=CARTESIAN_POINT('Ctrl Pts',(-4.22672928908836,-2.07667717695002,
37.4600995182911));
#40199=CARTESIAN_POINT('Ctrl Pts',(-2.71866117345227,-3.84534913947293,
37.5394714083445));
#40200=CARTESIAN_POINT('Ctrl Pts',(-0.548333213620079,-4.67730256316236,
37.6188432983979));
#40201=CARTESIAN_POINT('Ctrl Pts',(1.75556750333961,-4.36987543548734,37.6982151884513));
#40202=CARTESIAN_POINT('Ctrl Pts',(3.63181586235974,-2.99795632430491,37.7775870785047));
#40203=CARTESIAN_POINT('Ctrl Pts',(4.62336191621364,-0.895741688343936,
37.8569589685581));
#40204=CARTESIAN_POINT('Ctrl Pts',(4.48866724088475,1.42467364012841,37.9363308586115));
#40205=CARTESIAN_POINT('Ctrl Pts',(3.26054316123161,3.3980416234756,38.0157027486649));
#40206=CARTESIAN_POINT('Ctrl Pts',(1.23815798448111,4.54365418850126,38.0950746387183));
#40207=CARTESIAN_POINT('Ctrl Pts',(-1.08583973646279,4.58244265094544,38.1744465287717));
#40208=CARTESIAN_POINT('Ctrl Pts',(-3.1453293014664,3.50495822568428,38.2538184188251));
#40209=CARTESIAN_POINT('Ctrl Pts',(-4.43862360995231,1.57367373662757,38.3331903088785));
#40210=CARTESIAN_POINT('Ctrl Pts',(-4.65067903319431,-0.740954194968168,
38.412562198932));
#40211=CARTESIAN_POINT('Ctrl Pts',(-3.72983933538423,-2.87508731801368,
38.4919340889853));
#40212=CARTESIAN_POINT('Ctrl Pts',(-1.9004190363744,-4.30885554699714,38.5713059790388));
#40213=CARTESIAN_POINT('Ctrl Pts',(0.391939142907767,-4.69299607822647,
38.6506778690921));
#40214=CARTESIAN_POINT('Ctrl Pts',(2.588821796549,-3.93393319787887,38.7300497591456));
#40215=CARTESIAN_POINT('Ctrl Pts',(4.15507322474385,-2.21657281258971,38.8094216491989));
#40216=CARTESIAN_POINT('Ctrl Pts',(4.70915794841682,0.040739642006525,38.8887935392524));
#40217=CARTESIAN_POINT('Ctrl Pts',(4.11610234038245,2.28812831500406,38.9681654293058));
#40218=CARTESIAN_POINT('Ctrl Pts',(2.52037308462918,3.97813341921603,39.0475373193591));
#40219=CARTESIAN_POINT('Ctrl Pts',(0.310686955552019,4.69907511544173,39.1269092094126));
#40220=CARTESIAN_POINT('Ctrl Pts',(-1.97468264266246,4.27533046137757,39.2062810994659));
#40221=CARTESIAN_POINT('Ctrl Pts',(-3.77902238214566,2.81012864743349,39.2856529895194));
#40222=CARTESIAN_POINT('Ctrl Pts',(-4.66280353786911,0.660378394081937,
39.3650248795728));
#40223=CARTESIAN_POINT('Ctrl Pts',(-4.41073058968569,-1.65022475069991,
39.4443967696262));
#40224=CARTESIAN_POINT('Ctrl Pts',(-3.0842237862698,-3.55886290155649,39.5237686596796));
#40225=CARTESIAN_POINT('Ctrl Pts',(-1.00638734295308,-4.60052063353569,
39.603140549733));
#40226=CARTESIAN_POINT('Ctrl Pts',(1.3165658861068,-4.521594850557,39.6825124397864));
#40227=CARTESIAN_POINT('Ctrl Pts',(3.31887653668104,-3.34104229843822,39.7618843298398));
#40228=CARTESIAN_POINT('Ctrl Pts',(4.51258247789865,-1.34695556252384,39.8412562198932));
#40229=CARTESIAN_POINT('Ctrl Pts',(4.60729903172253,0.975909964327458,39.9206281099466));
#40230=CARTESIAN_POINT('Ctrl Pts',(3.92183073605334,2.36502208507764,39.9735427033156));
#40231=CARTESIAN_POINT('Ctrl Pts',(3.43378788736169,2.9358415841302,40.));
#40232=CARTESIAN_POINT('Ctrl Pts',(4.5177656910975,-0.000116631996953637,
0.887416697508071));
#40233=CARTESIAN_POINT('Ctrl Pts',(4.51716522512143,0.582848551743655,0.907954496247182));
#40234=CARTESIAN_POINT('Ctrl Pts',(4.40381632429852,1.16604045169665,0.928492294986294));
#40235=CARTESIAN_POINT('Ctrl Pts',(4.18378127438632,1.70573618195762,0.949030093725405));
#40236=CARTESIAN_POINT('Ctrl Pts',(3.90032671966707,2.40098547504095,0.975487390409873));
#40237=CARTESIAN_POINT('Ctrl Pts',(3.43982409908107,3.02405189544283,1.00194468709434));
#40238=CARTESIAN_POINT('Ctrl Pts',(2.85836212737567,3.49904666560206,1.02840198377881));
#40239=CARTESIAN_POINT('Ctrl Pts',(2.27690015567027,3.97404143576128,1.05485928046328));
#40240=CARTESIAN_POINT('Ctrl Pts',(1.57447883284546,4.30096455567785,1.08131657714775));
#40241=CARTESIAN_POINT('Ctrl Pts',(0.83665229586908,4.43999713904637,1.10777387383221));
#40242=CARTESIAN_POINT('Ctrl Pts',(0.0988257588927,4.57902972241489,1.13423117051668));
#40243=CARTESIAN_POINT('Ctrl Pts',(-0.674405992235245,4.53017176923536,
1.16068846720115));
#40244=CARTESIAN_POINT('Ctrl Pts',(-1.38886418452507,4.29937413054889,1.18714576388562));
#40245=CARTESIAN_POINT('Ctrl Pts',(-2.1033223768149,4.06857649186242,1.21360306057009));
#40246=CARTESIAN_POINT('Ctrl Pts',(-2.7590070102666,3.65583916766901,1.24006035725455));
#40247=CARTESIAN_POINT('Ctrl Pts',(-3.27605642296673,3.11143310386793,1.26651765393902));
#40248=CARTESIAN_POINT('Ctrl Pts',(-3.79310583566684,2.56702704006687,1.29297495062349));
#40249=CARTESIAN_POINT('Ctrl Pts',(-4.17152002761538,1.89095223665816,1.31943224730795));
#40250=CARTESIAN_POINT('Ctrl Pts',(-4.36520856862574,1.16555385826357,1.34588954399242));
#40251=CARTESIAN_POINT('Ctrl Pts',(-4.5588971096361,0.440155479868968,1.37234684067689));
#40252=CARTESIAN_POINT('Ctrl Pts',(-4.56785999970828,-0.334566473511511,
1.39880413736136));
#40253=CARTESIAN_POINT('Ctrl Pts',(-4.39100556896818,-1.06425172631823,
1.42526143404583));
#40254=CARTESIAN_POINT('Ctrl Pts',(-4.21415113822807,-1.79393697912495,
1.4517187307303));
#40255=CARTESIAN_POINT('Ctrl Pts',(-3.85147938667567,-2.4785855313579,1.47817602741476));
#40256=CARTESIAN_POINT('Ctrl Pts',(-3.3471633321549,-3.03480794657228,1.50463332409923));
#40257=CARTESIAN_POINT('Ctrl Pts',(-2.84284727763412,-3.59103036178665,
1.5310906207837));
#40258=CARTESIAN_POINT('Ctrl Pts',(-2.19688692014498,-4.01882663998244,
1.55754791746817));
#40259=CARTESIAN_POINT('Ctrl Pts',(-1.48795951638605,-4.26609166819824,
1.58400521415264));
#40260=CARTESIAN_POINT('Ctrl Pts',(-0.779032112627116,-4.51335669641404,
1.6104625108371));
#40261=CARTESIAN_POINT('Ctrl Pts',(-0.0071376625983989,-4.58009047464984,
1.63691980752157));
#40262=CARTESIAN_POINT('Ctrl Pts',(0.733707943998554,-4.4581649024313,1.66337710420604));
#40263=CARTESIAN_POINT('Ctrl Pts',(1.47455355059551,-4.33623933021276,1.68983440089051));
#40264=CARTESIAN_POINT('Ctrl Pts',(2.18435031376069,-4.02565440753988,1.71629169757498));
#40265=CARTESIAN_POINT('Ctrl Pts',(2.77664577327776,-3.56423903433516,1.74274899425944));
#40266=CARTESIAN_POINT('Ctrl Pts',(3.36894123279483,-3.10282366113044,1.76920629094391));
#40267=CARTESIAN_POINT('Ctrl Pts',(3.84373538866378,-2.49057783739389,1.79566358762838));
#40268=CARTESIAN_POINT('Ctrl Pts',(4.14319883817832,-1.80207242682533,1.82212088431285));
#40269=CARTESIAN_POINT('Ctrl Pts',(4.38955443642782,-1.23566887208905,1.84388615537792));
#40270=CARTESIAN_POINT('Ctrl Pts',(4.51725253079926,-0.617655577060232,
1.865651426443));
#40271=CARTESIAN_POINT('Ctrl Pts',(4.51787557461174,0.000108094638884985,
1.88741669750807));
#40272=CARTESIAN_POINT('Ctrl Pts',(1.3130361863565,-4.90075024188322,0.));
#40273=CARTESIAN_POINT('Ctrl Pts',(1.45293783176837,-4.85499972547219,-2.12441198790355E-17));
#40274=CARTESIAN_POINT('Ctrl Pts',(1.59048961161953,-4.80314405262584,1.00940613638452E-17));
#40275=CARTESIAN_POINT('Ctrl Pts',(1.72536214292615,-4.74546564178603,1.90819582357449E-17));
#40276=CARTESIAN_POINT('Ctrl Pts',(1.86158804346972,-4.68720846085782,2.81600435471549E-17));
#40277=CARTESIAN_POINT('Ctrl Pts',(1.9950813260058,-4.62301070705921,2.02661125299078E-16));
#40278=CARTESIAN_POINT('Ctrl Pts',(2.12548189098024,-4.5531145507957,1.45716771982052E-16));
#40279=CARTESIAN_POINT('Ctrl Pts',(2.25528319940241,-4.4835396027235,8.90341067708004E-17));
#40280=CARTESIAN_POINT('Ctrl Pts',(2.38202075670042,-4.40831802172382,2.31151513749735E-16));
#40281=CARTESIAN_POINT('Ctrl Pts',(2.50530950004123,-4.32764726500609,1.45716771982052E-16));
#40282=CARTESIAN_POINT('Ctrl Pts',(2.62711997854446,-4.24794377212644,6.13064155008212E-17));
#40283=CARTESIAN_POINT('Ctrl Pts',(2.74556437761014,-4.16292050991704,2.71959880884896E-17));
#40284=CARTESIAN_POINT('Ctrl Pts',(2.86023373369319,-4.07273466802712,-6.93889390390723E-17));
#40285=CARTESIAN_POINT('Ctrl Pts',(2.90383704830196,-4.03844127202745,-1.06115603492979E-16));
#40286=CARTESIAN_POINT('Ctrl Pts',(2.94689409015111,-4.00340109988822,-3.37664978924697E-16));
#40287=CARTESIAN_POINT('Ctrl Pts',(2.98938067979849,-3.96762172921426,-3.7470027081099E-16));
#40288=CARTESIAN_POINT('Ctrl Pts',(3.0045493035191,-3.95484772651792,-3.87922664316067E-16));
#40289=CARTESIAN_POINT('Ctrl Pts',(3.0196457209465,-3.94197897848992,-6.77418652234536E-17));
#40290=CARTESIAN_POINT('Ctrl Pts',(3.03465663588118,-3.92902653262601,-5.55111512312578E-17));
#40291=CARTESIAN_POINT('Ctrl Pts',(3.14512636784121,-3.83370567916447,3.44982654016709E-17));
#40292=CARTESIAN_POINT('Ctrl Pts',(3.25112830521826,-3.73372148501147,-5.43481287766778E-16));
#40293=CARTESIAN_POINT('Ctrl Pts',(3.35231677944077,-3.62929621080565,-5.13478148889135E-16));
#40294=CARTESIAN_POINT('Ctrl Pts',(3.36921809466263,-3.61185425914028,-5.08466782607427E-16));
#40295=CARTESIAN_POINT('Ctrl Pts',(3.38598504383309,-3.59428832049142,-2.69772873285687E-16));
#40296=CARTESIAN_POINT('Ctrl Pts',(3.40261591802407,-3.57659932769537,-2.63677968348475E-16));
#40297=CARTESIAN_POINT('Ctrl Pts',(3.50230123740107,-3.4705716543402,-2.26333319460949E-16));
#40298=CARTESIAN_POINT('Ctrl Pts',(3.59710111637371,-3.36012540834712,3.61502860778476E-17));
#40299=CARTESIAN_POINT('Ctrl Pts',(3.68681562587056,-3.2456540248488,-6.93889390390723E-17));
#40300=CARTESIAN_POINT('Ctrl Pts',(3.77658274630639,-3.13111551233192,-1.74990055122844E-16));
#40301=CARTESIAN_POINT('Ctrl Pts',(3.86125888590103,-3.01254641429341,-2.14930374901985E-16));
#40302=CARTESIAN_POINT('Ctrl Pts',(3.94059800782458,-2.89031628889591,-9.71445146547012E-17));
#40303=CARTESIAN_POINT('Ctrl Pts',(4.01127293754548,-2.78143424794555,7.77859507059291E-18));
#40304=CARTESIAN_POINT('Ctrl Pts',(4.07771240145114,-2.66964644715424,3.21618427330635E-16));
#40305=CARTESIAN_POINT('Ctrl Pts',(4.13970845878657,-2.55520469810914,3.46944695195361E-16));
#40306=CARTESIAN_POINT('Ctrl Pts',(4.1548365715119,-2.52727892743195,3.53124743599032E-16));
#40307=CARTESIAN_POINT('Ctrl Pts',(4.16969994577116,-2.49919510449128,-5.38761705143296E-16));
#40308=CARTESIAN_POINT('Ctrl Pts',(4.18429524804614,-2.47095685207318,-5.41233724504764E-16));
#40309=CARTESIAN_POINT('Ctrl Pts',(4.1935591046312,-2.45303361104087,-5.42802752155488E-16));
#40310=CARTESIAN_POINT('Ctrl Pts',(4.20271084368267,-2.4350560800449,-1.54877819716967E-16));
#40311=CARTESIAN_POINT('Ctrl Pts',(4.21174771778014,-2.41702978670704,-1.66533453693773E-16));
#40312=CARTESIAN_POINT('Ctrl Pts',(4.27617843190164,-2.28850670005169,-2.49635288749205E-16));
#40313=CARTESIAN_POINT('Ctrl Pts',(4.33481139244535,-2.15743447779131,-2.0244448216388E-16));
#40314=CARTESIAN_POINT('Ctrl Pts',(4.38745860743762,-2.0241905870822,-2.77555756156289E-16));
#40315=CARTESIAN_POINT('Ctrl Pts',(4.43978289169495,-1.89176399596928,-3.52206307982929E-16));
#40316=CARTESIAN_POINT('Ctrl Pts',(4.48619490051256,-1.75719157307499,-5.94819252645897E-16));
#40317=CARTESIAN_POINT('Ctrl Pts',(4.52646203441684,-1.6208264292839,-5.55111512312578E-16));
#40318=CARTESIAN_POINT('Ctrl Pts',(4.54111387023209,-1.5712078072459,-5.40663220727154E-16));
#40319=CARTESIAN_POINT('Ctrl Pts',(4.55495165294679,-1.52135171714656,-2.34210881400015E-17));
#40320=CARTESIAN_POINT('Ctrl Pts',(4.56796247846719,-1.47127487515823,-2.77555756156289E-17));
#40321=CARTESIAN_POINT('Ctrl Pts',(4.60395075905375,-1.33276103239401,-1.11900177134892E-17));
#40322=CARTESIAN_POINT('Ctrl Pts',(4.63361579821919,-1.19255796729143,2.91143634808383E-16));
#40323=CARTESIAN_POINT('Ctrl Pts',(4.65692008513065,-1.05110298842804,2.77555756156289E-16));
#40324=CARTESIAN_POINT('Ctrl Pts',(4.67001847025983,-0.971596938805809,
2.69918566125548E-16));
#40325=CARTESIAN_POINT('Ctrl Pts',(4.68110649292123,-0.891695424459561,
-5.05694400348962E-17));
#40326=CARTESIAN_POINT('Ctrl Pts',(4.69017032387523,-0.811477248591749,
-5.55111512312578E-17));
#40327=CARTESIAN_POINT('Ctrl Pts',(4.69376322527145,-0.779678774244579,
-5.74700448985431E-17));
#40328=CARTESIAN_POINT('Ctrl Pts',(4.69703800287417,-0.74783055663592,9.2602246089847E-18));
#40329=CARTESIAN_POINT('Ctrl Pts',(4.69999357182281,-0.715937571621207,
0.));
#40330=CARTESIAN_POINT('Ctrl Pts',(4.7021844555123,-0.692296160477742,-6.86435519161465E-18));
#40331=CARTESIAN_POINT('Ctrl Pts',(4.70420012738525,-0.668626688781088,
-5.81512878434173E-17));
#40332=CARTESIAN_POINT('Ctrl Pts',(4.70603832259692,-0.644957088113592,
-5.55111512312578E-17));
#40333=CARTESIAN_POINT('Ctrl Pts',(4.7169850543804,-0.50400101974599,-3.97887365597508E-17));
#40334=CARTESIAN_POINT('Ctrl Pts',(4.72166050160268,-0.362862391559157,
3.85433575684503E-16));
#40335=CARTESIAN_POINT('Ctrl Pts',(4.72009704228143,-0.221963242879035,
3.88578058618805E-16));
#40336=CARTESIAN_POINT('Ctrl Pts',(4.71853510529174,-0.0812012869083159,
3.91719479787741E-16));
#40337=CARTESIAN_POINT('Ctrl Pts',(4.71074633224057,0.0593224521016401,
3.13145818824179E-16));
#40338=CARTESIAN_POINT('Ctrl Pts',(4.69671116060458,0.199185274316974,2.22044604925031E-16));
#40339=CARTESIAN_POINT('Ctrl Pts',(4.68289306772495,0.336884870581422,1.3235243244906E-16));
#40340=CARTESIAN_POINT('Ctrl Pts',(4.6630201315191,0.473944543714825,-1.38004669694731E-16));
#40341=CARTESIAN_POINT('Ctrl Pts',(4.63702542177262,0.609947964574148,-1.38777878078145E-16));
#40342=CARTESIAN_POINT('Ctrl Pts',(4.62055356019607,0.696128173708246,-1.39267830902609E-16));
#40343=CARTESIAN_POINT('Ctrl Pts',(4.60162268181677,0.781883974967431,8.79945197126988E-17));
#40344=CARTESIAN_POINT('Ctrl Pts',(4.58020591978812,0.867104757427645,1.11022302462516E-16));
#40345=CARTESIAN_POINT('Ctrl Pts',(4.56733705680351,0.918312058113609,6.78760316859931E-17));
#40346=CARTESIAN_POINT('Ctrl Pts',(4.55357049340461,0.96932610659445,-4.99175148350681E-16));
#40347=CARTESIAN_POINT('Ctrl Pts',(4.53891402393445,1.0201248132638,-5.55111512312578E-16));
#40348=CARTESIAN_POINT('Ctrl Pts',(4.5307224586103,1.04851643410481,-5.86374592437204E-16));
#40349=CARTESIAN_POINT('Ctrl Pts',(4.52225289509851,1.0768407763045,9.91752405205522E-17));
#40350=CARTESIAN_POINT('Ctrl Pts',(4.51350658698018,1.10509389044702,1.11022302462516E-16));
#40351=CARTESIAN_POINT('Ctrl Pts',(4.50742875670279,1.12472704654475,1.19254853933931E-16));
#40352=CARTESIAN_POINT('Ctrl Pts',(4.50121763562789,1.14432449467847,-5.35474147175706E-16));
#40353=CARTESIAN_POINT('Ctrl Pts',(4.49487767268156,1.16387312026907,-5.27355936696949E-16));
#40354=CARTESIAN_POINT('Ctrl Pts',(4.45189774593679,1.2963973168547,-4.72320900273343E-16));
#40355=CARTESIAN_POINT('Ctrl Pts',(4.40295499932666,1.42682794112182,5.0484926233065E-16));
#40356=CARTESIAN_POINT('Ctrl Pts',(4.34826585417728,1.55478882374,3.88578058618805E-16));
#40357=CARTESIAN_POINT('Ctrl Pts',(4.29692960608226,1.67490464560194,2.79435241634665E-16));
#40358=CARTESIAN_POINT('Ctrl Pts',(4.24052923074577,1.79284458992044,2.95867102710926E-16));
#40359=CARTESIAN_POINT('Ctrl Pts',(4.17920839057011,1.90827559700852,4.9960036108132E-16));
#40360=CARTESIAN_POINT('Ctrl Pts',(4.15338816346376,1.95687986938296,5.85385862147007E-16));
#40361=CARTESIAN_POINT('Ctrl Pts',(4.12669516016291,2.0050390084677,-2.10958088174218E-16));
#40362=CARTESIAN_POINT('Ctrl Pts',(4.09913850024111,2.05272668507128,-1.66533453693773E-16));
#40363=CARTESIAN_POINT('Ctrl Pts',(4.08221130669435,2.08201973197734,-1.3924479141655E-16));
#40364=CARTESIAN_POINT('Ctrl Pts',(4.06495515473503,2.11113968242291,3.92725569055683E-16));
#40365=CARTESIAN_POINT('Ctrl Pts',(4.04738928099658,2.14005245629164,3.33066907387547E-16));
#40366=CARTESIAN_POINT('Ctrl Pts',(3.97588097586157,2.2577524629574,9.02045342409376E-17));
#40367=CARTESIAN_POINT('Ctrl Pts',(3.89920169633387,2.37209762967783,1.73844745989399E-16));
#40368=CARTESIAN_POINT('Ctrl Pts',(3.81753428055142,2.4827050770719,1.11022302462516E-16));
#40369=CARTESIAN_POINT('Ctrl Pts',(3.73700167373633,2.59177557950503,4.90728077314622E-17));
#40370=CARTESIAN_POINT('Ctrl Pts',(3.65161810526706,2.69721206501942,-2.17511715066662E-16));
#40371=CARTESIAN_POINT('Ctrl Pts',(3.56152350731999,2.79861134980753,-2.22044604925031E-16));
#40372=CARTESIAN_POINT('Ctrl Pts',(3.54164701408898,2.82098186084422,-2.23044642181868E-16));
#40373=CARTESIAN_POINT('Ctrl Pts',(3.52154110171521,2.8431557130462,3.77586732270394E-16));
#40374=CARTESIAN_POINT('Ctrl Pts',(3.50120707213069,2.86512829543052,4.44089209850063E-16));
#40375=CARTESIAN_POINT('Ctrl Pts',(3.47910313325541,2.88901340959032,5.16017817963063E-16));
#40376=CARTESIAN_POINT('Ctrl Pts',(3.45672963690434,2.91266069254474,2.77193395410128E-16));
#40377=CARTESIAN_POINT('Ctrl Pts',(3.43409108914483,2.93606647242265,2.77555756156289E-16));
#40378=CARTESIAN_POINT('Origin',(0.,0.,20.5));
#40379=CARTESIAN_POINT('Origin',(0.,0.,41.));
#40380=CARTESIAN_POINT('',(-4.,4.89858719658941E-16,41.));
#40381=CARTESIAN_POINT('Origin',(0.,0.,41.));
#40382=CARTESIAN_POINT('Origin',(-4.45462538595717E-16,-1.65775395963113E-16,
375.));
#40383=CARTESIAN_POINT('Ctrl Pts',(-3.43378788736335,2.93584158412826,375.));
#40384=CARTESIAN_POINT('Ctrl Pts',(-3.52812472271588,2.83822707478694,375.));
#40385=CARTESIAN_POINT('Ctrl Pts',(-3.61783741229297,2.73641228828402,375.));
#40386=CARTESIAN_POINT('Ctrl Pts',(-3.70278930559469,2.6308098016192,375.));
#40387=CARTESIAN_POINT('Ctrl Pts',(-3.78883118430305,2.52385236964479,375.));
#40388=CARTESIAN_POINT('Ctrl Pts',(-3.86998980756465,2.41300886934011,375.));
#40389=CARTESIAN_POINT('Ctrl Pts',(-3.94608965952372,2.29866645157891,375.));
#40390=CARTESIAN_POINT('Ctrl Pts',(-3.98412572654406,2.24151606621978,375.));
#40391=CARTESIAN_POINT('Ctrl Pts',(-4.02089745503991,2.18349099620346,375.));
#40392=CARTESIAN_POINT('Ctrl Pts',(-4.0563792513302,2.12463643972661,375.));
#40393=CARTESIAN_POINT('Ctrl Pts',(-4.0706431485814,2.10097655116059,375.));
#40394=CARTESIAN_POINT('Ctrl Pts',(-4.08469915763129,2.07718134398868,375.));
#40395=CARTESIAN_POINT('Ctrl Pts',(-4.09853534340515,2.05327180953563,375.));
#40396=CARTESIAN_POINT('Ctrl Pts',(-4.16827482663706,1.93275893089092,375.));
#40397=CARTESIAN_POINT('Ctrl Pts',(-4.23249571495574,1.80924176863962,375.));
#40398=CARTESIAN_POINT('Ctrl Pts',(-4.29102780012401,1.68312480250504,375.));
#40399=CARTESIAN_POINT('Ctrl Pts',(-4.34427585815273,1.56839313846413,375.));
#40400=CARTESIAN_POINT('Ctrl Pts',(-4.3928156984662,1.45150902581472,375.));
#40401=CARTESIAN_POINT('Ctrl Pts',(-4.4364893782082,1.33275463175064,375.));
#40402=CARTESIAN_POINT('Ctrl Pts',(-4.46204208504677,1.2632735109649,375.));
#40403=CARTESIAN_POINT('Ctrl Pts',(-4.48592844490179,1.19315178813539,375.));
#40404=CARTESIAN_POINT('Ctrl Pts',(-4.50811171504532,1.12244350259313,375.));
#40405=CARTESIAN_POINT('Ctrl Pts',(-4.5141904988611,1.10306762252609,375.));
#40406=CARTESIAN_POINT('Ctrl Pts',(-4.52013855791141,1.08365664730297,375.));
#40407=CARTESIAN_POINT('Ctrl Pts',(-4.52595509671778,1.06421299497352,375.));
#40408=CARTESIAN_POINT('Ctrl Pts',(-4.53519138586709,1.0333377268782,375.));
#40409=CARTESIAN_POINT('Ctrl Pts',(-4.54409635013865,1.00237910104441,375.));
#40410=CARTESIAN_POINT('Ctrl Pts',(-4.55266817723945,0.971342071123453,
375.));
#40411=CARTESIAN_POINT('Ctrl Pts',(-4.58939773349738,0.838351015289689,
375.));
#40412=CARTESIAN_POINT('Ctrl Pts',(-4.62001434120323,0.703922655316075,
375.));
#40413=CARTESIAN_POINT('Ctrl Pts',(-4.6446125449424,0.568489655194437,375.));
#40414=CARTESIAN_POINT('Ctrl Pts',(-4.6695978975114,0.43092508774079,375.));
#40415=CARTESIAN_POINT('Ctrl Pts',(-4.68837408722962,0.292323323451818,
375.));
#40416=CARTESIAN_POINT('Ctrl Pts',(-4.7009917947161,0.153114389433896,375.));
#40417=CARTESIAN_POINT('Ctrl Pts',(-4.71369611133585,0.0129499121739395,
375.));
#40418=CARTESIAN_POINT('Ctrl Pts',(-4.72015723771216,-0.127830868720726,
375.));
#40419=CARTESIAN_POINT('Ctrl Pts',(-4.72037601386282,-0.2688014592115,375.));
#40420=CARTESIAN_POINT('Ctrl Pts',(-4.72051776383518,-0.360139464952745,
375.));
#40421=CARTESIAN_POINT('Ctrl Pts',(-4.71803791594725,-0.451557379168488,
375.));
#40422=CARTESIAN_POINT('Ctrl Pts',(-4.7129250253839,-0.542939603201634,
375.));
#40423=CARTESIAN_POINT('Ctrl Pts',(-4.71050429468246,-0.586205100974703,
375.));
#40424=CARTESIAN_POINT('Ctrl Pts',(-4.70749320436126,-0.629462591214061,
375.));
#40425=CARTESIAN_POINT('Ctrl Pts',(-4.70388981020381,-0.672699721412066,
375.));
#40426=CARTESIAN_POINT('Ctrl Pts',(-4.70250698353675,-0.689292260011098,
375.));
#40427=CARTESIAN_POINT('Ctrl Pts',(-4.7010370790231,-0.705879562100339,
375.));
#40428=CARTESIAN_POINT('Ctrl Pts',(-4.69948096449077,-0.722452069367425,
375.));
#40429=CARTESIAN_POINT('Ctrl Pts',(-4.68606574819498,-0.865323153038659,
375.));
#40430=CARTESIAN_POINT('Ctrl Pts',(-4.66623214709618,-1.0072815713457,375.));
#40431=CARTESIAN_POINT('Ctrl Pts',(-4.64004375541204,-1.14788248706686,
375.));
#40432=CARTESIAN_POINT('Ctrl Pts',(-4.6270279916287,-1.21776185685865,375.));
#40433=CARTESIAN_POINT('Ctrl Pts',(-4.61244171628795,-1.28730612660771,
375.));
#40434=CARTESIAN_POINT('Ctrl Pts',(-4.59628803251995,-1.35646150527604,
375.));
#40435=CARTESIAN_POINT('Ctrl Pts',(-4.56399682193468,-1.4947030932479,375.));
#40436=CARTESIAN_POINT('Ctrl Pts',(-4.52544561415923,-1.63139110841489,
375.));
#40437=CARTESIAN_POINT('Ctrl Pts',(-4.48088607305284,-1.76617553752727,
375.));
#40438=CARTESIAN_POINT('Ctrl Pts',(-4.43597574851398,-1.90202102210641,
375.));
#40439=CARTESIAN_POINT('Ctrl Pts',(-4.38496188398045,-2.03593355195248,
375.));
#40440=CARTESIAN_POINT('Ctrl Pts',(-4.32805045687434,-2.16754392308446,
375.));
#40441=CARTESIAN_POINT('Ctrl Pts',(-4.30216783694698,-2.22739870775111,
375.));
#40442=CARTESIAN_POINT('Ctrl Pts',(-4.27506473176287,-2.28677711825493,
375.));
#40443=CARTESIAN_POINT('Ctrl Pts',(-4.24675722722924,-2.34564306219817,
375.));
#40444=CARTESIAN_POINT('Ctrl Pts',(-4.22863084786129,-2.38333718074896,
375.));
#40445=CARTESIAN_POINT('Ctrl Pts',(-4.21001058428347,-2.42082115169986,
375.));
#40446=CARTESIAN_POINT('Ctrl Pts',(-4.190900240747,-2.45808525714998,375.));
#40447=CARTESIAN_POINT('Ctrl Pts',(-4.18310501328873,-2.47328551649951,
375.));
#40448=CARTESIAN_POINT('Ctrl Pts',(-4.17522954608524,-2.48844657780472,
375.));
#40449=CARTESIAN_POINT('Ctrl Pts',(-4.16727814768109,-2.50356042854303,
375.));
#40450=CARTESIAN_POINT('Ctrl Pts',(-4.09969026676857,-2.63203005010014,
375.));
#40451=CARTESIAN_POINT('Ctrl Pts',(-4.02654009074559,-2.75724655837471,
375.));
#40452=CARTESIAN_POINT('Ctrl Pts',(-3.94810710693448,-2.87885707775794,
375.));
#40453=CARTESIAN_POINT('Ctrl Pts',(-3.86905485941559,-3.00142776692534,
375.));
#40454=CARTESIAN_POINT('Ctrl Pts',(-3.78463578072622,-3.12033603731368,
375.));
#40455=CARTESIAN_POINT('Ctrl Pts',(-3.69508499761951,-3.23520722691392,
375.));
#40456=CARTESIAN_POINT('Ctrl Pts',(-3.62943480927899,-3.31941994924341,
375.));
#40457=CARTESIAN_POINT('Ctrl Pts',(-3.56102553573526,-3.40146273807253,
375.));
#40458=CARTESIAN_POINT('Ctrl Pts',(-3.48993392179959,-3.48117995730746,
375.));
#40459=CARTESIAN_POINT('Ctrl Pts',(-3.39320786765338,-3.58964186493951,
375.));
#40460=CARTESIAN_POINT('Ctrl Pts',(-3.29151757709749,-3.69380035593463,
375.));
#40461=CARTESIAN_POINT('Ctrl Pts',(-3.18521993250538,-3.79343311373674,
375.));
#40462=CARTESIAN_POINT('Ctrl Pts',(-3.1484894856507,-3.82786055311678,375.));
#40463=CARTESIAN_POINT('Ctrl Pts',(-3.1112085895158,-3.86174730075506,375.));
#40464=CARTESIAN_POINT('Ctrl Pts',(-3.07339099123149,-3.89508311993719,
375.));
#40465=CARTESIAN_POINT('Ctrl Pts',(-3.05466088259105,-3.91159351571128,
375.));
#40466=CARTESIAN_POINT('Ctrl Pts',(-3.03579911530405,-3.92796876126283,
375.));
#40467=CARTESIAN_POINT('Ctrl Pts',(-3.01680731961894,-3.94420755857869,
375.));
#40468=CARTESIAN_POINT('Ctrl Pts',(-3.00397674416022,-3.95517824917451,
375.));
#40469=CARTESIAN_POINT('Ctrl Pts',(-2.99108750647465,-3.96608603020355,
375.));
#40470=CARTESIAN_POINT('Ctrl Pts',(-2.97814807270005,-3.97692398964623,
375.));
#40471=CARTESIAN_POINT('Ctrl Pts',(-2.86441519405387,-4.07218567941864,
375.));
#40472=CARTESIAN_POINT('Ctrl Pts',(-2.74664729621727,-4.16219378118691,
375.));
#40473=CARTESIAN_POINT('Ctrl Pts',(-2.62528201158405,-4.24677543677276,
375.));
#40474=CARTESIAN_POINT('Ctrl Pts',(-2.50379141827822,-4.33144442223239,
375.));
#40475=CARTESIAN_POINT('Ctrl Pts',(-2.3786953776454,-4.41067622052404,375.));
#40476=CARTESIAN_POINT('Ctrl Pts',(-2.25039003171722,-4.4842647871821,375.));
#40477=CARTESIAN_POINT('Ctrl Pts',(-2.12228319217728,-4.5577395019934,375.));
#40478=CARTESIAN_POINT('Ctrl Pts',(-1.9909763337868,-4.62558889864692,375.));
#40479=CARTESIAN_POINT('Ctrl Pts',(-1.85683056691249,-4.68756837108862,
375.));
#40480=CARTESIAN_POINT('Ctrl Pts',(-1.72268480003817,-4.74954784353032,
375.));
#40481=CARTESIAN_POINT('Ctrl Pts',(-1.58569949586696,-4.80565788540407,
375.));
#40482=CARTESIAN_POINT('Ctrl Pts',(-1.44621200484621,-4.85560714827263,
375.));
#40483=CARTESIAN_POINT('Ctrl Pts',(-1.40211572701684,-4.87139764358304,
375.));
#40484=CARTESIAN_POINT('Ctrl Pts',(-1.35776924324391,-4.88657205481219,
375.));
#40485=CARTESIAN_POINT('Ctrl Pts',(-1.31318542874385,-4.90112866933901,
375.));
#40486=CARTESIAN_POINT('Ctrl Pts',(1.31303618635831,-4.90075024188273,375.));
#40487=CARTESIAN_POINT('Ctrl Pts',(1.45436548505342,-4.85453285551617,375.));
#40488=CARTESIAN_POINT('Ctrl Pts',(1.5934293761686,-4.80203848222433,375.));
#40489=CARTESIAN_POINT('Ctrl Pts',(1.72987023226972,-4.74352674861442,375.));
#40490=CARTESIAN_POINT('Ctrl Pts',(1.86675271207831,-4.68482562767973,375.));
#40491=CARTESIAN_POINT('Ctrl Pts',(2.00099581082903,-4.620067688427,375.));
#40492=CARTESIAN_POINT('Ctrl Pts',(2.13221219437754,-4.54946990611926,375.));
#40493=CARTESIAN_POINT('Ctrl Pts',(2.19270449791029,-4.5169234941499,375.));
#40494=CARTESIAN_POINT('Ctrl Pts',(2.25255310159603,-4.48313534130926,375.));
#40495=CARTESIAN_POINT('Ctrl Pts',(2.31171758991926,-4.44812388272337,375.));
#40496=CARTESIAN_POINT('Ctrl Pts',(2.3344624112488,-4.43466429923687,375.));
#40497=CARTESIAN_POINT('Ctrl Pts',(2.35710754237018,-4.42102302699321,375.));
#40498=CARTESIAN_POINT('Ctrl Pts',(2.37964612843956,-4.40720380568676,375.));
#40499=CARTESIAN_POINT('Ctrl Pts',(2.50549113115601,-4.33004368847728,375.));
#40500=CARTESIAN_POINT('Ctrl Pts',(2.62778788875034,-4.24748071485227,375.));
#40501=CARTESIAN_POINT('Ctrl Pts',(2.74616817727066,-4.15974114711123,375.));
#40502=CARTESIAN_POINT('Ctrl Pts',(2.86286389724632,-4.07325012604791,375.));
#40503=CARTESIAN_POINT('Ctrl Pts',(2.97575433427861,-3.98172826743118,375.));
#40504=CARTESIAN_POINT('Ctrl Pts',(3.08445220151971,-3.8853563473526,375.));
#40505=CARTESIAN_POINT('Ctrl Pts',(3.13995990370008,-3.83614301894012,375.));
#40506=CARTESIAN_POINT('Ctrl Pts',(3.19437368596074,-3.78566438686541,375.));
#40507=CARTESIAN_POINT('Ctrl Pts',(3.24763776430821,-3.73394147802337,375.));
#40508=CARTESIAN_POINT('Ctrl Pts',(3.2699643084639,-3.71226094127233,375.));
#40509=CARTESIAN_POINT('Ctrl Pts',(3.29209335275734,-3.69035703897681,375.));
#40510=CARTESIAN_POINT('Ctrl Pts',(3.31399620763943,-3.66825627851417,375.));
#40511=CARTESIAN_POINT('Ctrl Pts',(3.34216498231236,-3.63983298187436,375.));
#40512=CARTESIAN_POINT('Ctrl Pts',(3.36996576521876,-3.6110784436862,375.));
#40513=CARTESIAN_POINT('Ctrl Pts',(3.39739154337912,-3.58199736557932,375.));
#40514=CARTESIAN_POINT('Ctrl Pts',(3.49658091940006,-3.47682135290355,375.));
#40515=CARTESIAN_POINT('Ctrl Pts',(3.59086820857194,-3.3673769231021,375.));
#40516=CARTESIAN_POINT('Ctrl Pts',(3.6800850008747,-3.25406730243395,375.));
#40517=CARTESIAN_POINT('Ctrl Pts',(3.76996985501536,-3.13990921107455,375.));
#40518=CARTESIAN_POINT('Ctrl Pts',(3.85470838531078,-3.02182713075438,375.));
#40519=CARTESIAN_POINT('Ctrl Pts',(3.93408537345353,-2.90020291820586,375.));
#40520=CARTESIAN_POINT('Ctrl Pts',(4.01274556585136,-2.77967700530409,375.));
#40521=CARTESIAN_POINT('Ctrl Pts',(4.08614088023802,-2.65567191437214,375.));
#40522=CARTESIAN_POINT('Ctrl Pts',(4.15401504305787,-2.52854018053819,375.));
#40523=CARTESIAN_POINT('Ctrl Pts',(4.19807507197777,-2.44601352184147,375.));
#40524=CARTESIAN_POINT('Ctrl Pts',(4.23980760353704,-2.36216897889331,375.));
#40525=CARTESIAN_POINT('Ctrl Pts',(4.27913099033935,-2.27710078886137,375.));
#40526=CARTESIAN_POINT('Ctrl Pts',(4.29645860907187,-2.23961599207746,375.));
#40527=CARTESIAN_POINT('Ctrl Pts',(4.31331832747089,-2.20189359019125,375.));
#40528=CARTESIAN_POINT('Ctrl Pts',(4.32970256286081,-2.16394161183312,375.));
#40529=CARTESIAN_POINT('Ctrl Pts',(4.33919451441291,-2.14195472435813,375.));
#40530=CARTESIAN_POINT('Ctrl Pts',(4.34852813367479,-2.11988754210219,375.));
#40531=CARTESIAN_POINT('Ctrl Pts',(4.35769217797944,-2.0977656675703,375.));
#40532=CARTESIAN_POINT('Ctrl Pts',(4.41245445040556,-1.96557030933995,375.));
#40533=CARTESIAN_POINT('Ctrl Pts',(4.46123822222855,-1.83125898605536,375.));
#40534=CARTESIAN_POINT('Ctrl Pts',(4.50384926204605,-1.6951979775962,375.));
#40535=CARTESIAN_POINT('Ctrl Pts',(4.52559692351824,-1.62575567428212,375.));
#40536=CARTESIAN_POINT('Ctrl Pts',(4.54573592530189,-1.55585726815914,375.));
#40537=CARTESIAN_POINT('Ctrl Pts',(4.56423545664257,-1.48554983900212,375.));
#40538=CARTESIAN_POINT('Ctrl Pts',(4.60056463169787,-1.34748088717324,375.));
#40539=CARTESIAN_POINT('Ctrl Pts',(4.63057447100037,-1.20783464517222,375.));
#40540=CARTESIAN_POINT('Ctrl Pts',(4.65426082259252,-1.06704756524395,375.));
#40541=CARTESIAN_POINT('Ctrl Pts',(4.67788678995459,-0.926619397467839,
375.));
#40542=CARTESIAN_POINT('Ctrl Pts',(4.69522141344644,-0.785055397710089,
375.));
#40543=CARTESIAN_POINT('Ctrl Pts',(4.7062090782541,-0.642791899249072,375.));
#40544=CARTESIAN_POINT('Ctrl Pts',(4.71102657060836,-0.58041710641334,375.));
#40545=CARTESIAN_POINT('Ctrl Pts',(4.71462329627092,-0.5179079594038,375.));
#40546=CARTESIAN_POINT('Ctrl Pts',(4.71699147233722,-0.455302034234564,
375.));
#40547=CARTESIAN_POINT('Ctrl Pts',(4.71854674616479,-0.414186275042497,
375.));
#40548=CARTESIAN_POINT('Ctrl Pts',(4.71957210036622,-0.373028786701393,
375.));
#40549=CARTESIAN_POINT('Ctrl Pts',(4.72006488912048,-0.331840385723362,
375.));
#40550=CARTESIAN_POINT('Ctrl Pts',(4.72028902811531,-0.313106340528846,
375.));
#40551=CARTESIAN_POINT('Ctrl Pts',(4.72040288834379,-0.294371677101196,
375.));
#40552=CARTESIAN_POINT('Ctrl Pts',(4.72040648677608,-0.275644826658347,
375.));
#40553=CARTESIAN_POINT('Ctrl Pts',(4.72043355701338,-0.134766732053278,
375.));
#40554=CARTESIAN_POINT('Ctrl Pts',(4.71422662120245,0.0057990813089247,
375.));
#40555=CARTESIAN_POINT('Ctrl Pts',(4.70180390274057,0.145635587850549,375.));
#40556=CARTESIAN_POINT('Ctrl Pts',(4.68946458626375,0.284533278764535,375.));
#40557=CARTESIAN_POINT('Ctrl Pts',(4.67099254981089,0.422712188593173,375.));
#40558=CARTESIAN_POINT('Ctrl Pts',(4.6463550982981,0.559757549565289,375.));
#40559=CARTESIAN_POINT('Ctrl Pts',(4.62907635772754,0.655870219230258,375.));
#40560=CARTESIAN_POINT('Ctrl Pts',(4.60876410990094,0.751425238603689,375.));
#40561=CARTESIAN_POINT('Ctrl Pts',(4.58539251247819,0.846274706840598,375.));
#40562=CARTESIAN_POINT('Ctrl Pts',(4.55189132819966,0.982233300369681,375.));
#40563=CARTESIAN_POINT('Ctrl Pts',(4.51210568697928,1.11674373042915,375.));
#40564=CARTESIAN_POINT('Ctrl Pts',(4.46619637471526,1.24939846486887,375.));
#40565=CARTESIAN_POINT('Ctrl Pts',(4.4514821415469,1.29191517002461,375.));
#40566=CARTESIAN_POINT('Ctrl Pts',(4.43613853638538,1.33424101402745,375.));
#40567=CARTESIAN_POINT('Ctrl Pts',(4.42016997732094,1.37636185265469,375.));
#40568=CARTESIAN_POINT('Ctrl Pts',(4.41229563070378,1.39713229799154,375.));
#40569=CARTESIAN_POINT('Ctrl Pts',(4.40426931219602,1.41785288761014,375.));
#40570=CARTESIAN_POINT('Ctrl Pts',(4.39609151624634,1.43852188916379,375.));
#40571=CARTESIAN_POINT('Ctrl Pts',(4.38944561986513,1.45531908531226,375.));
#40572=CARTESIAN_POINT('Ctrl Pts',(4.38270019096179,1.4720807922257,375.));
#40573=CARTESIAN_POINT('Ctrl Pts',(4.37586028060643,1.48879486186589,375.));
#40574=CARTESIAN_POINT('Ctrl Pts',(4.32342038722716,1.61693748133431,375.));
#40575=CARTESIAN_POINT('Ctrl Pts',(4.26535943234438,1.74246391819237,375.));
#40576=CARTESIAN_POINT('Ctrl Pts',(4.20190818178381,1.86501937630542,375.));
#40577=CARTESIAN_POINT('Ctrl Pts',(4.13850743678452,1.98747728343019,375.));
#40578=CARTESIAN_POINT('Ctrl Pts',(4.06972452623307,2.10696961603591,375.));
#40579=CARTESIAN_POINT('Ctrl Pts',(3.99574428312086,2.22311713285455,375.));
#40580=CARTESIAN_POINT('Ctrl Pts',(3.9230204444275,2.3372921196134,375.));
#40581=CARTESIAN_POINT('Ctrl Pts',(3.84527380385539,2.44823547455532,375.));
#40582=CARTESIAN_POINT('Ctrl Pts',(3.7626432675861,2.55555363817714,375.));
#40583=CARTESIAN_POINT('Ctrl Pts',(3.68595020843944,2.65516037730487,375.));
#40584=CARTESIAN_POINT('Ctrl Pts',(3.60504931330013,2.75164424921775,375.));
#40585=CARTESIAN_POINT('Ctrl Pts',(3.52002795172102,2.84465807652531,375.));
#40586=CARTESIAN_POINT('Ctrl Pts',(3.49183173897392,2.87550488507407,375.));
#40587=CARTESIAN_POINT('Ctrl Pts',(3.46318217104164,2.90596975880766,375.));
#40588=CARTESIAN_POINT('Ctrl Pts',(3.43408816985932,2.93604417002309,375.));
#40589=CARTESIAN_POINT('Origin',(0.,0.,402.208336844637));
#40590=CARTESIAN_POINT('Ctrl Pts',(-5.07353386009457,0.000128968315485402,
399.708336844637));
#40591=CARTESIAN_POINT('Ctrl Pts',(-5.07374798994712,0.217328374468673,
399.701523610908));
#40592=CARTESIAN_POINT('Ctrl Pts',(-5.00706367321595,1.27523772951867,399.668334418693));
#40593=CARTESIAN_POINT('Ctrl Pts',(-4.28603436807985,3.09622957226831,399.608769267991));
#40594=CARTESIAN_POINT('Ctrl Pts',(-2.29040909926245,4.7655795591539,399.529641392531));
#40595=CARTESIAN_POINT('Ctrl Pts',(0.259800278618912,5.28102545063066,399.450513517072));
#40596=CARTESIAN_POINT('Ctrl Pts',(2.7471033957984,4.51775909222651,399.371385641611));
#40597=CARTESIAN_POINT('Ctrl Pts',(4.56924148852249,2.66059337678593,399.292257766152));
#40598=CARTESIAN_POINT('Ctrl Pts',(5.2850143906551,0.159209483399153,399.213129890692));
#40599=CARTESIAN_POINT('Ctrl Pts',(4.7211096918349,-2.38072426286758,399.134002015232));
#40600=CARTESIAN_POINT('Ctrl Pts',(3.01406746059458,-4.34420558161996,399.054874139772));
#40601=CARTESIAN_POINT('Ctrl Pts',(0.577219342712345,-5.25581036421826,
398.975746264313));
#40602=CARTESIAN_POINT('Ctrl Pts',(-1.99939275815206,-4.89480881878609,
398.896618388853));
#40603=CARTESIAN_POINT('Ctrl Pts',(-4.09188543486623,-3.34861140683646,
398.817490513394));
#40604=CARTESIAN_POINT('Ctrl Pts',(-4.96571105424643,-1.479143747598,398.754729998654));
#40605=CARTESIAN_POINT('Ctrl Pts',(-5.07346848196321,-0.319197162169717,
398.718345442402));
#40606=CARTESIAN_POINT('Ctrl Pts',(-5.07327504304777,-8.56681209025073E-5,
398.708336844637));
#40607=CARTESIAN_POINT('Ctrl Pts',(-5.07330191118131,0.000105688062508012,
399.791663155363));
#40608=CARTESIAN_POINT('Ctrl Pts',(-5.07350034043644,0.308800908665525,
399.781980894782));
#40609=CARTESIAN_POINT('Ctrl Pts',(-4.97021252404761,1.45829359598981,399.745922675715));
#40610=CARTESIAN_POINT('Ctrl Pts',(-4.11241943286933,3.32339561801255,399.683488498161));
#40611=CARTESIAN_POINT('Ctrl Pts',(-2.02945797892606,4.8824090247121,399.604360622701));
#40612=CARTESIAN_POINT('Ctrl Pts',(0.54487554882432,5.2592655238007,399.525232747241));
#40613=CARTESIAN_POINT('Ctrl Pts',(2.98728943775363,4.36266186092565,399.446104871781));
#40614=CARTESIAN_POINT('Ctrl Pts',(4.70637522433117,2.40972094089285,399.366976996322));
#40615=CARTESIAN_POINT('Ctrl Pts',(5.28589404837916,-0.126697339701679,
399.287849120862));
#40616=CARTESIAN_POINT('Ctrl Pts',(4.58552092441564,-2.6324361653814,399.208721245402));
#40617=CARTESIAN_POINT('Ctrl Pts',(2.77484145336967,-4.50077558224301,399.129593369943));
#40618=CARTESIAN_POINT('Ctrl Pts',(0.292280359106768,-5.27932726882375,
399.050465494482));
#40619=CARTESIAN_POINT('Ctrl Pts',(-2.26105137922953,-4.77957858969287,
398.971337619023));
#40620=CARTESIAN_POINT('Ctrl Pts',(-4.26690751412045,-3.12253502339944,
398.892209743563));
#40621=CARTESIAN_POINT('Ctrl Pts',(-5.00313619365009,-1.29606201606178,
398.832318255676));
#40622=CARTESIAN_POINT('Ctrl Pts',(-5.07372209014652,-0.227734309753026,
398.798802726276));
#40623=CARTESIAN_POINT('Ctrl Pts',(-5.07350261625086,-0.000127405426567848,
398.791663155363));
#40624=CARTESIAN_POINT('Ctrl Pts',(3.43378788736214,2.93584158412968,400.));
#40625=CARTESIAN_POINT('Ctrl Pts',(3.92033033613488,2.36677696691239,399.973624041513));
#40626=CARTESIAN_POINT('Ctrl Pts',(4.60446627899797,0.982571495138102,399.92087212454));
#40627=CARTESIAN_POINT('Ctrl Pts',(4.51560363134058,-1.33271150407048,399.84174424908));
#40628=CARTESIAN_POINT('Ctrl Pts',(3.3333277577492,-3.32493526877752,399.762616373621));
#40629=CARTESIAN_POINT('Ctrl Pts',(1.34394627169084,-4.51226606526834,399.683488498161));
#40630=CARTESIAN_POINT('Ctrl Pts',(-0.97085300939813,-4.60694214684371,
399.604360622701));
#40631=CARTESIAN_POINT('Ctrl Pts',(-3.05057500858779,-3.58616495104857,
399.525232747241));
#40632=CARTESIAN_POINT('Ctrl Pts',(-4.391652180308,-1.69703895278099,399.446104871782));
#40633=CARTESIAN_POINT('Ctrl Pts',(-4.66936408063869,0.602987533589634,
399.366976996322));
#40634=CARTESIAN_POINT('Ctrl Pts',(-3.81646794512629,2.7570149696695,399.287849120862));
#40635=CARTESIAN_POINT('Ctrl Pts',(-2.03947802510898,4.24347545201977,399.208721245402));
#40636=CARTESIAN_POINT('Ctrl Pts',(0.231337257318392,4.70245047492642,399.129593369942));
#40637=CARTESIAN_POINT('Ctrl Pts',(2.44613812014511,4.02280553037415,399.050465494483));
#40638=CARTESIAN_POINT('Ctrl Pts',(4.06864765349505,2.36910590664905,398.971337619023));
#40639=CARTESIAN_POINT('Ctrl Pts',(4.70600239738688,0.141766919667795,398.892209743563));
#40640=CARTESIAN_POINT('Ctrl Pts',(4.20387758402063,-2.11989850176798,398.813081868103));
#40641=CARTESIAN_POINT('Ctrl Pts',(2.68385431845262,-3.86826607662479,398.733953992643));
#40642=CARTESIAN_POINT('Ctrl Pts',(0.513980740606018,-4.67999788571173,
398.654826117184));
#40643=CARTESIAN_POINT('Ctrl Pts',(-1.78034465333125,-4.35854670077871,
398.575698241724));
#40644=CARTESIAN_POINT('Ctrl Pts',(-3.64358944799884,-2.98174652775848,
398.496570366264));
#40645=CARTESIAN_POINT('Ctrl Pts',(-4.62460016500653,-0.88296644150622,
398.417442490804));
#40646=CARTESIAN_POINT('Ctrl Pts',(-4.48584151198124,1.42960916071621,398.338314615345));
#40647=CARTESIAN_POINT('Ctrl Pts',(-3.2609115695794,3.39602888062287,398.259186739885));
#40648=CARTESIAN_POINT('Ctrl Pts',(-1.24640657987359,4.54015716254393,398.180058864425));
#40649=CARTESIAN_POINT('Ctrl Pts',(1.06989485946835,4.5849625311949,398.100930988966));
#40650=CARTESIAN_POINT('Ctrl Pts',(3.12713920196537,3.51959611807719,398.021803113505));
#40651=CARTESIAN_POINT('Ctrl Pts',(4.42719923245446,1.6020185326593,397.942675238046));
#40652=CARTESIAN_POINT('Ctrl Pts',(4.65528721806493,-0.70346097272927,397.863547362586));
#40653=CARTESIAN_POINT('Ctrl Pts',(3.75617547838133,-2.83860920142977,397.784419487126));
#40654=CARTESIAN_POINT('Ctrl Pts',(1.94756884202228,-4.28643581876784,397.705291611666));
#40655=CARTESIAN_POINT('Ctrl Pts',(-0.332608926446521,-4.69637389108681,
397.626163736207));
#40656=CARTESIAN_POINT('Ctrl Pts',(-2.53225102161336,-3.96916378931016,
397.547035860747));
#40657=CARTESIAN_POINT('Ctrl Pts',(-4.11875100068,-2.28088724342758,397.467907985287));
#40658=CARTESIAN_POINT('Ctrl Pts',(-4.70796450115822,-0.0403321046706491,
397.388780109827));
#40659=CARTESIAN_POINT('Ctrl Pts',(-4.15722335570028,2.20998877681613,397.309652234368));
#40660=CARTESIAN_POINT('Ctrl Pts',(-2.59988029611171,3.92519794006916,397.230524358908));
#40661=CARTESIAN_POINT('Ctrl Pts',(-0.413019825824474,4.6899862522516,397.151396483448));
#40662=CARTESIAN_POINT('Ctrl Pts',(1.87384646846516,4.31917304995456,397.072268607988));
#40663=CARTESIAN_POINT('Ctrl Pts',(3.70699226699225,2.90254453114723,396.993140732528));
#40664=CARTESIAN_POINT('Ctrl Pts',(4.6425520586224,0.783113533157272,396.914012857069));
#40665=CARTESIAN_POINT('Ctrl Pts',(4.45399573023398,-1.52593527316547,396.834884981609));
#40666=CARTESIAN_POINT('Ctrl Pts',(3.18697903443818,-3.46550444479366,396.755757106149));
#40667=CARTESIAN_POINT('Ctrl Pts',(1.14828881478399,-4.56595983563972,396.676629230689));
#40668=CARTESIAN_POINT('Ctrl Pts',(-1.16844028323631,-4.56084462872216,
396.597501355229));
#40669=CARTESIAN_POINT('Ctrl Pts',(-3.20225116276825,-3.45139738560812,
396.51837347977));
#40670=CARTESIAN_POINT('Ctrl Pts',(-4.46069062869795,-1.50625214950199,
396.43924560431));
#40671=CARTESIAN_POINT('Ctrl Pts',(-4.63904866983842,0.803606783012363,
396.36011772885));
#40672=CARTESIAN_POINT('Ctrl Pts',(-3.69413887779848,2.91888581043708,396.28098985339));
#40673=CARTESIAN_POINT('Ctrl Pts',(-1.85475531148862,4.32740559196129,396.201861977931));
#40674=CARTESIAN_POINT('Ctrl Pts',(0.433726147102728,4.68811668499756,396.122734102471));
#40675=CARTESIAN_POINT('Ctrl Pts',(2.61718809326315,3.9136789479101,396.043606227011));
#40676=CARTESIAN_POINT('Ctrl Pts',(4.16694183591648,2.19160949051653,395.964478351551));
#40677=CARTESIAN_POINT('Ctrl Pts',(4.70774049744502,-0.0611214491752849,
395.885350476092));
#40678=CARTESIAN_POINT('Ctrl Pts',(4.10863875177974,-2.29905285502682,395.806222600631));
#40679=CARTESIAN_POINT('Ctrl Pts',(2.5146990390031,-3.98030716981366,395.727094725172));
#40680=CARTESIAN_POINT('Ctrl Pts',(0.311867128348267,-4.69779685779291,
395.647966849712));
#40681=CARTESIAN_POINT('Ctrl Pts',(-1.96647817706303,-4.27779382415375,
395.568838974252));
#40682=CARTESIAN_POINT('Ctrl Pts',(-3.7686737720159,-2.82199475955442,395.489711098792));
#40683=CARTESIAN_POINT('Ctrl Pts',(-4.65834821810063,-0.682896992050643,
395.410583223333));
#40684=CARTESIAN_POINT('Ctrl Pts',(-4.42008176906904,1.62155282910444,395.331455347873));
#40685=CARTESIAN_POINT('Ctrl Pts',(-3.11156664954973,3.53337082801154,395.252327472413));
#40686=CARTESIAN_POINT('Ctrl Pts',(-1.0496378504197,4.58964233963818,395.173199596953));
#40687=CARTESIAN_POINT('Ctrl Pts',(1.2664431505466,4.53460893234099,395.094071721494));
#40688=CARTESIAN_POINT('Ctrl Pts',(3.27587618232697,3.381596022723,395.014943846034));
#40689=CARTESIAN_POINT('Ctrl Pts',(4.49211073679585,1.40978634948583,394.935815970574));
#40690=CARTESIAN_POINT('Ctrl Pts',(4.6206560142512,-0.903379444528889,394.856688095114));
#40691=CARTESIAN_POINT('Ctrl Pts',(3.63038693161045,-2.99780705677087,394.777560219655));
#40692=CARTESIAN_POINT('Ctrl Pts',(1.7610805392752,-4.36636596691336,394.698432344195));
#40693=CARTESIAN_POINT('Ctrl Pts',(-0.534641970284508,-4.6776825871839,
394.619304468735));
#40694=CARTESIAN_POINT('Ctrl Pts',(-2.7009098933051,-3.85637681912437,394.540176593275));
#40695=CARTESIAN_POINT('Ctrl Pts',(-4.21319778305003,-2.1013140802211,394.461048717815));
#40696=CARTESIAN_POINT('Ctrl Pts',(-4.7053304898376,0.162546621736014,394.381920842356));
#40697=CARTESIAN_POINT('Ctrl Pts',(-4.05814633235487,2.38704938533492,394.302792966896));
#40698=CARTESIAN_POINT('Ctrl Pts',(-2.42835010030815,4.03356817385879,394.223665091436));
#40699=CARTESIAN_POINT('Ctrl Pts',(-0.210569617716467,4.70342607669429,
394.144537215976));
#40700=CARTESIAN_POINT('Ctrl Pts',(2.05819676630879,4.23442823696295,394.065409340517));
#40701=CARTESIAN_POINT('Ctrl Pts',(3.82860532171676,2.74013461591856,393.986281465057));
#40702=CARTESIAN_POINT('Ctrl Pts',(4.67198130861809,0.582363352861709,393.907153589597));
#40703=CARTESIAN_POINT('Ctrl Pts',(4.38411537617703,-1.71641742918247,393.828025714137));
#40704=CARTESIAN_POINT('Ctrl Pts',(3.03470943208895,-3.59959651705903,393.748897838677));
#40705=CARTESIAN_POINT('Ctrl Pts',(0.950499494613711,-4.61119367773381,
393.669769963218));
#40706=CARTESIAN_POINT('Ctrl Pts',(-1.36385795450447,-4.50626762440581,
393.590642087758));
#40707=CARTESIAN_POINT('Ctrl Pts',(-3.34798007341745,-3.31022444115695,
393.511514212298));
#40708=CARTESIAN_POINT('Ctrl Pts',(-4.52144496705717,-1.31266592578101,
393.432386336838));
#40709=CARTESIAN_POINT('Ctrl Pts',(-4.60011779179461,1.00273262859438,393.353258461379));
#40710=CARTESIAN_POINT('Ctrl Pts',(-3.56494924255402,3.07533629394358,393.274130585919));
#40711=CARTESIAN_POINT('Ctrl Pts',(-1.6665880225581,4.40329885266706,393.195002710459));
#40712=CARTESIAN_POINT('Ctrl Pts',(0.635309536488234,4.6650764426406,393.115874834999));
#40713=CARTESIAN_POINT('Ctrl Pts',(2.78337754615093,3.79728401076558,393.03674695954));
#40714=CARTESIAN_POINT('Ctrl Pts',(4.25749736347943,2.01004294053605,392.957619084079));
#40715=CARTESIAN_POINT('Ctrl Pts',(4.70073559740488,-0.263896316995348,
392.87849120862));
#40716=CARTESIAN_POINT('Ctrl Pts',(4.00576954320095,-2.47393750721331,392.79936333316));
#40717=CARTESIAN_POINT('Ctrl Pts',(2.3408735755072,-4.08495622085785,392.7202354577));
#40718=CARTESIAN_POINT('Ctrl Pts',(0.109174330666369,-4.70687129507029,
392.64110758224));
#40719=CARTESIAN_POINT('Ctrl Pts',(-2.14895964736531,-4.18909642486643,
392.561979706781));
#40720=CARTESIAN_POINT('Ctrl Pts',(-3.88675908733054,-2.65700211138166,
392.482851831321));
#40721=CARTESIAN_POINT('Ctrl Pts',(-4.68344499975174,-0.481559297629621,
392.403723955861));
#40722=CARTESIAN_POINT('Ctrl Pts',(-4.34611325228191,1.81048502373608,392.324596080401));
#40723=CARTESIAN_POINT('Ctrl Pts',(-2.95644307012664,3.66415076053556,392.245468204942));
#40724=CARTESIAN_POINT('Ctrl Pts',(-0.850919781515802,4.63060384272486,
392.166340329482));
#40725=CARTESIAN_POINT('Ctrl Pts',(1.46063946127848,4.47583386498977,392.087212454022));
#40726=CARTESIAN_POINT('Ctrl Pts',(3.41852935514023,3.23731578176699,392.008084578562));
#40727=CARTESIAN_POINT('Ctrl Pts',(4.54867969835275,1.21493597552573,391.928956703102));
#40728=CARTESIAN_POINT('Ctrl Pts',(4.57744353923776,-1.10162020130516,391.849828827643));
#40729=CARTESIAN_POINT('Ctrl Pts',(3.4978561961279,-3.1514375218371,391.770700952183));
#40730=CARTESIAN_POINT('Ctrl Pts',(1.57132163822667,-4.43818709971468,391.691573076723));
#40731=CARTESIAN_POINT('Ctrl Pts',(-0.735682101486766,-4.65030410493606,
391.612445201263));
#40732=CARTESIAN_POINT('Ctrl Pts',(-2.86455275856638,-3.73642796213481,
391.533317325804));
#40733=CARTESIAN_POINT('Ctrl Pts',(-4.29982000702773,-1.91783845252855,
391.454189450344));
#40734=CARTESIAN_POINT('Ctrl Pts',(-4.6939579537506,0.36512347398464,391.375061574884));
#40735=CARTESIAN_POINT('Ctrl Pts',(-3.95153270508603,2.55967687481616,391.295933699424));
#40736=CARTESIAN_POINT('Ctrl Pts',(-2.25231008366655,4.13444744915776,391.216805823965));
#40737=CARTESIAN_POINT('Ctrl Pts',(-0.00772834933684394,4.70813091315965,
391.137677948505));
#40738=CARTESIAN_POINT('Ctrl Pts',(2.2387246751714,4.14181943735019,391.058550073045));
#40739=CARTESIAN_POINT('Ctrl Pts',(3.94310806559349,2.572635847897,390.979422197585));
#40740=CARTESIAN_POINT('Ctrl Pts',(4.69273396842282,0.380531633959359,390.900294322126));
#40741=CARTESIAN_POINT('Ctrl Pts',(4.30609304338418,-1.90371193318514,390.821166446665));
#40742=CARTESIAN_POINT('Ctrl Pts',(2.87680390605944,-3.72700358316359,390.742038571206));
#40743=CARTESIAN_POINT('Ctrl Pts',(0.750944950216976,-4.64786382164717,
390.662910695746));
#40744=CARTESIAN_POINT('Ctrl Pts',(-1.55674273110369,-4.4433217857802,390.583782820286));
#40745=CARTESIAN_POINT('Ctrl Pts',(-3.48749126846685,-3.16290389914089,
390.504654944827));
#40746=CARTESIAN_POINT('Ctrl Pts',(-4.57380228443991,-1.11664187888751,
390.425527069367));
#40747=CARTESIAN_POINT('Ctrl Pts',(-4.55264378519931,1.19999624496042,390.346399193907));
#40748=CARTESIAN_POINT('Ctrl Pts',(-3.42913894648368,3.22607540341852,390.267271318447));
#40749=CARTESIAN_POINT('Ctrl Pts',(-1.4753256225101,4.47101450796107,390.188143442987));
#40750=CARTESIAN_POINT('Ctrl Pts',(0.835713058034306,4.63337243349421,390.109015567528));
#40751=CARTESIAN_POINT('Ctrl Pts',(2.94439783745191,3.67383693128064,390.029887692068));
#40752=CARTESIAN_POINT('Ctrl Pts',(4.34014606149365,1.8247434306593,389.950759816608));
#40753=CARTESIAN_POINT('Ctrl Pts',(4.68500070602262,-0.466181088634749,
389.871631941148));
#40754=CARTESIAN_POINT('Ctrl Pts',(3.89546100247805,-2.64422767571286,389.792504065689));
#40755=CARTESIAN_POINT('Ctrl Pts',(2.16270074857769,-4.18201887787879,389.713376190229));
#40756=CARTESIAN_POINT('Ctrl Pts',(-0.0937212205934936,-4.70720434606822,
389.634248314769));
#40757=CARTESIAN_POINT('Ctrl Pts',(-2.32745016801145,-4.09261922712786,
389.555120439309));
#40758=CARTESIAN_POINT('Ctrl Pts',(-3.99762609128131,-2.48707500030459,
389.475992563849));
#40759=CARTESIAN_POINT('Ctrl Pts',(-4.69984390136856,-0.279327273286843,
389.39686468839));
#40760=CARTESIAN_POINT('Ctrl Pts',(-4.26407333256687,1.99605486831531,389.31773681293));
#40761=CARTESIAN_POINT('Ctrl Pts',(-2.79582891973421,3.78812579970769,389.23860893747));
#40762=CARTESIAN_POINT('Ctrl Pts',(-0.650621423278113,4.6629655999594,389.159481062011));
#40763=CARTESIAN_POINT('Ctrl Pts',(1.65212313914968,4.40874648351652,389.08035318655));
#40764=CARTESIAN_POINT('Ctrl Pts',(3.55483379145156,3.08702334587661,389.001225311091));
#40765=CARTESIAN_POINT('Ctrl Pts',(4.59680105983476,1.01782927799078,388.922097435631));
#40766=CARTESIAN_POINT('Ctrl Pts',(4.52573004525854,-1.29781507938429,388.842969560171));
#40767=CARTESIAN_POINT('Ctrl Pts',(3.35882940195932,-3.29921528114894,388.763841684711));
#40768=CARTESIAN_POINT('Ctrl Pts',(1.37864455043625,-4.50176583424611,388.684713809252));
#40769=CARTESIAN_POINT('Ctrl Pts',(-0.935355957508586,-4.61428929040934,
388.605585933792));
#40770=CARTESIAN_POINT('Ctrl Pts',(-3.02287570734582,-3.60953998187742,
388.526458058332));
#40771=CARTESIAN_POINT('Ctrl Pts',(-4.37845680177713,-1.73080110290138,
388.447330182872));
#40772=CARTESIAN_POINT('Ctrl Pts',(-4.67386801345155,0.567022235602428,
388.368202307413));
#40773=CARTESIAN_POINT('Ctrl Pts',(-3.83758047185038,2.72755064937495,388.289074431953));
#40774=CARTESIAN_POINT('Ctrl Pts',(-2.07208717966135,4.22764841758585,388.209946556493));
#40775=CARTESIAN_POINT('Ctrl Pts',(0.19512727177995,4.70409202404044,388.130818681033));
#40776=CARTESIAN_POINT('Ctrl Pts',(2.41509492687017,4.04151863994701,388.051690805573));
#40777=CARTESIAN_POINT('Ctrl Pts',(4.0502878493588,2.40035929814049,387.972562930114));
#40778=CARTESIAN_POINT('Ctrl Pts',(4.7047714971451,0.17799320909573,387.893435054654));
#40779=CARTESIAN_POINT('Ctrl Pts',(4.22007363136663,-2.08747095037925,387.814307179194));
#40780=CARTESIAN_POINT('Ctrl Pts',(2.71355571127686,-3.84748902852625,387.735179303735));
#40781=CARTESIAN_POINT('Ctrl Pts',(0.549995785174607,-4.67590216526428,
387.656051428274));
#40782=CARTESIAN_POINT('Ctrl Pts',(-1.74673639624114,-4.37212401298038,
387.576923552815));
#40783=CARTESIAN_POINT('Ctrl Pts',(-3.62052565410023,-3.00970935653847,
387.497795677355));
#40784=CARTESIAN_POINT('Ctrl Pts',(-4.61766534522889,-0.918544055723703,
387.418667801895));
#40785=CARTESIAN_POINT('Ctrl Pts',(-4.49671481660818,1.39503128313651,387.339539926435));
#40786=CARTESIAN_POINT('Ctrl Pts',(-3.28696021026318,3.37082319307611,387.260412050976));
#40787=CARTESIAN_POINT('Ctrl Pts',(-1.28132331513389,4.53042679942271,387.181284175516));
#40788=CARTESIAN_POINT('Ctrl Pts',(1.03456453147854,4.59306353679543,387.102156300057));
#40789=CARTESIAN_POINT('Ctrl Pts',(3.09994992763925,3.54356696973015,387.023028424596));
#40790=CARTESIAN_POINT('Ctrl Pts',(4.414734438574,1.63605509066836,386.943900549137));
#40791=CARTESIAN_POINT('Ctrl Pts',(4.66056504541948,-0.667600090059401,
386.864772673676));
#40792=CARTESIAN_POINT('Ctrl Pts',(3.77791798959212,-2.80960710540626,386.785644798217));
#40793=CARTESIAN_POINT('Ctrl Pts',(1.9805114526468,-4.27131488054533,386.706516922757));
#40794=CARTESIAN_POINT('Ctrl Pts',(-0.29644271708526,-4.69879539225962,
386.627389047298));
#40795=CARTESIAN_POINT('Ctrl Pts',(-2.50161825456297,-3.98854140398097,
386.548261171838));
#40796=CARTESIAN_POINT('Ctrl Pts',(-4.10106888673475,-2.31252900718875,
386.469133296378));
#40797=CARTESIAN_POINT('Ctrl Pts',(-4.70751446766038,-0.0765764950965269,
386.390005420918));
#40798=CARTESIAN_POINT('Ctrl Pts',(-4.1741143707138,2.17791773100677,386.310877545459));
#40799=CARTESIAN_POINT('Ctrl Pts',(-2.63002248363295,3.90506570475047,386.231749669998));
#40800=CARTESIAN_POINT('Ctrl Pts',(-0.449114760664552,4.68666751056509,
386.152621794539));
#40801=CARTESIAN_POINT('Ctrl Pts',(1.84053856942387,4.33347137954045,386.073493919079));
#40802=CARTESIAN_POINT('Ctrl Pts',(3.68453635289055,2.93099783129588,385.994366043619));
#40803=CARTESIAN_POINT('Ctrl Pts',(4.63638545244831,0.818832314432457,385.915238168159));
#40804=CARTESIAN_POINT('Ctrl Pts',(4.46561157225142,-1.49159971460418,385.8361102927));
#40805=CARTESIAN_POINT('Ctrl Pts',(3.21356474331376,-3.44086588860477,385.75698241724));
#40806=CARTESIAN_POINT('Ctrl Pts',(1.18340710698663,-4.55698409498724,385.67785454178));
#40807=CARTESIAN_POINT('Ctrl Pts',(-1.13329271318905,-4.56970502867152,
385.59872666632));
#40808=CARTESIAN_POINT('Ctrl Pts',(-3.17558470949784,-3.47594852891073,
385.519598790861));
#40809=CARTESIAN_POINT('Ctrl Pts',(-4.44896212663648,-1.54054938855827,
385.440470915401));
#40810=CARTESIAN_POINT('Ctrl Pts',(-4.64509797905953,0.767867949435454,
385.361343039941));
#40811=CARTESIAN_POINT('Ctrl Pts',(-3.71650125952819,2.89035894150857,385.282215164481));
#40812=CARTESIAN_POINT('Ctrl Pts',(-1.88801609003413,4.31299799056357,385.203087289022));
#40813=CARTESIAN_POINT('Ctrl Pts',(0.397620511444409,4.69131691017691,385.123959413562));
#40814=CARTESIAN_POINT('Ctrl Pts',(2.58697997463334,3.93371211881083,385.044831538102));
#40815=CARTESIAN_POINT('Ctrl Pts',(4.14994562361626,2.22362491078451,384.965703662642));
#40816=CARTESIAN_POINT('Ctrl Pts',(4.70807153923669,-0.0248757766222604,
384.886575787182));
#40817=CARTESIAN_POINT('Ctrl Pts',(4.12621689144541,-2.26735321191552,384.807447911723));
#40818=CARTESIAN_POINT('Ctrl Pts',(2.54526802482854,-3.96082909308373,384.728320036263));
#40819=CARTESIAN_POINT('Ctrl Pts',(0.348025193093154,-4.69525663705463,
384.649192160803));
#40820=CARTESIAN_POINT('Ctrl Pts',(-1.93348610236405,-4.29280653125647,
384.570064285343));
#40821=CARTESIAN_POINT('Ctrl Pts',(-3.74683616493588,-2.85092531925369,
384.490936409884));
#40822=CARTESIAN_POINT('Ctrl Pts',(-4.65295268895202,-0.718740354514286,
384.411808534423));
#40823=CARTESIAN_POINT('Ctrl Pts',(-4.43243475474589,1.58747553296225,384.332680658964));
#40824=CARTESIAN_POINT('Ctrl Pts',(-3.1386770817443,3.50931084393592,384.253552783504));
#40825=CARTESIAN_POINT('Ctrl Pts',(-1.08494139264941,4.58142538925924,384.174424908044));
#40826=CARTESIAN_POINT('Ctrl Pts',(1.23149465895138,4.54422461238519,384.095297032584));
#40827=CARTESIAN_POINT('Ctrl Pts',(3.24974493247929,3.40671605753374,384.016169157125));
#40828=CARTESIAN_POINT('Ctrl Pts',(4.48112397259501,1.44432834392579,383.937041281665));
#40829=CARTESIAN_POINT('Ctrl Pts',(4.62747399638768,-0.867779255104094,
383.857913406205));
#40830=CARTESIAN_POINT('Ctrl Pts',(3.65335880005533,-2.96976866117404,383.778785530746));
#40831=CARTESIAN_POINT('Ctrl Pts',(1.79464404134943,-4.35267839240186,383.699657655285));
#40832=CARTESIAN_POINT('Ctrl Pts',(-0.498613673709388,-4.68166005036923,
383.620529779826));
#40833=CARTESIAN_POINT('Ctrl Pts',(-2.6711404500085,-3.87705624400286,383.541401904366));
#40834=CARTESIAN_POINT('Ctrl Pts',(-4.19689536445816,-2.13368829087633,
383.462274028906));
#40835=CARTESIAN_POINT('Ctrl Pts',(-4.70644245320202,0.126316497461169,
383.383146153446));
#40836=CARTESIAN_POINT('Ctrl Pts',(-4.07640343439582,2.35573586441245,383.304018277987));
#40837=CARTESIAN_POINT('Ctrl Pts',(-2.45933168995915,4.01475330021607,383.224890402527));
#40838=CARTESIAN_POINT('Ctrl Pts',(-0.246774022640667,4.70166555643666,
383.145762527067));
#40839=CARTESIAN_POINT('Ctrl Pts',(2.02553583557396,4.25014835054481,383.066634651607));
#40840=CARTESIAN_POINT('Ctrl Pts',(3.80739616178709,2.76952900148059,382.987506776148));
#40841=CARTESIAN_POINT('Ctrl Pts',(4.66735936186835,0.618314652917929,382.908378900688));
#40842=CARTESIAN_POINT('Ctrl Pts',(4.39719976949725,-1.68261421899571,382.829251025228));
#40843=CARTESIAN_POINT('Ctrl Pts',(3.06233199907708,-3.57612627716942,382.750123149768));
#40844=CARTESIAN_POINT('Ctrl Pts',(0.985971893936046,-4.60373933310752,
382.670995274309));
#40845=CARTESIAN_POINT('Ctrl Pts',(-1.32912476943063,-4.51663411957612,
382.591867398849));
#40846=CARTESIAN_POINT('Ctrl Pts',(-3.32239616084197,-3.33590170317647,
382.512739523389));
#40847=CARTESIAN_POINT('Ctrl Pts',(-4.51120504233833,-1.34743663628917,
382.433611647929));
#40848=CARTESIAN_POINT('Ctrl Pts',(-4.6077012809677,0.967287614002028,382.354483772469));
#40849=CARTESIAN_POINT('Ctrl Pts',(-3.58851993089967,3.04779939109664,382.27535589701));
#40850=CARTESIAN_POINT('Ctrl Pts',(-1.70043866320114,4.39033766076413,382.19622802155));
#40851=CARTESIAN_POINT('Ctrl Pts',(0.599375308465022,4.66982929692676,382.11710014609));
#40852=CARTESIAN_POINT('Ctrl Pts',(2.75406060140474,3.81860008728635,382.03797227063));
#40853=CARTESIAN_POINT('Ctrl Pts',(4.24189630850143,2.0427609088572,381.95884439517));
#40854=CARTESIAN_POINT('Ctrl Pts',(4.70262796601022,-0.227698564184567,
381.879716519711));
#40855=CARTESIAN_POINT('Ctrl Pts',(4.02469713006905,-2.44302464867774,381.800588644251));
#40856=CARTESIAN_POINT('Ctrl Pts',(2.37225338291554,-4.06681328684744,381.721460768791));
#40857=CARTESIAN_POINT('Ctrl Pts',(0.145408264526719,-4.70589129277765,
381.642332893331));
#40858=CARTESIAN_POINT('Ctrl Pts',(-2.11664502645219,-4.20551664541093,
381.563205017872));
#40859=CARTESIAN_POINT('Ctrl Pts',(-3.86618822286509,-2.68684667374458,
381.484077142412));
#40860=CARTESIAN_POINT('Ctrl Pts',(-4.67959878156707,-0.517601841562701,
381.404949266952));
#40861=CARTESIAN_POINT('Ctrl Pts',(-4.35992297760592,1.77697159577105,381.325821391492));
#40862=CARTESIAN_POINT('Ctrl Pts',(-2.98456494557718,3.6412811630613,381.246693516033));
#40863=CARTESIAN_POINT('Ctrl Pts',(-0.886544566588966,4.62391556522009,
381.167565640573));
#40864=CARTESIAN_POINT('Ctrl Pts',(1.4261377108192,4.48694636168212,381.088437765113));
#40865=CARTESIAN_POINT('Ctrl Pts',(3.39350465953423,3.26353834795189,381.009309889653));
#40866=CARTESIAN_POINT('Ctrl Pts',(4.53919136794792,1.2499192565843,380.930182014193));
#40867=CARTESIAN_POINT('Ctrl Pts',(4.58578901411133,-1.06634682017112,380.851054138734));
#40868=CARTESIAN_POINT('Ctrl Pts',(3.52201475950248,-3.12441489829372,380.771926263274));
#40869=CARTESIAN_POINT('Ctrl Pts',(1.60544369914822,-4.42595830885227,380.692798387814));
#40870=CARTESIAN_POINT('Ctrl Pts',(-0.699858627803908,-4.65583014337095,
380.613670512354));
#40871=CARTESIAN_POINT('Ctrl Pts',(-2.83570192547335,-3.75837079233806,
380.534542636895));
#40872=CARTESIAN_POINT('Ctrl Pts',(-4.28492755989611,-1.95088498617316,
380.455414761435));
#40873=CARTESIAN_POINT('Ctrl Pts',(-4.69662984888973,0.32897490079206,380.376286885975));
#40874=CARTESIAN_POINT('Ctrl Pts',(-3.97112198789876,2.52917903282076,380.297159010515));
#40875=CARTESIAN_POINT('Ctrl Pts',(-2.28407353785474,4.11698487931458,380.218031135056));
#40876=CARTESIAN_POINT('Ctrl Pts',(-0.0439749871787381,4.70793188388869,
380.138903259595));
#40877=CARTESIAN_POINT('Ctrl Pts',(2.20677136913111,4.15893214025144,380.059775384136));
#40878=CARTESIAN_POINT('Ctrl Pts',(3.92318504851847,2.60291672896277,379.980647508676));
#40879=CARTESIAN_POINT('Ctrl Pts',(4.68966526476571,0.416648685685039,379.901519633216));
#40880=CARTESIAN_POINT('Ctrl Pts',(4.32062168826984,-1.8705038491501,379.822391757756));
#40881=CARTESIAN_POINT('Ctrl Pts',(2.90541203179102,-3.70474524743025,379.743263882297));
#40882=CARTESIAN_POINT('Ctrl Pts',(0.786705578939987,-4.64194471691529,
379.664136006837));
#40883=CARTESIAN_POINT('Ctrl Pts',(-1.52248843588733,-4.45517512399035,
379.585008131377));
#40884=CARTESIAN_POINT('Ctrl Pts',(-3.46303740985959,-3.18965959323972,
379.505880255917));
#40885=CARTESIAN_POINT('Ctrl Pts',(-4.56506995418396,-1.15182148627296,
379.426752380458));
#40886=CARTESIAN_POINT('Ctrl Pts',(-4.56174737061485,1.16491087621397,379.347624504998));
#40887=CARTESIAN_POINT('Ctrl Pts',(-3.45387416703998,3.19957960693074,379.268496629538));
#40888=CARTESIAN_POINT('Ctrl Pts',(-1.50970325938777,4.45952379648624,379.189368754078));
#40889=CARTESIAN_POINT('Ctrl Pts',(0.800016973052387,4.63966909010343,379.110240878619));
#40890=CARTESIAN_POINT('Ctrl Pts',(2.91602651267941,3.69639632617822,379.031113003159));
#40891=CARTESIAN_POINT('Ctrl Pts',(4.32596913740423,1.85810318471799,378.951985127699));
#40892=CARTESIAN_POINT('Ctrl Pts',(4.68845088702114,-0.430098480378534,
378.872857252239));
#40893=CARTESIAN_POINT('Ctrl Pts',(3.91570288509923,-2.61415901170123,378.79372937678));
#40894=CARTESIAN_POINT('Ctrl Pts',(2.19483310042462,-4.16524478081583,378.714601501319));
#40895=CARTESIAN_POINT('Ctrl Pts',(-0.0574787096237898,-4.70778638223669,
378.63547362586));
#40896=CARTESIAN_POINT('Ctrl Pts',(-2.29587301412136,-4.11041646623094,
378.5563457504));
#40897=CARTESIAN_POINT('Ctrl Pts',(-3.97836017269986,-2.5177781393738,378.47721787494));
#40898=CARTESIAN_POINT('Ctrl Pts',(-4.69755413716848,-0.315502062123824,
378.398089999481));
#40899=CARTESIAN_POINT('Ctrl Pts',(-4.27931415074721,1.96316754813432,378.318962124021));
#40900=CARTESIAN_POINT('Ctrl Pts',(-2.82491001177881,3.76648906120608,378.239834248561));
#40901=CARTESIAN_POINT('Ctrl Pts',(-0.686501290471962,4.65781841649216,
378.160706373101));
#40902=CARTESIAN_POINT('Ctrl Pts',(1.61813220490064,4.421335159236,378.081578497641));
#40903=CARTESIAN_POINT('Ctrl Pts',(3.5309621248084,3.11429974408401,378.002450622182));
#40904=CARTESIAN_POINT('Ctrl Pts',(4.58882878451957,1.05318887631696,377.923322746722));
#40905=CARTESIAN_POINT('Ctrl Pts',(4.53558751403461,-1.26293401465255,377.844194871262));
#40906=CARTESIAN_POINT('Ctrl Pts',(3.38412979408371,-3.27325861484057,377.765066995802));
#40907=CARTESIAN_POINT('Ctrl Pts',(1.41326180027294,-4.49101853778431,377.685939120342));
#40908=CARTESIAN_POINT('Ctrl Pts',(-0.899803836436171,-4.62135364138776,
377.606811244883));
#40909=CARTESIAN_POINT('Ctrl Pts',(-2.99499706490511,-3.63270546618397,
377.527683369423));
#40910=CARTESIAN_POINT('Ctrl Pts',(-4.36500198367802,-1.76445858702323,
377.448555493963));
#40911=CARTESIAN_POINT('Ctrl Pts',(-4.67809487824384,0.531022346970404,
377.369427618503));
#40912=CARTESIAN_POINT('Ctrl Pts',(-3.858465555114,2.69792512550514,377.290299743043));
#40913=CARTESIAN_POINT('Ctrl Pts',(-2.10457350875104,4.21157058222897,377.211171867584));
#40914=CARTESIAN_POINT('Ctrl Pts',(0.158905716619817,4.70545485538416,377.132043992124));
#40915=CARTESIAN_POINT('Ctrl Pts',(2.38390858774424,4.05999215123785,377.052916116664));
#40916=CARTESIAN_POINT('Ctrl Pts',(4.03168797525527,2.43147043844132,376.973788241204));
#40917=CARTESIAN_POINT('Ctrl Pts',(4.70326173563702,0.21420893755303,376.894660365745));
#40918=CARTESIAN_POINT('Ctrl Pts',(4.23601954588194,-2.0549196650327,376.815532490285));
#40919=CARTESIAN_POINT('Ctrl Pts',(2.74309626604883,-3.82648393411214,376.736404614825));
#40920=CARTESIAN_POINT('Ctrl Pts',(0.585978230290955,-4.67152929311995,
376.657276739365));
#40921=CARTESIAN_POINT('Ctrl Pts',(-1.71302460639056,-4.38544218074737,
376.578148863906));
#40922=CARTESIAN_POINT('Ctrl Pts',(-3.59724726405772,-3.03749379327437,
376.499020988446));
#40923=CARTESIAN_POINT('Ctrl Pts',(-4.61045682670426,-0.954067226005277,
376.419893112986));
#40924=CARTESIAN_POINT('Ctrl Pts',(-4.50732159153776,1.36037071913331,376.340765237526));
#40925=CARTESIAN_POINT('Ctrl Pts',(-3.31281402583599,3.34541770982772,376.261637362067));
#40926=CARTESIAN_POINT('Ctrl Pts',(-1.31616410382415,4.52042790819332,376.182509486607));
#40927=CARTESIAN_POINT('Ctrl Pts',(0.999172883001983,4.60089230230265,376.103381611147));
#40928=CARTESIAN_POINT('Ctrl Pts',(3.07257691207793,3.5673277858007,376.024253735687));
#40929=CARTESIAN_POINT('Ctrl Pts',(4.40200797556968,1.66999467821426,375.945125860228));
#40930=CARTESIAN_POINT('Ctrl Pts',(4.66556662820138,-0.631699641477607,
375.865997984767));
#40931=CARTESIAN_POINT('Ctrl Pts',(3.79943658220811,-2.78043846928895,375.786870109308));
#40932=CARTESIAN_POINT('Ctrl Pts',(2.01333666035538,-4.25594079109181,375.707742233848));
#40933=CARTESIAN_POINT('Ctrl Pts',(-0.260258907652536,-4.70093834665202,
375.628614358388));
#40934=CARTESIAN_POINT('Ctrl Pts',(-2.47083727331916,-4.00768269259632,
375.549486482929));
#40935=CARTESIAN_POINT('Ctrl Pts',(-4.08314356267804,-2.34403352650038,
375.470358607469));
#40936=CARTESIAN_POINT('Ctrl Pts',(-4.70678568739368,-0.112816719080636,
375.391230732009));
#40937=CARTESIAN_POINT('Ctrl Pts',(-4.19075739000426,2.14571838351356,375.312102856549));
#40938=CARTESIAN_POINT('Ctrl Pts',(-2.66001002678919,3.8847003407523,375.232974981089));
#40939=CARTESIAN_POINT('Ctrl Pts',(-0.48518044668226,4.68307451075752,375.153847105629));
#40940=CARTESIAN_POINT('Ctrl Pts',(1.80711601134657,4.34750540330396,375.07471923017));
#40941=CARTESIAN_POINT('Ctrl Pts',(3.66187380043387,2.9592933100083,374.99559135471));
#40942=CARTESIAN_POINT('Ctrl Pts',(4.62991897355734,0.854469882696709,374.91646347925));
#40943=CARTESIAN_POINT('Ctrl Pts',(4.477014386818,-1.45709927207541,374.837335603791));
#40944=CARTESIAN_POINT('Ctrl Pts',(3.23983968516725,-3.41613747848395,374.758207728331));
#40945=CARTESIAN_POINT('Ctrl Pts',(1.8923805371004,-4.17007422695688,374.705455811358));
#40946=CARTESIAN_POINT('Ctrl Pts',(1.16918346556986,-4.36383719750612,374.679079852871));
#40947=CARTESIAN_POINT('Ctrl Pts',(3.57461543774233,3.05624720968358,400.106973382376));
#40948=CARTESIAN_POINT('Ctrl Pts',(4.0811121130032,2.46384394177512,400.08059742389));
#40949=CARTESIAN_POINT('Ctrl Pts',(4.79330604666853,1.02286901533234,400.027845506917));
#40950=CARTESIAN_POINT('Ctrl Pts',(4.70079893715141,-1.38736907251624,399.948717631457));
#40951=CARTESIAN_POINT('Ctrl Pts',(3.47003520682193,-3.46129852254691,399.869589755997));
#40952=CARTESIAN_POINT('Ctrl Pts',(1.39906460383401,-4.69732448980706,399.790461880537));
#40953=CARTESIAN_POINT('Ctrl Pts',(-1.01066992750072,-4.79588345555735,
399.711334005077));
#40954=CARTESIAN_POINT('Ctrl Pts',(-3.17568611614676,-3.73324183578399,
399.632206129617));
#40955=CARTESIAN_POINT('Ctrl Pts',(-4.57176395161188,-1.76663842906183,
399.553078254158));
#40956=CARTESIAN_POINT('Ctrl Pts',(-4.86086545663507,0.627717441216646,
399.473950378698));
#40957=CARTESIAN_POINT('Ctrl Pts',(-3.97299008611081,2.8700865038691,399.394822503238));
#40958=CARTESIAN_POINT('Ctrl Pts',(-2.12312171649347,4.41751015439781,399.315694627778));
#40959=CARTESIAN_POINT('Ctrl Pts',(0.240824931085231,4.89530880016116,399.236566752319));
#40960=CARTESIAN_POINT('Ctrl Pts',(2.54645987869621,4.18779005099161,399.157438876859));
#40961=CARTESIAN_POINT('Ctrl Pts',(4.23551226517086,2.46626839669468,399.078311001399));
#40962=CARTESIAN_POINT('Ctrl Pts',(4.89900639514296,0.147581107578247,398.999183125939));
#40963=CARTESIAN_POINT('Ctrl Pts',(4.37628828662539,-2.20684042213451,398.920055250479));
#40964=CARTESIAN_POINT('Ctrl Pts',(2.79392536583327,-4.02691257828985,398.84092737502));
#40965=CARTESIAN_POINT('Ctrl Pts',(0.53506027464146,-4.87193537854724,398.76179949956));
#40966=CARTESIAN_POINT('Ctrl Pts',(-1.85336068827152,-4.53730074011451,
398.6826716241));
#40967=CARTESIAN_POINT('Ctrl Pts',(-3.7930214436213,-3.10403482078447,398.60354374864));
#40968=CARTESIAN_POINT('Ctrl Pts',(-4.81426566971713,-0.919178929028494,
398.524415873181));
#40969=CARTESIAN_POINT('Ctrl Pts',(-4.6698162047254,1.48824072524753,398.445287997721));
#40970=CARTESIAN_POINT('Ctrl Pts',(-3.39464906397748,3.53530784716552,398.366160122261));
#40971=CARTESIAN_POINT('Ctrl Pts',(-1.29752458459001,4.7263594652241,398.287032246801));
#40972=CARTESIAN_POINT('Ctrl Pts',(1.1137737119676,4.77300240524464,398.207904371341));
#40973=CARTESIAN_POINT('Ctrl Pts',(3.25539038344674,3.66394286164299,398.128776495882));
#40974=CARTESIAN_POINT('Ctrl Pts',(4.60876887024317,1.66772100264832,398.049648620422));
#40975=CARTESIAN_POINT('Ctrl Pts',(4.84621126950363,-0.732311527518088,
397.970520744962));
#40976=CARTESIAN_POINT('Ctrl Pts',(3.91022488643166,-2.95502710301166,397.891392869503));
#40977=CARTESIAN_POINT('Ctrl Pts',(2.02744312611193,-4.46223242473778,397.812264994043));
#40978=CARTESIAN_POINT('Ctrl Pts',(-0.346249984625578,-4.88898300162196,
397.733137118583));
#40979=CARTESIAN_POINT('Ctrl Pts',(-2.63610446859942,-4.13194833857237,
397.654009243123));
#40980=CARTESIAN_POINT('Ctrl Pts',(-4.28767046602801,-2.3744316828985,397.574881367663));
#40981=CARTESIAN_POINT('Ctrl Pts',(-4.90104896930931,-0.0419862171810207,
397.495753492204));
#40982=CARTESIAN_POINT('Ctrl Pts',(-4.3277206609419,2.30062550686931,397.416625616744));
#40983=CARTESIAN_POINT('Ctrl Pts',(-2.70650737541695,4.08617934858649,397.337497741284));
#40984=CARTESIAN_POINT('Ctrl Pts',(-0.429958720199221,4.88233339100534,
397.258369865824));
#40985=CARTESIAN_POINT('Ctrl Pts',(1.95069722820886,4.49631228517985,397.179241990364));
#40986=CARTESIAN_POINT('Ctrl Pts',(3.85902455825875,3.0215845678645,397.100114114904));
#40987=CARTESIAN_POINT('Ctrl Pts',(4.83295381183918,0.815230822914742,397.020986239445));
#40988=CARTESIAN_POINT('Ctrl Pts',(4.63666435411759,-1.58851739343839,396.941858363985));
#40989=CARTESIAN_POINT('Ctrl Pts',(3.31768438527967,-3.60763276424756,396.862730488525));
#40990=CARTESIAN_POINT('Ctrl Pts',(1.19538278395727,-4.75322036537541,396.783602613066));
#40991=CARTESIAN_POINT('Ctrl Pts',(-1.21636071054614,-4.7478953720402,396.704474737606));
#40992=CARTESIAN_POINT('Ctrl Pts',(-3.33358285876919,-3.59294714207171,
396.625346862146));
#40993=CARTESIAN_POINT('Ctrl Pts',(-4.64363382578808,-1.5680270195369,396.546218986686));
#40994=CARTESIAN_POINT('Ctrl Pts',(-4.82930674101173,0.836564548148951,
396.467091111227));
#40995=CARTESIAN_POINT('Ctrl Pts',(-3.84564402196864,3.03859604065724,396.387963235766));
#40996=CARTESIAN_POINT('Ctrl Pts',(-1.93082309891163,4.50488246269648,396.308835360307));
#40997=CARTESIAN_POINT('Ctrl Pts',(0.451514255406424,4.88038714849199,396.229707484847));
#40998=CARTESIAN_POINT('Ctrl Pts',(2.724525005195,4.07418793602703,396.150579609387));
#40999=CARTESIAN_POINT('Ctrl Pts',(4.33783771841656,2.28149244370514,396.071451733927));
#41000=CARTESIAN_POINT('Ctrl Pts',(4.90081577868788,-0.063628180588346,
395.992323858468));
#41001=CARTESIAN_POINT('Ctrl Pts',(4.27714349050859,-2.39334230807068,395.913195983008));
#41002=CARTESIAN_POINT('Ctrl Pts',(2.61783263875445,-4.14354873477711,395.834068107548));
#41003=CARTESIAN_POINT('Ctrl Pts',(0.324657517612272,-4.89046432747023,
395.754940232088));
#41004=CARTESIAN_POINT('Ctrl Pts',(-2.04712797653699,-4.45323600201927,
395.675812356629));
#41005=CARTESIAN_POINT('Ctrl Pts',(-3.92323576387579,-2.93773126460658,
395.596684481169));
#41006=CARTESIAN_POINT('Ctrl Pts',(-4.84939780820125,-0.710904170626361,
395.517556605709));
#41007=CARTESIAN_POINT('Ctrl Pts',(-4.6013595032905,1.68805644558445,395.438428730249));
#41008=CARTESIAN_POINT('Ctrl Pts',(-3.23917916478794,3.67828250415935,395.35930085479));
#41009=CARTESIAN_POINT('Ctrl Pts',(-1.09268591631945,4.77787414341129,395.28017297933));
#41010=CARTESIAN_POINT('Ctrl Pts',(1.31838290117699,4.72058368932118,395.20104510387));
#41011=CARTESIAN_POINT('Ctrl Pts',(3.41022740996214,3.52028306451966,395.12191722841));
#41012=CARTESIAN_POINT('Ctrl Pts',(4.6763425448897,1.46760493487027,395.04278935295));
#41013=CARTESIAN_POINT('Ctrl Pts',(4.81015976025467,-0.940429116322842,
394.963661477491));
#41014=CARTESIAN_POINT('Ctrl Pts',(3.77927746162617,-3.12075402908423,394.884533602031));
#41015=CARTESIAN_POINT('Ctrl Pts',(1.83330650852657,-4.54544069236363,394.805405726571));
#41016=CARTESIAN_POINT('Ctrl Pts',(-0.556568868938532,-4.8695251242939,
394.726277851111));
#41017=CARTESIAN_POINT('Ctrl Pts',(-2.81168042909494,-4.01453571495453,
394.647149975651));
#41018=CARTESIAN_POINT('Ctrl Pts',(-4.3859907284844,-2.18749381065409,394.568022100192));
#41019=CARTESIAN_POINT('Ctrl Pts',(-4.89830693111745,0.169213033090633,
394.488894224732));
#41020=CARTESIAN_POINT('Ctrl Pts',(-4.2245802606628,2.48494777877106,394.409766349272));
#41021=CARTESIAN_POINT('Ctrl Pts',(-2.52794233119419,4.19899409527539,394.330638473813));
#41022=CARTESIAN_POINT('Ctrl Pts',(-0.219205562748669,4.89632441360466,
394.251510598353));
#41023=CARTESIAN_POINT('Ctrl Pts',(2.14260815638517,4.40809189221286,394.172382722893));
#41024=CARTESIAN_POINT('Ctrl Pts',(3.98562524447155,2.85251384792995,394.093254847433));
#41025=CARTESIAN_POINT('Ctrl Pts',(4.86359002316223,0.606247415332937,394.014126971973));
#41026=CARTESIAN_POINT('Ctrl Pts',(4.56391804578379,-1.78681166141541,393.934999096514));
#41027=CARTESIAN_POINT('Ctrl Pts',(3.15916985581216,-3.74722426125376,393.855871221054));
#41028=CARTESIAN_POINT('Ctrl Pts',(0.989481668194294,-4.80030935152189,
393.776743345594));
#41029=CARTESIAN_POINT('Ctrl Pts',(-1.41979291062284,-4.69108003906842,
393.697615470134));
#41030=CARTESIAN_POINT('Ctrl Pts',(-3.48528844770473,-3.44598437000184,
393.618487594675));
#41031=CARTESIAN_POINT('Ctrl Pts',(-4.70687983950021,-1.3665013788897,393.539359719215));
#41032=CARTESIAN_POINT('Ctrl Pts',(-4.788779217989,1.04385700330924,393.460231843755));
#41033=CARTESIAN_POINT('Ctrl Pts',(-3.71115602221747,3.2014629188482,393.381103968295));
#41034=CARTESIAN_POINT('Ctrl Pts',(-1.7349386360522,4.58388828083041,393.301976092836));
#41035=CARTESIAN_POINT('Ctrl Pts',(0.661365043902099,4.85640197272687,393.222848217375));
#41036=CARTESIAN_POINT('Ctrl Pts',(2.89753027033354,3.95301937441519,393.143720341916));
#41037=CARTESIAN_POINT('Ctrl Pts',(4.43210713674341,2.09247943130372,393.064592466456));
#41038=CARTESIAN_POINT('Ctrl Pts',(4.89352359156256,-0.27471931279354,392.985464590996));
#41039=CARTESIAN_POINT('Ctrl Pts',(4.17005537874506,-2.57539938265902,392.906336715536));
#41040=CARTESIAN_POINT('Ctrl Pts',(2.43687819262455,-4.2524896844451,392.827208840076));
#41041=CARTESIAN_POINT('Ctrl Pts',(0.113651821430644,-4.89991092832171,
392.748080964617));
#41042=CARTESIAN_POINT('Ctrl Pts',(-2.23709343224997,-4.3609009180885,392.668953089157));
#41043=CARTESIAN_POINT('Ctrl Pts',(-4.04616402995999,-2.76597188790106,
392.589825213697));
#41044=CARTESIAN_POINT('Ctrl Pts',(-4.87552386667384,-0.501309153611575,
392.510697338238));
#41045=CARTESIAN_POINT('Ctrl Pts',(-4.52435736725662,1.88473718468963,392.431569462777));
#41046=CARTESIAN_POINT('Ctrl Pts',(-3.07769361007314,3.81442602294447,392.352441587318));
#41047=CARTESIAN_POINT('Ctrl Pts',(-0.885817961698088,4.82051557208708,
392.273313711858));
#41048=CARTESIAN_POINT('Ctrl Pts',(1.52054364990864,4.65939812107997,392.194185836399));
#41049=CARTESIAN_POINT('Ctrl Pts',(3.55873111796869,3.37008555855818,392.115057960939));
#41050=CARTESIAN_POINT('Ctrl Pts',(4.73523152985659,1.2647632982709,392.035930085479));
#41051=CARTESIAN_POINT('Ctrl Pts',(4.76517504210868,-1.14680018314682,391.956802210019));
#41052=CARTESIAN_POINT('Ctrl Pts',(3.64131133542052,-3.28068523338327,391.877674334559));
#41053=CARTESIAN_POINT('Ctrl Pts',(1.63576515787017,-4.62020737524832,391.7985464591));
#41054=CARTESIAN_POINT('Ctrl Pts',(-0.765854118981568,-4.84102378742762,
391.71941858364));
#41055=CARTESIAN_POINT('Ctrl Pts',(-2.98203466518281,-3.88966747905899,
391.64029070818));
#41056=CARTESIAN_POINT('Ctrl Pts',(-4.47616552938631,-1.99649342486641,
391.56116283272));
#41057=CARTESIAN_POINT('Ctrl Pts',(-4.88646798113091,0.380098028649711,
391.482034957261));
#41058=CARTESIAN_POINT('Ctrl Pts',(-4.11359416297415,2.66465511921264,391.402907081801));
#41059=CARTESIAN_POINT('Ctrl Pts',(-2.34468250799326,4.30401066201183,391.323779206341));
#41060=CARTESIAN_POINT('Ctrl Pts',(-0.00804530674402572,4.90122220625023,
391.244651330881));
#41061=CARTESIAN_POINT('Ctrl Pts',(2.33053993060416,4.31168499242009,391.165523455421));
#41062=CARTESIAN_POINT('Ctrl Pts',(4.10482400961136,2.67814556962822,391.086395579962));
#41063=CARTESIAN_POINT('Ctrl Pts',(4.88519379734561,0.396138112754947,391.007267704502));
#41064=CARTESIAN_POINT('Ctrl Pts',(4.48269583741255,-1.98178754442679,390.928139829042));
#41065=CARTESIAN_POINT('Ctrl Pts',(2.99478826045289,-3.87985658459878,390.849011953582));
#41066=CARTESIAN_POINT('Ctrl Pts',(0.781742932293461,-4.8384834225003,390.769884078122));
#41067=CARTESIAN_POINT('Ctrl Pts',(-1.62058833618616,-4.62555264661623,
390.690756202663));
#41068=CARTESIAN_POINT('Ctrl Pts',(-3.63052131820232,-3.29262187323105,
390.611628327203));
#41069=CARTESIAN_POINT('Ctrl Pts',(-4.76138445106458,-1.16243793432658,
390.532500451743));
#41070=CARTESIAN_POINT('Ctrl Pts',(-4.7393581930353,1.24921085494409,390.453372576283));
#41071=CARTESIAN_POINT('Ctrl Pts',(-3.56977583309043,3.35838418640342,390.374244700824));
#41072=CARTESIAN_POINT('Ctrl Pts',(-1.53583212443933,4.65438111111899,390.295116825364));
#41073=CARTESIAN_POINT('Ctrl Pts',(0.869987575460632,4.82339770914085,390.215988949904));
#41074=CARTESIAN_POINT('Ctrl Pts',(3.06515437466237,3.82450944586218,390.136861074444));
#41075=CARTESIAN_POINT('Ctrl Pts',(4.51814544822977,1.89958036172247,390.057733198985));
#41076=CARTESIAN_POINT('Ctrl Pts',(4.87714337604219,-0.485300248844855,
389.978605323525));
#41077=CARTESIAN_POINT('Ctrl Pts',(4.05522283069102,-2.75267354320184,389.899477448065));
#41078=CARTESIAN_POINT('Ctrl Pts',(2.25139808767325,-4.35353310459702,389.820349572605));
#41079=CARTESIAN_POINT('Ctrl Pts',(-0.0975649437201896,-4.9002576385082,
389.741221697145));
#41080=CARTESIAN_POINT('Ctrl Pts',(-2.42290426026896,-4.26046696825261,
389.662093821685));
#41081=CARTESIAN_POINT('Ctrl Pts',(-4.16157794510521,-2.58907567460185,
389.582965946226));
#41082=CARTESIAN_POINT('Ctrl Pts',(-4.89259532501792,-0.290783128145012,
389.503838070766));
#41083=CARTESIAN_POINT('Ctrl Pts',(-4.43895280146969,2.07791767602217,389.424710195306));
#41084=CARTESIAN_POINT('Ctrl Pts',(-2.91049230342699,3.9434855640275,389.345582319846));
#41085=CARTESIAN_POINT('Ctrl Pts',(-0.67730490643744,4.85420455952536,389.266454444387));
#41086=CARTESIAN_POINT('Ctrl Pts',(1.71988051445791,4.58955933156866,389.187326568927));
#41087=CARTESIAN_POINT('Ctrl Pts',(3.70062571316616,3.21362928370005,389.108198693467));
#41088=CARTESIAN_POINT('Ctrl Pts',(4.78532645921196,1.05957280106983,389.029070818007));
#41089=CARTESIAN_POINT('Ctrl Pts',(4.71134065862855,-1.35104146507597,388.949942942548));
#41090=CARTESIAN_POINT('Ctrl Pts',(3.49658273219959,-3.43452369898426,388.870815067087));
#41091=CARTESIAN_POINT('Ctrl Pts',(1.43518593891208,-4.68639362012519,388.791687191628));
#41092=CARTESIAN_POINT('Ctrl Pts',(-0.973717059752046,-4.80353192240344,
388.712559316168));
#41093=CARTESIAN_POINT('Ctrl Pts',(-3.14685080276043,-3.75757553046736,
388.633431440709));
#41094=CARTESIAN_POINT('Ctrl Pts',(-4.55802740021425,-1.80178524272377,
388.554303565248));
#41095=CARTESIAN_POINT('Ctrl Pts',(-4.8655541061066,0.590277123519319,388.475175689789));
#41096=CARTESIAN_POINT('Ctrl Pts',(-3.9949684861848,2.83941378393346,388.396047814329));
#41097=CARTESIAN_POINT('Ctrl Pts',(-2.15706824758342,4.401034016827,388.316919938869));
#41098=CARTESIAN_POINT('Ctrl Pts',(0.2031298906366,4.89701767298537,388.237792063409));
#41099=CARTESIAN_POINT('Ctrl Pts',(2.51414353256258,4.20727062829036,388.15866418795));
#41100=CARTESIAN_POINT('Ctrl Pts',(4.21639948317845,2.49880356175781,388.07953631249));
#41101=CARTESIAN_POINT('Ctrl Pts',(4.8977250128471,0.185293120576435,388.00040843703));
#41102=CARTESIAN_POINT('Ctrl Pts',(4.39314857117775,-2.17308294217223,387.92128056157));
#41103=CARTESIAN_POINT('Ctrl Pts',(2.82484488118912,-4.00528341559255,387.842152686111));
#41104=CARTESIAN_POINT('Ctrl Pts',(0.572552379142054,-4.86767168317048,
387.763024810651));
#41105=CARTESIAN_POINT('Ctrl Pts',(-1.8183740791475,-4.55143488916249,387.683896935191));
#41106=CARTESIAN_POINT('Ctrl Pts',(-3.76901175041157,-3.13314446958014,
387.604769059731));
#41107=CARTESIAN_POINT('Ctrl Pts',(-4.80704643700727,-0.956215663151738,
387.525641184272));
#41108=CARTESIAN_POINT('Ctrl Pts',(-4.68113544861982,1.45224472926429,387.446513308812));
#41109=CARTESIAN_POINT('Ctrl Pts',(-3.4217660194141,3.50906841631565,387.367385433352));
#41110=CARTESIAN_POINT('Ctrl Pts',(-1.33387333558782,4.71623003749912,387.288257557892));
#41111=CARTESIAN_POINT('Ctrl Pts',(1.07699440584981,4.78143565174407,387.209129682432));
#41112=CARTESIAN_POINT('Ctrl Pts',(3.22708601435485,3.68889681313483,387.130001806972));
#41113=CARTESIAN_POINT('Ctrl Pts',(4.59579286645524,1.70315347829848,387.050873931513));
#41114=CARTESIAN_POINT('Ctrl Pts',(4.85170555271451,-0.694979907450764,
386.971746056053));
#41115=CARTESIAN_POINT('Ctrl Pts',(3.93285910810722,-2.92483556422906,386.892618180594));
#41116=CARTESIAN_POINT('Ctrl Pts',(2.06173678907561,-4.44649134201037,386.813490305133));
#41117=CARTESIAN_POINT('Ctrl Pts',(-0.308600515715983,-4.89150381413537,
386.734362429674));
#41118=CARTESIAN_POINT('Ctrl Pts',(-2.60421538121517,-4.15212067385372,
386.655234554214));
#41119=CARTESIAN_POINT('Ctrl Pts',(-4.26926316786226,-2.40737114827269,
386.576106678754));
#41120=CARTESIAN_POINT('Ctrl Pts',(-4.90058047890116,-0.0797170735407659,
386.496978803294));
#41121=CARTESIAN_POINT('Ctrl Pts',(-4.34530441538657,2.26723915360136,386.417850927834));
#41122=CARTESIAN_POINT('Ctrl Pts',(-2.7378857634756,4.06522144392636,386.338723052375));
#41123=CARTESIAN_POINT('Ctrl Pts',(-0.46753399145535,4.87887854007813,386.259595176915));
#41124=CARTESIAN_POINT('Ctrl Pts',(1.91602329550907,4.51119702219572,386.180467301455));
#41125=CARTESIAN_POINT('Ctrl Pts',(3.83564767539653,3.05120480338935,386.101339425996));
#41126=CARTESIAN_POINT('Ctrl Pts',(4.82653429894221,0.852414513681883,386.022211550536));
#41127=CARTESIAN_POINT('Ctrl Pts',(4.6487565885712,-1.55277365453466,385.943083675076));
#41128=CARTESIAN_POINT('Ctrl Pts',(3.34536043531169,-3.58198372411883,385.863955799616));
#41129=CARTESIAN_POINT('Ctrl Pts',(1.23194135821188,-4.74387650892475,385.784827924157));
#41130=CARTESIAN_POINT('Ctrl Pts',(-1.17977165769507,-4.75711915739983,
385.705700048696));
#41131=CARTESIAN_POINT('Ctrl Pts',(-3.30582275282872,-3.61850518431036,
385.626572173237));
#41132=CARTESIAN_POINT('Ctrl Pts',(-4.63142431084255,-1.60373086736447,
385.547444297777));
#41133=CARTESIAN_POINT('Ctrl Pts',(-4.8356041463375,0.799359982689007,385.468316422318));
#41134=CARTESIAN_POINT('Ctrl Pts',(-3.86892353648086,3.00889921912741,385.389188546857));
#41135=CARTESIAN_POINT('Ctrl Pts',(-1.96544797859558,4.48988397238009,385.310060671398));
#41136=CARTESIAN_POINT('Ctrl Pts',(0.413927844466849,4.88371862227708,385.230932795938));
#41137=CARTESIAN_POINT('Ctrl Pts',(2.69307798204115,4.09504271340925,385.151804920478));
#41138=CARTESIAN_POINT('Ctrl Pts',(4.32014445230215,2.31482089010014,385.072677045018));
#41139=CARTESIAN_POINT('Ctrl Pts',(4.90116039726593,-0.0258959895184648,
384.993549169559));
#41140=CARTESIAN_POINT('Ctrl Pts',(4.29544255017007,-2.3603425895809,384.914421294099));
#41141=CARTESIAN_POINT('Ctrl Pts',(2.6496553290988,-4.12327181725621,384.835293418639));
#41142=CARTESIAN_POINT('Ctrl Pts',(0.362298507876016,-4.88781992642853,
384.756165543179));
#41143=CARTESIAN_POINT('Ctrl Pts',(-2.01278282086323,-4.46886441481938,
384.67703766772));
#41144=CARTESIAN_POINT('Ctrl Pts',(-3.90050254623037,-2.96784833319553,
384.59790979226));
#41145=CARTESIAN_POINT('Ctrl Pts',(-4.84378099597461,-0.748217551943446,
384.5187819168));
#41146=CARTESIAN_POINT('Ctrl Pts',(-4.61421911336287,1.65258156103648,384.43965404134));
#41147=CARTESIAN_POINT('Ctrl Pts',(-3.26740145825086,3.65323576471889,384.36052616588));
#41148=CARTESIAN_POINT('Ctrl Pts',(-1.12943733813143,4.76932019697102,384.281398290421));
#41149=CARTESIAN_POINT('Ctrl Pts',(1.28200109144381,4.730593730552,384.202270414961));
#41150=CARTESIAN_POINT('Ctrl Pts',(3.38302445736953,3.54643332981752,384.123142539501));
#41151=CARTESIAN_POINT('Ctrl Pts',(4.66490518818293,1.50356357606356,384.044014664042));
#41152=CARTESIAN_POINT('Ctrl Pts',(4.81725736354257,-0.903368881131035,
383.964886788581));
#41153=CARTESIAN_POINT('Ctrl Pts',(3.80319145930759,-3.09156571430251,383.885758913122));
#41154=CARTESIAN_POINT('Ctrl Pts',(1.86824652712842,-4.53119175889452,383.806631037662));
#41155=CARTESIAN_POINT('Ctrl Pts',(-0.519062968936094,-4.87366571240583,
383.727503162202));
#41156=CARTESIAN_POINT('Ctrl Pts',(-2.78069007236013,-4.03606325067867,
383.648375286742));
#41157=CARTESIAN_POINT('Ctrl Pts',(-4.36901971015636,-2.22119576225652,
383.569247411283));
#41158=CARTESIAN_POINT('Ctrl Pts',(-4.89946449866066,0.131497027969629,
383.490119535823));
#41159=CARTESIAN_POINT('Ctrl Pts',(-4.24358612851044,2.45235001823044,383.410991660363));
#41160=CARTESIAN_POINT('Ctrl Pts',(-2.56019454719736,4.17940758032786,383.331863784903));
#41161=CARTESIAN_POINT('Ctrl Pts',(-0.256894793709217,4.89449169035623,
383.252735909444));
#41162=CARTESIAN_POINT('Ctrl Pts',(2.10860772565226,4.4244567238612,383.173608033984));
#41163=CARTESIAN_POINT('Ctrl Pts',(3.96354624804163,2.88311376494861,383.094480158524));
#41164=CARTESIAN_POINT('Ctrl Pts',(4.85877851973045,0.643673161011885,383.015352283064));
#41165=CARTESIAN_POINT('Ctrl Pts',(4.57753906021165,-1.7516221037192,382.936224407605));
#41166=CARTESIAN_POINT('Ctrl Pts',(3.18792528789615,-3.72279145276676,382.857096532144));
#41167=CARTESIAN_POINT('Ctrl Pts',(1.0264088723172,-4.79254928705272,382.777968656685));
#41168=CARTESIAN_POINT('Ctrl Pts',(-1.38363523762741,-4.70187168808304,
382.698840781225));
#41169=CARTESIAN_POINT('Ctrl Pts',(-3.45865527994654,-3.47271471567979,
382.619712905766));
#41170=CARTESIAN_POINT('Ctrl Pts',(-4.69621995188282,-1.40269811632394,
382.540585030305));
#41171=CARTESIAN_POINT('Ctrl Pts',(-4.79667372352029,1.00695830702717,382.461457154846));
#41172=CARTESIAN_POINT('Ctrl Pts',(-3.73569339878306,3.17279666418915,382.382329279386));
#41173=CARTESIAN_POINT('Ctrl Pts',(-1.77017756943694,4.57039552059375,382.303201403927));
#41174=CARTESIAN_POINT('Ctrl Pts',(0.623957070419554,4.86134975251467,382.224073528466));
#41175=CARTESIAN_POINT('Ctrl Pts',(2.86701097015694,3.97520967233186,382.144945653007));
#41176=CARTESIAN_POINT('Ctrl Pts',(4.41586624656651,2.12653923886574,382.065817777547));
#41177=CARTESIAN_POINT('Ctrl Pts',(4.89549357056314,-0.237037006764906,
381.986689902087));
#41178=CARTESIAN_POINT('Ctrl Pts',(4.18975922954695,-2.54321871659263,381.907562026627));
#41179=CARTESIAN_POINT('Ctrl Pts',(2.46954495821251,-4.2336026669219,381.828434151167));
#41180=CARTESIAN_POINT('Ctrl Pts',(0.151371792377024,-4.89889073387779,
381.749306275708));
#41181=CARTESIAN_POINT('Ctrl Pts',(-2.20345351430222,-4.37799456969858,
381.670178400248));
#41182=CARTESIAN_POINT('Ctrl Pts',(-4.0247495069615,-2.79704044450812,381.591050524788));
#41183=CARTESIAN_POINT('Ctrl Pts',(-4.87151990622233,-0.53882988528894,
381.511922649328));
#41184=CARTESIAN_POINT('Ctrl Pts',(-4.53873346122441,1.84984929385154,381.432794773869));
#41185=CARTESIAN_POINT('Ctrl Pts',(-3.10696882840965,3.79061849060175,381.353666898409));
#41186=CARTESIAN_POINT('Ctrl Pts',(-0.922903801262455,4.8135529929166,381.274539022949));
#41187=CARTESIAN_POINT('Ctrl Pts',(1.48462690319438,4.67096636685734,381.195411147489));
#41188=CARTESIAN_POINT('Ctrl Pts',(3.53268010195595,3.39738357258133,381.11628327203));
#41189=CARTESIAN_POINT('Ctrl Pts',(4.72535406116718,1.30118132426344,381.03715539657));
#41190=CARTESIAN_POINT('Ctrl Pts',(4.77386278412913,-1.11008015940651,380.95802752111));
#41191=CARTESIAN_POINT('Ctrl Pts',(3.66646069712405,-3.25255434980657,380.87889964565));
#41192=CARTESIAN_POINT('Ctrl Pts',(1.67128664310421,-4.60747705350581,380.799771770191));
#41193=CARTESIAN_POINT('Ctrl Pts',(-0.728561442129978,-4.84677646142697,
380.72064389473));
#41194=CARTESIAN_POINT('Ctrl Pts',(-2.95200059297187,-3.91251023527028,
380.641516019271));
#41195=CARTESIAN_POINT('Ctrl Pts',(-4.46066230869571,-2.03089527297259,
380.562388143811));
#41196=CARTESIAN_POINT('Ctrl Pts',(-4.88924945684393,0.342466919208695,
380.483260268352));
#41197=CARTESIAN_POINT('Ctrl Pts',(-4.13398684739545,2.63290649047066,380.404132392891));
#41198=CARTESIAN_POINT('Ctrl Pts',(-2.37774865459918,4.28583191195745,380.325004517432));
#41199=CARTESIAN_POINT('Ctrl Pts',(-0.045778502691498,4.90101501433043,
380.245876641972));
#41200=CARTESIAN_POINT('Ctrl Pts',(2.29727614588441,4.32949952668338,380.166748766512));
#41201=CARTESIAN_POINT('Ctrl Pts',(4.08408390371697,2.70966833937311,380.087620891052));
#41202=CARTESIAN_POINT('Ctrl Pts',(4.88199923908331,0.433736407961101,380.008493015593));
#41203=CARTESIAN_POINT('Ctrl Pts',(4.49782033548913,-1.94721752037656,379.929365140133));
#41204=CARTESIAN_POINT('Ctrl Pts',(3.02456967131446,-3.8566853832489,379.850237264673));
#41205=CARTESIAN_POINT('Ctrl Pts',(0.818970186768649,-4.83232156164975,
379.771109389213));
#41206=CARTESIAN_POINT('Ctrl Pts',(-1.5849291934243,-4.63789211752843,379.691981513754));
#41207=CARTESIAN_POINT('Ctrl Pts',(-3.60506455052847,-3.32047487997185,
379.612853638294));
#41208=CARTESIAN_POINT('Ctrl Pts',(-4.75229398783147,-1.19906033844088,
379.533725762834));
#41209=CARTESIAN_POINT('Ctrl Pts',(-4.74883513745721,1.21268655441244,379.454597887374));
#41210=CARTESIAN_POINT('Ctrl Pts',(-3.59552550201493,3.33080173627333,379.375470011914));
#41211=CARTESIAN_POINT('Ctrl Pts',(-1.57161966738812,4.64241913909978,379.296342136455));
#41212=CARTESIAN_POINT('Ctrl Pts',(0.832827511814025,4.82995260614083,379.217214260995));
#41213=CARTESIAN_POINT('Ctrl Pts',(3.03561947651265,3.84799405350607,379.138086385535));
#41214=CARTESIAN_POINT('Ctrl Pts',(4.50338709582942,1.93430827613337,379.058958510075));
#41215=CARTESIAN_POINT('Ctrl Pts',(4.88073505691033,-0.447737809714184,
378.979830634616));
#41216=CARTESIAN_POINT('Ctrl Pts',(4.07629487954206,-2.72137169402128,378.900702759156));
#41217=CARTESIAN_POINT('Ctrl Pts',(2.28484826128058,-4.33607106317736,378.821574883696));
#41218=CARTESIAN_POINT('Ctrl Pts',(-0.0598360438974424,-4.90086354532054,
378.742447008237));
#41219=CARTESIAN_POINT('Ctrl Pts',(-2.39003205456549,-4.27899411312408,
378.663319132776));
#41220=CARTESIAN_POINT('Ctrl Pts',(-4.14152188682712,-2.62103802012351,
378.584191257317));
#41221=CARTESIAN_POINT('Ctrl Pts',(-4.89021165231393,-0.328441528394388,
378.505063381857));
#41222=CARTESIAN_POINT('Ctrl Pts',(-4.45481868070814,2.04368157109047,378.425935506397));
#41223=CARTESIAN_POINT('Ctrl Pts',(-2.94076607803947,3.92096145304356,378.346807630937));
#41224=CARTESIAN_POINT('Ctrl Pts',(-0.714656289627798,4.84884627820851,
378.267679755477));
#41225=CARTESIAN_POINT('Ctrl Pts',(1.68449553370326,4.60266429787517,378.188551880018));
#41226=CARTESIAN_POINT('Ctrl Pts',(3.67577501448982,3.24202434982427,378.109424004558));
#41227=CARTESIAN_POINT('Ctrl Pts',(4.77702722252339,1.09638257796792,378.030296129098));
#41228=CARTESIAN_POINT('Ctrl Pts',(4.72160240490404,-1.31472984753725,377.951168253638));
#41229=CARTESIAN_POINT('Ctrl Pts',(3.52292075167996,-3.40750249000403,377.872040378179));
#41230=CARTESIAN_POINT('Ctrl Pts',(1.47122292189925,-4.67520555228101,377.792912502719));
#41231=CARTESIAN_POINT('Ctrl Pts',(-0.936706864306466,-4.81088599868696,
377.713784627259));
#41232=CARTESIAN_POINT('Ctrl Pts',(-3.11782879297974,-3.78169108464289,
377.634656751799));
#41233=CARTESIAN_POINT('Ctrl Pts',(-4.54402076903412,-1.83682309779347,
377.555528876339));
#41234=CARTESIAN_POINT('Ctrl Pts',(-4.86995432435985,0.552800796535157,
377.47640100088));
#41235=CARTESIAN_POINT('Ctrl Pts',(-4.01671011481814,2.80857324909262,377.39727312542));
#41236=CARTESIAN_POINT('Ctrl Pts',(-2.19088691585556,4.3842967924097,377.31814524996));
#41237=CARTESIAN_POINT('Ctrl Pts',(0.165422806069439,4.89843639718154,377.2390173745));
#41238=CARTESIAN_POINT('Ctrl Pts',(2.48167816983692,4.22650178082969,377.159889499041));
#41239=CARTESIAN_POINT('Ctrl Pts',(4.19703678539643,2.53119064158134,377.080761623581));
#41240=CARTESIAN_POINT('Ctrl Pts',(4.89615333254211,0.222994139474255,377.001633748121));
#41241=CARTESIAN_POINT('Ctrl Pts',(4.40974846437591,-2.13919665363753,376.922505872661));
#41242=CARTESIAN_POINT('Ctrl Pts',(2.85559696215369,-3.98341685387501,376.843377997201));
#41243=CARTESIAN_POINT('Ctrl Pts',(0.610010547211784,-4.86311946946737,
376.764250121742));
#41244=CARTESIAN_POINT('Ctrl Pts',(-1.78327969114604,-4.56529926566563,
376.685122246282));
#41245=CARTESIAN_POINT('Ctrl Pts',(-3.74477865997579,-3.16206841006309,
376.605994370822));
#41246=CARTESIAN_POINT('Ctrl Pts',(-4.79954228053442,-0.99319572046786,
376.526866495362));
#41247=CARTESIAN_POINT('Ctrl Pts',(-4.69217723182007,1.41616265569688,376.447738619902));
#41248=CARTESIAN_POINT('Ctrl Pts',(-3.44868015951322,3.48262099568224,376.368610744443));
#41249=CARTESIAN_POINT('Ctrl Pts',(-1.37014302527182,4.70582106870975,376.289482868983));
#41250=CARTESIAN_POINT('Ctrl Pts',(1.04015126435086,4.78958549295691,376.210354993523));
#41251=CARTESIAN_POINT('Ctrl Pts',(3.1985903683765,3.71363211500125,376.131227118063));
#41252=CARTESIAN_POINT('Ctrl Pts',(4.58254446188996,1.73848500650345,376.052099242604));
#41253=CARTESIAN_POINT('Ctrl Pts',(4.85691226192656,-0.657607098782336,
375.972971367144));
#41254=CARTESIAN_POINT('Ctrl Pts',(3.95526022777064,-2.89447065515981,375.893843491684));
#41255=CARTESIAN_POINT('Ctrl Pts',(2.09590823415934,-4.43048672573689,375.814715616224));
#41256=CARTESIAN_POINT('Ctrl Pts',(-0.270932724915457,-4.89373465602332,
375.735587740765));
#41257=CARTESIAN_POINT('Ctrl Pts',(-2.57217200103202,-4.17204699080374,
375.656459865305));
#41258=CARTESIAN_POINT('Ctrl Pts',(-4.25060268497819,-2.44016774048634,
375.577331989845));
#41259=CARTESIAN_POINT('Ctrl Pts',(-4.8998218096771,-0.117443592583374,
375.498204114385));
#41260=CARTESIAN_POINT('Ctrl Pts',(-4.36263000323237,2.23371923670199,375.419076238926));
#41261=CARTESIAN_POINT('Ctrl Pts',(-2.76910316484765,4.04402084944263,375.339948363465));
#41262=CARTESIAN_POINT('Ctrl Pts',(-0.505078814327535,4.87513818307261,
375.260820488006));
#41263=CARTESIAN_POINT('Ctrl Pts',(1.88123000134211,4.52580661359865,375.181692612546));
#41264=CARTESIAN_POINT('Ctrl Pts',(3.81205567946445,3.08066074485737,375.102564737086));
#41265=CARTESIAN_POINT('Ctrl Pts',(4.81980261485754,0.889513660705449,375.023436861627));
#41266=CARTESIAN_POINT('Ctrl Pts',(4.6606270588275,-1.51685826939215,374.944308986167));
#41267=CARTESIAN_POINT('Ctrl Pts',(3.37271297305025,-3.55624114494146,374.865181110707));
#41268=CARTESIAN_POINT('Ctrl Pts',(1.96999142168877,-4.34109857602843,374.812429193734));
#41269=CARTESIAN_POINT('Ctrl Pts',(1.21713437249897,-4.54280821229842,374.786053235247));
#41270=CARTESIAN_POINT('Ctrl Pts',(3.71544298812251,3.17665283523749,400.213946764753));
#41271=CARTESIAN_POINT('Ctrl Pts',(4.24189388987153,2.56091091663784,400.187570806266));
#41272=CARTESIAN_POINT('Ctrl Pts',(4.98214581433909,1.06316653552657,400.134818889293));
#41273=CARTESIAN_POINT('Ctrl Pts',(4.88599424296224,-1.44202664096201,400.055691013833));
#41274=CARTESIAN_POINT('Ctrl Pts',(3.60674265589465,-3.5976617763163,399.976563138373));
#41275=CARTESIAN_POINT('Ctrl Pts',(1.45418293597717,-4.88238291434578,399.897435262914));
#41276=CARTESIAN_POINT('Ctrl Pts',(-1.05048684560331,-4.98482476427098,
399.818307387454));
#41277=CARTESIAN_POINT('Ctrl Pts',(-3.30079722370572,-3.88031872051941,
399.739179511994));
#41278=CARTESIAN_POINT('Ctrl Pts',(-4.75187572291575,-1.83623790534267,
399.660051636534));
#41279=CARTESIAN_POINT('Ctrl Pts',(-5.05236683263146,0.652447348843657,
399.580923761074));
#41280=CARTESIAN_POINT('Ctrl Pts',(-4.12951222709533,2.98315803806871,399.501795885615));
#41281=CARTESIAN_POINT('Ctrl Pts',(-2.20676540787796,4.59154485677586,399.422668010155));
#41282=CARTESIAN_POINT('Ctrl Pts',(0.250312604852073,5.08816712539591,399.343540134695));
#41283=CARTESIAN_POINT('Ctrl Pts',(2.64678163724731,4.35277457160906,399.264412259235));
#41284=CARTESIAN_POINT('Ctrl Pts',(4.40237687684668,2.5634308867403,399.185284383776));
#41285=CARTESIAN_POINT('Ctrl Pts',(5.09201039289903,0.153395295488701,399.106156508315));
#41286=CARTESIAN_POINT('Ctrl Pts',(4.54869898923014,-2.29378234250105,399.027028632856));
#41287=CARTESIAN_POINT('Ctrl Pts',(2.90399641321393,-4.1855590799549,398.947900757396));
#41288=CARTESIAN_POINT('Ctrl Pts',(0.556139808676901,-5.06387287138275,
398.868772881936));
#41289=CARTESIAN_POINT('Ctrl Pts',(-1.92637672321179,-4.7160547794503,398.789645006477));
#41290=CARTESIAN_POINT('Ctrl Pts',(-3.94245343924376,-3.22632311381047,
398.710517131017));
#41291=CARTESIAN_POINT('Ctrl Pts',(-5.00393117442772,-0.955391416550765,
398.631389255557));
#41292=CARTESIAN_POINT('Ctrl Pts',(-4.85379089746955,1.54687228977885,398.552261380098));
#41293=CARTESIAN_POINT('Ctrl Pts',(-3.52838655837555,3.67458681370817,398.473133504638));
#41294=CARTESIAN_POINT('Ctrl Pts',(-1.34864258930642,4.91256176790427,398.394005629178));
#41295=CARTESIAN_POINT('Ctrl Pts',(1.15765256446685,4.96104227929438,398.314877753718));
#41296=CARTESIAN_POINT('Ctrl Pts',(3.38364156492812,3.80828960520879,398.235749878258));
#41297=CARTESIAN_POINT('Ctrl Pts',(4.79033850803188,1.73342347263734,398.156622002798));
#41298=CARTESIAN_POINT('Ctrl Pts',(5.03713532094231,-0.761162082306909,
398.077494127339));
#41299=CARTESIAN_POINT('Ctrl Pts',(4.064274294482,-3.07144500459355,397.998366251879));
#41300=CARTESIAN_POINT('Ctrl Pts',(2.10731741020158,-4.63802903070772,397.919238376419));
#41301=CARTESIAN_POINT('Ctrl Pts',(-0.359891042804634,-5.08159211215712,
397.840110500959));
#41302=CARTESIAN_POINT('Ctrl Pts',(-2.73995791558548,-4.29473288783458,
397.7609826255));
#41303=CARTESIAN_POINT('Ctrl Pts',(-4.45658993137603,-2.46797612236942,
397.68185475004));
#41304=CARTESIAN_POINT('Ctrl Pts',(-5.0941334374604,-0.0436403296913884,
397.60272687458));
#41305=CARTESIAN_POINT('Ctrl Pts',(-4.49821796618352,2.39126223692249,397.52359899912));
#41306=CARTESIAN_POINT('Ctrl Pts',(-2.81313445472219,4.24716075710381,397.44447112366));
#41307=CARTESIAN_POINT('Ctrl Pts',(-0.446897614573966,5.07468052975907,
397.365343248201));
#41308=CARTESIAN_POINT('Ctrl Pts',(2.02754798795257,4.67345152040515,397.286215372741));
#41309=CARTESIAN_POINT('Ctrl Pts',(4.01105684952524,3.14062460458175,397.207087497281));
#41310=CARTESIAN_POINT('Ctrl Pts',(5.02335556505595,0.847348112672217,397.127959621822));
#41311=CARTESIAN_POINT('Ctrl Pts',(4.8193329780012,-1.65109951371132,397.048831746361));
#41312=CARTESIAN_POINT('Ctrl Pts',(3.44838973612117,-3.74976108370145,396.969703870902));
#41313=CARTESIAN_POINT('Ctrl Pts',(1.24247675313054,-4.94048089511111,396.890575995442));
#41314=CARTESIAN_POINT('Ctrl Pts',(-1.26428113785597,-4.93494611535824,
396.811448119982));
#41315=CARTESIAN_POINT('Ctrl Pts',(-3.46491455477013,-3.73449689853531,
396.732320244522));
#41316=CARTESIAN_POINT('Ctrl Pts',(-4.82657702287821,-1.62980188957181,
396.653192369063));
#41317=CARTESIAN_POINT('Ctrl Pts',(-5.01956481218505,0.869522313285533,
396.574064493603));
#41318=CARTESIAN_POINT('Ctrl Pts',(-3.99714916613881,3.15830627087741,396.494936618143));
#41319=CARTESIAN_POINT('Ctrl Pts',(-2.00689088633465,4.68235933343167,396.415808742683));
#41320=CARTESIAN_POINT('Ctrl Pts',(0.469302363710116,5.07265761198643,396.336680867223));
#41321=CARTESIAN_POINT('Ctrl Pts',(2.83186191712685,4.23469692414397,396.257552991764));
#41322=CARTESIAN_POINT('Ctrl Pts',(4.50873360091663,2.37137539689376,396.178425116304));
#41323=CARTESIAN_POINT('Ctrl Pts',(5.09389105993074,-0.066134912001412,
396.099297240844));
#41324=CARTESIAN_POINT('Ctrl Pts',(4.44564822923743,-2.48763176111453,396.020169365385));
#41325=CARTESIAN_POINT('Ctrl Pts',(2.72096623850579,-4.30679029974057,395.941041489925));
#41326=CARTESIAN_POINT('Ctrl Pts',(0.337447906876279,-5.08313179714755,
395.861913614465));
#41327=CARTESIAN_POINT('Ctrl Pts',(-2.12777777601096,-4.6286781798848,395.782785739005));
#41328=CARTESIAN_POINT('Ctrl Pts',(-4.07779775573568,-3.05346776965875,
395.703657863545));
#41329=CARTESIAN_POINT('Ctrl Pts',(-5.04044739830187,-0.738911349202079,
395.624529988086));
#41330=CARTESIAN_POINT('Ctrl Pts',(-4.78263723751197,1.75456006206446,395.545402112625));
#41331=CARTESIAN_POINT('Ctrl Pts',(-3.36679168002614,3.82319418030715,395.466274237166));
#41332=CARTESIAN_POINT('Ctrl Pts',(-1.13573398221921,4.9661059471844,395.387146361706));
#41333=CARTESIAN_POINT('Ctrl Pts',(1.37032265180738,4.90655844630137,395.308018486247));
#41334=CARTESIAN_POINT('Ctrl Pts',(3.54457863759732,3.65897010631632,395.228890610786));
#41335=CARTESIAN_POINT('Ctrl Pts',(4.86057435298355,1.52542352025471,395.149762735327));
#41336=CARTESIAN_POINT('Ctrl Pts',(4.99966350625814,-0.977478788116796,
395.070634859867));
#41337=CARTESIAN_POINT('Ctrl Pts',(3.9281679916419,-3.24370100139759,394.991506984407));
#41338=CARTESIAN_POINT('Ctrl Pts',(1.90553247777794,-4.72451541781389,394.912379108947));
#41339=CARTESIAN_POINT('Ctrl Pts',(-0.578495767592555,-5.0613676614039,
394.833251233488));
#41340=CARTESIAN_POINT('Ctrl Pts',(-2.92245096488478,-4.17269461078471,
394.754123358028));
#41341=CARTESIAN_POINT('Ctrl Pts',(-4.55878367391877,-2.27367354108707,
394.674995482568));
#41342=CARTESIAN_POINT('Ctrl Pts',(-5.09128337239731,0.175879444445247,
394.595867607109));
#41343=CARTESIAN_POINT('Ctrl Pts',(-4.39101418897073,2.58284617220721,394.516739731648));
#41344=CARTESIAN_POINT('Ctrl Pts',(-2.62753456208024,4.36442001669197,394.437611856189));
#41345=CARTESIAN_POINT('Ctrl Pts',(-0.227841507780872,5.08922275051504,
394.358483980729));
#41346=CARTESIAN_POINT('Ctrl Pts',(2.22701954646155,4.58175554746277,394.279356105269));
#41347=CARTESIAN_POINT('Ctrl Pts',(4.14264516722633,2.96489307994134,394.200228229809));
#41348=CARTESIAN_POINT('Ctrl Pts',(5.05519873770637,0.630131477804167,394.12110035435));
#41349=CARTESIAN_POINT('Ctrl Pts',(4.74372071539057,-1.85720589364835,394.04197247889));
#41350=CARTESIAN_POINT('Ctrl Pts',(3.28363027953537,-3.89485200544849,393.96284460343));
#41351=CARTESIAN_POINT('Ctrl Pts',(1.02846384177488,-4.98942502530997,393.883716727971));
#41352=CARTESIAN_POINT('Ctrl Pts',(-1.47572786674121,-4.87589245373102,
393.80458885251));
#41353=CARTESIAN_POINT('Ctrl Pts',(-3.62259682199201,-3.58174429884674,
393.725460977051));
#41354=CARTESIAN_POINT('Ctrl Pts',(-4.89231471194326,-1.42033683199839,
393.646333101591));
#41355=CARTESIAN_POINT('Ctrl Pts',(-4.97744064418338,1.0849813780241,393.567205226131));
#41356=CARTESIAN_POINT('Ctrl Pts',(-3.85736280188092,3.32758954375282,393.488077350671));
#41357=CARTESIAN_POINT('Ctrl Pts',(-1.8032892495463,4.76447770899377,393.408949475212));
#41358=CARTESIAN_POINT('Ctrl Pts',(0.687420551315965,5.04772750281314,393.329821599752));
#41359=CARTESIAN_POINT('Ctrl Pts',(3.01168299451616,4.1087547380648,393.250693724292));
#41360=CARTESIAN_POINT('Ctrl Pts',(4.60671691000739,2.1749159220714,393.171565848832));
#41361=CARTESIAN_POINT('Ctrl Pts',(5.08631158572023,-0.285542308591735,
393.092437973373));
#41362=CARTESIAN_POINT('Ctrl Pts',(4.33434121428917,-2.67686125810472,393.013310097913));
#41363=CARTESIAN_POINT('Ctrl Pts',(2.5328828097419,-4.42002314803234,392.934182222453));
#41364=CARTESIAN_POINT('Ctrl Pts',(0.118129312194917,-5.09295056157313,
392.855054346993));
#41365=CARTESIAN_POINT('Ctrl Pts',(-2.32522721713463,-4.53270541131057,
392.775926471534));
#41366=CARTESIAN_POINT('Ctrl Pts',(-4.20556897258945,-2.87494166442045,
392.696798596073));
#41367=CARTESIAN_POINT('Ctrl Pts',(-5.06760273359595,-0.521059009593531,
392.617670720614));
#41368=CARTESIAN_POINT('Ctrl Pts',(-4.70260148223132,1.95898934564318,392.538542845154));
#41369=CARTESIAN_POINT('Ctrl Pts',(-3.19894415001964,3.96470128535339,392.459414969695));
#41370=CARTESIAN_POINT('Ctrl Pts',(-0.920716141880372,5.01042730144931,
392.380287094234));
#41371=CARTESIAN_POINT('Ctrl Pts',(1.58044783853879,4.84296237717018,392.301159218775));
#41372=CARTESIAN_POINT('Ctrl Pts',(3.69893288079714,3.50285533534937,392.222031343315));
#41373=CARTESIAN_POINT('Ctrl Pts',(4.92178336136043,1.31459062101607,392.142903467856));
#41374=CARTESIAN_POINT('Ctrl Pts',(4.9529065449796,-1.19198016498848,392.063775592395));
#41375=CARTESIAN_POINT('Ctrl Pts',(3.78476647471314,-3.40993294492945,391.984647716936));
#41376=CARTESIAN_POINT('Ctrl Pts',(1.70020867751367,-4.80222765078197,391.905519841476));
#41377=CARTESIAN_POINT('Ctrl Pts',(-0.796026136476369,-5.03174346991918,
391.826391966016));
#41378=CARTESIAN_POINT('Ctrl Pts',(-3.09951657179924,-4.04290699598317,
391.747264090556));
#41379=CARTESIAN_POINT('Ctrl Pts',(-4.65251105174488,-2.07514839720426,
391.668136215097));
#41380=CARTESIAN_POINT('Ctrl Pts',(-5.07897800851123,0.395072583314779,
391.589008339637));
#41381=CARTESIAN_POINT('Ctrl Pts',(-4.27565562086226,2.76963336360912,391.509880464177));
#41382=CARTESIAN_POINT('Ctrl Pts',(-2.43705493231998,4.47357387486589,391.430752588717));
#41383=CARTESIAN_POINT('Ctrl Pts',(-0.00836226415120685,5.0943134993408,
391.351624713257));
#41384=CARTESIAN_POINT('Ctrl Pts',(2.42235518603692,4.48155054748998,391.272496837798));
#41385=CARTESIAN_POINT('Ctrl Pts',(4.26653995362923,2.78365529135943,391.193368962338));
#41386=CARTESIAN_POINT('Ctrl Pts',(5.0776536262684,0.411744591550536,391.114241086878));
#41387=CARTESIAN_POINT('Ctrl Pts',(4.65929863144093,-2.05986315566845,391.035113211418));
#41388=CARTESIAN_POINT('Ctrl Pts',(3.11277261484635,-4.03270958603397,390.955985335959));
#41389=CARTESIAN_POINT('Ctrl Pts',(0.812540914369942,-5.02910302335342,
390.876857460499));
#41390=CARTESIAN_POINT('Ctrl Pts',(-1.68443394126863,-4.80778350745226,
390.797729585039));
#41391=CARTESIAN_POINT('Ctrl Pts',(-3.7735513679378,-3.42233984732121,390.718601709579));
#41392=CARTESIAN_POINT('Ctrl Pts',(-4.94896661768926,-1.20823398976565,
390.639473834119));
#41393=CARTESIAN_POINT('Ctrl Pts',(-4.92607260087128,1.29842546492777,390.56034595866));
#41394=CARTESIAN_POINT('Ctrl Pts',(-3.71041271969718,3.49069296938833,390.4812180832));
#41395=CARTESIAN_POINT('Ctrl Pts',(-1.59633862636855,4.83774771427692,390.40209020774));
#41396=CARTESIAN_POINT('Ctrl Pts',(0.904262092886961,5.01342298478748,390.32296233228));
#41397=CARTESIAN_POINT('Ctrl Pts',(3.18591091187283,3.97518196044373,390.243834456821));
#41398=CARTESIAN_POINT('Ctrl Pts',(4.69614483496588,1.97441729278565,390.164706581361));
#41399=CARTESIAN_POINT('Ctrl Pts',(5.06928604606176,-0.504419409054961,
390.085578705901));
#41400=CARTESIAN_POINT('Ctrl Pts',(4.21498465890399,-2.86111941069082,390.006450830441));
#41401=CARTESIAN_POINT('Ctrl Pts',(2.34009542676882,-4.52504733131526,389.927322954981));
#41402=CARTESIAN_POINT('Ctrl Pts',(-0.101408666846889,-5.09331093094817,
389.848195079522));
#41403=CARTESIAN_POINT('Ctrl Pts',(-2.51835835252648,-4.42831470937736,
389.769067204062));
#41404=CARTESIAN_POINT('Ctrl Pts',(-4.3255297989291,-2.6910763488991,389.689939328602));
#41405=CARTESIAN_POINT('Ctrl Pts',(-5.08534674866728,-0.302238983003182,
389.610811453142));
#41406=CARTESIAN_POINT('Ctrl Pts',(-4.61383227037253,2.15978048372904,389.531683577683));
#41407=CARTESIAN_POINT('Ctrl Pts',(-3.02515568711978,4.09884532834732,389.452555702223));
#41408=CARTESIAN_POINT('Ctrl Pts',(-0.703988389596766,5.04544351909133,
389.373427826763));
#41409=CARTESIAN_POINT('Ctrl Pts',(1.78763788976615,4.7703721796208,389.294299951303));
#41410=CARTESIAN_POINT('Ctrl Pts',(3.84641763488075,3.34023522152349,389.215172075843));
#41411=CARTESIAN_POINT('Ctrl Pts',(4.97385185858917,1.10131632414888,389.136044200384));
#41412=CARTESIAN_POINT('Ctrl Pts',(4.89695127199855,-1.40426785076764,389.056916324924));
#41413=CARTESIAN_POINT('Ctrl Pts',(3.63433606243988,-3.56983211681959,388.977788449464));
#41414=CARTESIAN_POINT('Ctrl Pts',(1.4917273273879,-4.87102140600428,388.898660574004));
#41415=CARTESIAN_POINT('Ctrl Pts',(-1.0120781619955,-4.99277455439754,388.819532698545));
#41416=CARTESIAN_POINT('Ctrl Pts',(-3.27082589817505,-3.9056110790573,388.740404823085));
#41417=CARTESIAN_POINT('Ctrl Pts',(-4.73759799865136,-1.87276938254615,
388.661276947625));
#41418=CARTESIAN_POINT('Ctrl Pts',(-5.05724019876165,0.613532011436209,
388.582149072166));
#41419=CARTESIAN_POINT('Ctrl Pts',(-4.15235650051922,2.95127691849197,388.503021196705));
#41420=CARTESIAN_POINT('Ctrl Pts',(-2.24204931550549,4.57441961606814,388.423893321246));
#41421=CARTESIAN_POINT('Ctrl Pts',(0.211132509493252,5.0899433219303,388.344765445786));
#41422=CARTESIAN_POINT('Ctrl Pts',(2.613192138255,4.37302261663371,388.265637570326));
#41423=CARTESIAN_POINT('Ctrl Pts',(4.3825111169981,2.59724782537512,388.186509694867));
#41424=CARTESIAN_POINT('Ctrl Pts',(5.09067852854909,0.192593032057139,388.107381819407));
#41425=CARTESIAN_POINT('Ctrl Pts',(4.56622351098889,-2.25869493396522,388.028253943947));
#41426=CARTESIAN_POINT('Ctrl Pts',(2.93613405110136,-4.16307780265885,387.949126068487));
#41427=CARTESIAN_POINT('Ctrl Pts',(0.595108973109503,-5.05944120107668,
387.869998193027));
#41428=CARTESIAN_POINT('Ctrl Pts',(-1.89001176205386,-4.73074576534459,
387.790870317568));
#41429=CARTESIAN_POINT('Ctrl Pts',(-3.91749784672291,-3.2565795826218,387.711742442108));
#41430=CARTESIAN_POINT('Ctrl Pts',(-4.99642752878567,-0.993887270579772,
387.632614566648));
#41431=CARTESIAN_POINT('Ctrl Pts',(-4.86555608063145,1.50945817539208,387.553486691188));
#41432=CARTESIAN_POINT('Ctrl Pts',(-3.55657182856503,3.6473136395552,387.474358815728));
#41433=CARTESIAN_POINT('Ctrl Pts',(-1.38642335604174,4.90203327557553,387.395230940269));
#41434=CARTESIAN_POINT('Ctrl Pts',(1.11942428022107,4.96980776669272,387.316103064809));
#41435=CARTESIAN_POINT('Ctrl Pts',(3.35422210107046,3.83422665653951,387.236975189349));
#41436=CARTESIAN_POINT('Ctrl Pts',(4.77685129433647,1.77025186592861,387.157847313889));
#41437=CARTESIAN_POINT('Ctrl Pts',(5.04284606000954,-0.72235972484213,387.07871943843));
#41438=CARTESIAN_POINT('Ctrl Pts',(4.08780022662232,-3.04006402305186,386.99959156297));
#41439=CARTESIAN_POINT('Ctrl Pts',(2.14296212550442,-4.62166780347541,386.92046368751));
#41440=CARTESIAN_POINT('Ctrl Pts',(-0.320758314346703,-5.08421223601112,
386.84133581205));
#41441=CARTESIAN_POINT('Ctrl Pts',(-2.70681250786736,-4.31569994372646,
386.76220793659));
#41442=CARTESIAN_POINT('Ctrl Pts',(-4.43745744898977,-2.50221328935662,
386.683080061131));
#41443=CARTESIAN_POINT('Ctrl Pts',(-5.09364649014193,-0.082857651985011,
386.603952185671));
#41444=CARTESIAN_POINT('Ctrl Pts',(-4.51649446005934,2.35656057619595,386.524824310211));
#41445=CARTESIAN_POINT('Ctrl Pts',(-2.84574904331825,4.22537718310224,386.445696434751));
#41446=CARTESIAN_POINT('Ctrl Pts',(-0.485953222246148,5.07108956959117,
386.366568559292));
#41447=CARTESIAN_POINT('Ctrl Pts',(1.99150802159427,4.68892266485099,386.287440683832));
#41448=CARTESIAN_POINT('Ctrl Pts',(3.98675899790251,3.17141177548282,386.208312808372));
#41449=CARTESIAN_POINT('Ctrl Pts',(5.01668314543611,0.885996712931309,386.129184932912));
#41450=CARTESIAN_POINT('Ctrl Pts',(4.83190160489097,-1.61394759446514,386.050057057452));
#41451=CARTESIAN_POINT('Ctrl Pts',(3.47715612730962,-3.72310155963289,385.970929181992));
#41452=CARTESIAN_POINT('Ctrl Pts',(1.28047560943712,-4.93076892286227,385.891801306533));
#41453=CARTESIAN_POINT('Ctrl Pts',(-1.22625060220108,-4.94453328612815,
385.812673431073));
#41454=CARTESIAN_POINT('Ctrl Pts',(-3.43606079615961,-3.76106183970999,
385.733545555613));
#41455=CARTESIAN_POINT('Ctrl Pts',(-4.81388649504862,-1.66691234617067,
385.654417680153));
#41456=CARTESIAN_POINT('Ctrl Pts',(-5.02611031361548,0.830852015942555,
385.575289804694));
#41457=CARTESIAN_POINT('Ctrl Pts',(-4.02134581343353,3.12743949674625,385.496161929234));
#41458=CARTESIAN_POINT('Ctrl Pts',(-2.04287986715703,4.66676995419661,385.417034053774));
#41459=CARTESIAN_POINT('Ctrl Pts',(0.430235177489289,5.07612033437727,385.337906178314));
#41460=CARTESIAN_POINT('Ctrl Pts',(2.79917598944896,4.25637330800767,385.258778302855));
#41461=CARTESIAN_POINT('Ctrl Pts',(4.49034328098805,2.40601686941577,385.179650427394));
#41462=CARTESIAN_POINT('Ctrl Pts',(5.09424925529516,-0.0269162024146704,
385.100522551935));
#41463=CARTESIAN_POINT('Ctrl Pts',(4.46466820889472,-2.45333196724627,385.021394676475));
#41464=CARTESIAN_POINT('Ctrl Pts',(2.75404263336906,-4.28571454142868,384.942266801016));
#41465=CARTESIAN_POINT('Ctrl Pts',(0.376571822658881,-5.08038321580243,
384.863138925555));
#41466=CARTESIAN_POINT('Ctrl Pts',(-2.09207953936242,-4.64492229838228,
384.784011050096));
#41467=CARTESIAN_POINT('Ctrl Pts',(-4.05416892752487,-3.08477134713736,
384.704883174636));
#41468=CARTESIAN_POINT('Ctrl Pts',(-5.03460930299721,-0.777694749372607,
384.625755299176));
#41469=CARTESIAN_POINT('Ctrl Pts',(-4.79600347197984,1.71768758911072,384.546627423717));
#41470=CARTESIAN_POINT('Ctrl Pts',(-3.39612583475742,3.79716068550186,384.467499548257));
#41471=CARTESIAN_POINT('Ctrl Pts',(-1.17393328361345,4.9572150046828,384.388371672797));
#41472=CARTESIAN_POINT('Ctrl Pts',(1.33250752393625,4.91696284871881,384.309243797337));
#41473=CARTESIAN_POINT('Ctrl Pts',(3.51630398225976,3.6861506021013,384.230115921877));
#41474=CARTESIAN_POINT('Ctrl Pts',(4.84868640377085,1.56279880820132,384.150988046418));
#41475=CARTESIAN_POINT('Ctrl Pts',(5.00704073069747,-0.938958507157973,
384.071860170958));
#41476=CARTESIAN_POINT('Ctrl Pts',(3.95302411855986,-3.213362767431,383.992732295498));
#41477=CARTESIAN_POINT('Ctrl Pts',(1.94184901290741,-4.70970512538717,383.913604420038));
#41478=CARTESIAN_POINT('Ctrl Pts',(-0.539512264162803,-5.06567137444245,
383.834476544579));
#41479=CARTESIAN_POINT('Ctrl Pts',(-2.89023969471176,-4.19507025735449,
383.755348669118));
#41480=CARTESIAN_POINT('Ctrl Pts',(-4.54114405585455,-2.30870323363671,
383.676220793659));
#41481=CARTESIAN_POINT('Ctrl Pts',(-5.0924865441193,0.136677558478088,383.597092918199));
#41482=CARTESIAN_POINT('Ctrl Pts',(-4.41076882262505,2.54896417204843,383.51796504274));
#41483=CARTESIAN_POINT('Ctrl Pts',(-2.66105740443557,4.34406186043965,383.43883716728));
#41484=CARTESIAN_POINT('Ctrl Pts',(-0.267015564777766,5.08731782427579,
383.35970929182));
#41485=CARTESIAN_POINT('Ctrl Pts',(2.19167961573057,4.59876509717759,383.28058141636));
#41486=CARTESIAN_POINT('Ctrl Pts',(4.11969633429617,2.99669852841663,383.201453540901));
#41487=CARTESIAN_POINT('Ctrl Pts',(5.05019767759256,0.669031669105843,383.12232566544));
#41488=CARTESIAN_POINT('Ctrl Pts',(4.75787835092606,-1.8206299884427,383.043197789981));
#41489=CARTESIAN_POINT('Ctrl Pts',(3.31351857671521,-3.8694566283641,382.964069914521));
#41490=CARTESIAN_POINT('Ctrl Pts',(1.06684585069835,-4.98135924099793,382.884942039061));
#41491=CARTESIAN_POINT('Ctrl Pts',(-1.43814570582419,-4.88710925658996,
382.805814163602));
#41492=CARTESIAN_POINT('Ctrl Pts',(-3.59491439905111,-3.60952772818311,
382.726686288142));
#41493=CARTESIAN_POINT('Ctrl Pts',(-4.8812348614273,-1.45795959635872,382.647558412682));
#41494=CARTESIAN_POINT('Ctrl Pts',(-4.98564616607288,1.04662900005231,382.568430537222));
#41495=CARTESIAN_POINT('Ctrl Pts',(-3.88286686666645,3.29779393728166,382.489302661762));
#41496=CARTESIAN_POINT('Ctrl Pts',(-1.83991647567274,4.75045338042336,382.410174786303));
#41497=CARTESIAN_POINT('Ctrl Pts',(0.648538832374088,5.05287020810257,382.331046910843));
#41498=CARTESIAN_POINT('Ctrl Pts',(2.97996133890915,4.13181925737738,382.251919035383));
#41499=CARTESIAN_POINT('Ctrl Pts',(4.58983618463159,2.21031756887428,382.172791159923));
#41500=CARTESIAN_POINT('Ctrl Pts',(5.08835917511605,-0.246375449345246,
382.093663284464));
#41501=CARTESIAN_POINT('Ctrl Pts',(4.35482132902486,-2.64341278450753,382.014535409004));
#41502=CARTESIAN_POINT('Ctrl Pts',(2.56683653350947,-4.40039204699635,381.935407533544));
#41503=CARTESIAN_POINT('Ctrl Pts',(0.157335320227334,-5.09189017497793,
381.856279658084));
#41504=CARTESIAN_POINT('Ctrl Pts',(-2.29026200215225,-4.55047249398623,
381.777151782624));
#41505=CARTESIAN_POINT('Ctrl Pts',(-4.1833107910579,-2.90723421527166,381.698023907165));
#41506=CARTESIAN_POINT('Ctrl Pts',(-5.06344103087761,-0.560057929015174,
381.618896031705));
#41507=CARTESIAN_POINT('Ctrl Pts',(-4.71754394484289,1.92272699193202,381.539768156245));
#41508=CARTESIAN_POINT('Ctrl Pts',(-3.22937271124211,3.9399558181422,381.460640280785));
#41509=CARTESIAN_POINT('Ctrl Pts',(-0.959263035935946,5.0031904206131,381.381512405325));
#41510=CARTESIAN_POINT('Ctrl Pts',(1.54311609556955,4.85498637203256,381.302384529866));
#41511=CARTESIAN_POINT('Ctrl Pts',(3.67185554437766,3.53122879721078,381.223256654406));
#41512=CARTESIAN_POINT('Ctrl Pts',(4.91151675438643,1.35244339194259,381.144128778947));
#41513=CARTESIAN_POINT('Ctrl Pts',(4.96193655414693,-1.15381349864191,381.065000903486));
#41514=CARTESIAN_POINT('Ctrl Pts',(3.81090663474561,-3.38069380131942,380.985873028027));
#41515=CARTESIAN_POINT('Ctrl Pts',(1.73712958706021,-4.78899579815935,380.906745152567));
#41516=CARTESIAN_POINT('Ctrl Pts',(-0.757264256456047,-5.03772277948299,
380.827617277107));
#41517=CARTESIAN_POINT('Ctrl Pts',(-3.06829926047039,-4.0666496782025,380.748489401647));
#41518=CARTESIAN_POINT('Ctrl Pts',(-4.63639705749532,-2.11090555977201,
380.669361526187));
#41519=CARTESIAN_POINT('Ctrl Pts',(-5.08186906479814,0.355958937625331,
380.590233650728));
#41520=CARTESIAN_POINT('Ctrl Pts',(-4.29685170689215,2.73663394812055,380.511105775268));
#41521=CARTESIAN_POINT('Ctrl Pts',(-2.47142377134362,4.45467894460033,380.431977899808));
#41522=CARTESIAN_POINT('Ctrl Pts',(-0.0475820182042561,5.09409814477217,
380.352850024348));
#41523=CARTESIAN_POINT('Ctrl Pts',(2.38778092263769,4.50006691311533,380.273722148889));
#41524=CARTESIAN_POINT('Ctrl Pts',(4.24498275891546,2.81641994978345,380.194594273428));
#41525=CARTESIAN_POINT('Ctrl Pts',(5.07433321340091,0.450824130237162,380.115466397969));
#41526=CARTESIAN_POINT('Ctrl Pts',(4.67501898270842,-2.02393119160303,380.036338522509));
#41527=CARTESIAN_POINT('Ctrl Pts',(3.14372731083789,-4.00862551906755,379.957210647049));
#41528=CARTESIAN_POINT('Ctrl Pts',(0.851234794597309,-5.02269840638422,
379.87808277159));
#41529=CARTESIAN_POINT('Ctrl Pts',(-1.64736995096127,-4.82060911106652,
379.79895489613));
#41530=CARTESIAN_POINT('Ctrl Pts',(-3.74709169119734,-3.45129016670399,
379.71982702067));
#41531=CARTESIAN_POINT('Ctrl Pts',(-4.93951802147898,-1.2462991906088,379.64069914521));
#41532=CARTESIAN_POINT('Ctrl Pts',(-4.93592290429957,1.26046223261093,379.56157126975));
#41533=CARTESIAN_POINT('Ctrl Pts',(-3.73717683698987,3.46202386561592,379.482443394291));
#41534=CARTESIAN_POINT('Ctrl Pts',(-1.63353607538846,4.82531448171332,379.403315518831));
#41535=CARTESIAN_POINT('Ctrl Pts',(0.865638050575662,5.02023612217824,379.324187643371));
#41536=CARTESIAN_POINT('Ctrl Pts',(3.15521244034589,3.99959178083392,379.245059767911));
#41537=CARTESIAN_POINT('Ctrl Pts',(4.6808050542546,2.01051336754875,379.165931892452));
#41538=CARTESIAN_POINT('Ctrl Pts',(5.07301922679952,-0.465377139049836,
379.086804016992));
#41539=CARTESIAN_POINT('Ctrl Pts',(4.23688687398491,-2.82858437634132,379.007676141532));
#41540=CARTESIAN_POINT('Ctrl Pts',(2.37486342213654,-4.5068973455389,378.928548266072));
#41541=CARTESIAN_POINT('Ctrl Pts',(-0.0621933781710937,-5.0939407084044,
378.849420390613));
#41542=CARTESIAN_POINT('Ctrl Pts',(-2.48419109500962,-4.44757176001722,
378.770292515152));
#41543=CARTESIAN_POINT('Ctrl Pts',(-4.30468360095437,-2.72429790087321,
378.691164639693));
#41544=CARTESIAN_POINT('Ctrl Pts',(-5.08286916745938,-0.341380994664952,
378.612036764233));
#41545=CARTESIAN_POINT('Ctrl Pts',(-4.63032321066906,2.12419559404662,378.532908888774));
#41546=CARTESIAN_POINT('Ctrl Pts',(-3.05662214430013,4.07543384488105,378.453781013314));
#41547=CARTESIAN_POINT('Ctrl Pts',(-0.742811288783636,5.03987413992486,
378.374653137854));
#41548=CARTESIAN_POINT('Ctrl Pts',(1.75085886250587,4.78399343651434,378.295525262394));
#41549=CARTESIAN_POINT('Ctrl Pts',(3.82058790417125,3.36974895556452,378.216397386935));
#41550=CARTESIAN_POINT('Ctrl Pts',(4.9652256605272,1.13957627961887,378.137269511474));
#41551=CARTESIAN_POINT('Ctrl Pts',(4.90761729577347,-1.36652568042196,378.058141636015));
#41552=CARTESIAN_POINT('Ctrl Pts',(3.66171170927622,-3.54174636516749,377.979013760555));
#41553=CARTESIAN_POINT('Ctrl Pts',(1.52918404352555,-4.85939256677772,377.899885885095));
#41554=CARTESIAN_POINT('Ctrl Pts',(-0.973609892176757,-5.00041835598616,
377.820758009635));
#41555=CARTESIAN_POINT('Ctrl Pts',(-3.24066052105438,-3.93067670310182,
377.741630134176));
#41556=CARTESIAN_POINT('Ctrl Pts',(-4.72303955439021,-1.90918760856372,
377.662502258716));
#41557=CARTESIAN_POINT('Ctrl Pts',(-5.06181377047586,0.574579246099912,
377.583374383256));
#41558=CARTESIAN_POINT('Ctrl Pts',(-4.17495467452228,2.91922137268011,377.504246507796));
#41559=CARTESIAN_POINT('Ctrl Pts',(-2.27720032296007,4.55702300259043,377.425118632336));
#41560=CARTESIAN_POINT('Ctrl Pts',(0.171939895519064,5.09141793897891,377.345990756877));
#41561=CARTESIAN_POINT('Ctrl Pts',(2.5794477519296,4.39301141042152,377.266862881417));
#41562=CARTESIAN_POINT('Ctrl Pts',(4.36238559553759,2.63091084472138,377.187735005957));
#41563=CARTESIAN_POINT('Ctrl Pts',(5.08904492944719,0.231779341395482,377.108607130498));
#41564=CARTESIAN_POINT('Ctrl Pts',(4.58347738286989,-2.22347364224237,377.029479255037));
#41565=CARTESIAN_POINT('Ctrl Pts',(2.96809765825856,-4.14034977363789,376.950351379578));
#41566=CARTESIAN_POINT('Ctrl Pts',(0.634042864132613,-5.0547096458148,376.871223504118));
#41567=CARTESIAN_POINT('Ctrl Pts',(-1.85353477590152,-4.7451563505839,376.792095628658));
#41568=CARTESIAN_POINT('Ctrl Pts',(-3.89231005589385,-3.28664302685179,
376.712967753199));
#41569=CARTESIAN_POINT('Ctrl Pts',(-4.98862773436458,-1.03232421493045,
376.633839877739));
#41570=CARTESIAN_POINT('Ctrl Pts',(-4.87703287210239,1.47195459226046,376.554712002279));
#41571=CARTESIAN_POINT('Ctrl Pts',(-3.58454629319045,3.61982428153675,376.475584126819));
#41572=CARTESIAN_POINT('Ctrl Pts',(-1.42412194671949,4.89121422922617,376.39645625136));
#41573=CARTESIAN_POINT('Ctrl Pts',(1.08112964569973,4.97827868361118,376.3173283759));
#41574=CARTESIAN_POINT('Ctrl Pts',(3.32460382467506,3.85993644420179,376.23820050044));
#41575=CARTESIAN_POINT('Ctrl Pts',(4.76308094821025,1.80697533479263,376.15907262498));
#41576=CARTESIAN_POINT('Ctrl Pts',(5.04825789565173,-0.683514556087066,
376.07994474952));
#41577=CARTESIAN_POINT('Ctrl Pts',(4.11108387333318,-3.00850284103068,376.000816874061));
#41578=CARTESIAN_POINT('Ctrl Pts',(2.1784798079633,-4.60503266038196,375.921688998601));
#41579=CARTESIAN_POINT('Ctrl Pts',(-0.281606542178375,-5.08653096539461,
375.842561123141));
#41580=CARTESIAN_POINT('Ctrl Pts',(-2.67350672874489,-4.33641128901115,
375.763433247681));
#41581=CARTESIAN_POINT('Ctrl Pts',(-4.41806180727835,-2.5363019544723,375.684305372222));
#41582=CARTESIAN_POINT('Ctrl Pts',(-5.09285793196053,-0.12207046608611,
375.605177496761));
#41583=CARTESIAN_POINT('Ctrl Pts',(-4.53450261646048,2.32172008989041,375.526049621302));
#41584=CARTESIAN_POINT('Ctrl Pts',(-2.8781963029061,4.20334135813296,375.446921745842));
#41585=CARTESIAN_POINT('Ctrl Pts',(-0.524977181972811,5.06720185538771,
375.367793870382));
#41586=CARTESIAN_POINT('Ctrl Pts',(1.95534399133764,4.70410782389334,375.288665994923));
#41587=CARTESIAN_POINT('Ctrl Pts',(3.96223755849503,3.20202817970643,375.209538119463));
#41588=CARTESIAN_POINT('Ctrl Pts',(5.00968625615773,0.924557438714191,375.130410244003));
#41589=CARTESIAN_POINT('Ctrl Pts',(4.84423973083701,-1.5766172667089,375.051282368543));
#41590=CARTESIAN_POINT('Ctrl Pts',(3.50558626093324,-3.69634481139898,374.972154493084));
#41591=CARTESIAN_POINT('Ctrl Pts',(2.04760230627713,-4.51212292509998,374.91940257611));
#41592=CARTESIAN_POINT('Ctrl Pts',(1.26508527942809,-4.72177922709072,374.893026617624));
#41593=CARTESIAN_POINT('Ctrl Pts',(3.8562705385027,3.2970584607914,400.320920147129));
#41594=CARTESIAN_POINT('Ctrl Pts',(4.40267566673985,2.65797789150057,400.294544188642));
#41595=CARTESIAN_POINT('Ctrl Pts',(5.17098558200965,1.10346405572081,400.241792271669));
#41596=CARTESIAN_POINT('Ctrl Pts',(5.07118954877308,-1.49668420940778,400.162664396209));
#41597=CARTESIAN_POINT('Ctrl Pts',(3.74345010496737,-3.73402503008569,400.08353652075));
#41598=CARTESIAN_POINT('Ctrl Pts',(1.50930126812034,-5.0674413388845,400.00440864529));
#41599=CARTESIAN_POINT('Ctrl Pts',(-1.09030376370591,-5.17376607298461,
399.925280769831));
#41600=CARTESIAN_POINT('Ctrl Pts',(-3.42590833126468,-4.02739560525483,
399.84615289437));
#41601=CARTESIAN_POINT('Ctrl Pts',(-4.93198749421962,-1.90583738162352,
399.767025018911));
#41602=CARTESIAN_POINT('Ctrl Pts',(-5.24386820862784,0.677177256470671,
399.68789714345));
#41603=CARTESIAN_POINT('Ctrl Pts',(-4.28603436807985,3.09622957226831,399.608769267991));
#41604=CARTESIAN_POINT('Ctrl Pts',(-2.29040909926245,4.7655795591539,399.529641392531));
#41605=CARTESIAN_POINT('Ctrl Pts',(0.259800278618912,5.28102545063066,399.450513517072));
#41606=CARTESIAN_POINT('Ctrl Pts',(2.7471033957984,4.51775909222651,399.371385641611));
#41607=CARTESIAN_POINT('Ctrl Pts',(4.56924148852249,2.66059337678593,399.292257766152));
#41608=CARTESIAN_POINT('Ctrl Pts',(5.2850143906551,0.159209483399153,399.213129890692));
#41609=CARTESIAN_POINT('Ctrl Pts',(4.7211096918349,-2.38072426286758,399.134002015232));
#41610=CARTESIAN_POINT('Ctrl Pts',(3.01406746059458,-4.34420558161996,399.054874139772));
#41611=CARTESIAN_POINT('Ctrl Pts',(0.577219342712345,-5.25581036421826,
398.975746264313));
#41612=CARTESIAN_POINT('Ctrl Pts',(-1.99939275815206,-4.89480881878609,
398.896618388853));
#41613=CARTESIAN_POINT('Ctrl Pts',(-4.09188543486623,-3.34861140683646,
398.817490513394));
#41614=CARTESIAN_POINT('Ctrl Pts',(-5.19359667913832,-0.991603904073038,
398.738362637933));
#41615=CARTESIAN_POINT('Ctrl Pts',(-5.03776559021372,1.60550385431017,398.659234762474));
#41616=CARTESIAN_POINT('Ctrl Pts',(-3.66212405277363,3.81386578025083,398.580106887014));
#41617=CARTESIAN_POINT('Ctrl Pts',(-1.39976059402284,5.09876407058445,398.500979011554));
#41618=CARTESIAN_POINT('Ctrl Pts',(1.2015314169661,5.14908215334412,398.421851136094));
#41619=CARTESIAN_POINT('Ctrl Pts',(3.51189274640949,3.9526363487746,398.342723260634));
#41620=CARTESIAN_POINT('Ctrl Pts',(4.97190814582059,1.79912594262636,398.263595385175));
#41621=CARTESIAN_POINT('Ctrl Pts',(5.22805937238099,-0.790012637095727,
398.184467509715));
#41622=CARTESIAN_POINT('Ctrl Pts',(4.21832370253235,-3.18786290617544,398.105339634255));
#41623=CARTESIAN_POINT('Ctrl Pts',(2.18719169429123,-4.81382563667766,398.026211758795));
#41624=CARTESIAN_POINT('Ctrl Pts',(-0.37353210098369,-5.27420122269227,
397.947083883336));
#41625=CARTESIAN_POINT('Ctrl Pts',(-2.84381136257153,-4.45751743709679,
397.867956007876));
#41626=CARTESIAN_POINT('Ctrl Pts',(-4.62550939672404,-2.56152056184034,
397.788828132416));
#41627=CARTESIAN_POINT('Ctrl Pts',(-5.2872179056115,-0.0452944422017613,
397.709700256956));
#41628=CARTESIAN_POINT('Ctrl Pts',(-4.66871527142514,2.48189896697567,397.630572381496));
#41629=CARTESIAN_POINT('Ctrl Pts',(-2.91976153402742,4.40814216562114,397.551444506037));
#41630=CARTESIAN_POINT('Ctrl Pts',(-0.463836508948714,5.26702766851281,
397.472316630577));
#41631=CARTESIAN_POINT('Ctrl Pts',(2.10439874769627,4.85059075563045,397.393188755117));
#41632=CARTESIAN_POINT('Ctrl Pts',(4.16308914079174,3.25966464129901,397.314060879657));
#41633=CARTESIAN_POINT('Ctrl Pts',(5.21375731827273,0.87946540242969,397.234933004198));
#41634=CARTESIAN_POINT('Ctrl Pts',(5.00200160188481,-1.71368163398425,397.155805128738));
#41635=CARTESIAN_POINT('Ctrl Pts',(3.57909508696266,-3.89188940315535,397.076677253278));
#41636=CARTESIAN_POINT('Ctrl Pts',(1.28957072230382,-5.12774142484681,396.997549377819));
#41637=CARTESIAN_POINT('Ctrl Pts',(-1.31220156516579,-5.12199685867627,
396.918421502358));
#41638=CARTESIAN_POINT('Ctrl Pts',(-3.59624625077107,-3.87604665499891,
396.839293626899));
#41639=CARTESIAN_POINT('Ctrl Pts',(-5.00952021996834,-1.69157675960673,
396.760165751439));
#41640=CARTESIAN_POINT('Ctrl Pts',(-5.20982288335836,0.90248007842212,396.681037875979));
#41641=CARTESIAN_POINT('Ctrl Pts',(-4.14865431030898,3.27801650109757,396.601910000519));
#41642=CARTESIAN_POINT('Ctrl Pts',(-2.08295867375766,4.85983620416686,396.52278212506));
#41643=CARTESIAN_POINT('Ctrl Pts',(0.487090472013812,5.26492807548086,396.4436542496));
#41644=CARTESIAN_POINT('Ctrl Pts',(2.93919882905869,4.3952059122609,396.36452637414));
#41645=CARTESIAN_POINT('Ctrl Pts',(4.67962948341671,2.46125835008237,396.28539849868));
#41646=CARTESIAN_POINT('Ctrl Pts',(5.2869663411736,-0.0686416434144708,
396.206270623221));
#41647=CARTESIAN_POINT('Ctrl Pts',(4.61415296796628,-2.58192121415839,396.127142747761));
#41648=CARTESIAN_POINT('Ctrl Pts',(2.82409983825713,-4.47003186470401,396.048014872301));
#41649=CARTESIAN_POINT('Ctrl Pts',(0.350238296140284,-5.27579926682488,
395.968886996841));
#41650=CARTESIAN_POINT('Ctrl Pts',(-2.20842757548492,-4.80412035775031,
395.889759121382));
#41651=CARTESIAN_POINT('Ctrl Pts',(-4.23235974759556,-3.16920427471092,
395.810631245921));
#41652=CARTESIAN_POINT('Ctrl Pts',(-5.23149698840249,-0.766918527777797,
395.731503370462));
#41653=CARTESIAN_POINT('Ctrl Pts',(-4.96391497173342,1.82106367854447,395.652375495002));
#41654=CARTESIAN_POINT('Ctrl Pts',(-3.49440419526435,3.96810585645496,395.573247619542));
#41655=CARTESIAN_POINT('Ctrl Pts',(-1.17878204811896,5.1543377509575,395.494119744082));
#41656=CARTESIAN_POINT('Ctrl Pts',(1.42226240243777,5.09253320328156,395.414991868623));
#41657=CARTESIAN_POINT('Ctrl Pts',(3.67892986523249,3.79765714811298,395.335863993163));
#41658=CARTESIAN_POINT('Ctrl Pts',(5.0448061610774,1.58324210563915,395.256736117703));
#41659=CARTESIAN_POINT('Ctrl Pts',(5.18916725226161,-1.01452845991075,395.177608242243));
#41660=CARTESIAN_POINT('Ctrl Pts',(4.07705852165763,-3.36664797371096,395.098480366784));
#41661=CARTESIAN_POINT('Ctrl Pts',(1.97775844702931,-4.90359014326416,395.019352491324));
#41662=CARTESIAN_POINT('Ctrl Pts',(-0.60042266624658,-5.25321019851391,
394.940224615864));
#41663=CARTESIAN_POINT('Ctrl Pts',(-3.03322150067462,-4.33085350661488,
394.861096740404));
#41664=CARTESIAN_POINT('Ctrl Pts',(-4.73157661935314,-2.35985327152006,
394.781968864945));
#41665=CARTESIAN_POINT('Ctrl Pts',(-5.28425981367717,0.182545855799866,
394.702840989484));
#41666=CARTESIAN_POINT('Ctrl Pts',(-4.55744811727866,2.68074456564335,394.623713114025));
#41667=CARTESIAN_POINT('Ctrl Pts',(-2.72712679296628,4.52984593810856,394.544585238565));
#41668=CARTESIAN_POINT('Ctrl Pts',(-0.236477452813074,5.28212108742541,
394.465457363106));
#41669=CARTESIAN_POINT('Ctrl Pts',(2.31143093653793,4.75541920271268,394.386329487645));
#41670=CARTESIAN_POINT('Ctrl Pts',(4.29966508998112,3.07727231195273,394.307201612186));
#41671=CARTESIAN_POINT('Ctrl Pts',(5.2468074522505,0.654015540275394,394.228073736726));
#41672=CARTESIAN_POINT('Ctrl Pts',(4.92352338499734,-1.92760012588128,394.148945861266));
#41673=CARTESIAN_POINT('Ctrl Pts',(3.40809070325859,-4.04247974964323,394.069817985806));
#41674=CARTESIAN_POINT('Ctrl Pts',(1.06744601535546,-5.17854069909805,393.990690110347));
#41675=CARTESIAN_POINT('Ctrl Pts',(-1.53166282285958,-5.06070486839363,
393.911562234887));
#41676=CARTESIAN_POINT('Ctrl Pts',(-3.75990519627929,-3.71750422769163,
393.832434359427));
#41677=CARTESIAN_POINT('Ctrl Pts',(-5.07774958438631,-1.47417228510708,
393.753306483967));
#41678=CARTESIAN_POINT('Ctrl Pts',(-5.16610207037776,1.12610575273896,393.674178608508));
#41679=CARTESIAN_POINT('Ctrl Pts',(-4.00356958154437,3.45371616865744,393.595050733048));
#41680=CARTESIAN_POINT('Ctrl Pts',(-1.8716398630404,4.94506713715712,393.515922857588));
#41681=CARTESIAN_POINT('Ctrl Pts',(0.713476058729831,5.23905303289941,393.436794982128));
#41682=CARTESIAN_POINT('Ctrl Pts',(3.12583571869877,4.26449010171441,393.357667106669));
#41683=CARTESIAN_POINT('Ctrl Pts',(4.78132668327137,2.25735241283907,393.278539231209));
#41684=CARTESIAN_POINT('Ctrl Pts',(5.2790995798779,-0.296365304389928,393.199411355749));
#41685=CARTESIAN_POINT('Ctrl Pts',(4.49862704983328,-2.77832313355043,393.120283480289));
#41686=CARTESIAN_POINT('Ctrl Pts',(2.62888742685924,-4.58755661161959,393.041155604829));
#41687=CARTESIAN_POINT('Ctrl Pts',(0.122606802959192,-5.28599019482455,
392.96202772937));
#41688=CARTESIAN_POINT('Ctrl Pts',(-2.41336100201929,-4.70450990453263,
392.88289985391));
#41689=CARTESIAN_POINT('Ctrl Pts',(-4.3649739152189,-2.98391144093985,392.80377197845));
#41690=CARTESIAN_POINT('Ctrl Pts',(-5.25968160051806,-0.540808865575483,
392.724644102991));
#41691=CARTESIAN_POINT('Ctrl Pts',(-4.88084559720602,2.03324150659673,392.64551622753));
#41692=CARTESIAN_POINT('Ctrl Pts',(-3.32019468996614,4.11497654776232,392.566388352071));
#41693=CARTESIAN_POINT('Ctrl Pts',(-0.955614322062658,5.20033903081154,
392.487260476611));
#41694=CARTESIAN_POINT('Ctrl Pts',(1.64035202716895,5.02652663326038,392.408132601151));
#41695=CARTESIAN_POINT('Ctrl Pts',(3.83913464362559,3.63562511214056,392.329004725691));
#41696=CARTESIAN_POINT('Ctrl Pts',(5.10833519286426,1.36441794376124,392.249876850232));
#41697=CARTESIAN_POINT('Ctrl Pts',(5.14063804785052,-1.23716014683014,392.170748974772));
#41698=CARTESIAN_POINT('Ctrl Pts',(3.92822161400576,-3.53918065647562,392.091621099312));
#41699=CARTESIAN_POINT('Ctrl Pts',(1.76465219715718,-4.98424792631562,392.012493223852));
#41700=CARTESIAN_POINT('Ctrl Pts',(-0.826198153971171,-5.22246315241074,
391.933365348392));
#41701=CARTESIAN_POINT('Ctrl Pts',(-3.21699847841567,-4.19614651290735,
391.854237472933));
#41702=CARTESIAN_POINT('Ctrl Pts',(-4.82885657410346,-2.15380336954211,
391.775109597473));
#41703=CARTESIAN_POINT('Ctrl Pts',(-5.27148803589155,0.41004713797985,391.695981722013));
#41704=CARTESIAN_POINT('Ctrl Pts',(-4.43771707875037,2.8746116080056,391.616853846554));
#41705=CARTESIAN_POINT('Ctrl Pts',(-2.52942735664669,4.64313708771996,391.537725971094));
#41706=CARTESIAN_POINT('Ctrl Pts',(-0.00867922155838994,5.28740479243137,
391.458598095634));
#41707=CARTESIAN_POINT('Ctrl Pts',(2.51417044146968,4.65141610255989,391.379470220174));
#41708=CARTESIAN_POINT('Ctrl Pts',(4.42825589764708,2.88916501309064,391.300342344714));
#41709=CARTESIAN_POINT('Ctrl Pts',(5.27011345519119,0.427351070346123,391.221214469255));
#41710=CARTESIAN_POINT('Ctrl Pts',(4.8359014254693,-2.1379387669101,391.142086593795));
#41711=CARTESIAN_POINT('Ctrl Pts',(3.23075696923981,-4.18556258746916,391.062958718335));
#41712=CARTESIAN_POINT('Ctrl Pts',(0.843338896446427,-5.21972262420654,
390.983830842875));
#41713=CARTESIAN_POINT('Ctrl Pts',(-1.7482795463511,-4.99001436828829,390.904702967415));
#41714=CARTESIAN_POINT('Ctrl Pts',(-3.91658141767327,-3.55205782141137,
390.825575091956));
#41715=CARTESIAN_POINT('Ctrl Pts',(-5.13654878431394,-1.25403004520473,
390.746447216496));
#41716=CARTESIAN_POINT('Ctrl Pts',(-5.11278700870727,1.34764007491144,390.667319341036));
#41717=CARTESIAN_POINT('Ctrl Pts',(-3.85104960630393,3.62300175237324,390.588191465576));
#41718=CARTESIAN_POINT('Ctrl Pts',(-1.65684512829777,5.02111431743484,390.509063590116));
#41719=CARTESIAN_POINT('Ctrl Pts',(0.938536610313288,5.20344826043412,390.429935714657));
#41720=CARTESIAN_POINT('Ctrl Pts',(3.30666744908329,4.12585447502528,390.350807839197));
#41721=CARTESIAN_POINT('Ctrl Pts',(4.874144221702,2.04925422384882,390.271679963737));
#41722=CARTESIAN_POINT('Ctrl Pts',(5.26142871608132,-0.523538569265068,
390.192552088277));
#41723=CARTESIAN_POINT('Ctrl Pts',(4.37474648711696,-2.96956527817979,390.113424212818));
#41724=CARTESIAN_POINT('Ctrl Pts',(2.42879276586438,-4.69656155803349,390.034296337358));
#41725=CARTESIAN_POINT('Ctrl Pts',(-0.105252389973582,-5.28636422338813,
389.955168461898));
#41726=CARTESIAN_POINT('Ctrl Pts',(-2.61381244478399,-4.59616245050211,
389.876040586438));
#41727=CARTESIAN_POINT('Ctrl Pts',(-4.48948165275299,-2.79307702319636,
389.796912710979));
#41728=CARTESIAN_POINT('Ctrl Pts',(-5.27809817231664,-0.313694837861352,
389.717784835519));
#41729=CARTESIAN_POINT('Ctrl Pts',(-4.78871173927535,2.2416432914359,389.638656960059));
#41730=CARTESIAN_POINT('Ctrl Pts',(-3.13981907081257,4.25420509266713,389.559529084599));
#41731=CARTESIAN_POINT('Ctrl Pts',(-0.730671872756092,5.23668247865729,
389.48040120914));
#41732=CARTESIAN_POINT('Ctrl Pts',(1.85539526507438,4.95118502767294,389.401273333679));
#41733=CARTESIAN_POINT('Ctrl Pts',(3.99220955659535,3.46684115934693,389.32214545822));
#41734=CARTESIAN_POINT('Ctrl Pts',(5.16237725796638,1.14305984722794,389.24301758276));
#41735=CARTESIAN_POINT('Ctrl Pts',(5.08256188536855,-1.45749423645932,389.1638897073));
#41736=CARTESIAN_POINT('Ctrl Pts',(3.77208939268016,-3.70514053465492,389.08476183184));
#41737=CARTESIAN_POINT('Ctrl Pts',(1.54826871586373,-5.05564919188336,389.005633956381));
#41738=CARTESIAN_POINT('Ctrl Pts',(-1.05043926423896,-5.18201718639165,
388.926506080921));
#41739=CARTESIAN_POINT('Ctrl Pts',(-3.39480099358967,-4.05364662764723,
388.847378205461));
#41740=CARTESIAN_POINT('Ctrl Pts',(-4.91716859708847,-1.94375352236854,
388.768250330001));
#41741=CARTESIAN_POINT('Ctrl Pts',(-5.2489262914167,0.636786899353102,388.689122454542));
#41742=CARTESIAN_POINT('Ctrl Pts',(-4.30974451485365,3.06314005305047,388.609994579082));
#41743=CARTESIAN_POINT('Ctrl Pts',(-2.32703038342756,4.74780521530929,388.530866703622));
#41744=CARTESIAN_POINT('Ctrl Pts',(0.2191351283499,5.28286897087523,388.451738828163));
#41745=CARTESIAN_POINT('Ctrl Pts',(2.71224074394742,4.53877460497707,388.372610952702));
#41746=CARTESIAN_POINT('Ctrl Pts',(4.54862275081774,2.69569208899244,388.293483077243));
#41747=CARTESIAN_POINT('Ctrl Pts',(5.28363204425109,0.199892943537846,388.214355201783));
#41748=CARTESIAN_POINT('Ctrl Pts',(4.73929845080001,-2.34430692575821,388.135227326323));
#41749=CARTESIAN_POINT('Ctrl Pts',(3.04742322101362,-4.32087218972514,388.056099450863));
#41750=CARTESIAN_POINT('Ctrl Pts',(0.617665567076949,-5.25121071898288,
387.976971575404));
#41751=CARTESIAN_POINT('Ctrl Pts',(-1.96164944496022,-4.9100566415267,387.897843699944));
#41752=CARTESIAN_POINT('Ctrl Pts',(-4.06598394303424,-3.38001469566346,
387.818715824484));
#41753=CARTESIAN_POINT('Ctrl Pts',(-5.18580862056406,-1.03155887800781,
387.739587949024));
#41754=CARTESIAN_POINT('Ctrl Pts',(-5.04997671264308,1.56667162151986,387.660460073564));
#41755=CARTESIAN_POINT('Ctrl Pts',(-3.69137763771595,3.78555886279474,387.581332198105));
#41756=CARTESIAN_POINT('Ctrl Pts',(-1.43897337649567,5.08783651365194,387.502204322645));
#41757=CARTESIAN_POINT('Ctrl Pts',(1.16185415459233,5.15817988164137,387.423076447186));
#41758=CARTESIAN_POINT('Ctrl Pts',(3.48135818778607,3.97955649994419,387.343948571725));
#41759=CARTESIAN_POINT('Ctrl Pts',(4.95790972221771,1.83735025355874,387.264820696266));
#41760=CARTESIAN_POINT('Ctrl Pts',(5.23398656730458,-0.749739542233496,
387.185692820806));
#41761=CARTESIAN_POINT('Ctrl Pts',(4.24274134513742,-3.15529248187465,387.106564945346));
#41762=CARTESIAN_POINT('Ctrl Pts',(2.22418746193322,-4.79684426494046,387.027437069886));
#41763=CARTESIAN_POINT('Ctrl Pts',(-0.332916112977428,-5.27692065788687,
386.948309194427));
#41764=CARTESIAN_POINT('Ctrl Pts',(-2.80940963451955,-4.47927921359921,
386.869181318967));
#41765=CARTESIAN_POINT('Ctrl Pts',(-4.6056517301173,-2.59705543044056,386.790053443507));
#41766=CARTESIAN_POINT('Ctrl Pts',(-5.2867125013827,-0.0859982304292488,
386.710925568047));
#41767=CARTESIAN_POINT('Ctrl Pts',(-4.68768450473212,2.44588199879054,386.631797692588));
#41768=CARTESIAN_POINT('Ctrl Pts',(-2.95361232316089,4.38553292227813,386.552669817127));
#41769=CARTESIAN_POINT('Ctrl Pts',(-0.504372453036948,5.26330059910421,
386.473541941668));
#41770=CARTESIAN_POINT('Ctrl Pts',(2.06699274767947,4.86664830750627,386.394414066208));
#41771=CARTESIAN_POINT('Ctrl Pts',(4.1378703204085,3.29161874757629,386.315286190749));
#41772=CARTESIAN_POINT('Ctrl Pts',(5.20683199193,0.919578912180737,386.236158315288));
#41773=CARTESIAN_POINT('Ctrl Pts',(5.01504662121074,-1.67512153439562,386.157030439829));
#41774=CARTESIAN_POINT('Ctrl Pts',(3.60895181930755,-3.86421939514695,386.077902564369));
#41775=CARTESIAN_POINT('Ctrl Pts',(1.32900986066236,-5.11766133679979,385.998774688909));
#41776=CARTESIAN_POINT('Ctrl Pts',(-1.2727295467071,-5.13194741485647,385.91964681345));
#41777=CARTESIAN_POINT('Ctrl Pts',(-3.5662988394905,-3.90361849510962,385.84051893799));
#41778=CARTESIAN_POINT('Ctrl Pts',(-4.99634867925468,-1.73009382497687,
385.76139106253));
#41779=CARTESIAN_POINT('Ctrl Pts',(-5.21661648089346,0.862344049196109,
385.68226318707));
#41780=CARTESIAN_POINT('Ctrl Pts',(-4.1737680903862,3.24597977436508,385.60313531161));
#41781=CARTESIAN_POINT('Ctrl Pts',(-2.12031175571847,4.84365593601313,385.524007436151));
#41782=CARTESIAN_POINT('Ctrl Pts',(0.446542510511727,5.26852204647746,385.44487956069));
#41783=CARTESIAN_POINT('Ctrl Pts',(2.90527399685678,4.41770390260608,385.365751685231));
#41784=CARTESIAN_POINT('Ctrl Pts',(4.66054210967394,2.4972128487314,385.286623809771));
#41785=CARTESIAN_POINT('Ctrl Pts',(5.2873381133244,-0.0279364153108744,
385.207495934311));
#41786=CARTESIAN_POINT('Ctrl Pts',(4.63389386761938,-2.54632134491165,385.128368058852));
#41787=CARTESIAN_POINT('Ctrl Pts',(2.85842993763932,-4.44815726560116,385.049240183392));
#41788=CARTESIAN_POINT('Ctrl Pts',(0.390845137441743,-5.27294650517633,
384.970112307932));
#41789=CARTESIAN_POINT('Ctrl Pts',(-2.1713762578616,-4.82098018194518,384.890984432472));
#41790=CARTESIAN_POINT('Ctrl Pts',(-4.20783530881936,-3.2016943610792,384.811856557012));
#41791=CARTESIAN_POINT('Ctrl Pts',(-5.2254376100198,-0.807171946801767,
384.732728681553));
#41792=CARTESIAN_POINT('Ctrl Pts',(-4.97778783059681,1.78279361718495,384.653600806093));
#41793=CARTESIAN_POINT('Ctrl Pts',(-3.52485021126398,3.94108560628483,384.574472930633));
#41794=CARTESIAN_POINT('Ctrl Pts',(-1.21842922909547,5.14510981239459,384.495345055173));
#41795=CARTESIAN_POINT('Ctrl Pts',(1.38301395642869,5.10333196688562,384.416217179714));
#41796=CARTESIAN_POINT('Ctrl Pts',(3.64958350715001,3.82586787438508,384.337089304254));
#41797=CARTESIAN_POINT('Ctrl Pts',(5.03246761935876,1.62203404033908,384.257961428794));
#41798=CARTESIAN_POINT('Ctrl Pts',(5.19682409785237,-0.974548133184912,
384.178833553334));
#41799=CARTESIAN_POINT('Ctrl Pts',(4.10285677781212,-3.33515982055948,384.099705677875));
#41800=CARTESIAN_POINT('Ctrl Pts',(2.0154514986864,-4.88821849187982,384.020577802414));
#41801=CARTESIAN_POINT('Ctrl Pts',(-0.559961559389509,-5.25767703647906,
383.941449926955));
#41802=CARTESIAN_POINT('Ctrl Pts',(-2.99978931706339,-4.3540772640303,383.862322051495));
#41803=CARTESIAN_POINT('Ctrl Pts',(-4.71326840155275,-2.39621070501691,
383.783194176035));
#41804=CARTESIAN_POINT('Ctrl Pts',(-5.28550858957794,0.14185808898655,383.704066300575));
#41805=CARTESIAN_POINT('Ctrl Pts',(-4.57795151673967,2.64557832586642,383.624938425116));
#41806=CARTESIAN_POINT('Ctrl Pts',(-2.76192026167378,4.50871614055144,383.545810549656));
#41807=CARTESIAN_POINT('Ctrl Pts',(-0.277136335846315,5.28014395819535,
383.466682674197));
#41808=CARTESIAN_POINT('Ctrl Pts',(2.27475150580887,4.77307347049397,383.387554798736));
#41809=CARTESIAN_POINT('Ctrl Pts',(4.27584642055071,3.11028329188466,383.308426923277));
#41810=CARTESIAN_POINT('Ctrl Pts',(5.24161683545466,0.6943901771998,383.229299047817));
#41811=CARTESIAN_POINT('Ctrl Pts',(4.93821764164047,-1.8896378731662,383.150171172357));
#41812=CARTESIAN_POINT('Ctrl Pts',(3.43911186553428,-4.01612180396144,383.071043296897));
#41813=CARTESIAN_POINT('Ctrl Pts',(1.1072828290795,-5.17016919494313,382.991915421438));
#41814=CARTESIAN_POINT('Ctrl Pts',(-1.49265617402097,-5.07234682509687,
382.912787545978));
#41815=CARTESIAN_POINT('Ctrl Pts',(-3.73117351815568,-3.74634074068643,
382.833659670518));
#41816=CARTESIAN_POINT('Ctrl Pts',(-5.06624977097178,-1.5132210763935,382.754531795058));
#41817=CARTESIAN_POINT('Ctrl Pts',(-5.17461860862547,1.08629969307746,382.675403919598));
#41818=CARTESIAN_POINT('Ctrl Pts',(-4.03004033454984,3.42279121037416,382.596276044139));
#41819=CARTESIAN_POINT('Ctrl Pts',(-1.90965538190854,4.93051124025298,382.517148168679));
#41820=CARTESIAN_POINT('Ctrl Pts',(0.673120594328623,5.24439066369047,382.438020293219));
#41821=CARTESIAN_POINT('Ctrl Pts',(3.09291170766135,4.28842884242289,382.35889241776));
#41822=CARTESIAN_POINT('Ctrl Pts',(4.76380612269667,2.29409589888282,382.2797645423));
#41823=CARTESIAN_POINT('Ctrl Pts',(5.28122477966896,-0.255713891925586,
382.20063666684));
#41824=CARTESIAN_POINT('Ctrl Pts',(4.51988342850276,-2.74360685242242,382.12150879138));
#41825=CARTESIAN_POINT('Ctrl Pts',(2.66412810880644,-4.56718142707082,382.04238091592));
#41826=CARTESIAN_POINT('Ctrl Pts',(0.16329884807764,-5.28488961607806,381.96325304046));
#41827=CARTESIAN_POINT('Ctrl Pts',(-2.37707049000228,-4.72295041827389,
381.884125165001));
#41828=CARTESIAN_POINT('Ctrl Pts',(-4.3418720751543,-3.0174279860352,381.804997289541));
#41829=CARTESIAN_POINT('Ctrl Pts',(-5.25536215553288,-0.581285972741413,
381.725869414081));
#41830=CARTESIAN_POINT('Ctrl Pts',(-4.89635442846138,1.99560469001251,381.646741538622));
#41831=CARTESIAN_POINT('Ctrl Pts',(-3.35177659407457,4.08929314568265,381.567613663161));
#41832=CARTESIAN_POINT('Ctrl Pts',(-0.995622270609436,5.1928278483096,381.488485787702));
#41833=CARTESIAN_POINT('Ctrl Pts',(1.60160528794473,5.03900637720777,381.409357912242));
#41834=CARTESIAN_POINT('Ctrl Pts',(3.81103098679937,3.66507402184023,381.330230036782));
#41835=CARTESIAN_POINT('Ctrl Pts',(5.09767944760569,1.40370545962173,381.251102161322));
#41836=CARTESIAN_POINT('Ctrl Pts',(5.15001032416474,-1.1975468378773,381.171974285863));
#41837=CARTESIAN_POINT('Ctrl Pts',(3.95535257236717,-3.50883325283227,381.092846410403));
#41838=CARTESIAN_POINT('Ctrl Pts',(1.8029725310162,-4.97051454281288,381.013718534943));
#41839=CARTESIAN_POINT('Ctrl Pts',(-0.785967070782117,-5.22866909753901,
380.934590659483));
#41840=CARTESIAN_POINT('Ctrl Pts',(-3.18459792796892,-4.22078912113472,
380.855462784024));
#41841=CARTESIAN_POINT('Ctrl Pts',(-4.81213180629493,-2.19091584657144,
380.776334908564));
#41842=CARTESIAN_POINT('Ctrl Pts',(-5.27448867275235,0.369450956041967,
380.697207033104));
#41843=CARTESIAN_POINT('Ctrl Pts',(-4.45971656638884,2.84036140577044,380.618079157644));
#41844=CARTESIAN_POINT('Ctrl Pts',(-2.56509888808806,4.6235259772432,380.538951282184));
#41845=CARTESIAN_POINT('Ctrl Pts',(-0.0493855337170155,5.28718127521391,
380.459823406725));
#41846=CARTESIAN_POINT('Ctrl Pts',(2.47828569939099,4.67063429954727,380.380695531265));
#41847=CARTESIAN_POINT('Ctrl Pts',(4.40588161411396,2.92317156019379,380.301567655805));
#41848=CARTESIAN_POINT('Ctrl Pts',(5.26666718771851,0.467911852513223,380.222439780345));
#41849=CARTESIAN_POINT('Ctrl Pts',(4.8522176299277,-2.10064486282949,380.143311904886));
#41850=CARTESIAN_POINT('Ctrl Pts',(3.26288495036134,-4.1605656548862,380.064184029426));
#41851=CARTESIAN_POINT('Ctrl Pts',(0.883499402425967,-5.21307525111868,
379.985056153966));
#41852=CARTESIAN_POINT('Ctrl Pts',(-1.70981070849824,-5.0033261046046,379.905928278506));
#41853=CARTESIAN_POINT('Ctrl Pts',(-3.88911883186622,-3.58210545343612,
379.826800403046));
#41854=CARTESIAN_POINT('Ctrl Pts',(-5.1267420551265,-1.29353804277671,379.747672527587));
#41855=CARTESIAN_POINT('Ctrl Pts',(-5.12301067114194,1.3082379108094,379.668544652126));
#41856=CARTESIAN_POINT('Ctrl Pts',(-3.87882817196482,3.59324599495851,379.589416776668));
#41857=CARTESIAN_POINT('Ctrl Pts',(-1.69545248338881,5.00820982432685,379.510288901207));
#41858=CARTESIAN_POINT('Ctrl Pts',(0.898448589337301,5.21051963821565,379.431161025747));
#41859=CARTESIAN_POINT('Ctrl Pts',(3.27480540417913,4.15118950816177,379.352033150288));
#41860=CARTESIAN_POINT('Ctrl Pts',(4.85822301267979,2.08671845896413,379.272905274828));
#41861=CARTESIAN_POINT('Ctrl Pts',(5.26530339668872,-0.483016468385486,
379.193777399368));
#41862=CARTESIAN_POINT('Ctrl Pts',(4.39747886842774,-2.93579705866137,379.114649523908));
#41863=CARTESIAN_POINT('Ctrl Pts',(2.4648785829925,-4.67772362790043,379.035521648449));
#41864=CARTESIAN_POINT('Ctrl Pts',(-0.0645507124447473,-5.28701787148826,
378.956393772989));
#41865=CARTESIAN_POINT('Ctrl Pts',(-2.57835013545374,-4.61614940691036,
378.877265897529));
#41866=CARTESIAN_POINT('Ctrl Pts',(-4.46784531508162,-2.82755778162292,
378.798138022069));
#41867=CARTESIAN_POINT('Ctrl Pts',(-5.27552668260484,-0.354320460935515,
378.719010146609));
#41868=CARTESIAN_POINT('Ctrl Pts',(-4.80582774062997,2.20470961700277,378.63988227115));
#41869=CARTESIAN_POINT('Ctrl Pts',(-3.17247821056078,4.22990623671853,378.56075439569));
#41870=CARTESIAN_POINT('Ctrl Pts',(-0.770966287939471,5.23090200164121,
378.48162652023));
#41871=CARTESIAN_POINT('Ctrl Pts',(1.81722219130848,4.96532257515351,378.40249864477));
#41872=CARTESIAN_POINT('Ctrl Pts',(3.96540079385267,3.49747356130477,378.323370769311));
#41873=CARTESIAN_POINT('Ctrl Pts',(5.15342409853101,1.18276998126983,378.244242893851));
#41874=CARTESIAN_POINT('Ctrl Pts',(5.09363218664291,-1.41832151330666,378.165115018391));
#41875=CARTESIAN_POINT('Ctrl Pts',(3.80050266687247,-3.67599024033094,378.085987142931));
#41876=CARTESIAN_POINT('Ctrl Pts',(1.58714516515185,-5.04357958127442,378.006859267472));
#41877=CARTESIAN_POINT('Ctrl Pts',(-1.01051292004705,-5.18995071328536,
377.927731392012));
#41878=CARTESIAN_POINT('Ctrl Pts',(-3.36349224912901,-4.07966232156074,
377.848603516552));
#41879=CARTESIAN_POINT('Ctrl Pts',(-4.90205833974629,-1.98155211933397,
377.769475641092));
#41880=CARTESIAN_POINT('Ctrl Pts',(-5.25367321659188,0.596357695664665,
377.690347765633));
#41881=CARTESIAN_POINT('Ctrl Pts',(-4.33319923422642,3.02986949626759,377.611219890172));
#41882=CARTESIAN_POINT('Ctrl Pts',(-2.36351373006459,4.72974921277116,377.532092014713));
#41883=CARTESIAN_POINT('Ctrl Pts',(0.178456984968689,5.28439948077629,377.452964139253));
#41884=CARTESIAN_POINT('Ctrl Pts',(2.67721733402229,4.55952104001336,377.373836263793));
#41885=CARTESIAN_POINT('Ctrl Pts',(4.52773440567874,2.73063104786141,377.294708388334));
#41886=CARTESIAN_POINT('Ctrl Pts',(5.28193652635228,0.240564543316707,377.215580512874));
#41887=CARTESIAN_POINT('Ctrl Pts',(4.75720630136386,-2.3077506308472,377.136452637414));
#41888=CARTESIAN_POINT('Ctrl Pts',(3.08059835436342,-4.29728269340077,377.057324761954));
#41889=CARTESIAN_POINT('Ctrl Pts',(0.658075181053442,-5.24629982216222,
376.978196886494));
#41890=CARTESIAN_POINT('Ctrl Pts',(-1.923789860657,-4.92501343550216,376.899069011035));
#41891=CARTESIAN_POINT('Ctrl Pts',(-4.03984145181191,-3.4112176436405,376.819941135575));
#41892=CARTESIAN_POINT('Ctrl Pts',(-5.17771318819473,-1.07145270939303,
376.740813260115));
#41893=CARTESIAN_POINT('Ctrl Pts',(-5.0618885123847,1.52774652882403,376.661685384655));
#41894=CARTESIAN_POINT('Ctrl Pts',(-3.72041242686768,3.75702756739127,376.582557509196));
#41895=CARTESIAN_POINT('Ctrl Pts',(-1.47810086816716,5.0766073897426,376.503429633736));
#41896=CARTESIAN_POINT('Ctrl Pts',(1.12210802704861,5.16697187426544,376.424301758276));
#41897=CARTESIAN_POINT('Ctrl Pts',(3.45061728097363,4.00624077340234,376.345173882816));
#41898=CARTESIAN_POINT('Ctrl Pts',(4.94361743453053,1.87546566308182,376.266046007357));
#41899=CARTESIAN_POINT('Ctrl Pts',(5.23960352937691,-0.709422013391795,
376.186918131896));
#41900=CARTESIAN_POINT('Ctrl Pts',(4.2669075188957,-3.12253502690154,376.107790256437));
#41901=CARTESIAN_POINT('Ctrl Pts',(2.26105138176727,-4.77957859502704,376.028662380977));
#41902=CARTESIAN_POINT('Ctrl Pts',(-0.292280359441297,-5.27932727476591,
375.949534505517));
#41903=CARTESIAN_POINT('Ctrl Pts',(-2.77484145645776,-4.50077558721857,
375.870406630058));
#41904=CARTESIAN_POINT('Ctrl Pts',(-4.58552092957851,-2.63243616845826,
375.791278754598));
#41905=CARTESIAN_POINT('Ctrl Pts',(-5.28589405424394,-0.126697339588848,
375.712150879138));
#41906=CARTESIAN_POINT('Ctrl Pts',(-4.70637522968859,2.40972094307884,375.633023003678));
#41907=CARTESIAN_POINT('Ctrl Pts',(-2.98728944096456,4.36266186682328,375.553895128218));
#41908=CARTESIAN_POINT('Ctrl Pts',(-0.544875549618088,5.2592655277028,375.474767252759));
#41909=CARTESIAN_POINT('Ctrl Pts',(2.02945798133318,4.88240903418803,375.395639377299));
#41910=CARTESIAN_POINT('Ctrl Pts',(4.1124194375256,3.3233956145555,375.316511501839));
#41911=CARTESIAN_POINT('Ctrl Pts',(5.19956989745793,0.959601216722932,375.237383626379));
#41912=CARTESIAN_POINT('Ctrl Pts',(5.02785240284651,-1.63637626402564,375.15825575092));
#41913=CARTESIAN_POINT('Ctrl Pts',(3.63845954881624,-3.83644847785649,375.07912787546));
#41914=CARTESIAN_POINT('Ctrl Pts',(2.1252131908655,-4.68314727417153,375.026375958487));
#41915=CARTESIAN_POINT('Ctrl Pts',(1.3130361863572,-4.90075024188303,375.));
#41916=CARTESIAN_POINT('Ctrl Pts',(3.43378788736214,2.93584158412968,400.));
#41917=CARTESIAN_POINT('Ctrl Pts',(3.5274081047691,2.83896859117363,400.));
#41918=CARTESIAN_POINT('Ctrl Pts',(3.61639766139016,2.73803801067182,400.));
#41919=CARTESIAN_POINT('Ctrl Pts',(3.70064392711817,2.63347462098305,400.));
#41920=CARTESIAN_POINT('Ctrl Pts',(3.7863602040819,2.52708670700993,400.));
#41921=CARTESIAN_POINT('Ctrl Pts',(3.86716669541736,2.4169376104458,400.));
#41922=CARTESIAN_POINT('Ctrl Pts',(3.94291532865978,2.30342952486372,400.));
#41923=CARTESIAN_POINT('Ctrl Pts',(4.0194785589048,2.18870077902246,400.));
#41924=CARTESIAN_POINT('Ctrl Pts',(4.09087506217895,2.07053982333204,400.));
#41925=CARTESIAN_POINT('Ctrl Pts',(4.15691470252894,1.94932444936402,400.));
#41926=CARTESIAN_POINT('Ctrl Pts',(4.22265038067262,1.82866699624951,400.));
#41927=CARTESIAN_POINT('Ctrl Pts',(4.28307881326963,1.70498249960347,400.));
#41928=CARTESIAN_POINT('Ctrl Pts',(4.33796903578875,1.57861622186133,400.));
#41929=CARTESIAN_POINT('Ctrl Pts',(4.35514545623615,1.53907329021963,400.));
#41930=CARTESIAN_POINT('Ctrl Pts',(4.37177922400871,1.4992675947038,400.));
#41931=CARTESIAN_POINT('Ctrl Pts',(4.38786228046478,1.45920932342454,400.));
#41932=CARTESIAN_POINT('Ctrl Pts',(4.39466658849891,1.44226174770453,400.));
#41933=CARTESIAN_POINT('Ctrl Pts',(4.40137035215038,1.4252737748662,400.));
#41934=CARTESIAN_POINT('Ctrl Pts',(4.40797035684919,1.40825358562441,400.));
#41935=CARTESIAN_POINT('Ctrl Pts',(4.45876403554847,1.27726609952389,400.));
#41936=CARTESIAN_POINT('Ctrl Pts',(4.50346815482664,1.14424239282724,400.));
#41937=CARTESIAN_POINT('Ctrl Pts',(4.54192438339399,1.0095915875114,400.));
#41938=CARTESIAN_POINT('Ctrl Pts',(4.54556160496616,0.996856204140475,400.));
#41939=CARTESIAN_POINT('Ctrl Pts',(4.54914290628383,0.984106240915922,400.));
#41940=CARTESIAN_POINT('Ctrl Pts',(4.55266813447105,0.971342029205324,400.));
#41941=CARTESIAN_POINT('Ctrl Pts',(4.58957020263633,0.837726335240427,400.));
#41942=CARTESIAN_POINT('Ctrl Pts',(4.62033177525015,0.702551284224113,400.));
#41943=CARTESIAN_POINT('Ctrl Pts',(4.64501953741251,0.566245432199611,400.));
#41944=CARTESIAN_POINT('Ctrl Pts',(4.66997011124341,0.428488546737278,400.));
#41945=CARTESIAN_POINT('Ctrl Pts',(4.68871702492031,0.289575922051531,400.));
#41946=CARTESIAN_POINT('Ctrl Pts',(4.70127911966368,0.149931994443125,400.));
#41947=CARTESIAN_POINT('Ctrl Pts',(4.71259060845871,0.0241901691579915,
400.));
#41948=CARTESIAN_POINT('Ctrl Pts',(4.71888682786237,-0.102145233205809,
400.));
#41949=CARTESIAN_POINT('Ctrl Pts',(4.72014590598849,-0.228768981279396,
400.));
#41950=CARTESIAN_POINT('Ctrl Pts',(4.72038025896983,-0.252337536919386,
400.));
#41951=CARTESIAN_POINT('Ctrl Pts',(4.72044000678068,-0.275916082362071,
400.));
#41952=CARTESIAN_POINT('Ctrl Pts',(4.72032487691908,-0.299502644881673,
400.));
#41953=CARTESIAN_POINT('Ctrl Pts',(4.7202295663887,-0.319028836890583,400.));
#41954=CARTESIAN_POINT('Ctrl Pts',(4.72001432373552,-0.338562445738198,
400.));
#41955=CARTESIAN_POINT('Ctrl Pts',(4.71967941555818,-0.358084898519809,
400.));
#41956=CARTESIAN_POINT('Ctrl Pts',(4.71723826258667,-0.50038448044343,400.));
#41957=CARTESIAN_POINT('Ctrl Pts',(4.70844382065583,-0.642283037525432,
400.));
#41958=CARTESIAN_POINT('Ctrl Pts',(4.69336920270997,-0.783339178745919,
400.));
#41959=CARTESIAN_POINT('Ctrl Pts',(4.6781762779915,-0.925502339519639,400.));
#41960=CARTESIAN_POINT('Ctrl Pts',(4.65660432919034,-1.06681060067863,400.));
#41961=CARTESIAN_POINT('Ctrl Pts',(4.62867689090467,-1.20682343753469,400.));
#41962=CARTESIAN_POINT('Ctrl Pts',(4.61869343839589,-1.25687498515869,400.));
#41963=CARTESIAN_POINT('Ctrl Pts',(4.6078973313099,-1.30676103650428,400.));
#41964=CARTESIAN_POINT('Ctrl Pts',(4.59628802798414,-1.35646151489045,400.));
#41965=CARTESIAN_POINT('Ctrl Pts',(4.56393613692852,-1.49496288892161,400.));
#41966=CARTESIAN_POINT('Ctrl Pts',(4.5252728763513,-1.63202392528166,400.));
#41967=CARTESIAN_POINT('Ctrl Pts',(4.48051876179014,-1.76728613860278,400.));
#41968=CARTESIAN_POINT('Ctrl Pts',(4.45444111221125,-1.84610169857621,400.));
#41969=CARTESIAN_POINT('Ctrl Pts',(4.42629449108343,-1.92430635496666,400.));
#41970=CARTESIAN_POINT('Ctrl Pts',(4.3961147432142,-2.00182684735068,400.));
#41971=CARTESIAN_POINT('Ctrl Pts',(4.37905752655991,-2.04564046168142,400.));
#41972=CARTESIAN_POINT('Ctrl Pts',(4.36135075314648,-2.08923549081769,400.));
#41973=CARTESIAN_POINT('Ctrl Pts',(4.34300012999985,-2.13259835388101,400.));
#41974=CARTESIAN_POINT('Ctrl Pts',(4.33569114983399,-2.14986960965973,400.));
#41975=CARTESIAN_POINT('Ctrl Pts',(4.32828379731778,-2.1670950989908,400.));
#41976=CARTESIAN_POINT('Ctrl Pts',(4.32077934892109,-2.18427268326289,400.));
#41977=CARTESIAN_POINT('Ctrl Pts',(4.26291559960507,-2.31672204897711,400.));
#41978=CARTESIAN_POINT('Ctrl Pts',(4.19927220468674,-2.44635051906979,400.));
#41979=CARTESIAN_POINT('Ctrl Pts',(4.13013682131626,-2.57280699644751,400.));
#41980=CARTESIAN_POINT('Ctrl Pts',(4.06045781537672,-2.70025782131784,400.));
#41981=CARTESIAN_POINT('Ctrl Pts',(3.98519984558575,-2.82448729912954,400.));
#41982=CARTESIAN_POINT('Ctrl Pts',(3.90460511771477,-2.94512595263581,400.));
#41983=CARTESIAN_POINT('Ctrl Pts',(3.82424500701874,-3.06541341815719,400.));
#41984=CARTESIAN_POINT('Ctrl Pts',(3.73857881602801,-3.18213164834041,400.));
#41985=CARTESIAN_POINT('Ctrl Pts',(3.6477996177404,-3.29489368172134,400.));
#41986=CARTESIAN_POINT('Ctrl Pts',(3.5967838663573,-3.35826326383848,400.));
#41987=CARTESIAN_POINT('Ctrl Pts',(3.54415252096129,-3.42038297838046,400.));
#41988=CARTESIAN_POINT('Ctrl Pts',(3.48993392052895,-3.48117996717138,400.));
#41989=CARTESIAN_POINT('Ctrl Pts',(3.44896085489101,-3.52712432929906,400.));
#41990=CARTESIAN_POINT('Ctrl Pts',(3.40708123835602,-3.57231323683387,400.));
#41991=CARTESIAN_POINT('Ctrl Pts',(3.36432098798037,-3.61672891625407,400.));
#41992=CARTESIAN_POINT('Ctrl Pts',(3.33855500174508,-3.64349241212974,400.));
#41993=CARTESIAN_POINT('Ctrl Pts',(3.31246924398559,-3.66997513430726,400.));
#41994=CARTESIAN_POINT('Ctrl Pts',(3.28606918882681,-3.69617297251379,400.));
#41995=CARTESIAN_POINT('Ctrl Pts',(3.27036247014898,-3.71175938217099,400.));
#41996=CARTESIAN_POINT('Ctrl Pts',(3.25455092639766,-3.72723854435311,400.));
#41997=CARTESIAN_POINT('Ctrl Pts',(3.23863897351742,-3.74260697959096,400.));
#41998=CARTESIAN_POINT('Ctrl Pts',(3.1336340986207,-3.84402511673945,400.));
#41999=CARTESIAN_POINT('Ctrl Pts',(3.02421929001433,-3.94066423251855,400.));
#42000=CARTESIAN_POINT('Ctrl Pts',(2.9108005879282,-4.03233943093569,400.));
#42001=CARTESIAN_POINT('Ctrl Pts',(2.80145832608402,-4.12071968362393,400.));
#42002=CARTESIAN_POINT('Ctrl Pts',(2.6883940765038,-4.20448664484191,400.));
#42003=CARTESIAN_POINT('Ctrl Pts',(2.57193725133249,-4.28344581179871,400.));
#42004=CARTESIAN_POINT('Ctrl Pts',(2.52394060920348,-4.31598812843542,400.));
#42005=CARTESIAN_POINT('Ctrl Pts',(2.47536734937678,-4.34771342641671,400.));
#42006=CARTESIAN_POINT('Ctrl Pts',(2.4262391678432,-4.37860645542617,400.));
#42007=CARTESIAN_POINT('Ctrl Pts',(2.4057205129273,-4.39150909871084,400.));
#42008=CARTESIAN_POINT('Ctrl Pts',(2.38510290902907,-4.40426785187222,400.));
#42009=CARTESIAN_POINT('Ctrl Pts',(2.36439500508045,-4.41687723791363,400.));
#42010=CARTESIAN_POINT('Ctrl Pts',(2.23718127032588,-4.49433979014823,400.));
#42011=CARTESIAN_POINT('Ctrl Pts',(2.10670807231056,-4.56608151115334,400.));
#42012=CARTESIAN_POINT('Ctrl Pts',(1.97337536799814,-4.63189274468176,400.));
#42013=CARTESIAN_POINT('Ctrl Pts',(1.84010399988323,-4.69767370348621,400.));
#42014=CARTESIAN_POINT('Ctrl Pts',(1.70397511685538,-4.75753010362705,400.));
#42015=CARTESIAN_POINT('Ctrl Pts',(1.56535633801641,-4.81121182598771,400.));
#42016=CARTESIAN_POINT('Ctrl Pts',(1.52584133805609,-4.82651446589492,400.));
#42017=CARTESIAN_POINT('Ctrl Pts',(1.48612384295406,-4.84131506971587,400.));
#42018=CARTESIAN_POINT('Ctrl Pts',(1.44621200692229,-4.85560715259022,400.));
#42019=CARTESIAN_POINT('Ctrl Pts',(1.4021027224054,-4.87140230542011,400.));
#42020=CARTESIAN_POINT('Ctrl Pts',(1.35775607141996,-4.88657636029028,400.));
#42021=CARTESIAN_POINT('Ctrl Pts',(1.31318543090145,-4.90112867346808,400.));
#42022=CARTESIAN_POINT('Ctrl Pts',(-4.51746064445937,-7.62825515632226E-5,
398.387416697508));
#42023=CARTESIAN_POINT('Ctrl Pts',(-4.51763289072636,-0.284226777710601,
398.397425295273));
#42024=CARTESIAN_POINT('Ctrl Pts',(-4.49123863994107,-0.568345670691312,
398.407433893039));
#42025=CARTESIAN_POINT('Ctrl Pts',(-4.4379719366677,-0.847333855511198,
398.417442490804));
#42026=CARTESIAN_POINT('Ctrl Pts',(-4.29759659267063,-1.58255980359031,
398.443818449291));
#42027=CARTESIAN_POINT('Ctrl Pts',(-3.97059302033473,-2.2821531656744,398.470194407778));
#42028=CARTESIAN_POINT('Ctrl Pts',(-3.49655043505552,-2.86141654221982,
398.496570366264));
#42029=CARTESIAN_POINT('Ctrl Pts',(-3.0225078497763,-3.44067991876523,398.522946324751));
#42030=CARTESIAN_POINT('Ctrl Pts',(-2.40142625155378,-3.89961330977197,
398.549322283237));
#42031=CARTESIAN_POINT('Ctrl Pts',(-1.70849788678631,-4.18265520276417,
398.575698241724));
#42032=CARTESIAN_POINT('Ctrl Pts',(-1.01556952201883,-4.46569709575638,
398.60207420021));
#42033=CARTESIAN_POINT('Ctrl Pts',(-0.250794390706405,-4.57284749073406,
398.628450158697));
#42034=CARTESIAN_POINT('Ctrl Pts',(0.493238771257572,-4.49113405337507,
398.654826117184));
#42035=CARTESIAN_POINT('Ctrl Pts',(1.23727193322155,-4.40942061601609,398.68120207567));
#42036=CARTESIAN_POINT('Ctrl Pts',(1.96056312583708,-4.13884334632044,398.707578034157));
#42037=CARTESIAN_POINT('Ctrl Pts',(2.57554593307285,-3.71216011566315,398.733953992643));
#42038=CARTESIAN_POINT('Ctrl Pts',(3.19052874030862,-3.28547688500585,398.76032995113));
#42039=CARTESIAN_POINT('Ctrl Pts',(3.69720316216463,-2.70268769338692,398.786705909617));
#42040=CARTESIAN_POINT('Ctrl Pts',(4.03422784198701,-2.03434886067149,398.813081868103));
#42041=CARTESIAN_POINT('Ctrl Pts',(4.37125252180939,-1.36601002795605,398.83945782659));
#42042=CARTESIAN_POINT('Ctrl Pts',(4.53862745959814,-0.612121554144129,
398.865833785076));
#42043=CARTESIAN_POINT('Ctrl Pts',(4.51608913784387,0.136045847258709,398.892209743563));
#42044=CARTESIAN_POINT('Ctrl Pts',(4.49355081608961,0.884213248661547,398.91858570205));
#42045=CARTESIAN_POINT('Ctrl Pts',(4.28109923479233,1.6266595776553,398.944961660536));
#42046=CARTESIAN_POINT('Ctrl Pts',(3.90445518858537,2.27349934610636,398.971337619023));
#42047=CARTESIAN_POINT('Ctrl Pts',(3.5278111423784,2.92033911455742,398.997713577509));
#42048=CARTESIAN_POINT('Ctrl Pts',(2.98697463126176,3.47157232246578,399.024089535996));
#42049=CARTESIAN_POINT('Ctrl Pts',(2.34742289856565,3.86046308384535,399.050465494483));
#42050=CARTESIAN_POINT('Ctrl Pts',(1.70787116586954,4.24935384522491,399.076841452969));
#42051=CARTESIAN_POINT('Ctrl Pts',(0.969604211593966,4.47590216007566,399.103217411456));
#42052=CARTESIAN_POINT('Ctrl Pts',(0.222001520718283,4.51268048034993,399.129593369942));
#42053=CARTESIAN_POINT('Ctrl Pts',(-0.525601170157399,4.5494588006242,399.155969328429));
#42054=CARTESIAN_POINT('Ctrl Pts',(-1.28253959763319,4.39646712632199,399.182345286915));
#42055=CARTESIAN_POINT('Ctrl Pts',(-1.95717379804064,4.07222787544583,399.208721245402));
#42056=CARTESIAN_POINT('Ctrl Pts',(-2.63180799844808,3.74798862456968,399.235097203889));
#42057=CARTESIAN_POINT('Ctrl Pts',(-3.22413797178719,3.25250179711959,399.261473162375));
#42058=CARTESIAN_POINT('Ctrl Pts',(-3.66245231437547,2.64575381071457,399.287849120862));
#42059=CARTESIAN_POINT('Ctrl Pts',(-4.10076665696376,2.03900582430954,399.314225079348));
#42060=CARTESIAN_POINT('Ctrl Pts',(-4.38506536880122,1.32099667894959,399.340601037835));
#42061=CARTESIAN_POINT('Ctrl Pts',(-4.48092940799817,0.578654358541173,
399.366976996322));
#42062=CARTESIAN_POINT('Ctrl Pts',(-4.50569226564232,0.386898228114258,
399.37379023005));
#42063=CARTESIAN_POINT('Ctrl Pts',(-4.51788177656568,0.193518461005119,
399.380603463779));
#42064=CARTESIAN_POINT('Ctrl Pts',(-4.51769110620511,0.00011483889287206,
399.387416697508));
#42065=CARTESIAN_POINT('Ctrl Pts',(-1.31303618635555,-4.90075024188347,
400.));
#42066=CARTESIAN_POINT('Ctrl Pts',(-2.12521319086393,-4.68314727417224,
399.973624041513));
#42067=CARTESIAN_POINT('Ctrl Pts',(-3.63845957255092,-3.83644859241818,
399.92087212454));
#42068=CARTESIAN_POINT('Ctrl Pts',(-5.02785239518849,-1.63637624738159,
399.84174424908));
#42069=CARTESIAN_POINT('Ctrl Pts',(-5.19956989353463,0.959601198026513,
399.76261637362));
#42070=CARTESIAN_POINT('Ctrl Pts',(-4.11241943286933,3.32339561801255,399.683488498161));
#42071=CARTESIAN_POINT('Ctrl Pts',(-2.02945797892606,4.8824090247121,399.604360622701));
#42072=CARTESIAN_POINT('Ctrl Pts',(0.54487554882432,5.2592655238007,399.525232747241));
#42073=CARTESIAN_POINT('Ctrl Pts',(2.98728943775363,4.36266186092565,399.446104871781));
#42074=CARTESIAN_POINT('Ctrl Pts',(4.70637522433117,2.40972094089285,399.366976996322));
#42075=CARTESIAN_POINT('Ctrl Pts',(5.28589404837916,-0.126697339701679,
399.287849120862));
#42076=CARTESIAN_POINT('Ctrl Pts',(4.58552092441564,-2.6324361653814,399.208721245402));
#42077=CARTESIAN_POINT('Ctrl Pts',(2.77484145336967,-4.50077558224301,399.129593369943));
#42078=CARTESIAN_POINT('Ctrl Pts',(0.292280359106768,-5.27932726882375,
399.050465494482));
#42079=CARTESIAN_POINT('Ctrl Pts',(-2.26105137922953,-4.77957858969287,
398.971337619023));
#42080=CARTESIAN_POINT('Ctrl Pts',(-4.26690751412045,-3.12253502339944,
398.892209743563));
#42081=CARTESIAN_POINT('Ctrl Pts',(-5.23960352350959,-0.709422012603199,
398.813081868103));
#42082=CARTESIAN_POINT('Ctrl Pts',(-4.94361742899746,1.87546566098248,398.733953992643));
#42083=CARTESIAN_POINT('Ctrl Pts',(-3.45061727711166,4.00624076891526,398.654826117184));
#42084=CARTESIAN_POINT('Ctrl Pts',(-1.12210802579434,5.16697186848109,398.575698241724));
#42085=CARTESIAN_POINT('Ctrl Pts',(1.47810086651078,5.07660738405961,398.496570366264));
#42086=CARTESIAN_POINT('Ctrl Pts',(3.72041242270134,3.75702756318667,398.417442490805));
#42087=CARTESIAN_POINT('Ctrl Pts',(5.06188850671742,1.52774652711538,398.338314615344));
#42088=CARTESIAN_POINT('Ctrl Pts',(5.17771318239863,-1.0714527081918,398.259186739885));
#42089=CARTESIAN_POINT('Ctrl Pts',(4.03984144729043,-3.41121763982034,398.180058864425));
#42090=CARTESIAN_POINT('Ctrl Pts',(1.92378985850489,-4.92501342998799,398.100930988965));
#42091=CARTESIAN_POINT('Ctrl Pts',(-0.658075180315041,-5.24629981628919,
398.021803113506));
#42092=CARTESIAN_POINT('Ctrl Pts',(-3.08059835091328,-4.29728268859095,
397.942675238046));
#42093=CARTESIAN_POINT('Ctrl Pts',(-4.75720629603741,-2.30775062826524,
397.863547362586));
#42094=CARTESIAN_POINT('Ctrl Pts',(-5.28193652043922,0.240564543045645,
397.784419487126));
#42095=CARTESIAN_POINT('Ctrl Pts',(-4.52773440061085,2.73063104480294,397.705291611666));
#42096=CARTESIAN_POINT('Ctrl Pts',(-2.67721733102668,4.55952103490808,397.626163736206));
#42097=CARTESIAN_POINT('Ctrl Pts',(-0.178456984770649,5.28439947486034,
397.547035860747));
#42098=CARTESIAN_POINT('Ctrl Pts',(2.36351372741711,4.72974920747697,397.467907985287));
#42099=CARTESIAN_POINT('Ctrl Pts',(4.33319922937441,3.02986949287705,397.388780109827));
#42100=CARTESIAN_POINT('Ctrl Pts',(5.25367321071018,0.596357694998765,397.309652234368));
#42101=CARTESIAN_POINT('Ctrl Pts',(4.90205833425909,-1.98155211711401,397.230524358907));
#42102=CARTESIAN_POINT('Ctrl Pts',(3.36349224536493,-4.07966231699243,397.151396483448));
#42103=CARTESIAN_POINT('Ctrl Pts',(1.01051291891753,-5.18995070747486,397.072268607988));
#42104=CARTESIAN_POINT('Ctrl Pts',(-1.58714516337332,-5.04357957562867,
396.993140732529));
#42105=CARTESIAN_POINT('Ctrl Pts',(-3.80050266261658,-3.67599023621695,
396.914012857068));
#42106=CARTESIAN_POINT('Ctrl Pts',(-5.09363218094012,-1.41832151172053,
396.834884981609));
#42107=CARTESIAN_POINT('Ctrl Pts',(-5.15342409276215,1.182769979944,396.755757106149));
#42108=CARTESIAN_POINT('Ctrl Pts',(-3.96540078941456,3.49747355738801,396.676629230689));
#42109=CARTESIAN_POINT('Ctrl Pts',(-1.81722218927578,4.96532256959422,396.597501355229));
#42110=CARTESIAN_POINT('Ctrl Pts',(0.770966287074601,5.23090199578547,396.51837347977));
#42111=CARTESIAN_POINT('Ctrl Pts',(3.17247820700774,4.22990623198423,396.43924560431));
#42112=CARTESIAN_POINT('Ctrl Pts',(4.8058277352491,2.20470961453625,396.36011772885));
#42113=CARTESIAN_POINT('Ctrl Pts',(5.275526676699,-0.354320460537079,396.28098985339));
#42114=CARTESIAN_POINT('Ctrl Pts',(4.46784531008081,-2.82755777845599,396.201861977931));
#42115=CARTESIAN_POINT('Ctrl Pts',(2.57835013256881,-4.61614940174172,396.122734102471));
#42116=CARTESIAN_POINT('Ctrl Pts',(0.0645507123742531,-5.2870178655694,
396.043606227011));
#42117=CARTESIAN_POINT('Ctrl Pts',(-2.46487858023149,-4.67772362266456,
395.964478351551));
#42118=CARTESIAN_POINT('Ctrl Pts',(-4.39747886350376,-2.93579705537622,
395.885350476092));
#42119=CARTESIAN_POINT('Ctrl Pts',(-5.26530339079403,-0.48301646784655,
395.806222600631));
#42120=CARTESIAN_POINT('Ctrl Pts',(-4.85822300724173,2.08671845662638,395.727094725172));
#42121=CARTESIAN_POINT('Ctrl Pts',(-3.27480540051438,4.15118950351341,395.647966849712));
#42122=CARTESIAN_POINT('Ctrl Pts',(-0.898448588333209,5.21051963238218,
395.568838974252));
#42123=CARTESIAN_POINT('Ctrl Pts',(1.69545248148909,5.00820981872071,395.489711098793));
#42124=CARTESIAN_POINT('Ctrl Pts',(3.87882816762124,3.59324599093717,395.410583223333));
#42125=CARTESIAN_POINT('Ctrl Pts',(5.12301066540628,1.30823790934658,395.331455347873));
#42126=CARTESIAN_POINT('Ctrl Pts',(5.12674204938754,-1.29353804132683,395.252327472413));
#42127=CARTESIAN_POINT('Ctrl Pts',(3.88911882751359,-3.58210544942458,395.173199596953));
#42128=CARTESIAN_POINT('Ctrl Pts',(1.70981070658587,-5.00332609900278,395.094071721494));
#42129=CARTESIAN_POINT('Ctrl Pts',(-0.883499401435098,-5.21307524528295,
395.014943846034));
#42130=CARTESIAN_POINT('Ctrl Pts',(-3.26288494670713,-4.16056565022955,
394.935815970574));
#42131=CARTESIAN_POINT('Ctrl Pts',(-4.85221762449495,-2.10064486047942,
394.856688095114));
#42132=CARTESIAN_POINT('Ctrl Pts',(-5.26666718182262,0.467911851987696,
394.777560219655));
#42133=CARTESIAN_POINT('Ctrl Pts',(-4.40588160918252,2.92317155691987,394.698432344195));
#42134=CARTESIAN_POINT('Ctrl Pts',(-2.47828569661807,4.67063429431767,394.619304468735));
#42135=CARTESIAN_POINT('Ctrl Pts',(0.0493855336599835,5.28718126929493,
394.540176593275));
#42136=CARTESIAN_POINT('Ctrl Pts',(2.56509888521489,4.623525972068,394.461048717816));
#42137=CARTESIAN_POINT('Ctrl Pts',(4.45971656139522,2.84036140259214,394.381920842355));
#42138=CARTESIAN_POINT('Ctrl Pts',(5.27448866684743,0.369450955630144,394.302792966896));
#42139=CARTESIAN_POINT('Ctrl Pts',(4.81213180090847,-2.19091584411711,394.223665091436));
#42140=CARTESIAN_POINT('Ctrl Pts',(3.18459792440514,-4.2207891164085,394.144537215977));
#42141=CARTESIAN_POINT('Ctrl Pts',(0.785967069903959,-5.22866909168525,
394.065409340517));
#42142=CARTESIAN_POINT('Ctrl Pts',(-1.8029725289961,-4.97051453724898,393.986281465057));
#42143=CARTESIAN_POINT('Ctrl Pts',(-3.95535256793798,-3.50883324890547,
393.907153589597));
#42144=CARTESIAN_POINT('Ctrl Pts',(-5.15001031839888,-1.19754683653839,
393.828025714137));
#42145=CARTESIAN_POINT('Ctrl Pts',(-5.0976794418993,1.40370545804854,393.748897838677));
#42146=CARTESIAN_POINT('Ctrl Pts',(-3.81103098253419,3.66507401773587,393.669769963218));
#42147=CARTESIAN_POINT('Ctrl Pts',(-1.60160528615343,5.03900637156607,393.590642087758));
#42148=CARTESIAN_POINT('Ctrl Pts',(0.995622269493122,5.19282784249655,393.511514212298));
#42149=CARTESIAN_POINT('Ctrl Pts',(3.3517765903209,4.08929314110579,393.432386336838));
#42150=CARTESIAN_POINT('Ctrl Pts',(4.89635442297923,1.99560468778007,393.353258461378));
#42151=CARTESIAN_POINT('Ctrl Pts',(5.2553621496497,-0.581285972088894,393.274130585919));
#42152=CARTESIAN_POINT('Ctrl Pts',(4.34187207029457,-3.01742798265574,393.195002710459));
#42153=CARTESIAN_POINT('Ctrl Pts',(2.37707048734272,-4.72295041298575,393.115874834999));
#42154=CARTESIAN_POINT('Ctrl Pts',(-0.163298847893048,-5.28488961016167,
393.03674695954));
#42155=CARTESIAN_POINT('Ctrl Pts',(-2.66412810582239,-4.56718142195876,
392.957619084079));
#42156=CARTESIAN_POINT('Ctrl Pts',(-4.51988342344183,-2.74360684935247,
392.87849120862));
#42157=CARTESIAN_POINT('Ctrl Pts',(-5.28122477375654,-0.255713891641081,
392.79936333316));
#42158=CARTESIAN_POINT('Ctrl Pts',(-4.76380611736435,2.29409589631297,392.7202354577));
#42159=CARTESIAN_POINT('Ctrl Pts',(-3.09291170420029,4.28842883762094,392.64110758224));
#42160=CARTESIAN_POINT('Ctrl Pts',(-0.67312059357683,5.24439065781915,392.561979706781));
#42161=CARTESIAN_POINT('Ctrl Pts',(1.90965537976903,4.9305112347339,392.482851831321));
#42162=CARTESIAN_POINT('Ctrl Pts',(4.03004033003705,3.4227912065437,392.403723955861));
#42163=CARTESIAN_POINT('Ctrl Pts',(5.17461860283211,1.0862996918631,392.324596080401));
#42164=CARTESIAN_POINT('Ctrl Pts',(5.06624976530063,-1.51322107469774,392.245468204942));
#42165=CARTESIAN_POINT('Ctrl Pts',(3.73117351397988,-3.74634073649114,392.166340329482));
#42166=CARTESIAN_POINT('Ctrl Pts',(1.49265617235166,-5.07234681941786,392.087212454022));
#42167=CARTESIAN_POINT('Ctrl Pts',(-1.10728282783815,-5.1701691891555,392.008084578562));
#42168=CARTESIAN_POINT('Ctrl Pts',(-3.43911186168285,-4.01612179946654,
391.928956703103));
#42169=CARTESIAN_POINT('Ctrl Pts',(-4.93821763611149,-1.8896378710524,391.849828827643));
#42170=CARTESIAN_POINT('Ctrl Pts',(-5.24161682958689,0.694390176420624,
391.770700952183));
#42171=CARTESIAN_POINT('Ctrl Pts',(-4.27584641576499,3.1102832884012,391.691573076723));
#42172=CARTESIAN_POINT('Ctrl Pts',(-2.27475150326393,4.77307346514974,391.612445201264));
#42173=CARTESIAN_POINT('Ctrl Pts',(0.277136335534271,5.28014395228432,391.533317325804));
#42174=CARTESIAN_POINT('Ctrl Pts',(2.76192025858026,4.50871613550486,391.454189450344));
#42175=CARTESIAN_POINT('Ctrl Pts',(4.57795151161372,2.64557832290629,391.375061574885));
#42176=CARTESIAN_POINT('Ctrl Pts',(5.28550858366077,0.141858088829558,391.295933699424));
#42177=CARTESIAN_POINT('Ctrl Pts',(4.71326839627705,-2.39621070233275,391.216805823965));
#42178=CARTESIAN_POINT('Ctrl Pts',(2.99978931370662,-4.35407725915487,391.137677948505));
#42179=CARTESIAN_POINT('Ctrl Pts',(0.559961558764467,-5.2576770305929,391.058550073045));
#42180=CARTESIAN_POINT('Ctrl Pts',(-2.01545149642842,-4.88821848640817,
390.979422197585));
#42181=CARTESIAN_POINT('Ctrl Pts',(-4.10285677321784,-3.33515981682715,
390.900294322126));
#42182=CARTESIAN_POINT('Ctrl Pts',(-5.19682409203417,-0.974548132095691,
390.821166446665));
#42183=CARTESIAN_POINT('Ctrl Pts',(-5.03246761372548,1.62203403852146,390.742038571206));
#42184=CARTESIAN_POINT('Ctrl Pts',(-3.64958350306562,3.82586787010077,390.662910695746));
#42185=CARTESIAN_POINT('Ctrl Pts',(-1.38301395488213,5.10333196117197,390.583782820286));
#42186=CARTESIAN_POINT('Ctrl Pts',(1.21842922772966,5.14510980663504,390.504654944826));
#42187=CARTESIAN_POINT('Ctrl Pts',(3.52485020731651,3.94108560187402,390.425527069367));
#42188=CARTESIAN_POINT('Ctrl Pts',(4.97778782502355,1.78279361519087,390.346399193907));
#42189=CARTESIAN_POINT('Ctrl Pts',(5.2254376041702,-0.807171945896316,390.267271318447));
#42190=CARTESIAN_POINT('Ctrl Pts',(4.2078353041098,-3.20169435749343,390.188143442988));
#42191=CARTESIAN_POINT('Ctrl Pts',(2.17137625543244,-4.82098017654731,390.109015567527));
#42192=CARTESIAN_POINT('Ctrl Pts',(-0.390845137002325,-5.27294649927341,
390.029887692068));
#42193=CARTESIAN_POINT('Ctrl Pts',(-2.85842993443779,-4.44815726062243,
389.950759816608));
#42194=CARTESIAN_POINT('Ctrl Pts',(-4.63389386243089,-2.54632134206259,
389.871631941148));
#42195=CARTESIAN_POINT('Ctrl Pts',(-5.2873381074052,-0.0279364152813674,
389.792504065688));
#42196=CARTESIAN_POINT('Ctrl Pts',(-4.66054210445731,2.49721284593419,389.713376190229));
#42197=CARTESIAN_POINT('Ctrl Pts',(-2.90527399360582,4.41770389765948,389.634248314769));
#42198=CARTESIAN_POINT('Ctrl Pts',(-0.446542510013585,5.2685220405792,389.55512043931));
#42199=CARTESIAN_POINT('Ctrl Pts',(2.12031175334316,4.84365593059135,389.475992563849));
#42200=CARTESIAN_POINT('Ctrl Pts',(4.17376808571255,3.24597977073262,389.39686468839));
#42201=CARTESIAN_POINT('Ctrl Pts',(5.21661647505316,0.862344048232485,389.31773681293));
#42202=CARTESIAN_POINT('Ctrl Pts',(4.99634867366186,-1.73009382303836,389.23860893747));
#42203=CARTESIAN_POINT('Ctrl Pts',(3.56629883549932,-3.90361849073832,389.15948106201));
#42204=CARTESIAN_POINT('Ctrl Pts',(1.27272954528402,-5.13194740911081,389.08035318655));
#42205=CARTESIAN_POINT('Ctrl Pts',(-1.3290098591728,-5.11766133107102,389.001225311091));
#42206=CARTESIAN_POINT('Ctrl Pts',(-3.60895181526604,-3.86421939082217,
388.922097435631));
#42207=CARTESIAN_POINT('Ctrl Pts',(-5.01504661559582,-1.67512153252199,
388.842969560171));
#42208=CARTESIAN_POINT('Ctrl Pts',(-5.20683198610126,0.919578911149497,
388.763841684712));
#42209=CARTESIAN_POINT('Ctrl Pts',(-4.13787031577727,3.29161874388992,388.684713809251));
#42210=CARTESIAN_POINT('Ctrl Pts',(-2.0669927453671,4.86664830205737,388.605585933792));
#42211=CARTESIAN_POINT('Ctrl Pts',(0.504372452470541,5.2633005932121,388.526458058332));
#42212=CARTESIAN_POINT('Ctrl Pts',(2.95361231985281,4.38553291736953,388.447330182872));
#42213=CARTESIAN_POINT('Ctrl Pts',(4.68768449948338,2.44588199605403,388.368202307412));
#42214=CARTESIAN_POINT('Ctrl Pts',(5.28671249546426,-0.0859982303311033,
388.289074431953));
#42215=CARTESIAN_POINT('Ctrl Pts',(4.60565172496217,-2.59705542753155,388.209946556493));
#42216=CARTESIAN_POINT('Ctrl Pts',(2.80940963137597,-4.47927920858367,388.130818681033));
#42217=CARTESIAN_POINT('Ctrl Pts',(0.332916112606594,-5.27692065197923,
388.051690805573));
#42218=CARTESIAN_POINT('Ctrl Pts',(-2.22418745944155,-4.79684425957118,
387.972562930114));
#42219=CARTESIAN_POINT('Ctrl Pts',(-4.24274134038657,-3.15529247834378,
387.893435054654));
#42220=CARTESIAN_POINT('Ctrl Pts',(-5.23398656144486,-0.749739541395986,
387.814307179194));
#42221=CARTESIAN_POINT('Ctrl Pts',(-4.95790971666796,1.83735025150007,387.735179303734));
#42222=CARTESIAN_POINT('Ctrl Pts',(-3.48135818389009,3.97955649548785,387.656051428275));
#42223=CARTESIAN_POINT('Ctrl Pts',(-1.16185415329344,5.15817987586638,387.576923552815));
#42224=CARTESIAN_POINT('Ctrl Pts',(1.43897337488296,5.0878365079566,387.497795677355));
#42225=CARTESIAN_POINT('Ctrl Pts',(3.69137763358211,3.7855588585581,387.418667801895));
#42226=CARTESIAN_POINT('Ctrl Pts',(5.04997670698908,1.56667161976776,387.339539926436));
#42227=CARTESIAN_POINT('Ctrl Pts',(5.1858086147589,-1.03155887685117,387.260412050976));
#42228=CARTESIAN_POINT('Ctrl Pts',(4.06598393848355,-3.38001469187811,387.181284175516));
#42229=CARTESIAN_POINT('Ctrl Pts',(1.96164944276588,-4.91005663602919,387.102156300056));
#42230=CARTESIAN_POINT('Ctrl Pts',(-0.617665566383616,-5.25121071310437,
387.023028424596));
#42231=CARTESIAN_POINT('Ctrl Pts',(-3.04742321760052,-4.32087218488899,
386.943900549136));
#42232=CARTESIAN_POINT('Ctrl Pts',(-4.73929844549354,-2.34430692313541,
386.864772673677));
#42233=CARTESIAN_POINT('Ctrl Pts',(-5.28363203833613,0.199892943312196,
386.785644798217));
#42234=CARTESIAN_POINT('Ctrl Pts',(-4.54862274572651,2.695692085973,386.706516922757));
#42235=CARTESIAN_POINT('Ctrl Pts',(-2.71224074091265,4.53877459989496,386.627389047297));
#42236=CARTESIAN_POINT('Ctrl Pts',(-0.219135128106394,5.28286896496098,
386.548261171838));
#42237=CARTESIAN_POINT('Ctrl Pts',(2.32703038082081,4.74780520999492,386.469133296378));
#42238=CARTESIAN_POINT('Ctrl Pts',(4.30974451002784,3.06314004962277,386.390005420918));
#42239=CARTESIAN_POINT('Ctrl Pts',(5.24892628554031,0.636786898642001,386.310877545458));
#42240=CARTESIAN_POINT('Ctrl Pts',(4.91716859158436,-1.94375352019086,386.231749669999));
#42241=CARTESIAN_POINT('Ctrl Pts',(3.39480098979053,-4.05364662310803,386.152621794539));
#42242=CARTESIAN_POINT('Ctrl Pts',(1.05043926306477,-5.18201718059,386.073493919079));
#42243=CARTESIAN_POINT('Ctrl Pts',(-1.54826871412865,-5.0556491862241,385.994366043619));
#42244=CARTESIAN_POINT('Ctrl Pts',(-3.772089388456,-3.70514053050835,385.91523816816));
#42245=CARTESIAN_POINT('Ctrl Pts',(-5.08256187967811,-1.45749423482943,
385.836110292699));
#42246=CARTESIAN_POINT('Ctrl Pts',(-5.16237725218749,1.14305984594648,385.75698241724));
#42247=CARTESIAN_POINT('Ctrl Pts',(-3.99220955212729,3.46684115546438,385.67785454178));
#42248=CARTESIAN_POINT('Ctrl Pts',(-1.85539526299902,4.95118502212943,385.59872666632));
#42249=CARTESIAN_POINT('Ctrl Pts',(0.73067187193628,5.23668247279509,385.51959879086));
#42250=CARTESIAN_POINT('Ctrl Pts',(3.13981906729605,4.25420508790564,385.440470915401));
#42251=CARTESIAN_POINT('Ctrl Pts',(4.78871173391359,2.24164328892807,385.361343039941));
#42252=CARTESIAN_POINT('Ctrl Pts',(5.27809816640793,-0.313694837508304,
385.282215164481));
#42253=CARTESIAN_POINT('Ctrl Pts',(4.48948164772799,-2.79307702006795,385.203087289022));
#42254=CARTESIAN_POINT('Ctrl Pts',(2.61381244185943,-4.59616244535579,385.123959413562));
#42255=CARTESIAN_POINT('Ctrl Pts',(0.105252389857621,-5.28636421747,385.044831538102));
#42256=CARTESIAN_POINT('Ctrl Pts',(-2.42879276314368,-4.69656155277656,
384.965703662642));
#42257=CARTESIAN_POINT('Ctrl Pts',(-4.3747464822184,-2.96956527485689,384.886575787182));
#42258=CARTESIAN_POINT('Ctrl Pts',(-5.26142871019096,-0.5235385686808,384.807447911723));
#42259=CARTESIAN_POINT('Ctrl Pts',(-4.87414421624611,2.04925422155296,384.728320036263));
#42260=CARTESIAN_POINT('Ctrl Pts',(-3.30666744538294,4.12585447040522,384.649192160803));
#42261=CARTESIAN_POINT('Ctrl Pts',(-0.93853660926441,5.20344825460853,384.570064285343));
#42262=CARTESIAN_POINT('Ctrl Pts',(1.65684512644118,5.02111431181428,384.490936409884));
#42263=CARTESIAN_POINT('Ctrl Pts',(3.85104960199139,3.62300174831864,384.411808534424));
#42264=CARTESIAN_POINT('Ctrl Pts',(5.11278700298303,1.34764007340457,384.332680658964));
#42265=CARTESIAN_POINT('Ctrl Pts',(5.13654877856401,-1.25403004379905,384.253552783504));
#42266=CARTESIAN_POINT('Ctrl Pts',(3.91658141328989,-3.55205781743347,384.174424908044));
#42267=CARTESIAN_POINT('Ctrl Pts',(1.74827954439566,-4.99001436270134,384.095297032584));
#42268=CARTESIAN_POINT('Ctrl Pts',(-0.843338895500463,-5.21972261836337,
384.016169157125));
#42269=CARTESIAN_POINT('Ctrl Pts',(-3.23075696562154,-4.18556258278454,
383.937041281665));
#42270=CARTESIAN_POINT('Ctrl Pts',(-4.8359014200548,-2.1379387645183,383.857913406205));
#42271=CARTESIAN_POINT('Ctrl Pts',(-5.27011344929143,0.427351069865941,
383.778785530745));
#42272=CARTESIAN_POINT('Ctrl Pts',(-4.42825589269063,2.88916500985471,383.699657655286));
#42273=CARTESIAN_POINT('Ctrl Pts',(-2.51417043865664,4.65141609735177,383.620529779826));
#42274=CARTESIAN_POINT('Ctrl Pts',(0.00867922154690349,5.28740478651213,
383.541401904366));
#42275=CARTESIAN_POINT('Ctrl Pts',(2.52942735381344,4.6431370825228,383.462274028906));
#42276=CARTESIAN_POINT('Ctrl Pts',(4.43771707378134,2.87461160478899,383.383146153446));
#42277=CARTESIAN_POINT('Ctrl Pts',(5.27148802998996,0.410047137522666,383.304018277987));
#42278=CARTESIAN_POINT('Ctrl Pts',(4.82885656869832,-2.15380336712922,383.224890402527));
#42279=CARTESIAN_POINT('Ctrl Pts',(3.2169984748157,-4.19614650820864,383.145762527067));
#42280=CARTESIAN_POINT('Ctrl Pts',(0.82619815304806,-5.22246314656389,383.066634651607));
#42281=CARTESIAN_POINT('Ctrl Pts',(-1.76465219517988,-4.98424792073636,
382.987506776148));
#42282=CARTESIAN_POINT('Ctrl Pts',(-3.92822160960685,-3.5391806525149,382.908378900688));
#42283=CARTESIAN_POINT('Ctrl Pts',(-5.14063804209515,-1.23716014544694,
382.829251025228));
#42284=CARTESIAN_POINT('Ctrl Pts',(-5.10833518714595,1.36441794223199,382.750123149768));
#42285=CARTESIAN_POINT('Ctrl Pts',(-3.83913463932894,3.63562510806912,382.670995274309));
#42286=CARTESIAN_POINT('Ctrl Pts',(-1.64035202533435,5.0265266276326,382.591867398849));
#42287=CARTESIAN_POINT('Ctrl Pts',(0.955614320991023,5.2003390249901,382.512739523389));
#42288=CARTESIAN_POINT('Ctrl Pts',(3.32019468624774,4.11497654315675,382.433611647929));
#42289=CARTESIAN_POINT('Ctrl Pts',(4.8808455917412,2.03324150432223,382.354483772469));
#42290=CARTESIAN_POINT('Ctrl Pts',(5.25968159463003,-0.540808864968189,
382.27535589701));
#42291=CARTESIAN_POINT('Ctrl Pts',(4.36497391033337,-2.98391143759783,382.19622802155));
#42292=CARTESIAN_POINT('Ctrl Pts',(2.41336099931917,-4.70450989926509,382.11710014609));
#42293=CARTESIAN_POINT('Ctrl Pts',(-0.122606802820077,-5.28599018890692,
382.03797227063));
#42294=CARTESIAN_POINT('Ctrl Pts',(-2.6288874239146,-4.58755660648474,381.958844395171));
#42295=CARTESIAN_POINT('Ctrl Pts',(-4.49862704479611,-2.77832313044165,
381.879716519711));
#42296=CARTESIAN_POINT('Ctrl Pts',(-5.27909957396784,-0.296365304059962,
381.800588644251));
#42297=CARTESIAN_POINT('Ctrl Pts',(-4.78132667791946,2.25735241031028,381.721460768791));
#42298=CARTESIAN_POINT('Ctrl Pts',(-3.12583571520092,4.26449009693918,381.642332893332));
#42299=CARTESIAN_POINT('Ctrl Pts',(-0.713476057932961,5.23905302703404,
381.563205017871));
#42300=CARTESIAN_POINT('Ctrl Pts',(1.87163986094335,4.94506713162178,381.484077142412));
#42301=CARTESIAN_POINT('Ctrl Pts',(4.00356957706116,3.45371616479241,381.404949266952));
#42302=CARTESIAN_POINT('Ctrl Pts',(5.16610206459392,1.12610575148009,381.325821391492));
#42303=CARTESIAN_POINT('Ctrl Pts',(5.07774957870228,-1.47417228345499,381.246693516033));
#42304=CARTESIAN_POINT('Ctrl Pts',(3.75990519207135,-3.71750422352859,381.167565640573));
#42305=CARTESIAN_POINT('Ctrl Pts',(1.53166282114666,-5.06070486272762,381.088437765113));
#42306=CARTESIAN_POINT('Ctrl Pts',(-1.0674460141586,-5.17854069330105,381.009309889653));
#42307=CARTESIAN_POINT('Ctrl Pts',(-3.40809069944175,-4.04247974511891,
380.930182014193));
#42308=CARTESIAN_POINT('Ctrl Pts',(-4.92352337948473,-1.92760012372517,
380.851054138734));
#42309=CARTESIAN_POINT('Ctrl Pts',(-5.24680744637695,0.654015539541282,
380.771926263274));
#42310=CARTESIAN_POINT('Ctrl Pts',(-4.29966508516876,3.07727230850615,380.692798387814));
#42311=CARTESIAN_POINT('Ctrl Pts',(-2.31143093395199,4.75541919738815,380.613670512354));
#42312=CARTESIAN_POINT('Ctrl Pts',(0.236477452546483,5.28212108151216,380.534542636895));
#42313=CARTESIAN_POINT('Ctrl Pts',(2.7271267899117,4.52984593303835,380.455414761435));
#42314=CARTESIAN_POINT('Ctrl Pts',(4.55744811217567,2.68074456264382,380.376286885975));
#42315=CARTESIAN_POINT('Ctrl Pts',(5.28425980776137,0.182545855597361,380.297159010515));
#42316=CARTESIAN_POINT('Ctrl Pts',(4.73157661405697,-2.35985326887651,380.218031135055));
#42317=CARTESIAN_POINT('Ctrl Pts',(3.03322149728047,-4.33085350176541,380.138903259596));
#42318=CARTESIAN_POINT('Ctrl Pts',(0.600422665576261,-5.25321019263273,
380.059775384136));
#42319=CARTESIAN_POINT('Ctrl Pts',(-1.97775844481349,-4.90359013777528,
379.980647508676));
#42320=CARTESIAN_POINT('Ctrl Pts',(-4.07705851709219,-3.36664796994342,
379.901519633216));
#42321=CARTESIAN_POINT('Ctrl Pts',(-5.18916724645199,-1.01452845877678,
379.822391757756));
#42322=CARTESIAN_POINT('Ctrl Pts',(-5.04480615543027,1.58324210386498,379.743263882297));
#42323=CARTESIAN_POINT('Ctrl Pts',(-3.67892986111526,3.7976571438602,379.664136006837));
#42324=CARTESIAN_POINT('Ctrl Pts',(-1.42226240084736,5.09253319757995,379.585008131377));
#42325=CARTESIAN_POINT('Ctrl Pts',(1.17878204679748,5.15433774518764,379.505880255918));
#42326=CARTESIAN_POINT('Ctrl Pts',(3.49440419135096,3.9681058520139,379.426752380457));
#42327=CARTESIAN_POINT('Ctrl Pts',(4.96391496617568,1.82106367650753,379.347624504998));
#42328=CARTESIAN_POINT('Ctrl Pts',(5.2314969825461,-0.766918526917405,379.268496629538));
#42329=CARTESIAN_POINT('Ctrl Pts',(4.23235974285854,-3.16920427116154,379.189368754078));
#42330=CARTESIAN_POINT('Ctrl Pts',(2.20842757301423,-4.80412035237133,379.110240878619));
#42331=CARTESIAN_POINT('Ctrl Pts',(-0.350238295746339,-5.27579926091873,
379.031113003158));
#42332=CARTESIAN_POINT('Ctrl Pts',(-2.82409983509395,-4.47003185970082,
378.951985127699));
#42333=CARTESIAN_POINT('Ctrl Pts',(-4.61415296279982,-2.58192121126957,
378.872857252239));
#42334=CARTESIAN_POINT('Ctrl Pts',(-5.28696633525482,-0.0686416433394937,
378.793729376779));
#42335=CARTESIAN_POINT('Ctrl Pts',(-4.67962947817872,2.46125834732535,378.71460150132));
#42336=CARTESIAN_POINT('Ctrl Pts',(-2.9391988257698,4.39520590733944,378.63547362586));
#42337=CARTESIAN_POINT('Ctrl Pts',(-0.487090471470337,5.2649280695866,378.5563457504));
#42338=CARTESIAN_POINT('Ctrl Pts',(2.08295867142411,4.85983619872698,378.47721787494));
#42339=CARTESIAN_POINT('Ctrl Pts',(4.1486543056634,3.27801649742928,378.398089999481));
#42340=CARTESIAN_POINT('Ctrl Pts',(5.20982287752563,0.902480077413658,378.318962124021));
#42341=CARTESIAN_POINT('Ctrl Pts',(5.00952021436078,-1.69157675771122,378.239834248561));
#42342=CARTESIAN_POINT('Ctrl Pts',(3.59624624674644,-3.8760466506584,378.160706373101));
#42343=CARTESIAN_POINT('Ctrl Pts',(1.31220156369858,-5.12199685294173,378.081578497641));
#42344=CARTESIAN_POINT('Ctrl Pts',(-1.28957072085835,-5.12774141910675,
378.002450622182));
#42345=CARTESIAN_POINT('Ctrl Pts',(-3.57909508295452,-3.89188939879962,
377.923322746722));
#42346=CARTESIAN_POINT('Ctrl Pts',(-5.00200159628448,-1.71368163206748,
377.844194871262));
#42347=CARTESIAN_POINT('Ctrl Pts',(-5.21375731243622,0.879465401443313,
377.765066995802));
#42348=CARTESIAN_POINT('Ctrl Pts',(-4.16308913613231,3.25966463764834,377.685939120343));
#42349=CARTESIAN_POINT('Ctrl Pts',(-2.1043987453421,4.85059075019948,377.606811244883));
#42350=CARTESIAN_POINT('Ctrl Pts',(0.463836508427624,5.26702766261653,377.527683369423));
#42351=CARTESIAN_POINT('Ctrl Pts',(2.91976153075723,4.40814216068722,377.448555493963));
#42352=CARTESIAN_POINT('Ctrl Pts',(4.66871526619766,2.48189896419878,377.369427618503));
#42353=CARTESIAN_POINT('Ctrl Pts',(5.28721789969248,-0.0452944421492617,
377.290299743044));
#42354=CARTESIAN_POINT('Ctrl Pts',(4.62550939154664,-2.56152055897115,377.211171867584));
#42355=CARTESIAN_POINT('Ctrl Pts',(2.84381135938942,-4.45751743210561,377.132043992124));
#42356=CARTESIAN_POINT('Ctrl Pts',(0.373532100567371,-5.27420121678766,
377.052916116664));
#42357=CARTESIAN_POINT('Ctrl Pts',(-2.18719169184094,-4.81382563128935,
376.973788241204));
#42358=CARTESIAN_POINT('Ctrl Pts',(-4.21832369780876,-3.18786290260816,
376.894660365745));
#42359=CARTESIAN_POINT('Ctrl Pts',(-5.2280593665279,-0.790012636213206,
376.815532490285));
#42360=CARTESIAN_POINT('Ctrl Pts',(-4.97190814025518,1.79912594061044,376.736404614825));
#42361=CARTESIAN_POINT('Ctrl Pts',(-3.51189274247934,3.95263634434836,376.657276739365));
#42362=CARTESIAN_POINT('Ctrl Pts',(-1.20153141562281,5.1490821475793,376.578148863906));
#42363=CARTESIAN_POINT('Ctrl Pts',(1.39976059245402,5.09876406487689,376.499020988446));
#42364=CARTESIAN_POINT('Ctrl Pts',(3.66212404867255,3.81386577598244,376.419893112986));
#42365=CARTESIAN_POINT('Ctrl Pts',(5.03776558457334,1.60550385251465,376.340765237526));
#42366=CARTESIAN_POINT('Ctrl Pts',(5.19359667332446,-0.99160390296118,376.261637362067));
#42367=CARTESIAN_POINT('Ctrl Pts',(4.09188543028651,-3.34861140308599,376.182509486607));
#42368=CARTESIAN_POINT('Ctrl Pts',(1.99939275591558,-4.89480881330613,376.103381611147));
#42369=CARTESIAN_POINT('Ctrl Pts',(-0.577219342064538,-5.2558103583336,
376.024253735687));
#42370=CARTESIAN_POINT('Ctrl Pts',(-3.01406745721832,-4.34420557675964,
375.945125860227));
#42371=CARTESIAN_POINT('Ctrl Pts',(-4.72110968654987,-2.38072426020005,
375.865997984768));
#42372=CARTESIAN_POINT('Ctrl Pts',(-5.28501438473626,0.159209483211192,
375.786870109308));
#42373=CARTESIAN_POINT('Ctrl Pts',(-4.56924148341307,2.66059337382158,375.707742233848));
#42374=CARTESIAN_POINT('Ctrl Pts',(-2.74710339271414,4.51775908713646,375.628614358388));
#42375=CARTESIAN_POINT('Ctrl Pts',(-0.25980027835232,5.28102544478076,375.549486482929));
#42376=CARTESIAN_POINT('Ctrl Pts',(2.29040909674433,4.76557955369675,375.470358607468));
#42377=CARTESIAN_POINT('Ctrl Pts',(4.28603436317887,3.09622956904483,375.391230732009));
#42378=CARTESIAN_POINT('Ctrl Pts',(5.24386820297344,0.677177255244125,375.312102856549));
#42379=CARTESIAN_POINT('Ctrl Pts',(4.93198748823577,-1.90583737857549,375.232974981089));
#42380=CARTESIAN_POINT('Ctrl Pts',(3.42590832840442,-4.02739560248487,375.153847105629));
#42381=CARTESIAN_POINT('Ctrl Pts',(1.09030376033057,-5.1737660638094,375.07471923017));
#42382=CARTESIAN_POINT('Ctrl Pts',(-1.50930126232148,-5.06744133910014,
374.99559135471));
#42383=CARTESIAN_POINT('Ctrl Pts',(-3.74345011231245,-3.7340250124542,374.91646347925));
#42384=CARTESIAN_POINT('Ctrl Pts',(-5.07118953303831,-1.49668421879837,
374.83733560379));
#42385=CARTESIAN_POINT('Ctrl Pts',(-5.17098566641861,1.10346413672945,374.758207728331));
#42386=CARTESIAN_POINT('Ctrl Pts',(-4.40267566674078,2.65797789149901,374.705455811358));
#42387=CARTESIAN_POINT('Ctrl Pts',(-3.85627053850387,3.29705846079003,374.679079852871));
#42388=CARTESIAN_POINT('Ctrl Pts',(-1.2650852794265,-4.72177922709115,400.106973382376));
#42389=CARTESIAN_POINT('Ctrl Pts',(-2.04760230627562,-4.51212292510067,
400.08059742389));
#42390=CARTESIAN_POINT('Ctrl Pts',(-3.50558628380115,-3.69634492177698,
400.027845506916));
#42391=CARTESIAN_POINT('Ctrl Pts',(-4.84423972345866,-1.57661725067267,
399.948717631457));
#42392=CARTESIAN_POINT('Ctrl Pts',(-5.0096862523777,0.92455742070055,399.869589755997));
#42393=CARTESIAN_POINT('Ctrl Pts',(-3.9622375540088,3.20202818303723,399.790461880537));
#42394=CARTESIAN_POINT('Ctrl Pts',(-1.95534398901843,4.70410781476347,399.711334005077));
#42395=CARTESIAN_POINT('Ctrl Pts',(0.524977181208032,5.06720185162811,399.632206129618));
#42396=CARTESIAN_POINT('Ctrl Pts',(2.87819629981243,4.2033413524507,399.553078254158));
#42397=CARTESIAN_POINT('Ctrl Pts',(4.53450261129871,2.32172008778426,399.473950378698));
#42398=CARTESIAN_POINT('Ctrl Pts',(5.09285792630992,-0.122070466194823,
399.394822503238));
#42399=CARTESIAN_POINT('Ctrl Pts',(4.41806180230403,-2.5363019515078,399.315694627778));
#42400=CARTESIAN_POINT('Ctrl Pts',(2.67350672576957,-4.3364112842173,399.236566752319));
#42401=CARTESIAN_POINT('Ctrl Pts',(0.281606541856066,-5.08653095966945,
399.157438876859));
#42402=CARTESIAN_POINT('Ctrl Pts',(-2.17847980551824,-4.60503265524259,
399.078311001399));
#42403=CARTESIAN_POINT('Ctrl Pts',(-4.1110838687323,-3.00850283765647,398.999183125939));
#42404=CARTESIAN_POINT('Ctrl Pts',(-5.04825788999868,-0.683514555327269,
398.920055250479));
#42405=CARTESIAN_POINT('Ctrl Pts',(-4.76308094287924,1.80697533276996,398.84092737502));
#42406=CARTESIAN_POINT('Ctrl Pts',(-3.32460382095413,3.85993643987858,398.76179949956));
#42407=CARTESIAN_POINT('Ctrl Pts',(-1.08112964449127,4.97827867803806,398.6826716241));
#42408=CARTESIAN_POINT('Ctrl Pts',(1.4241219451236,4.89121422375072,398.603543748641));
#42409=CARTESIAN_POINT('Ctrl Pts',(3.58454628917626,3.6198242774857,398.52441587318));
#42410=CARTESIAN_POINT('Ctrl Pts',(4.87703286664207,1.4719545906142,398.445287997721));
#42411=CARTESIAN_POINT('Ctrl Pts',(4.98862772878014,-1.03232421377308,398.366160122261));
#42412=CARTESIAN_POINT('Ctrl Pts',(3.89231005153748,-3.28664302317114,398.287032246801));
#42413=CARTESIAN_POINT('Ctrl Pts',(1.853534773828,-4.7451563452711,398.207904371342));
#42414=CARTESIAN_POINT('Ctrl Pts',(-0.634042863421179,-5.05470964015625,
398.128776495882));
#42415=CARTESIAN_POINT('Ctrl Pts',(-2.96809765493441,-4.14034976900372,
398.049648620422));
#42416=CARTESIAN_POINT('Ctrl Pts',(-4.58347737773795,-2.22347363975469,
397.970520744962));
#42417=CARTESIAN_POINT('Ctrl Pts',(-5.08904492375008,0.231779341134317,
397.891392869503));
#42418=CARTESIAN_POINT('Ctrl Pts',(-4.36238559065476,2.6309108417746,397.812264994043));
#42419=CARTESIAN_POINT('Ctrl Pts',(-2.57944774904339,4.39301140550268,397.733137118583));
#42420=CARTESIAN_POINT('Ctrl Pts',(-0.171939895328258,5.09141793327901,
397.654009243123));
#42421=CARTESIAN_POINT('Ctrl Pts',(2.27720032040928,4.55702299748958,397.574881367663));
#42422=CARTESIAN_POINT('Ctrl Pts',(4.17495466984747,2.91922136941339,397.495753492203));
#42423=CARTESIAN_POINT('Ctrl Pts',(5.06181376480896,0.574579245458329,397.416625616744));
#42424=CARTESIAN_POINT('Ctrl Pts',(4.72303954910339,-1.90918760642483,397.337497741284));
#42425=CARTESIAN_POINT('Ctrl Pts',(3.24066051742776,-3.93067669870034,397.258369865824));
#42426=CARTESIAN_POINT('Ctrl Pts',(0.973609891088484,-5.00041835038785,
397.179241990364));
#42427=CARTESIAN_POINT('Ctrl Pts',(-1.52918404181197,-4.85939256133815,
397.100114114905));
#42428=CARTESIAN_POINT('Ctrl Pts',(-3.66171170517574,-3.54174636120374,
397.020986239445));
#42429=CARTESIAN_POINT('Ctrl Pts',(-4.90761729027895,-1.36652567889375,
396.941858363985));
#42430=CARTESIAN_POINT('Ctrl Pts',(-4.965225654969,1.13957627834147,396.862730488525));
#42431=CARTESIAN_POINT('Ctrl Pts',(-3.82058789989522,3.3697489517908,396.783602613066));
#42432=CARTESIAN_POINT('Ctrl Pts',(-1.7508588605474,4.78399343115808,396.704474737606));
#42433=CARTESIAN_POINT('Ctrl Pts',(0.742811287950349,5.03987413428296,396.625346862146));
#42434=CARTESIAN_POINT('Ctrl Pts',(3.05662214087683,4.07543384031964,396.546218986686));
#42435=CARTESIAN_POINT('Ctrl Pts',(4.63032320548468,2.12419559167018,396.467091111227));
#42436=CARTESIAN_POINT('Ctrl Pts',(5.08286916176923,-0.341380994281065,
396.387963235767));
#42437=CARTESIAN_POINT('Ctrl Pts',(4.30468359613617,-2.72429789782194,396.308835360307));
#42438=CARTESIAN_POINT('Ctrl Pts',(2.48419109223004,-4.44757175503734,396.229707484847));
#42439=CARTESIAN_POINT('Ctrl Pts',(0.0621933781031742,-5.09394070270169,
396.150579609387));
#42440=CARTESIAN_POINT('Ctrl Pts',(-2.37486341947636,-4.50689734049423,
396.071451733928));
#42441=CARTESIAN_POINT('Ctrl Pts',(-4.23688686924074,-2.82858437317615,
395.992323858468));
#42442=CARTESIAN_POINT('Ctrl Pts',(-5.07301922112011,-0.46537713853058,
395.913195983008));
#42443=CARTESIAN_POINT('Ctrl Pts',(-4.68080504901513,2.01051336529637,395.834068107548));
#42444=CARTESIAN_POINT('Ctrl Pts',(-3.15521243681498,3.99959177635531,395.754940232089));
#42445=CARTESIAN_POINT('Ctrl Pts',(-0.865638049608238,5.0202361165578,395.675812356629));
#42446=CARTESIAN_POINT('Ctrl Pts',(1.63353607355812,4.82531447631191,395.596684481169));
#42447=CARTESIAN_POINT('Ctrl Pts',(3.73717683280492,3.46202386174144,395.517556605709));
#42448=CARTESIAN_POINT('Ctrl Pts',(4.93592289877338,1.26046223120153,395.43842873025));
#42449=CARTESIAN_POINT('Ctrl Pts',(4.93951801594962,-1.24629918921186,395.35930085479));
#42450=CARTESIAN_POINT('Ctrl Pts',(3.74709168700367,-3.45129016283895,395.28017297933));
#42451=CARTESIAN_POINT('Ctrl Pts',(1.64736994911874,-4.82060910566927,395.20104510387));
#42452=CARTESIAN_POINT('Ctrl Pts',(-0.851234793642623,-5.0226984007616,
395.12191722841));
#42453=CARTESIAN_POINT('Ctrl Pts',(-3.14372730731715,-4.00862551458096,
395.04278935295));
#42454=CARTESIAN_POINT('Ctrl Pts',(-4.67501897747406,-2.02393118933878,
394.963661477491));
#42455=CARTESIAN_POINT('Ctrl Pts',(-5.07433320772034,0.450824129730827,
394.884533602031));
#42456=CARTESIAN_POINT('Ctrl Pts',(-4.24498275416411,2.81641994662909,394.805405726571));
#42457=CARTESIAN_POINT('Ctrl Pts',(-2.38778091996604,4.50006690807671,394.726277851111));
#42458=CARTESIAN_POINT('Ctrl Pts',(0.0475820181493076,5.09409813906934,
394.647149975652));
#42459=CARTESIAN_POINT('Ctrl Pts',(2.47142376857538,4.45467893961412,394.568022100192));
#42460=CARTESIAN_POINT('Ctrl Pts',(4.29685170208089,2.73663394505832,394.488894224732));
#42461=CARTESIAN_POINT('Ctrl Pts',(5.08186905910887,0.355958937228547,394.409766349272));
#42462=CARTESIAN_POINT('Ctrl Pts',(4.63639705230557,-2.11090555740732,394.330638473812));
#42463=CARTESIAN_POINT('Ctrl Pts',(3.06829925703676,-4.06664967364888,394.251510598353));
#42464=CARTESIAN_POINT('Ctrl Pts',(0.757264255609957,-5.037722773843,394.172382722893));
#42465=CARTESIAN_POINT('Ctrl Pts',(-1.73712958511388,-4.78899579279863,
394.093254847433));
#42466=CARTESIAN_POINT('Ctrl Pts',(-3.81090663047816,-3.38069379753602,
394.014126971973));
#42467=CARTESIAN_POINT('Ctrl Pts',(-4.96193654859164,-1.15381349735189,
393.934999096513));
#42468=CARTESIAN_POINT('Ctrl Pts',(-4.91151674888844,1.35244339042685,393.855871221054));
#42469=CARTESIAN_POINT('Ctrl Pts',(-3.67185554026823,3.53122879325631,393.776743345594));
#42470=CARTESIAN_POINT('Ctrl Pts',(-1.54311609384367,4.85498636659688,393.697615470134));
#42471=CARTESIAN_POINT('Ctrl Pts',(0.959263034860399,5.00319041501234,393.618487594674));
#42472=CARTESIAN_POINT('Ctrl Pts',(3.22937270762551,3.93995581373248,393.539359719215));
#42473=CARTESIAN_POINT('Ctrl Pts',(4.71754393956094,1.92272698978111,393.460231843755));
#42474=CARTESIAN_POINT('Ctrl Pts',(5.06344102520928,-0.560057928386485,
393.381103968295));
#42475=CARTESIAN_POINT('Ctrl Pts',(4.18331078637565,-2.90723421201562,393.301976092835));
#42476=CARTESIAN_POINT('Ctrl Pts',(2.29026199958981,-4.55047248889121,393.222848217376));
#42477=CARTESIAN_POINT('Ctrl Pts',(-0.157335320049481,-5.0918901692776,
393.143720341916));
#42478=CARTESIAN_POINT('Ctrl Pts',(-2.5668365306344,-4.40039204207098,393.064592466456));
#42479=CARTESIAN_POINT('Ctrl Pts',(-4.35482132414875,-2.6434127815497,392.985464590996));
#42480=CARTESIAN_POINT('Ctrl Pts',(-5.08835916941954,-0.24637544907113,
392.906336715536));
#42481=CARTESIAN_POINT('Ctrl Pts',(-4.58983617949401,2.21031756639828,392.827208840077));
#42482=CARTESIAN_POINT('Ctrl Pts',(-2.97996133557448,4.13181925275079,392.748080964617));
#42483=CARTESIAN_POINT('Ctrl Pts',(-0.648538831649752,5.05287020244567,
392.668953089157));
#42484=CARTESIAN_POINT('Ctrl Pts',(1.83991647361136,4.75045337510584,392.589825213697));
#42485=CARTESIAN_POINT('Ctrl Pts',(3.88286686231846,3.29779393359108,392.510697338238));
#42486=CARTESIAN_POINT('Ctrl Pts',(4.98564616049109,1.04662899888231,392.431569462778));
#42487=CARTESIAN_POINT('Ctrl Pts',(4.88123485596325,-1.45795959472489,392.352441587318));
#42488=CARTESIAN_POINT('Ctrl Pts',(3.59491439502781,-3.60952772414103,392.273313711858));
#42489=CARTESIAN_POINT('Ctrl Pts',(1.43814570421584,-4.88710925111834,392.194185836399));
#42490=CARTESIAN_POINT('Ctrl Pts',(-1.06684584950233,-4.98135923542166,
392.115057960939));
#42491=CARTESIAN_POINT('Ctrl Pts',(-3.31351857300444,-3.86945662403335,
392.035930085479));
#42492=CARTESIAN_POINT('Ctrl Pts',(-4.75787834559899,-1.82062998640609,
391.956802210019));
#42493=CARTESIAN_POINT('Ctrl Pts',(-5.05019767193907,0.669031668355122,
391.877674334559));
#42494=CARTESIAN_POINT('Ctrl Pts',(-4.11969632968522,2.99669852506039,391.7985464591));
#42495=CARTESIAN_POINT('Ctrl Pts',(-2.19167961327856,4.59876509202852,391.71941858364));
#42496=CARTESIAN_POINT('Ctrl Pts',(0.267015564477117,5.08731781858062,391.64029070818));
#42497=CARTESIAN_POINT('Ctrl Pts',(2.66105740145502,4.34406185557737,391.56116283272));
#42498=CARTESIAN_POINT('Ctrl Pts',(4.4107688176863,2.54896416919641,391.48203495726));
#42499=CARTESIAN_POINT('Ctrl Pts',(5.09248653841822,0.136677558326831,391.402907081801));
#42500=CARTESIAN_POINT('Ctrl Pts',(4.54114405077152,-2.30870323105058,391.323779206341));
#42501=CARTESIAN_POINT('Ctrl Pts',(2.89023969147757,-4.1950702526571,391.244651330881));
#42502=CARTESIAN_POINT('Ctrl Pts',(0.539512263560586,-5.06567136877124,
391.165523455421));
#42503=CARTESIAN_POINT('Ctrl Pts',(-1.94184901073189,-4.70970512011533,
391.086395579962));
#42504=CARTESIAN_POINT('Ctrl Pts',(-3.95302411413336,-3.21336276383497,
391.007267704502));
#42505=CARTESIAN_POINT('Ctrl Pts',(-5.00704072509175,-0.93895850610853,
390.928139829042));
#42506=CARTESIAN_POINT('Ctrl Pts',(-4.84868639834328,1.56279880645007,390.849011953582));
#42507=CARTESIAN_POINT('Ctrl Pts',(-3.51630397832454,3.68615059797345,390.769884078122));
#42508=CARTESIAN_POINT('Ctrl Pts',(-1.33250752244617,4.91696284321382,390.690756202663));
#42509=CARTESIAN_POINT('Ctrl Pts',(1.17393328229752,4.95721499913359,390.611628327203));
#42510=CARTESIAN_POINT('Ctrl Pts',(3.39612583095411,3.79716068125213,390.532500451743));
#42511=CARTESIAN_POINT('Ctrl Pts',(4.79600346661011,1.71768758718946,390.453372576283));
#42512=CARTESIAN_POINT('Ctrl Pts',(5.03460929736123,-0.777694748500222,
390.374244700824));
#42513=CARTESIAN_POINT('Ctrl Pts',(4.05416892298729,-3.08477134368254,390.295116825364));
#42514=CARTESIAN_POINT('Ctrl Pts',(2.09207953702197,-4.64492229318153,390.215988949904));
#42515=CARTESIAN_POINT('Ctrl Pts',(-0.376571822235509,-5.08038321011508,
390.136861074444));
#42516=CARTESIAN_POINT('Ctrl Pts',(-2.75404263028444,-4.28571453663178,
390.057733198984));
#42517=CARTESIAN_POINT('Ctrl Pts',(-4.46466820389571,-2.45333196450126,
389.978605323525));
#42518=CARTESIAN_POINT('Ctrl Pts',(-5.09424924959213,-0.0269162023862396,
389.899477448065));
#42519=CARTESIAN_POINT('Ctrl Pts',(-4.49034327596192,2.40601686672071,389.820349572605));
#42520=CARTESIAN_POINT('Ctrl Pts',(-2.79917598631673,4.25637330324171,389.741221697145));
#42521=CARTESIAN_POINT('Ctrl Pts',(-0.430235177009337,5.07612032869441,
389.662093821686));
#42522=CARTESIAN_POINT('Ctrl Pts',(2.04287986486846,4.66676994897283,389.582965946226));
#42523=CARTESIAN_POINT('Ctrl Pts',(4.02134580893056,3.12743949324644,389.503838070766));
#42524=CARTESIAN_POINT('Ctrl Pts',(5.02611030798847,0.830852015014124,389.424710195306));
#42525=CARTESIAN_POINT('Ctrl Pts',(4.81388648966003,-1.66691234430295,389.345582319847));
#42526=CARTESIAN_POINT('Ctrl Pts',(3.43606079231419,-3.76106183549833,389.266454444386));
#42527=CARTESIAN_POINT('Ctrl Pts',(1.22625060082997,-4.94453328059232,389.187326568927));
#42528=CARTESIAN_POINT('Ctrl Pts',(-1.28047560800195,-4.93076891734271,
389.108198693467));
#42529=CARTESIAN_POINT('Ctrl Pts',(-3.4771561234157,-3.72310155546604,389.029070818007));
#42530=CARTESIAN_POINT('Ctrl Pts',(-4.8319015994811,-1.61394759265993,388.949942942547));
#42531=CARTESIAN_POINT('Ctrl Pts',(-5.01668313982022,0.88599671193773,388.870815067088));
#42532=CARTESIAN_POINT('Ctrl Pts',(-3.98675899344041,3.17141177193107,388.791687191628));
#42533=CARTESIAN_POINT('Ctrl Pts',(-1.99150801936634,4.68892265960108,388.712559316169));
#42534=CARTESIAN_POINT('Ctrl Pts',(0.485953221700427,5.07108956391423,388.633431440708));
#42535=CARTESIAN_POINT('Ctrl Pts',(2.84574904013097,4.2253771783729,388.554303565249));
#42536=CARTESIAN_POINT('Ctrl Pts',(4.51649445500228,2.35656057355938,388.475175689789));
#42537=CARTESIAN_POINT('Ctrl Pts',(5.09364648443963,-0.0828576518904476,
388.396047814329));
#42538=CARTESIAN_POINT('Ctrl Pts',(4.43745744402291,-2.50221328655385,388.316919938869));
#42539=CARTESIAN_POINT('Ctrl Pts',(2.70681250483858,-4.31569993889408,388.23779206341));
#42540=CARTESIAN_POINT('Ctrl Pts',(0.320758313989414,-5.08421223031922,
388.15866418795));
#42541=CARTESIAN_POINT('Ctrl Pts',(-2.14296212310374,-4.62166779830222,
388.07953631249));
#42542=CARTESIAN_POINT('Ctrl Pts',(-4.08780022204497,-3.04006401964993,
388.00040843703));
#42543=CARTESIAN_POINT('Ctrl Pts',(-5.04284605436382,-0.722359724035205,
387.921280561571));
#42544=CARTESIAN_POINT('Ctrl Pts',(-4.7768512889894,1.77025186394512,387.842152686111));
#42545=CARTESIAN_POINT('Ctrl Pts',(-3.35422209731677,3.83422665224591,387.763024810651));
#42546=CARTESIAN_POINT('Ctrl Pts',(-1.11942427896961,4.96980776112863,387.683896935191));
#42547=CARTESIAN_POINT('Ctrl Pts',(1.38642335448793,4.90203327008818,387.604769059731));
#42548=CARTESIAN_POINT('Ctrl Pts',(3.55657182458215,3.64731363547327,387.525641184271));
#42549=CARTESIAN_POINT('Ctrl Pts',(4.86555607518393,1.50945817370396,387.446513308812));
#42550=CARTESIAN_POINT('Ctrl Pts',(4.99642752319251,-0.993887269465375,
387.367385433352));
#42551=CARTESIAN_POINT('Ctrl Pts',(3.9174978423384,-3.25657957897469,387.288257557892));
#42552=CARTESIAN_POINT('Ctrl Pts',(1.89001175993966,-4.73074576004784,387.209129682432));
#42553=CARTESIAN_POINT('Ctrl Pts',(-0.595108972441489,-5.05944119541285,
387.130001806973));
#42554=CARTESIAN_POINT('Ctrl Pts',(-2.93613404781291,-4.1630777979993,387.050873931513));
#42555=CARTESIAN_POINT('Ctrl Pts',(-4.5662235058762,-2.2586949314382,386.971746056053));
#42556=CARTESIAN_POINT('Ctrl Pts',(-5.09067852285014,0.192593031839733,
386.892618180593));
#42557=CARTESIAN_POINT('Ctrl Pts',(-4.38251111209279,2.59724782246595,386.813490305134));
#42558=CARTESIAN_POINT('Ctrl Pts',(-2.61319213533106,4.37302261173721,386.734362429674));
#42559=CARTESIAN_POINT('Ctrl Pts',(-0.211132509258637,5.08994331623203,
386.655234554214));
#42560=CARTESIAN_POINT('Ctrl Pts',(2.24204931299394,4.57441961094785,386.576106678754));
#42561=CARTESIAN_POINT('Ctrl Pts',(4.15235649586965,2.95127691518944,386.496978803295));
#42562=CARTESIAN_POINT('Ctrl Pts',(5.05724019309986,0.613532010751077,386.417850927834));
#42563=CARTESIAN_POINT('Ctrl Pts',(4.73759799334825,-1.872769380448,386.338723052375));
#42564=CARTESIAN_POINT('Ctrl Pts',(3.27082589451466,-3.90561107468386,386.259595176915));
#42565=CARTESIAN_POINT('Ctrl Pts',(1.01207816086419,-4.99277454880777,386.180467301455));
#42566=CARTESIAN_POINT('Ctrl Pts',(-1.49172732571618,-4.87102140055169,
386.101339425996));
#42567=CARTESIAN_POINT('Ctrl Pts',(-3.63433605836998,-3.56983211282445,
386.022211550536));
#42568=CARTESIAN_POINT('Ctrl Pts',(-4.89695126651592,-1.40426784919727,
385.943083675076));
#42569=CARTESIAN_POINT('Ctrl Pts',(-4.97385185302132,1.10131632291422,385.863955799616));
#42570=CARTESIAN_POINT('Ctrl Pts',(-3.84641763057586,3.34023521778273,385.784827924157));
#42571=CARTESIAN_POINT('Ctrl Pts',(-1.78763788776658,4.77037217427974,385.705700048697));
#42572=CARTESIAN_POINT('Ctrl Pts',(0.703988388806892,5.0454435134432,385.626572173237));
#42573=CARTESIAN_POINT('Ctrl Pts',(3.02515568373168,4.09884532375971,385.547444297777));
#42574=CARTESIAN_POINT('Ctrl Pts',(4.61383226520657,2.15978048131279,385.468316422317));
#42575=CARTESIAN_POINT('Ctrl Pts',(5.08534674297434,-0.302238982663029,
385.389188546858));
#42576=CARTESIAN_POINT('Ctrl Pts',(4.32552979408761,-2.69107634588493,385.310060671397));
#42577=CARTESIAN_POINT('Ctrl Pts',(2.51835834970871,-4.42831470441898,385.230932795938));
#42578=CARTESIAN_POINT('Ctrl Pts',(0.10140866673516,-5.09331092524616,385.151804920478));
#42579=CARTESIAN_POINT('Ctrl Pts',(-2.34009542414748,-4.5250473262503,385.072677045019));
#42580=CARTESIAN_POINT('Ctrl Pts',(-4.21498465418432,-2.86111940748926,
384.993549169558));
#42581=CARTESIAN_POINT('Ctrl Pts',(-5.06928604038651,-0.504419408492031,
384.914421294099));
#42582=CARTESIAN_POINT('Ctrl Pts',(-4.69614482970923,1.97441729057362,384.835293418639));
#42583=CARTESIAN_POINT('Ctrl Pts',(-3.18591090830761,3.97518195599239,384.756165543179));
#42584=CARTESIAN_POINT('Ctrl Pts',(-0.904262091876385,5.01342297917464,
384.677037667719));
#42585=CARTESIAN_POINT('Ctrl Pts',(1.59633862457976,4.83774770886161,384.59790979226));
#42586=CARTESIAN_POINT('Ctrl Pts',(3.71041271554213,3.4906929654818,384.5187819168));
#42587=CARTESIAN_POINT('Ctrl Pts',(4.92607259535609,1.29842546347592,384.43965404134));
#42588=CARTESIAN_POINT('Ctrl Pts',(4.94896661214932,-1.20823398841131,384.360526165881));
#42589=CARTESIAN_POINT('Ctrl Pts',(3.77355136371449,-3.42233984348858,384.281398290421));
#42590=CARTESIAN_POINT('Ctrl Pts',(1.6844339393846,-4.80778350206934,384.202270414961));
#42591=CARTESIAN_POINT('Ctrl Pts',(-0.812540913458525,-5.02910301772363,
384.123142539501));
#42592=CARTESIAN_POINT('Ctrl Pts',(-3.11277261136022,-4.03270958152043,
384.044014664041));
#42593=CARTESIAN_POINT('Ctrl Pts',(-4.65929862622416,-2.05986315336399,
383.964886788582));
#42594=CARTESIAN_POINT('Ctrl Pts',(-5.07765362058409,0.411744591087888,
383.885758913121));
#42595=CARTESIAN_POINT('Ctrl Pts',(-4.26653994885377,2.78365528824167,383.806631037662));
#42596=CARTESIAN_POINT('Ctrl Pts',(-2.42235518332661,4.48155054247207,383.727503162202));
#42597=CARTESIAN_POINT('Ctrl Pts',(0.00836226414014005,5.09431349363773,
383.648375286742));
#42598=CARTESIAN_POINT('Ctrl Pts',(2.43705492959019,4.47357386985853,383.569247411283));
#42599=CARTESIAN_POINT('Ctrl Pts',(4.27565561607469,2.76963336050998,383.490119535823));
#42600=CARTESIAN_POINT('Ctrl Pts',(5.07897800282517,0.39507258287429,383.410991660363));
#42601=CARTESIAN_POINT('Ctrl Pts',(4.65251104653713,-2.07514839487948,383.331863784903));
#42602=CARTESIAN_POINT('Ctrl Pts',(3.09951656833074,-4.04290699145606,383.252735909444));
#42603=CARTESIAN_POINT('Ctrl Pts',(0.79602613558697,-5.03174346428585,383.173608033984));
#42604=CARTESIAN_POINT('Ctrl Pts',(-1.70020867560859,-4.80222764540647,
383.094480158524));
#42605=CARTESIAN_POINT('Ctrl Pts',(-3.78476647047488,-3.40993294111337,
383.015352283064));
#42606=CARTESIAN_POINT('Ctrl Pts',(-4.9529065394344,-1.1919801636558,382.936224407604));
#42607=CARTESIAN_POINT('Ctrl Pts',(-4.92178335585094,1.31459061954267,382.857096532145));
#42608=CARTESIAN_POINT('Ctrl Pts',(-3.6989328766574,3.50285533142662,382.777968656685));
#42609=CARTESIAN_POINT('Ctrl Pts',(-1.58044783677119,4.84296237174792,382.698840781225));
#42610=CARTESIAN_POINT('Ctrl Pts',(0.920716140847871,5.01042729584046,382.619712905765));
#42611=CARTESIAN_POINT('Ctrl Pts',(3.19894414643704,3.96470128091602,382.540585030306));
#42612=CARTESIAN_POINT('Ctrl Pts',(4.70260147696606,1.95898934345174,382.461457154846));
#42613=CARTESIAN_POINT('Ctrl Pts',(5.06760272792295,-0.521059009008414,
382.382329279386));
#42614=CARTESIAN_POINT('Ctrl Pts',(4.20556896788232,-2.87494166120048,382.303201403926));
#42615=CARTESIAN_POINT('Ctrl Pts',(2.32522721453312,-4.53270540623539,382.224073528466));
#42616=CARTESIAN_POINT('Ctrl Pts',(-0.118129312060885,-5.0929505558716,
382.144945653006));
#42617=CARTESIAN_POINT('Ctrl Pts',(-2.53288280690479,-4.42002314308501,
382.065817777547));
#42618=CARTESIAN_POINT('Ctrl Pts',(-4.33434120943595,-2.67686125510947,
381.986689902087));
#42619=CARTESIAN_POINT('Ctrl Pts',(-5.08631158002599,-0.285542308273818,
381.907562026627));
#42620=CARTESIAN_POINT('Ctrl Pts',(-4.60671690485093,2.17491591963496,381.828434151168));
#42621=CARTESIAN_POINT('Ctrl Pts',(-3.01168299114604,4.10875473346396,381.749306275708));
#42622=CARTESIAN_POINT('Ctrl Pts',(-0.687420550548197,5.04772749716196,
381.670178400248));
#42623=CARTESIAN_POINT('Ctrl Pts',(1.80328924752583,4.76447770366057,381.591050524788));
#42624=CARTESIAN_POINT('Ctrl Pts',(3.85736279756143,3.32758954002893,381.511922649328));
#42625=CARTESIAN_POINT('Ctrl Pts',(4.97744063861076,1.0849813768112,381.432794773869));
#42626=CARTESIAN_POINT('Ctrl Pts',(4.89231470646681,-1.42033683040663,381.353666898409));
#42627=CARTESIAN_POINT('Ctrl Pts',(3.62259681793774,-3.58174429483572,381.274539022949));
#42628=CARTESIAN_POINT('Ctrl Pts',(1.47572786509085,-4.87589244827193,381.195411147489));
#42629=CARTESIAN_POINT('Ctrl Pts',(-1.02846384062172,-4.98942501972467,
381.11628327203));
#42630=CARTESIAN_POINT('Ctrl Pts',(-3.28363027585792,-3.89485200108939,
381.03715539657));
#42631=CARTESIAN_POINT('Ctrl Pts',(-4.74372071007927,-1.85720589157097,
380.95802752111));
#42632=CARTESIAN_POINT('Ctrl Pts',(-5.05519873204731,0.630131477096863,
380.87889964565));
#42633=CARTESIAN_POINT('Ctrl Pts',(-4.14264516258972,2.96489307662063,380.79977177019));
#42634=CARTESIAN_POINT('Ctrl Pts',(-2.22701954397005,4.58175554233269,380.720643894731));
#42635=CARTESIAN_POINT('Ctrl Pts',(0.227841507524015,5.08922274481773,380.641516019271));
#42636=CARTESIAN_POINT('Ctrl Pts',(2.6275345591372,4.36442001180692,380.562388143811));
#42637=CARTESIAN_POINT('Ctrl Pts',(4.39101418405409,2.58284616931722,380.483260268351));
#42638=CARTESIAN_POINT('Ctrl Pts',(5.09128336669755,0.175879444250141,380.404132392892));
#42639=CARTESIAN_POINT('Ctrl Pts',(4.55878366881602,-2.27367353854006,380.325004517432));
#42640=CARTESIAN_POINT('Ctrl Pts',(2.92245096161458,-4.17269460611234,380.245876641972));
#42641=CARTESIAN_POINT('Ctrl Pts',(0.578495766946718,-5.0613676557375,380.166748766512));
#42642=CARTESIAN_POINT('Ctrl Pts',(-1.90553247564304,-4.72451541252546,
380.087620891052));
#42643=CARTESIAN_POINT('Ctrl Pts',(-3.92816798724318,-3.24370099776764,
380.008493015593));
#42644=CARTESIAN_POINT('Ctrl Pts',(-4.99966350066068,-0.977478787024238,
379.929365140133));
#42645=CARTESIAN_POINT('Ctrl Pts',(-4.86057434754265,1.52542351854533,379.850237264673));
#42646=CARTESIAN_POINT('Ctrl Pts',(-3.54457863363044,3.65897010221885,379.771109389213));
#42647=CARTESIAN_POINT('Ctrl Pts',(-1.37032265027505,4.90655844080798,379.691981513754));
#42648=CARTESIAN_POINT('Ctrl Pts',(1.13573398094598,4.96610594162524,379.612853638294));
#42649=CARTESIAN_POINT('Ctrl Pts',(3.36679167625567,3.82319417602828,379.533725762834));
#42650=CARTESIAN_POINT('Ctrl Pts',(4.78263723215717,1.75456006010191,379.454597887374));
#42651=CARTESIAN_POINT('Ctrl Pts',(5.04044739265935,-0.738911348373108,
379.375470011914));
#42652=CARTESIAN_POINT('Ctrl Pts',(4.07779775117163,-3.05346776623899,379.296342136454));
#42653=CARTESIAN_POINT('Ctrl Pts',(2.1277777736305,-4.62867817470224,379.217214260995));
#42654=CARTESIAN_POINT('Ctrl Pts',(-0.337447906496721,-5.0831317914571,
379.138086385535));
#42655=CARTESIAN_POINT('Ctrl Pts',(-2.72096623545812,-4.30679029492008,
379.058958510076));
#42656=CARTESIAN_POINT('Ctrl Pts',(-4.44564822425965,-2.48763175833121,
378.979830634615));
#42657=CARTESIAN_POINT('Ctrl Pts',(-5.09389105422811,-0.0661349119291711,
378.900702759156));
#42658=CARTESIAN_POINT('Ctrl Pts',(-4.50873359586993,2.37137539423742,378.821574883696));
#42659=CARTESIAN_POINT('Ctrl Pts',(-2.83186191395806,4.23469691940223,378.742447008236));
#42660=CARTESIAN_POINT('Ctrl Pts',(-0.469302363186489,5.07265760630743,
378.663319132776));
#42661=CARTESIAN_POINT('Ctrl Pts',(2.00689088408632,4.68235932819045,378.584191257317));
#42662=CARTESIAN_POINT('Ctrl Pts',(3.99714916166288,3.15830626734308,378.505063381856));
#42663=CARTESIAN_POINT('Ctrl Pts',(5.01956480656533,0.869522312313901,378.425935506397));
#42664=CARTESIAN_POINT('Ctrl Pts',(4.82657701747544,-1.62980188774553,378.346807630937));
#42665=CARTESIAN_POINT('Ctrl Pts',(3.46491455089248,-3.73449689435332,378.267679755478));
#42666=CARTESIAN_POINT('Ctrl Pts',(1.26428113644233,-4.93494610983311,378.188551880018));
#42667=CARTESIAN_POINT('Ctrl Pts',(-1.24247675173787,-4.94048088958068,
378.109424004558));
#42668=CARTESIAN_POINT('Ctrl Pts',(-3.4483897322594,-3.74976107950479,378.030296129098));
#42669=CARTESIAN_POINT('Ctrl Pts',(-4.81933297260539,-1.65109951186456,
377.951168253638));
#42670=CARTESIAN_POINT('Ctrl Pts',(-5.02335555943258,0.847348111721862,
377.872040378178));
#42671=CARTESIAN_POINT('Ctrl Pts',(-4.01105684503597,3.1406246010644,377.792912502719));
#42672=CARTESIAN_POINT('Ctrl Pts',(-2.02754798568437,4.67345151517251,377.713784627259));
#42673=CARTESIAN_POINT('Ctrl Pts',(0.44689761407191,5.07468052407812,377.634656751799));
#42674=CARTESIAN_POINT('Ctrl Pts',(2.81313445157142,4.24716075235008,377.555528876339));
#42675=CARTESIAN_POINT('Ctrl Pts',(4.49821796114695,2.39126223424701,377.47640100088));
#42676=CARTESIAN_POINT('Ctrl Pts',(5.09413343175754,-0.043640329640808,
377.39727312542));
#42677=CARTESIAN_POINT('Ctrl Pts',(4.4565899263877,-2.46797611960502,377.31814524996));
#42678=CARTESIAN_POINT('Ctrl Pts',(2.73995791251956,-4.29473288302567,377.2390173745));
#42679=CARTESIAN_POINT('Ctrl Pts',(0.35989104240352,-5.08159210646814,377.159889499041));
#42680=CARTESIAN_POINT('Ctrl Pts',(-2.10731740784078,-4.63802902551619,
377.080761623581));
#42681=CARTESIAN_POINT('Ctrl Pts',(-4.06427428993092,-3.07144500115654,
377.001633748121));
#42682=CARTESIAN_POINT('Ctrl Pts',(-5.03713531530297,-0.761162081456616,
376.922505872661));
#42683=CARTESIAN_POINT('Ctrl Pts',(-4.79033850266972,1.73342347069504,376.843377997201));
#42684=CARTESIAN_POINT('Ctrl Pts',(-3.38364156114149,3.8082896009442,376.764250121742));
#42685=CARTESIAN_POINT('Ctrl Pts',(-1.15765256317261,4.96104227374008,376.685122246282));
#42686=CARTESIAN_POINT('Ctrl Pts',(1.3486425877949,4.91256176240515,376.605994370822));
#42687=CARTESIAN_POINT('Ctrl Pts',(3.52838655442424,3.67458680959566,376.526866495362));
#42688=CARTESIAN_POINT('Ctrl Pts',(4.85379089203517,1.5468722880489,376.447738619903));
#42689=CARTESIAN_POINT('Ctrl Pts',(5.00393116882618,-0.955391415479512,
376.368610744443));
#42690=CARTESIAN_POINT('Ctrl Pts',(3.94245343483129,-3.22632311019696,376.289482868983));
#42691=CARTESIAN_POINT('Ctrl Pts',(1.92637672105698,-4.71605477417046,376.210354993523));
#42692=CARTESIAN_POINT('Ctrl Pts',(-0.556139808052753,-5.06387286571299,
376.131227118063));
#42693=CARTESIAN_POINT('Ctrl Pts',(-2.90399640996096,-4.18555907527208,
376.052099242604));
#42694=CARTESIAN_POINT('Ctrl Pts',(-4.54869898413812,-2.29378233993093,
375.972971367144));
#42695=CARTESIAN_POINT('Ctrl Pts',(-5.09201038719634,0.153395295307603,
375.893843491684));
#42696=CARTESIAN_POINT('Ctrl Pts',(-4.40237687192385,2.56343088388421,375.814715616224));
#42697=CARTESIAN_POINT('Ctrl Pts',(-2.64678163427568,4.35277456670489,375.735587740765));
#42698=CARTESIAN_POINT('Ctrl Pts',(-0.250312604595216,5.08816711975964,
375.656459865305));
#42699=CARTESIAN_POINT('Ctrl Pts',(2.2067654054518,4.59154485151799,375.577331989845));
#42700=CARTESIAN_POINT('Ctrl Pts',(4.12951222237333,2.98315803496294,375.498204114385));
#42701=CARTESIAN_POINT('Ctrl Pts',(5.05236682718355,0.652447347661906,375.419076238925));
#42702=CARTESIAN_POINT('Ctrl Pts',(4.75187571715042,-1.83623790240596,375.339948363465));
#42703=CARTESIAN_POINT('Ctrl Pts',(3.30079722094991,-3.88031871785061,375.260820488006));
#42704=CARTESIAN_POINT('Ctrl Pts',(1.05048684235124,-4.98482475543083,375.181692612546));
#42705=CARTESIAN_POINT('Ctrl Pts',(-1.45418293039009,-4.88238291455355,
375.102564737087));
#42706=CARTESIAN_POINT('Ctrl Pts',(-3.60674266297149,-3.59766175932869,
375.023436861626));
#42707=CARTESIAN_POINT('Ctrl Pts',(-4.8859942278021,-1.44202665000967,374.944308986167));
#42708=CARTESIAN_POINT('Ctrl Pts',(-4.98214589566551,1.06316661357685,374.865181110707));
#42709=CARTESIAN_POINT('Ctrl Pts',(-4.24189388987242,2.56091091663634,374.812429193734));
#42710=CARTESIAN_POINT('Ctrl Pts',(-3.71544298812364,3.17665283523617,374.786053235247));
#42711=CARTESIAN_POINT('Ctrl Pts',(-1.21713437249744,-4.54280821229883,
400.213946764753));
#42712=CARTESIAN_POINT('Ctrl Pts',(-1.96999142168732,-4.34109857602909,
400.187570806266));
#42713=CARTESIAN_POINT('Ctrl Pts',(-3.37271299505139,-3.55624125113577,
400.134818889293));
#42714=CARTESIAN_POINT('Ctrl Pts',(-4.66062705172882,-1.51685825396376,
400.055691013833));
#42715=CARTESIAN_POINT('Ctrl Pts',(-4.81980261122079,0.889513643374588,
399.976563138373));
#42716=CARTESIAN_POINT('Ctrl Pts',(-3.81205567514826,3.08066074806192,399.897435262913));
#42717=CARTESIAN_POINT('Ctrl Pts',(-1.8812299991108,4.52580660481483,399.818307387454));
#42718=CARTESIAN_POINT('Ctrl Pts',(0.505078813591743,4.87513817945551,399.739179511994));
#42719=CARTESIAN_POINT('Ctrl Pts',(2.76910316187124,4.04402084397575,399.660051636534));
#42720=CARTESIAN_POINT('Ctrl Pts',(4.36262999826625,2.23371923467566,399.580923761074));
#42721=CARTESIAN_POINT('Ctrl Pts',(4.89982180424067,-0.117443592687962,
399.501795885615));
#42722=CARTESIAN_POINT('Ctrl Pts',(4.25060268019241,-2.44016773763421,399.422668010155));
#42723=CARTESIAN_POINT('Ctrl Pts',(2.57217199816948,-4.17204698619159,399.343540134695));
#42724=CARTESIAN_POINT('Ctrl Pts',(0.270932724605363,-4.89373465051516,
399.264412259235));
#42725=CARTESIAN_POINT('Ctrl Pts',(-2.09590823180696,-4.43048672079232,
399.185284383776));
#42726=CARTESIAN_POINT('Ctrl Pts',(-3.95526022334416,-2.89447065191351,
399.106156508316));
#42727=CARTESIAN_POINT('Ctrl Pts',(-4.85691225648777,-0.657607098051338,
399.027028632856));
#42728=CARTESIAN_POINT('Ctrl Pts',(-4.58254445676102,1.73848500455744,398.947900757396));
#42729=CARTESIAN_POINT('Ctrl Pts',(-3.1985903647966,3.71363211084189,398.868772881936));
#42730=CARTESIAN_POINT('Ctrl Pts',(-1.0401512631882,4.78958548759503,398.789645006477));
#42731=CARTESIAN_POINT('Ctrl Pts',(1.37014302373642,4.70582106344184,398.710517131017));
#42732=CARTESIAN_POINT('Ctrl Pts',(3.44868015565118,3.48262099178473,398.631389255557));
#42733=CARTESIAN_POINT('Ctrl Pts',(4.69217722656672,1.41616265411303,398.552261380097));
#42734=CARTESIAN_POINT('Ctrl Pts',(4.79954227516165,-0.993195719354361,
398.473133504638));
#42735=CARTESIAN_POINT('Ctrl Pts',(3.74477865578454,-3.16206840652194,398.394005629178));
#42736=CARTESIAN_POINT('Ctrl Pts',(1.78327968915111,-4.56529926055421,398.314877753718));
#42737=CARTESIAN_POINT('Ctrl Pts',(-0.610010546527312,-4.8631194640233,
398.235749878258));
#42738=CARTESIAN_POINT('Ctrl Pts',(-2.85559695895555,-3.9834168494165,398.156622002799));
#42739=CARTESIAN_POINT('Ctrl Pts',(-4.40974845943849,-2.13919665124415,
398.077494127339));
#42740=CARTESIAN_POINT('Ctrl Pts',(-4.89615332706093,0.22299413922299,397.998366251879));
#42741=CARTESIAN_POINT('Ctrl Pts',(-4.19703678069868,2.53119063874627,397.919238376419));
#42742=CARTESIAN_POINT('Ctrl Pts',(-2.48167816706011,4.22650177609728,397.840110500959));
#42743=CARTESIAN_POINT('Ctrl Pts',(-0.165422805885864,4.89843639169769,
397.7609826255));
#42744=CARTESIAN_POINT('Ctrl Pts',(2.19088691340144,4.38429678750219,397.68185475004));
#42745=CARTESIAN_POINT('Ctrl Pts',(4.01671011032052,2.80857324594973,397.60272687458));
#42746=CARTESIAN_POINT('Ctrl Pts',(4.86995431890775,0.55280079591789,397.52359899912));
#42747=CARTESIAN_POINT('Ctrl Pts',(4.54402076394769,-1.83682309573565,397.444471123661));
#42748=CARTESIAN_POINT('Ctrl Pts',(3.11782878949058,-3.78169108040825,397.365343248201));
#42749=CARTESIAN_POINT('Ctrl Pts',(0.93670686325944,-4.81088599330085,397.286215372741));
#42750=CARTESIAN_POINT('Ctrl Pts',(-1.47122292025061,-4.67520554704762,
397.207087497281));
#42751=CARTESIAN_POINT('Ctrl Pts',(-3.52292074773491,-3.40750248619052,
397.127959621821));
#42752=CARTESIAN_POINT('Ctrl Pts',(-4.72160239961778,-1.31472984606697,
397.048831746362));
#42753=CARTESIAN_POINT('Ctrl Pts',(-4.77702721717586,1.09638257673893,396.969703870902));
#42754=CARTESIAN_POINT('Ctrl Pts',(-3.67577501037587,3.24202434619358,396.890575995442));
#42755=CARTESIAN_POINT('Ctrl Pts',(-1.68449553181902,4.60266429272193,396.811448119982));
#42756=CARTESIAN_POINT('Ctrl Pts',(0.714656288826095,4.84884627278046,396.732320244522));
#42757=CARTESIAN_POINT('Ctrl Pts',(2.94076607474594,3.92096144865504,396.653192369063));
#42758=CARTESIAN_POINT('Ctrl Pts',(4.45481867572026,2.0436815688041,396.574064493603));
#42759=CARTESIAN_POINT('Ctrl Pts',(4.89021164683945,-0.328441528025053,
396.494936618143));
#42760=CARTESIAN_POINT('Ctrl Pts',(4.14152188219155,-2.62103801718789,396.415808742683));
#42761=CARTESIAN_POINT('Ctrl Pts',(2.39003205189126,-4.27899410833295,396.336680867224));
#42762=CARTESIAN_POINT('Ctrl Pts',(0.0598360438320979,-4.90086353983399,
396.257552991764));
#42763=CARTESIAN_POINT('Ctrl Pts',(-2.28484825872123,-4.33607105832391,
396.178425116304));
#42764=CARTESIAN_POINT('Ctrl Pts',(-4.07629487497772,-2.72137169097608,
396.099297240844));
#42765=CARTESIAN_POINT('Ctrl Pts',(-4.88073505144618,-0.447737809214611,
396.020169365385));
#42766=CARTESIAN_POINT('Ctrl Pts',(-4.50338709078854,1.93430827396637,395.941041489924));
#42767=CARTESIAN_POINT('Ctrl Pts',(-3.03561947311557,3.84799404919722,395.861913614465));
#42768=CARTESIAN_POINT('Ctrl Pts',(-0.832827510883269,4.82995260073343,
395.782785739005));
#42769=CARTESIAN_POINT('Ctrl Pts',(1.57161966562715,4.64241913390311,395.703657863545));
#42770=CARTESIAN_POINT('Ctrl Pts',(3.5955254979886,3.3308017325457,395.624529988085));
#42771=CARTESIAN_POINT('Ctrl Pts',(4.74883513214048,1.21268655305647,395.545402112626));
#42772=CARTESIAN_POINT('Ctrl Pts',(4.75229398251168,-1.19906033709689,395.466274237166));
#42773=CARTESIAN_POINT('Ctrl Pts',(3.60506454649375,-3.32047487625331,395.387146361706));
#42774=CARTESIAN_POINT('Ctrl Pts',(1.5849291916516,-4.63789211233576,395.308018486247));
#42775=CARTESIAN_POINT('Ctrl Pts',(-0.818970185850148,-4.83232155624025,
395.228890610786));
#42776=CARTESIAN_POINT('Ctrl Pts',(-3.02456966792716,-3.85668537893236,
395.149762735327));
#42777=CARTESIAN_POINT('Ctrl Pts',(-4.49782033045318,-1.94721751819814,
395.070634859867));
#42778=CARTESIAN_POINT('Ctrl Pts',(-4.88199923361805,0.433736407473957,
394.991506984407));
#42779=CARTESIAN_POINT('Ctrl Pts',(-4.08408389914571,2.70966833633831,394.912379108948));
#42780=CARTESIAN_POINT('Ctrl Pts',(-2.29727614331402,4.32949952183574,394.833251233488));
#42781=CARTESIAN_POINT('Ctrl Pts',(0.04577850263863,4.90101500884376,394.754123358028));
#42782=CARTESIAN_POINT('Ctrl Pts',(2.37774865193587,4.28583190716024,394.674995482568));
#42783=CARTESIAN_POINT('Ctrl Pts',(4.13398684276656,2.63290648752449,394.595867607109));
#42784=CARTESIAN_POINT('Ctrl Pts',(4.8892494513703,0.34246691882695,394.516739731649));
#42785=CARTESIAN_POINT('Ctrl Pts',(4.46066230370267,-2.03089527069752,394.437611856189));
#42786=CARTESIAN_POINT('Ctrl Pts',(2.95200058966839,-3.91251023088926,394.358483980729));
#42787=CARTESIAN_POINT('Ctrl Pts',(0.728561441315958,-4.84677645600076,
394.279356105269));
#42788=CARTESIAN_POINT('Ctrl Pts',(-1.67128664123166,-4.60747704834829,
394.200228229809));
#42789=CARTESIAN_POINT('Ctrl Pts',(-3.66646069301835,-3.25255434616657,
394.12110035435));
#42790=CARTESIAN_POINT('Ctrl Pts',(-4.7738627787844,-1.11008015816539,394.04197247889));
#42791=CARTESIAN_POINT('Ctrl Pts',(-4.72535405587758,1.30118132280515,393.96284460343));
#42792=CARTESIAN_POINT('Ctrl Pts',(-3.53268009800228,3.39738356877675,393.88371672797));
#42793=CARTESIAN_POINT('Ctrl Pts',(-1.48462690153391,4.6709663616277,393.804588852511));
#42794=CARTESIAN_POINT('Ctrl Pts',(0.922903800227676,4.81355298752812,393.725460977051));
#42795=CARTESIAN_POINT('Ctrl Pts',(3.10696882493013,3.79061848635918,393.646333101591));
#42796=CARTESIAN_POINT('Ctrl Pts',(4.53873345614266,1.84984929178215,393.567205226131));
#42797=CARTESIAN_POINT('Ctrl Pts',(4.87151990076886,-0.538829884684078,
393.488077350672));
#42798=CARTESIAN_POINT('Ctrl Pts',(4.02474950245672,-2.79704044137549,393.408949475212));
#42799=CARTESIAN_POINT('Ctrl Pts',(2.2034535118369,-4.37799456479668,393.329821599752));
#42800=CARTESIAN_POINT('Ctrl Pts',(-0.151371792205916,-4.89889072839352,
393.250693724292));
#42801=CARTESIAN_POINT('Ctrl Pts',(-2.46954495544641,-4.23360266218321,
393.171565848832));
#42802=CARTESIAN_POINT('Ctrl Pts',(-4.18975922485567,-2.54321871374691,
393.092437973373));
#42803=CARTESIAN_POINT('Ctrl Pts',(-4.89549356508254,-0.23703700650118,
393.013310097913));
#42804=CARTESIAN_POINT('Ctrl Pts',(-4.41586624162366,2.12653923648359,392.934182222453));
#42805=CARTESIAN_POINT('Ctrl Pts',(-2.86701096694867,3.97520966788064,392.855054346993));
#42806=CARTESIAN_POINT('Ctrl Pts',(-0.623957069722673,4.86134974707218,
392.775926471534));
#42807=CARTESIAN_POINT('Ctrl Pts',(1.7701775674537,4.57039551547777,392.696798596074));
#42808=CARTESIAN_POINT('Ctrl Pts',(3.73569339459987,3.17279666063845,392.617670720614));
#42809=CARTESIAN_POINT('Ctrl Pts',(4.79667371815007,1.00695830590151,392.538542845154));
#42810=CARTESIAN_POINT('Ctrl Pts',(4.69621994662587,-1.40269811475204,392.459414969694));
#42811=CARTESIAN_POINT('Ctrl Pts',(3.45865527607574,-3.47271471179091,392.380287094234));
#42812=CARTESIAN_POINT('Ctrl Pts',(1.38363523608003,-4.70187168281881,392.301159218775));
#42813=CARTESIAN_POINT('Ctrl Pts',(-1.02640887116651,-4.79254928168782,
392.222031343315));
#42814=CARTESIAN_POINT('Ctrl Pts',(-3.18792528432602,-3.72279144860016,
392.142903467855));
#42815=CARTESIAN_POINT('Ctrl Pts',(-4.5775390550865,-1.75162210175979,392.063775592395));
#42816=CARTESIAN_POINT('Ctrl Pts',(-4.85877851429126,0.64367316028962,391.984647716936));
#42817=CARTESIAN_POINT('Ctrl Pts',(-3.96354624360545,2.88311376171958,391.905519841476));
#42818=CARTESIAN_POINT('Ctrl Pts',(-2.1086077232932,4.4244567189073,391.826391966016));
#42819=CARTESIAN_POINT('Ctrl Pts',(0.256894793419963,4.89449168487693,391.747264090557));
#42820=CARTESIAN_POINT('Ctrl Pts',(2.56019454432978,4.17940757564988,391.668136215096));
#42821=CARTESIAN_POINT('Ctrl Pts',(4.24358612375888,2.45235001548652,391.589008339637));
#42822=CARTESIAN_POINT('Ctrl Pts',(4.89946449317567,0.131497027824103,391.509880464177));
#42823=CARTESIAN_POINT('Ctrl Pts',(4.36901970526599,-2.22119575976841,391.430752588718));
#42824=CARTESIAN_POINT('Ctrl Pts',(2.78069006924853,-4.03606324615933,391.351624713257));
#42825=CARTESIAN_POINT('Ctrl Pts',(0.519062968356706,-4.87366570694958,
391.272496837798));
#42826=CARTESIAN_POINT('Ctrl Pts',(-1.86824652503536,-4.5311917538225,391.193368962338));
#42827=CARTESIAN_POINT('Ctrl Pts',(-3.80319145504887,-3.09156571084279,
391.114241086878));
#42828=CARTESIAN_POINT('Ctrl Pts',(-4.81725735814933,-0.903368880121367,
391.035113211418));
#42829=CARTESIAN_POINT('Ctrl Pts',(-4.66490518296109,1.50356357437869,390.955985335959));
#42830=CARTESIAN_POINT('Ctrl Pts',(-3.38302445358346,3.54643332584613,390.876857460499));
#42831=CARTESIAN_POINT('Ctrl Pts',(-1.28200109001022,4.73059372525567,390.797729585039));
#42832=CARTESIAN_POINT('Ctrl Pts',(1.12943733686538,4.76932019163214,390.718601709579));
#42833=CARTESIAN_POINT('Ctrl Pts',(3.2674014545917,3.65323576063024,390.639473834119));
#42834=CARTESIAN_POINT('Ctrl Pts',(4.61421910819667,1.65258155918805,390.56034595866));
#42835=CARTESIAN_POINT('Ctrl Pts',(4.84378099055226,-0.74821755110413,390.4812180832));
#42836=CARTESIAN_POINT('Ctrl Pts',(3.90050254186479,-2.96784832987165,390.40209020774));
#42837=CARTESIAN_POINT('Ctrl Pts',(2.01278281861149,-4.46886440981576,390.32296233228));
#42838=CARTESIAN_POINT('Ctrl Pts',(-0.362298507468694,-4.88781992095675,
390.243834456821));
#42839=CARTESIAN_POINT('Ctrl Pts',(-2.6496553261311,-4.12327181264112,390.164706581361));
#42840=CARTESIAN_POINT('Ctrl Pts',(-4.29544254536053,-2.36034258693993,
390.085578705901));
#42841=CARTESIAN_POINT('Ctrl Pts',(-4.90116039177906,-0.0258959894911138,
390.006450830441));
#42842=CARTESIAN_POINT('Ctrl Pts',(-4.32014444746653,2.31482088750723,389.927322954982));
#42843=CARTESIAN_POINT('Ctrl Pts',(-2.69307797902764,4.09504270882394,389.848195079522));
#42844=CARTESIAN_POINT('Ctrl Pts',(-0.41392784400509,4.88371861680963,389.769067204062));
#42845=CARTESIAN_POINT('Ctrl Pts',(1.96544797639375,4.48988396735431,389.689939328602));
#42846=CARTESIAN_POINT('Ctrl Pts',(3.86892353214857,3.00889921576025,389.610811453142));
#42847=CARTESIAN_POINT('Ctrl Pts',(4.83560414092378,0.799359981795764,389.531683577683));
#42848=CARTESIAN_POINT('Ctrl Pts',(4.63142430565821,-1.60373086556754,389.452555702223));
#42849=CARTESIAN_POINT('Ctrl Pts',(3.30582274912905,-3.61850518025834,389.373427826763));
#42850=CARTESIAN_POINT('Ctrl Pts',(1.17977165637593,-4.75711915207383,389.294299951303));
#42851=CARTESIAN_POINT('Ctrl Pts',(-1.23194135683111,-4.74387650361441,
389.215172075843));
#42852=CARTESIAN_POINT('Ctrl Pts',(-3.34536043156536,-3.58198372010992,
389.136044200384));
#42853=CARTESIAN_POINT('Ctrl Pts',(-4.64875658336638,-1.55277365279788,
389.056916324924));
#42854=CARTESIAN_POINT('Ctrl Pts',(-4.82653429353919,0.852414512725966,
388.977788449464));
#42855=CARTESIAN_POINT('Ctrl Pts',(-3.83564767110356,3.05120479997222,388.898660574004));
#42856=CARTESIAN_POINT('Ctrl Pts',(-1.91602329336559,4.5111970171448,388.819532698545));
#42857=CARTESIAN_POINT('Ctrl Pts',(0.467533990930312,4.87887853461636,388.740404823085));
#42858=CARTESIAN_POINT('Ctrl Pts',(2.73788576040913,4.06522143937628,388.661276947625));
#42859=CARTESIAN_POINT('Ctrl Pts',(4.34530441052119,2.26723915106472,388.582149072165));
#42860=CARTESIAN_POINT('Ctrl Pts',(4.90058047341499,-0.0797170734497908,
388.503021196706));
#42861=CARTESIAN_POINT('Ctrl Pts',(4.26926316308366,-2.40737114557615,388.423893321245));
#42862=CARTESIAN_POINT('Ctrl Pts',(2.60421537830119,-4.1521206692045,388.344765445786));
#42863=CARTESIAN_POINT('Ctrl Pts',(0.308600515372232,-4.89150380865921,
388.265637570326));
#42864=CARTESIAN_POINT('Ctrl Pts',(-2.06173678676592,-4.44649133703325,
388.186509694866));
#42865=CARTESIAN_POINT('Ctrl Pts',(-3.93285910370337,-2.92483556095608,
388.107381819407));
#42866=CARTESIAN_POINT('Ctrl Pts',(-4.85170554728278,-0.694979906674425,
388.028253943947));
#42867=CARTESIAN_POINT('Ctrl Pts',(-4.59579286131083,1.70315347639018,387.949126068487));
#42868=CARTESIAN_POINT('Ctrl Pts',(-3.22708601074344,3.68889680900396,387.869998193027));
#42869=CARTESIAN_POINT('Ctrl Pts',(-1.07699440464578,4.78143564639088,387.790870317567));
#42870=CARTESIAN_POINT('Ctrl Pts',(1.3338733340929,4.71623003221975,387.711742442108));
#42871=CARTESIAN_POINT('Ctrl Pts',(3.42176601558219,3.50906841238845,387.632614566648));
#42872=CARTESIAN_POINT('Ctrl Pts',(4.68113544337878,1.45224472764016,387.553486691188));
#42873=CARTESIAN_POINT('Ctrl Pts',(4.80704643162612,-0.956215662079578,
387.474358815728));
#42874=CARTESIAN_POINT('Ctrl Pts',(3.76901174619325,-3.13314446607126,387.395230940269));
#42875=CARTESIAN_POINT('Ctrl Pts',(1.81837407711343,-4.5514348840665,387.316103064809));
#42876=CARTESIAN_POINT('Ctrl Pts',(-0.572552378499359,-4.86767167772133,
387.236975189349));
#42877=CARTESIAN_POINT('Ctrl Pts',(-2.82484487802531,-4.00528341110962,
387.157847313889));
#42878=CARTESIAN_POINT('Ctrl Pts',(-4.39314856625886,-2.173082939741,387.07871943843));
#42879=CARTESIAN_POINT('Ctrl Pts',(-4.89772500736415,0.185293120367267,
386.99959156297));
#42880=CARTESIAN_POINT('Ctrl Pts',(-4.21639947845907,2.4988035589589,386.92046368751));
#42881=CARTESIAN_POINT('Ctrl Pts',(-2.51414352974947,4.20727062357945,386.84133581205));
#42882=CARTESIAN_POINT('Ctrl Pts',(-0.203129890410879,4.89701766750308,
386.762207936591));
#42883=CARTESIAN_POINT('Ctrl Pts',(2.15706824516707,4.40103401190078,386.68308006113));
#42884=CARTESIAN_POINT('Ctrl Pts',(3.99496848171146,2.83941378075611,386.603952185671));
#42885=CARTESIAN_POINT('Ctrl Pts',(4.86555410065941,0.590277122860157,386.524824310211));
#42886=CARTESIAN_POINT('Ctrl Pts',(4.55802739511214,-1.80178524070515,386.445696434751));
#42887=CARTESIAN_POINT('Ctrl Pts',(3.14685079923878,-3.75757552625969,386.366568559291));
#42888=CARTESIAN_POINT('Ctrl Pts',(0.973717058663619,-4.80353191702554,
386.287440683832));
#42889=CARTESIAN_POINT('Ctrl Pts',(-1.43518593730373,-4.68639361487927,
386.208312808372));
#42890=CARTESIAN_POINT('Ctrl Pts',(-3.49658272828396,-3.43452369514056,
386.129184932912));
#42891=CARTESIAN_POINT('Ctrl Pts',(-4.71134065335373,-1.35104146356512,
386.050057057452));
#42892=CARTESIAN_POINT('Ctrl Pts',(-4.78532645385515,1.05957279988197,385.970929181993));
#42893=CARTESIAN_POINT('Ctrl Pts',(-3.70062570902444,3.21362928010108,385.891801306533));
#42894=CARTESIAN_POINT('Ctrl Pts',(-1.71988051253413,4.58955932643004,385.812673431073));
#42895=CARTESIAN_POINT('Ctrl Pts',(0.677304905677504,4.85420455409132,385.733545555613));
#42896=CARTESIAN_POINT('Ctrl Pts',(2.91049230016732,3.94348555961378,385.654417680154));
#42897=CARTESIAN_POINT('Ctrl Pts',(4.43895279649954,2.07791767369751,385.575289804694));
#42898=CARTESIAN_POINT('Ctrl Pts',(4.89259531954076,-0.29078312781775,385.496161929234));
#42899=CARTESIAN_POINT('Ctrl Pts',(4.16157794044722,-2.58907567170192,385.417034053774));
#42900=CARTESIAN_POINT('Ctrl Pts',(2.42290425755801,-4.26046696348217,385.337906178315));
#42901=CARTESIAN_POINT('Ctrl Pts',(0.0975649436126985,-4.90025763302231,
385.258778302854));
#42902=CARTESIAN_POINT('Ctrl Pts',(-2.25139808515128,-4.35353309972404,
385.179650427395));
#42903=CARTESIAN_POINT('Ctrl Pts',(-4.05522282615024,-2.75267354012164,
385.100522551935));
#42904=CARTESIAN_POINT('Ctrl Pts',(-4.87714337058205,-0.485300248303261,
385.021394676475));
#42905=CARTESIAN_POINT('Ctrl Pts',(-4.51814544317236,1.89958035959429,384.942266801015));
#42906=CARTESIAN_POINT('Ctrl Pts',(-3.06515437123229,3.82450944157957,384.863138925556));
#42907=CARTESIAN_POINT('Ctrl Pts',(-0.869987574488363,4.82339770374075,
384.784011050096));
#42908=CARTESIAN_POINT('Ctrl Pts',(1.53583212271834,4.65438110590894,384.704883174636));
#42909=CARTESIAN_POINT('Ctrl Pts',(3.56977582909287,3.35838418264497,384.625755299176));
#42910=CARTESIAN_POINT('Ctrl Pts',(4.73935818772915,1.24921085354728,384.546627423716));
#42911=CARTESIAN_POINT('Ctrl Pts',(4.76138444573462,-1.16243793302357,384.467499548257));
#42912=CARTESIAN_POINT('Ctrl Pts',(3.6305213141391,-3.29262186954369,384.388371672797));
#42913=CARTESIAN_POINT('Ctrl Pts',(1.62058833437354,-4.62555264143734,384.309243797337));
#42914=CARTESIAN_POINT('Ctrl Pts',(-0.781742931416587,-4.83848341708389,
384.230115921878));
#42915=CARTESIAN_POINT('Ctrl Pts',(-2.9947882570989,-3.87985658025632,384.150988046417));
#42916=CARTESIAN_POINT('Ctrl Pts',(-4.48269583239351,-1.98178754220968,
384.071860170958));
#42917=CARTESIAN_POINT('Ctrl Pts',(-4.88519379187676,0.396138112309837,
383.992732295498));
#42918=CARTESIAN_POINT('Ctrl Pts',(-4.10482400501691,2.67814556662863,383.913604420039));
#42919=CARTESIAN_POINT('Ctrl Pts',(-2.33053992799659,4.31168498759236,383.834476544578));
#42920=CARTESIAN_POINT('Ctrl Pts',(0.00804530673338092,4.90122220076332,
383.755348669119));
#42921=CARTESIAN_POINT('Ctrl Pts',(2.34468250536694,4.30401065719426,383.676220793659));
#42922=CARTESIAN_POINT('Ctrl Pts',(4.11359415836805,2.66465511623097,383.5970929182));
#42923=CARTESIAN_POINT('Ctrl Pts',(4.88646797566037,0.380098028225917,383.517965042739));
#42924=CARTESIAN_POINT('Ctrl Pts',(4.47616552437595,-1.99649342262975,383.43883716728));
#42925=CARTESIAN_POINT('Ctrl Pts',(2.98203466184577,-3.88966747470347,383.35970929182));
#42926=CARTESIAN_POINT('Ctrl Pts',(0.765854118125881,-4.84102378200782,
383.28058141636));
#42927=CARTESIAN_POINT('Ctrl Pts',(-1.6357651560373,-4.62020737007657,383.2014535409));
#42928=CARTESIAN_POINT('Ctrl Pts',(-3.6413113313429,-3.28068522971184,383.122325665441));
#42929=CARTESIAN_POINT('Ctrl Pts',(-4.76517503677366,-1.14680018186465,
383.043197789981));
#42930=CARTESIAN_POINT('Ctrl Pts',(-4.73523152455593,1.26476329685335,382.964069914521));
#42931=CARTESIAN_POINT('Ctrl Pts',(-3.55873111398586,3.37008555478411,382.884942039061));
#42932=CARTESIAN_POINT('Ctrl Pts',(-1.52054364820804,4.65939811586324,382.805814163601));
#42933=CARTESIAN_POINT('Ctrl Pts',(0.885817960704724,4.82051556669083,382.726686288142));
#42934=CARTESIAN_POINT('Ctrl Pts',(3.07769360662633,3.8144260186753,382.647558412682));
#42935=CARTESIAN_POINT('Ctrl Pts',(4.52435736219093,1.88473718258125,382.568430537222));
#42936=CARTESIAN_POINT('Ctrl Pts',(4.87552386121587,-0.501309153048634,
382.489302661763));
#42937=CARTESIAN_POINT('Ctrl Pts',(4.04616402543129,-2.76597188480314,382.410174786302));
#42938=CARTESIAN_POINT('Ctrl Pts',(2.23709342974706,-4.36090091320568,382.331046910843));
#42939=CARTESIAN_POINT('Ctrl Pts',(-0.113651821301689,-4.89991092283629,
382.251919035383));
#42940=CARTESIAN_POINT('Ctrl Pts',(-2.43687818989498,-4.25248967968529,
382.172791159923));
#42941=CARTESIAN_POINT('Ctrl Pts',(-4.17005537407579,-2.5753993797773,382.093663284464));
#42942=CARTESIAN_POINT('Ctrl Pts',(-4.89352358608415,-0.274719312487676,
382.014535409004));
#42943=CARTESIAN_POINT('Ctrl Pts',(-4.43210713178239,2.09247942895964,381.935407533544));
#42944=CARTESIAN_POINT('Ctrl Pts',(-2.89753026709117,3.95301936998874,381.856279658084));
#42945=CARTESIAN_POINT('Ctrl Pts',(-0.661365043163431,4.85640196728989,
381.777151782624));
#42946=CARTESIAN_POINT('Ctrl Pts',(1.73493863410831,4.58388827569936,381.698023907165));
#42947=CARTESIAN_POINT('Ctrl Pts',(3.7111560180617,3.20146291526546,381.618896031705));
#42948=CARTESIAN_POINT('Ctrl Pts',(4.78877921262759,1.04385700214232,381.539768156245));
#42949=CARTESIAN_POINT('Ctrl Pts',(4.70687983423134,-1.36650137735827,381.460640280785));
#42950=CARTESIAN_POINT('Ctrl Pts',(3.48528844380413,-3.44598436614286,381.381512405325));
#42951=CARTESIAN_POINT('Ctrl Pts',(1.41979290903503,-4.69108003381625,381.302384529866));
#42952=CARTESIAN_POINT('Ctrl Pts',(-0.989481667084847,-4.80030934614829,
381.223256654406));
#42953=CARTESIAN_POINT('Ctrl Pts',(-3.1591698522741,-3.74722425705989,381.144128778946));
#42954=CARTESIAN_POINT('Ctrl Pts',(-4.56391804067381,-1.78681165941677,
381.065000903487));
#42955=CARTESIAN_POINT('Ctrl Pts',(-4.86359001771767,0.606247414652442,
380.985873028026));
#42956=CARTESIAN_POINT('Ctrl Pts',(-3.98562524001068,2.85251384473511,380.906745152567));
#42957=CARTESIAN_POINT('Ctrl Pts',(-2.1426081539881,4.40809188727722,380.827617277107));
#42958=CARTESIAN_POINT('Ctrl Pts',(0.219205562501549,4.89632440812331,380.748489401647));
#42959=CARTESIAN_POINT('Ctrl Pts',(2.52794232836271,4.19899409057548,380.669361526187));
#42960=CARTESIAN_POINT('Ctrl Pts',(4.22458025593252,2.48494777599062,380.590233650728));
#42961=CARTESIAN_POINT('Ctrl Pts',(4.89830692563373,0.169213032902914,380.511105775268));
#42962=CARTESIAN_POINT('Ctrl Pts',(4.38599072357506,-2.18749380820361,380.431977899808));
#42963=CARTESIAN_POINT('Ctrl Pts',(2.81168042594869,-4.01453571045926,380.352850024348));
#42964=CARTESIAN_POINT('Ctrl Pts',(0.556568868317172,-4.86952511884227,
380.273722148889));
#42965=CARTESIAN_POINT('Ctrl Pts',(-1.83330650647258,-4.54544068727564,
380.194594273429));
#42966=CARTESIAN_POINT('Ctrl Pts',(-3.77927745739419,-3.12075402559187,
380.115466397969));
#42967=CARTESIAN_POINT('Ctrl Pts',(-4.81015975486937,-0.940429115271696,
380.036338522509));
#42968=CARTESIAN_POINT('Ctrl Pts',(-4.67634253965503,1.46760493322567,379.95721064705));
#42969=CARTESIAN_POINT('Ctrl Pts',(-3.41022740614562,3.5202830605775,379.878082771589));
#42970=CARTESIAN_POINT('Ctrl Pts',(-1.31838289970275,4.72058368403601,379.79895489613));
#42971=CARTESIAN_POINT('Ctrl Pts',(1.09268591509449,4.77787413806285,379.71982702067));
#42972=CARTESIAN_POINT('Ctrl Pts',(3.23917916116038,3.67828250004266,379.64069914521));
#42973=CARTESIAN_POINT('Ctrl Pts',(4.60135949813868,1.68805644369628,379.56157126975));
#42974=CARTESIAN_POINT('Ctrl Pts',(4.8493978027726,-0.71090416982881,379.482443394291));
#42975=CARTESIAN_POINT('Ctrl Pts',(3.92323575948474,-2.93773126131644,379.403315518831));
#42976=CARTESIAN_POINT('Ctrl Pts',(2.04712797424676,-4.45323599703316,379.324187643371));
#42977=CARTESIAN_POINT('Ctrl Pts',(-0.324657517247101,-4.89046432199546,
379.245059767911));
#42978=CARTESIAN_POINT('Ctrl Pts',(-2.61783263582229,-4.14354873013934,
379.165931892452));
#42979=CARTESIAN_POINT('Ctrl Pts',(-4.27714348571947,-2.39334230539285,
379.086804016992));
#42980=CARTESIAN_POINT('Ctrl Pts',(-4.90081577320139,-0.0636281805188475,
379.007676141532));
#42981=CARTESIAN_POINT('Ctrl Pts',(-4.33783771356114,2.28149244114949,378.928548266072));
#42982=CARTESIAN_POINT('Ctrl Pts',(-2.72452500214632,4.07418793146503,378.849420390613));
#42983=CARTESIAN_POINT('Ctrl Pts',(-0.451514254902642,4.88038714302825,
378.770292515153));
#42984=CARTESIAN_POINT('Ctrl Pts',(1.93082309674852,4.50488245765392,378.691164639693));
#42985=CARTESIAN_POINT('Ctrl Pts',(3.84564401766237,3.03859603725688,378.612036764233));
#42986=CARTESIAN_POINT('Ctrl Pts',(4.82930673560502,0.836564547214143,378.532908888774));
#42987=CARTESIAN_POINT('Ctrl Pts',(4.64363382059009,-1.56802701777984,378.453781013314));
#42988=CARTESIAN_POINT('Ctrl Pts',(3.33358285503851,-3.59294713804823,378.374653137854));
#42989=CARTESIAN_POINT('Ctrl Pts',(1.21636070918609,-4.74789536672449,378.295525262394));
#42990=CARTESIAN_POINT('Ctrl Pts',(-1.19538278261738,-4.7532203600546,378.216397386934));
#42991=CARTESIAN_POINT('Ctrl Pts',(-3.31768438156428,-3.60763276020996,
378.137269511475));
#42992=CARTESIAN_POINT('Ctrl Pts',(-4.6366643489263,-1.58851739166163,378.058141636015));
#42993=CARTESIAN_POINT('Ctrl Pts',(-4.83295380642895,0.815230822000412,
377.979013760555));
#42994=CARTESIAN_POINT('Ctrl Pts',(-3.85902455393964,3.02158456448046,377.899885885095));
#42995=CARTESIAN_POINT('Ctrl Pts',(-1.95069722602663,4.49631228014555,377.820758009635));
#42996=CARTESIAN_POINT('Ctrl Pts',(0.429958719716191,4.88233338553971,377.741630134176));
#42997=CARTESIAN_POINT('Ctrl Pts',(2.70650737238561,4.08617934401293,377.662502258716));
#42998=CARTESIAN_POINT('Ctrl Pts',(4.32772065609622,2.30062550429524,377.583374383256));
#42999=CARTESIAN_POINT('Ctrl Pts',(4.9010489638226,-0.0419862171323538,
377.504246507796));
#43000=CARTESIAN_POINT('Ctrl Pts',(4.28767046122876,-2.37443168023888,377.425118632336));
#43001=CARTESIAN_POINT('Ctrl Pts',(2.63610446564972,-4.13194833394574,377.345990756877));
#43002=CARTESIAN_POINT('Ctrl Pts',(0.346249984239667,-4.88898299614862,
377.266862881417));
#43003=CARTESIAN_POINT('Ctrl Pts',(-2.0274431238406,-4.46223241974302,377.187735005957));
#43004=CARTESIAN_POINT('Ctrl Pts',(-3.91022488205308,-2.95502709970493,
377.108607130498));
#43005=CARTESIAN_POINT('Ctrl Pts',(-4.84621126407803,-0.732311526700024,
377.029479255038));
#43006=CARTESIAN_POINT('Ctrl Pts',(-4.60876886508425,1.66772100077964,376.950351379578));
#43007=CARTESIAN_POINT('Ctrl Pts',(-3.25539037980364,3.66394285754004,376.871223504118));
#43008=CARTESIAN_POINT('Ctrl Pts',(-1.11377371072242,4.77300239990086,376.792095628659));
#43009=CARTESIAN_POINT('Ctrl Pts',(1.29752458313577,4.72635945993341,376.712967753198));
#43010=CARTESIAN_POINT('Ctrl Pts',(3.39464906017594,3.53530784320889,376.633839877739));
#43011=CARTESIAN_POINT('Ctrl Pts',(4.66981619949699,1.48824072358315,376.554712002279));
#43012=CARTESIAN_POINT('Ctrl Pts',(4.8142656643279,-0.919178927997845,376.475584126819));
#43013=CARTESIAN_POINT('Ctrl Pts',(3.79302143937608,-3.10403481730793,376.396456251359));
#43014=CARTESIAN_POINT('Ctrl Pts',(1.85336068619839,-4.53730073503479,376.3173283759));
#43015=CARTESIAN_POINT('Ctrl Pts',(-0.535060274040971,-4.87193537309239,
376.23820050044));
#43016=CARTESIAN_POINT('Ctrl Pts',(-2.7939253627036,-4.02691257378452,376.15907262498));
#43017=CARTESIAN_POINT('Ctrl Pts',(-4.37628828172638,-2.20684041966181,
376.07994474952));
#43018=CARTESIAN_POINT('Ctrl Pts',(-4.89900638965642,0.147581107404016,
376.000816874061));
#43019=CARTESIAN_POINT('Ctrl Pts',(-4.23551226043463,2.46626839394683,375.921688998601));
#43020=CARTESIAN_POINT('Ctrl Pts',(-2.54645987583722,4.18779004627332,375.842561123141));
#43021=CARTESIAN_POINT('Ctrl Pts',(-0.24082493083811,4.89530879473852,375.763433247681));
#43022=CARTESIAN_POINT('Ctrl Pts',(2.12312171415927,4.41751014933925,375.684305372222));
#43023=CARTESIAN_POINT('Ctrl Pts',(3.97299008156779,2.87008650088106,375.605177496762));
#43024=CARTESIAN_POINT('Ctrl Pts',(4.86086545139366,0.627717440079687,375.526049621302));
#43025=CARTESIAN_POINT('Ctrl Pts',(4.57176394606508,-1.76663842623643,375.446921745842));
#43026=CARTESIAN_POINT('Ctrl Pts',(3.1756861134954,-3.73324183321634,375.367793870382));
#43027=CARTESIAN_POINT('Ctrl Pts',(1.01066992437191,-4.79588344705227,375.288665994922));
#43028=CARTESIAN_POINT('Ctrl Pts',(-1.39906459845869,-4.69732449000695,
375.209538119463));
#43029=CARTESIAN_POINT('Ctrl Pts',(-3.47003521363053,-3.46129850620319,
375.130410244003));
#43030=CARTESIAN_POINT('Ctrl Pts',(-4.70079892256589,-1.38736908122097,
375.051282368543));
#43031=CARTESIAN_POINT('Ctrl Pts',(-4.79330612491241,1.02286909042425,374.972154493083));
#43032=CARTESIAN_POINT('Ctrl Pts',(-4.08111211300407,2.46384394177367,374.91940257611));
#43033=CARTESIAN_POINT('Ctrl Pts',(-3.57461543774341,3.05624720968232,374.893026617624));
#43034=CARTESIAN_POINT('Ctrl Pts',(-1.16918346556839,-4.36383719750651,
400.320920147129));
#43035=CARTESIAN_POINT('Ctrl Pts',(-1.89238053709901,-4.17007422695751,
400.294544188642));
#43036=CARTESIAN_POINT('Ctrl Pts',(-3.23983970630162,-3.41613758049457,
400.241792271669));
#43037=CARTESIAN_POINT('Ctrl Pts',(-4.47701437999898,-1.45709925725484,
400.162664396209));
#43038=CARTESIAN_POINT('Ctrl Pts',(-4.62991897006387,0.854469866048622,
400.08353652075));
#43039=CARTESIAN_POINT('Ctrl Pts',(-3.66187379628773,2.9592933130866,400.00440864529));
#43040=CARTESIAN_POINT('Ctrl Pts',(-1.80711600920317,4.34750539486619,399.92528076983));
#43041=CARTESIAN_POINT('Ctrl Pts',(0.485180445975455,4.68307450728292,399.84615289437));
#43042=CARTESIAN_POINT('Ctrl Pts',(2.66001002393004,3.8847003355008,399.767025018911));
#43043=CARTESIAN_POINT('Ctrl Pts',(4.19075738523379,2.14571838156707,399.687897143451));
#43044=CARTESIAN_POINT('Ctrl Pts',(4.70678568217143,-0.112816719181106,
399.608769267991));
#43045=CARTESIAN_POINT('Ctrl Pts',(4.0831435580808,-2.34403352376061,399.529641392531));
#43046=CARTESIAN_POINT('Ctrl Pts',(2.47083727056938,-4.00768268816587,399.450513517072));
#43047=CARTESIAN_POINT('Ctrl Pts',(0.26025890735466,-4.70093834136087,399.371385641611));
#43048=CARTESIAN_POINT('Ctrl Pts',(-2.01333665809567,-4.25594078634204,
399.292257766152));
#43049=CARTESIAN_POINT('Ctrl Pts',(-3.79943657795602,-2.78043846617054,
399.213129890692));
#43050=CARTESIAN_POINT('Ctrl Pts',(-4.66556662297687,-0.631699640775407,
399.134002015232));
#43051=CARTESIAN_POINT('Ctrl Pts',(-4.40200797064279,1.66999467634492,399.054874139773));
#43052=CARTESIAN_POINT('Ctrl Pts',(-3.07257690863908,3.56732778180521,398.975746264313));
#43053=CARTESIAN_POINT('Ctrl Pts',(-0.999172881885126,4.60089229715201,
398.896618388853));
#43054=CARTESIAN_POINT('Ctrl Pts',(1.31616410234924,4.52042790313295,398.817490513393));
#43055=CARTESIAN_POINT('Ctrl Pts',(3.3128140221261,3.34541770608376,398.738362637933));
#43056=CARTESIAN_POINT('Ctrl Pts',(4.50732158649137,1.36037071761185,398.659234762474));
#43057=CARTESIAN_POINT('Ctrl Pts',(4.61045682154316,-0.954067224935643,
398.580106887014));
#43058=CARTESIAN_POINT('Ctrl Pts',(3.5972472600316,-3.03749378987274,398.500979011554));
#43059=CARTESIAN_POINT('Ctrl Pts',(1.71302460447423,-4.38544217583732,398.421851136094));
#43060=CARTESIAN_POINT('Ctrl Pts',(-0.58597822963345,-4.67152928789035,
398.342723260635));
#43061=CARTESIAN_POINT('Ctrl Pts',(-2.74309626297668,-3.82648392982927,
398.263595385175));
#43062=CARTESIAN_POINT('Ctrl Pts',(-4.23601954113904,-2.05491966273361,
398.184467509715));
#43063=CARTESIAN_POINT('Ctrl Pts',(-4.70326173037178,0.214208937311664,
398.105339634255));
#43064=CARTESIAN_POINT('Ctrl Pts',(-4.0316879707426,2.43147043571793,398.026211758796));
#43065=CARTESIAN_POINT('Ctrl Pts',(-2.38390858507682,4.05999214669189,397.947083883336));
#43066=CARTESIAN_POINT('Ctrl Pts',(-0.158905716443472,4.70545485011635,
397.867956007876));
#43067=CARTESIAN_POINT('Ctrl Pts',(2.10457350639361,4.2115705775148,397.788828132416));
#43068=CARTESIAN_POINT('Ctrl Pts',(3.85846555079357,2.69792512248606,397.709700256956));
#43069=CARTESIAN_POINT('Ctrl Pts',(4.67809487300653,0.531022346377457,397.630572381497));
#43070=CARTESIAN_POINT('Ctrl Pts',(4.36500197879199,-1.76445858504648,397.551444506037));
#43071=CARTESIAN_POINT('Ctrl Pts',(2.99499706155341,-3.63270546211616,397.472316630577));
#43072=CARTESIAN_POINT('Ctrl Pts',(0.899803835430396,-4.62135363621384,
397.393188755117));
#43073=CARTESIAN_POINT('Ctrl Pts',(-1.41326179868926,-4.4910185327571,397.314060879658));
#43074=CARTESIAN_POINT('Ctrl Pts',(-3.38412979029408,-3.2732586111773,397.234933004198));
#43075=CARTESIAN_POINT('Ctrl Pts',(-4.53558750895661,-1.26293401324019,
397.155805128738));
#43076=CARTESIAN_POINT('Ctrl Pts',(-4.58882877938272,1.0531888751364,397.076677253278));
#43077=CARTESIAN_POINT('Ctrl Pts',(-3.53096212085652,3.11429974059636,396.997549377818));
#43078=CARTESIAN_POINT('Ctrl Pts',(-1.61813220309064,4.42133515428577,396.918421502359));
#43079=CARTESIAN_POINT('Ctrl Pts',(0.686501289701844,4.65781841127795,396.839293626899));
#43080=CARTESIAN_POINT('Ctrl Pts',(2.82491000861503,3.76648905699045,396.760165751439));
#43081=CARTESIAN_POINT('Ctrl Pts',(4.27931414595585,1.96316754593802,396.681037875979));
#43082=CARTESIAN_POINT('Ctrl Pts',(4.69755413190968,-0.315502061769038,
396.601910000519));
#43083=CARTESIAN_POINT('Ctrl Pts',(3.97836016824692,-2.51777813655384,396.52278212506));
#43084=CARTESIAN_POINT('Ctrl Pts',(2.29587301155249,-4.11041646162856,396.4436542496));
#43085=CARTESIAN_POINT('Ctrl Pts',(0.0574787095610184,-4.70778637696628,
396.36452637414));
#43086=CARTESIAN_POINT('Ctrl Pts',(-2.1948330979661,-4.16524477615358,396.28539849868));
#43087=CARTESIAN_POINT('Ctrl Pts',(-3.9157028807147,-2.614159008776,396.206270623221));
#43088=CARTESIAN_POINT('Ctrl Pts',(-4.68845088177226,-0.430098479898641,
396.127142747761));
#43089=CARTESIAN_POINT('Ctrl Pts',(-4.32596913256195,1.85810318263636,396.048014872301));
#43090=CARTESIAN_POINT('Ctrl Pts',(-2.91602650941616,3.69639632203913,395.968886996841));
#43091=CARTESIAN_POINT('Ctrl Pts',(-0.8000169721583,4.63966908490906,395.889759121381));
#43092=CARTESIAN_POINT('Ctrl Pts',(1.50970325769618,4.4595237914943,395.810631245922));
#43093=CARTESIAN_POINT('Ctrl Pts',(3.45387416317228,3.19957960334997,395.731503370462));
#43094=CARTESIAN_POINT('Ctrl Pts',(4.56174736550757,1.16491087491141,395.652375495002));
#43095=CARTESIAN_POINT('Ctrl Pts',(4.56506994907375,-1.15182148498192,395.573247619542));
#43096=CARTESIAN_POINT('Ctrl Pts',(3.46303740598383,-3.18965958966768,395.494119744083));
#43097=CARTESIAN_POINT('Ctrl Pts',(1.52248843418447,-4.45517511900225,395.414991868623));
#43098=CARTESIAN_POINT('Ctrl Pts',(-0.786705578057672,-4.64194471171891,
395.335863993163));
#43099=CARTESIAN_POINT('Ctrl Pts',(-2.90541202853717,-3.70474524328377,
395.256736117703));
#43100=CARTESIAN_POINT('Ctrl Pts',(-4.32062168343229,-1.87050384705749,
395.177608242243));
#43101=CARTESIAN_POINT('Ctrl Pts',(-4.68966525951576,0.416648685217087,
395.098480366784));
#43102=CARTESIAN_POINT('Ctrl Pts',(-3.92318504412731,2.60291672604753,395.019352491324));
#43103=CARTESIAN_POINT('Ctrl Pts',(-2.20677136666199,4.15893213559478,394.940224615864));
#43104=CARTESIAN_POINT('Ctrl Pts',(0.0439749871279553,4.70793187861818,
394.861096740404));
#43105=CARTESIAN_POINT('Ctrl Pts',(2.28407353529635,4.11698487470637,394.781968864944));
#43106=CARTESIAN_POINT('Ctrl Pts',(3.97112198345224,2.52917902999067,394.702840989485));
#43107=CARTESIAN_POINT('Ctrl Pts',(4.69662984363174,0.328974900425354,394.623713114025));
#43108=CARTESIAN_POINT('Ctrl Pts',(4.28492755509978,-1.95088498398772,394.544585238566));
#43109=CARTESIAN_POINT('Ctrl Pts',(2.83570192230001,-3.75837078812964,394.465457363105));
#43110=CARTESIAN_POINT('Ctrl Pts',(0.699858627021958,-4.65583013815851,
394.386329487646));
#43111=CARTESIAN_POINT('Ctrl Pts',(-1.60544369734944,-4.42595830389794,
394.307201612186));
#43112=CARTESIAN_POINT('Ctrl Pts',(-3.52201475555854,-3.12441489479712,
394.228073736726));
#43113=CARTESIAN_POINT('Ctrl Pts',(-4.58578900897716,-1.06634681897889,
394.148945861266));
#43114=CARTESIAN_POINT('Ctrl Pts',(-4.53919136286672,1.24991925518346,394.069817985807));
#43115=CARTESIAN_POINT('Ctrl Pts',(-3.39350465573632,3.26353834429719,393.990690110347));
#43116=CARTESIAN_POINT('Ctrl Pts',(-1.42613770922415,4.48694635665851,393.911562234887));
#43117=CARTESIAN_POINT('Ctrl Pts',(0.886544565594953,4.62391556004391,393.832434359427));
#43118=CARTESIAN_POINT('Ctrl Pts',(2.98456494223475,3.64128115898587,393.753306483967));
#43119=CARTESIAN_POINT('Ctrl Pts',(4.35992297272438,1.77697159378319,393.674178608508));
#43120=CARTESIAN_POINT('Ctrl Pts',(4.67959877632843,-0.51760184098167,393.595050733048));
#43121=CARTESIAN_POINT('Ctrl Pts',(3.86618821853779,-2.68684667073537,393.515922857588));
#43122=CARTESIAN_POINT('Ctrl Pts',(2.116645024084,-4.20551664070214,393.436794982129));
#43123=CARTESIAN_POINT('Ctrl Pts',(-0.14540826436235,-4.70589128750945,
393.357667106668));
#43124=CARTESIAN_POINT('Ctrl Pts',(-2.37225338025842,-4.06681328229544,
393.278539231209));
#43125=CARTESIAN_POINT('Ctrl Pts',(-4.02469712556258,-2.44302464594413,
393.199411355749));
#43126=CARTESIAN_POINT('Ctrl Pts',(-4.70262796074555,-0.227698563931231,
393.120283480289));
#43127=CARTESIAN_POINT('Ctrl Pts',(-4.24189630375331,2.04276090656889,393.04115560483));
#43128=CARTESIAN_POINT('Ctrl Pts',(-2.75406059832286,3.81860008301049,392.962027729369));
#43129=CARTESIAN_POINT('Ctrl Pts',(-0.599375307795595,4.66982929169869,
392.88289985391));
#43130=CARTESIAN_POINT('Ctrl Pts',(1.70043866129603,4.39033765584971,392.80377197845));
#43131=CARTESIAN_POINT('Ctrl Pts',(3.58851992688128,3.04779938768583,392.72464410299));
#43132=CARTESIAN_POINT('Ctrl Pts',(4.60770127580904,0.967287612920714,392.64551622753));
#43133=CARTESIAN_POINT('Ctrl Pts',(4.51120503728849,-1.34743663477919,392.566388352071));
#43134=CARTESIAN_POINT('Ctrl Pts',(3.32239615712367,-3.3359016994408,392.487260476611));
#43135=CARTESIAN_POINT('Ctrl Pts',(1.32912476794421,-4.51663411451929,392.408132601151));
#43136=CARTESIAN_POINT('Ctrl Pts',(-0.985971892830688,-4.60373932795397,
392.329004725692));
#43137=CARTESIAN_POINT('Ctrl Pts',(-3.06233199564761,-3.57612627316698,
392.249876850231));
#43138=CARTESIAN_POINT('Ctrl Pts',(-4.397199764574,-1.68261421711348,392.170748974772));
#43139=CARTESIAN_POINT('Ctrl Pts',(-4.66735935664344,0.618314652224117,
392.091621099312));
#43140=CARTESIAN_POINT('Ctrl Pts',(-3.80739615752567,2.76952899837877,392.012493223852));
#43141=CARTESIAN_POINT('Ctrl Pts',(-2.02553583330784,4.25014834578608,391.933365348393));
#43142=CARTESIAN_POINT('Ctrl Pts',(0.24677402236281,4.70166555117323,391.854237472933));
#43143=CARTESIAN_POINT('Ctrl Pts',(2.45933168720454,4.01475329572239,391.775109597473));
#43144=CARTESIAN_POINT('Ctrl Pts',(4.07640342983146,2.35573586177663,391.695981722014));
#43145=CARTESIAN_POINT('Ctrl Pts',(4.70644244793312,0.126316497321376,391.616853846553));
#43146=CARTESIAN_POINT('Ctrl Pts',(4.19689535976046,-2.13368828848624,391.537725971094));
#43147=CARTESIAN_POINT('Ctrl Pts',(2.67114044701949,-3.87705623966156,391.458598095634));
#43148=CARTESIAN_POINT('Ctrl Pts',(0.498613673152825,-4.68166004512793,
391.379470220174));
#43149=CARTESIAN_POINT('Ctrl Pts',(-1.79464403933883,-4.35267838752966,
391.300342344714));
#43150=CARTESIAN_POINT('Ctrl Pts',(-3.65335879596438,-2.96976865785062,
391.221214469255));
#43151=CARTESIAN_POINT('Ctrl Pts',(-4.62747399120691,-0.867779254134205,
391.142086593794));
#43152=CARTESIAN_POINT('Ctrl Pts',(-4.4811239675789,1.4443283423073,391.062958718335));
#43153=CARTESIAN_POINT('Ctrl Pts',(-3.24974492884238,3.40671605371881,390.983830842875));
#43154=CARTESIAN_POINT('Ctrl Pts',(-1.23149465757426,4.54422460729751,390.904702967416));
#43155=CARTESIAN_POINT('Ctrl Pts',(1.08494139143324,4.58142538413069,390.825575091955));
#43156=CARTESIAN_POINT('Ctrl Pts',(3.1386770782293,3.50931084000835,390.746447216496));
#43157=CARTESIAN_POINT('Ctrl Pts',(4.43243474978322,1.58747553118664,390.667319341036));
#43158=CARTESIAN_POINT('Ctrl Pts',(4.65295268374329,-0.718740353708034,
390.588191465577));
#43159=CARTESIAN_POINT('Ctrl Pts',(3.74683616074228,-2.85092531606077,390.509063590117));
#43160=CARTESIAN_POINT('Ctrl Pts',(1.93348610020102,-4.29280652644998,390.429935714657));
#43161=CARTESIAN_POINT('Ctrl Pts',(-0.348025192701879,-4.69525663179842,
390.350807839197));
#43162=CARTESIAN_POINT('Ctrl Pts',(-2.54526802197775,-3.96082908865047,
390.271679963737));
#43163=CARTESIAN_POINT('Ctrl Pts',(-4.12621688682536,-2.2673532093786,390.192552088278));
#43164=CARTESIAN_POINT('Ctrl Pts',(-4.70807153396599,-0.0248757765959869,
390.113424212818));
#43165=CARTESIAN_POINT('Ctrl Pts',(-4.14994561897114,2.22362490829375,390.034296337358));
#43166=CARTESIAN_POINT('Ctrl Pts',(-2.58697997173855,3.93371211440616,389.955168461898));
#43167=CARTESIAN_POINT('Ctrl Pts',(-0.397620511000842,4.69131690492484,
389.876040586439));
#43168=CARTESIAN_POINT('Ctrl Pts',(1.88801608791904,4.31299798573579,389.796912710978));
#43169=CARTESIAN_POINT('Ctrl Pts',(3.71650125536658,2.89035893827407,389.717784835519));
#43170=CARTESIAN_POINT('Ctrl Pts',(4.64509797385908,0.767867948577403,389.638656960059));
#43171=CARTESIAN_POINT('Ctrl Pts',(4.44896212165639,-1.54054938683214,389.559529084599));
#43172=CARTESIAN_POINT('Ctrl Pts',(3.17558470594392,-3.47594852501834,389.480401209139));
#43173=CARTESIAN_POINT('Ctrl Pts',(1.13329271192188,-4.56970502355534,389.40127333368));
#43174=CARTESIAN_POINT('Ctrl Pts',(-1.18340710566026,-4.55698408988609,
389.32214545822));
#43175=CARTESIAN_POINT('Ctrl Pts',(-3.21356473971502,-3.44086588475379,
389.24301758276));
#43176=CARTESIAN_POINT('Ctrl Pts',(-4.46561156725167,-1.49159971293583,
389.1638897073));
#43177=CARTESIAN_POINT('Ctrl Pts',(-4.63638544725815,0.818832313514199,
389.084761831841));
#43178=CARTESIAN_POINT('Ctrl Pts',(-3.6845363487667,2.93099782801338,389.00563395638));
#43179=CARTESIAN_POINT('Ctrl Pts',(-1.84053856736483,4.33347137468852,388.926506080921));
#43180=CARTESIAN_POINT('Ctrl Pts',(0.449114760160199,4.6866675053185,388.847378205461));
#43181=CARTESIAN_POINT('Ctrl Pts',(2.63002248068729,3.90506570037965,388.768250330001));
#43182=CARTESIAN_POINT('Ctrl Pts',(4.1741143660401,2.17791772857007,388.689122454542));
#43183=CARTESIAN_POINT('Ctrl Pts',(4.70751446239035,-0.0765764950091339,
388.609994579082));
#43184=CARTESIAN_POINT('Ctrl Pts',(4.10106888214441,-2.31252900459844,388.530866703622));
#43185=CARTESIAN_POINT('Ctrl Pts',(2.5016182517638,-3.98854139951492,388.451738828162));
#43186=CARTESIAN_POINT('Ctrl Pts',(0.296442716755053,-4.6987953869992,388.372610952703));
#43187=CARTESIAN_POINT('Ctrl Pts',(-1.98051145042811,-4.27131487576429,
388.293483077243));
#43188=CARTESIAN_POINT('Ctrl Pts',(-3.77791798536176,-2.80960710226223,
388.214355201783));
#43189=CARTESIAN_POINT('Ctrl Pts',(-4.66056504020173,-0.667600089313645,
388.135227326323));
#43190=CARTESIAN_POINT('Ctrl Pts',(-4.41473443363227,1.63605508883523,388.056099450863));
#43191=CARTESIAN_POINT('Ctrl Pts',(-3.09994992417011,3.54356696576203,387.976971575404));
#43192=CARTESIAN_POINT('Ctrl Pts',(-1.03456453032195,4.59306353165313,387.897843699944));
#43193=CARTESIAN_POINT('Ctrl Pts',(1.28132331369787,4.53042679435133,387.818715824484));
#43194=CARTESIAN_POINT('Ctrl Pts',(3.28696020658222,3.37082318930362,387.739587949024));
#43195=CARTESIAN_POINT('Ctrl Pts',(4.49671481157362,1.39503128157636,387.660460073565));
#43196=CARTESIAN_POINT('Ctrl Pts',(4.61766534005973,-0.918544054693783,
387.581332198105));
#43197=CARTESIAN_POINT('Ctrl Pts',(3.6205256500481,-3.00970935316784,387.502204322645));
#43198=CARTESIAN_POINT('Ctrl Pts',(1.74673639428721,-4.37212400808516,387.423076447185));
#43199=CARTESIAN_POINT('Ctrl Pts',(-0.549995784557234,-4.67590216002981,
387.343948571725));
#43200=CARTESIAN_POINT('Ctrl Pts',(-2.71355570823769,-3.84748902421993,
387.264820696266));
#43201=CARTESIAN_POINT('Ctrl Pts',(-4.22007362664152,-2.08747094804379,
387.185692820806));
#43202=CARTESIAN_POINT('Ctrl Pts',(-4.70477149187816,0.177993208894804,
387.106564945346));
#43203=CARTESIAN_POINT('Ctrl Pts',(-4.05028784482536,2.40035929545185,387.027437069887));
#43204=CARTESIAN_POINT('Ctrl Pts',(-2.41509492416788,4.04151863542169,386.948309194426));
#43205=CARTESIAN_POINT('Ctrl Pts',(-0.195127271563123,4.70409201877413,
386.869181318967));
#43206=CARTESIAN_POINT('Ctrl Pts',(2.0720871773402,4.22764841285371,386.790053443507));
#43207=CARTESIAN_POINT('Ctrl Pts',(3.83758046755327,2.72755064632278,386.710925568048));
#43208=CARTESIAN_POINT('Ctrl Pts',(4.67386800821896,0.567022234969233,386.631797692587));
#43209=CARTESIAN_POINT('Ctrl Pts',(4.37845679687603,-1.73080110096229,386.552669817128));
#43210=CARTESIAN_POINT('Ctrl Pts',(3.02287570396291,-3.60953997783552,386.473541941668));
#43211=CARTESIAN_POINT('Ctrl Pts',(0.935355956463039,-4.61428928524331,
386.394414066208));
#43212=CARTESIAN_POINT('Ctrl Pts',(-1.37864454889126,-4.50176582920686,
386.315286190748));
#43213=CARTESIAN_POINT('Ctrl Pts',(-3.35882939819794,-3.29921527745666,
386.236158315289));
#43214=CARTESIAN_POINT('Ctrl Pts',(-4.52573004019154,-1.29781507793296,
386.157030439828));
#43215=CARTESIAN_POINT('Ctrl Pts',(-4.59680105468898,1.01782927684972,386.077902564369));
#43216=CARTESIAN_POINT('Ctrl Pts',(-3.55483378747301,3.08702334241943,385.998774688909));
#43217=CARTESIAN_POINT('Ctrl Pts',(-1.65212313730168,4.40874647858035,385.91964681345));
#43218=CARTESIAN_POINT('Ctrl Pts',(0.650621422548117,4.66296559473944,385.84051893799));
#43219=CARTESIAN_POINT('Ctrl Pts',(2.79582891660295,3.78812579546785,385.76139106253));
#43220=CARTESIAN_POINT('Ctrl Pts',(4.26407332779252,1.99605486608223,385.68226318707));
#43221=CARTESIAN_POINT('Ctrl Pts',(4.69984389610718,-0.279327272972474,
385.603135311611));
#43222=CARTESIAN_POINT('Ctrl Pts',(3.99762608680683,-2.48707499751891,385.52400743615));
#43223=CARTESIAN_POINT('Ctrl Pts',(2.32745016540729,-4.09261922254535,385.444879560691));
#43224=CARTESIAN_POINT('Ctrl Pts',(0.0937212204902381,-4.70720434079847,
385.365751685231));
#43225=CARTESIAN_POINT('Ctrl Pts',(-2.16270074615507,-4.18201887319778,
385.286623809771));
#43226=CARTESIAN_POINT('Ctrl Pts',(-3.89546099811616,-2.64422767275401,
385.207495934311));
#43227=CARTESIAN_POINT('Ctrl Pts',(-4.6850007007776,-0.466181088114491,
385.128368058852));
#43228=CARTESIAN_POINT('Ctrl Pts',(-4.34014605663549,1.82474342861496,385.049240183392));
#43229=CARTESIAN_POINT('Ctrl Pts',(-2.94439783415696,3.67383692716674,384.970112307932));
#43230=CARTESIAN_POINT('Ctrl Pts',(-0.83571305710034,4.63337242830686,384.890984432472));
#43231=CARTESIAN_POINT('Ctrl Pts',(1.47532562085691,4.47101450295627,384.811856557013));
#43232=CARTESIAN_POINT('Ctrl Pts',(3.42913894264361,3.22607539980813,384.732728681553));
#43233=CARTESIAN_POINT('Ctrl Pts',(4.55264378010221,1.19999624361863,384.653600806093));
#43234=CARTESIAN_POINT('Ctrl Pts',(4.57380227931992,-1.11664187763583,384.574472930633));
#43235=CARTESIAN_POINT('Ctrl Pts',(3.4874912645637,-3.1629038955988,384.495345055174));
#43236=CARTESIAN_POINT('Ctrl Pts',(1.55674272936248,-4.44332178080534,384.416217179713));
#43237=CARTESIAN_POINT('Ctrl Pts',(-0.750944949374648,-4.64786381644416,
384.337089304254));
#43238=CARTESIAN_POINT('Ctrl Pts',(-2.87680390283758,-3.72700357899221,
384.257961428794));
#43239=CARTESIAN_POINT('Ctrl Pts',(-4.30609303856287,-1.90371193105537,
384.178833553335));
#43240=CARTESIAN_POINT('Ctrl Pts',(-4.69273396316942,0.380531633531783,
384.099705677874));
#43241=CARTESIAN_POINT('Ctrl Pts',(-3.94310806118005,2.5726358450156,384.020577802415));
#43242=CARTESIAN_POINT('Ctrl Pts',(-2.23872467266656,4.14181943271266,383.941449926955));
#43243=CARTESIAN_POINT('Ctrl Pts',(0.00772834932661786,4.70813090788891,
383.862322051495));
#43244=CARTESIAN_POINT('Ctrl Pts',(2.2523100811437,4.13444744452999,383.783194176035));
#43245=CARTESIAN_POINT('Ctrl Pts',(3.9515327006614,2.55967687195196,383.704066300576));
#43246=CARTESIAN_POINT('Ctrl Pts',(4.69395794849557,0.365123473577542,383.624938425116));
#43247=CARTESIAN_POINT('Ctrl Pts',(4.29982000221476,-1.91783845038001,383.545810549656));
#43248=CARTESIAN_POINT('Ctrl Pts',(2.86455275536081,-3.73642795795088,383.466682674196));
#43249=CARTESIAN_POINT('Ctrl Pts',(0.735682100664791,-4.65030409972978,
383.387554798737));
#43250=CARTESIAN_POINT('Ctrl Pts',(-1.571321636466,-4.43818709474668,383.308426923276));
#43251=CARTESIAN_POINT('Ctrl Pts',(-3.49785619221092,-3.15143751831031,
383.229299047817));
#43252=CARTESIAN_POINT('Ctrl Pts',(-4.57744353411293,-1.10162020007351,
383.150171172357));
#43253=CARTESIAN_POINT('Ctrl Pts',(-4.54867969326092,1.21493597416402,383.071043296898));
#43254=CARTESIAN_POINT('Ctrl Pts',(-3.41852935131432,3.23731577814161,382.991915421438));
#43255=CARTESIAN_POINT('Ctrl Pts',(-1.46063945964488,4.47583385997855,382.912787545978));
#43256=CARTESIAN_POINT('Ctrl Pts',(0.850919780561573,4.6306038375412,382.833659670518));
#43257=CARTESIAN_POINT('Ctrl Pts',(2.95644306681562,3.66415075643457,382.754531795058));
#43258=CARTESIAN_POINT('Ctrl Pts',(4.3461132474158,1.81048502171076,382.675403919598));
#43259=CARTESIAN_POINT('Ctrl Pts',(4.68344499450879,-0.481559297088858,
382.596276044139));
#43260=CARTESIAN_POINT('Ctrl Pts',(3.88675908298024,-2.65700210840579,382.517148168679));
#43261=CARTESIAN_POINT('Ctrl Pts',(2.14895964496101,-4.18909642017598,382.438020293219));
#43262=CARTESIAN_POINT('Ctrl Pts',(-0.109174330542496,-4.70687128980098,
382.358892417759));
#43263=CARTESIAN_POINT('Ctrl Pts',(-2.34087357288517,-4.08495621628556,
382.2797645423));
#43264=CARTESIAN_POINT('Ctrl Pts',(-4.00576953871563,-2.47393750444512,
382.20063666684));
#43265=CARTESIAN_POINT('Ctrl Pts',(-4.7007355921423,-0.263896316701532,
382.12150879138));
#43266=CARTESIAN_POINT('Ctrl Pts',(-4.25749735871386,2.01004293828431,382.04238091592));
#43267=CARTESIAN_POINT('Ctrl Pts',(-2.78337754303629,3.79728400651352,381.963253040461));
#43268=CARTESIAN_POINT('Ctrl Pts',(-0.635309535778666,4.66507643741782,
381.884125165001));
#43269=CARTESIAN_POINT('Ctrl Pts',(1.6665880206908,4.40329884773815,381.804997289541));
#43270=CARTESIAN_POINT('Ctrl Pts',(3.56494923856197,3.07533629050199,381.725869414081));
#43271=CARTESIAN_POINT('Ctrl Pts',(4.60011778664443,1.00273262747343,381.646741538621));
#43272=CARTESIAN_POINT('Ctrl Pts',(4.52144496199587,-1.31266592430991,381.567613663161));
#43273=CARTESIAN_POINT('Ctrl Pts',(3.34798006967052,-3.31022443744999,381.488485787702));
#43274=CARTESIAN_POINT('Ctrl Pts',(1.36385795297921,-4.50626761936056,381.409357912242));
#43275=CARTESIAN_POINT('Ctrl Pts',(-0.950499493547971,-4.6111936725719,
381.330230036783));
#43276=CARTESIAN_POINT('Ctrl Pts',(-3.03470942869027,-3.59959651303038,
381.251102161322));
#43277=CARTESIAN_POINT('Ctrl Pts',(-4.38411537126835,-1.71641742726257,
381.171974285863));
#43278=CARTESIAN_POINT('Ctrl Pts',(-4.67198130338802,0.582363352208024,
381.092846410403));
#43279=CARTESIAN_POINT('Ctrl Pts',(-3.82860531743164,2.74013461284959,381.013718534943));
#43280=CARTESIAN_POINT('Ctrl Pts',(-2.05819676400615,4.23442823222176,380.934590659483));
#43281=CARTESIAN_POINT('Ctrl Pts',(0.210569617479083,4.70342607142888,380.855462784024));
#43282=CARTESIAN_POINT('Ctrl Pts',(2.42835009758821,4.03356816934405,380.776334908564));
#43283=CARTESIAN_POINT('Ctrl Pts',(4.05814632781095,2.38704938266401,380.697207033104));
#43284=CARTESIAN_POINT('Ctrl Pts',(4.70533048456991,0.162546621555695,380.618079157644));
#43285=CARTESIAN_POINT('Ctrl Pts',(4.2131977783341,-2.10131407786716,380.538951282185));
#43286=CARTESIAN_POINT('Ctrl Pts',(2.7009098902828,-3.85637681480619,380.459823406725));
#43287=CARTESIAN_POINT('Ctrl Pts',(0.53464196968763,-4.67768258194704,380.380695531265));
#43288=CARTESIAN_POINT('Ctrl Pts',(-1.76108053730214,-4.36636596202583,
380.301567655805));
#43289=CARTESIAN_POINT('Ctrl Pts',(-3.63038692754518,-2.99780705341609,
380.222439780345));
#43290=CARTESIAN_POINT('Ctrl Pts',(-4.62065600907807,-0.903379443519156,
380.143311904886));
#43291=CARTESIAN_POINT('Ctrl Pts',(-4.49211073176741,1.40978634790602,380.064184029426));
#43292=CARTESIAN_POINT('Ctrl Pts',(-3.27587617866081,3.38159601893615,379.985056153966));
#43293=CARTESIAN_POINT('Ctrl Pts',(-1.26644314913044,4.53460892726404,379.905928278506));
#43294=CARTESIAN_POINT('Ctrl Pts',(1.049637849243,4.58964233450045,379.826800403046));
#43295=CARTESIAN_POINT('Ctrl Pts',(3.11156664606508,3.53337082405704,379.747672527587));
#43296=CARTESIAN_POINT('Ctrl Pts',(4.42008176412018,1.62155282729066,379.668544652127));
#43297=CARTESIAN_POINT('Ctrl Pts',(4.65834821288585,-0.682896991284513,
379.589416776667));
#43298=CARTESIAN_POINT('Ctrl Pts',(3.76867376779785,-2.82199475639389,379.510288901207));
#43299=CARTESIAN_POINT('Ctrl Pts',(1.96647817486303,-4.27779381936408,379.431161025748));
#43300=CARTESIAN_POINT('Ctrl Pts',(-0.311867127997482,-4.69779685253383,
379.352033150288));
#43301=CARTESIAN_POINT('Ctrl Pts',(-2.51469903618647,-3.9803071653586,379.272905274828));
#43302=CARTESIAN_POINT('Ctrl Pts',(-4.1086387471793,-2.29905285245449,379.193777399368));
#43303=CARTESIAN_POINT('Ctrl Pts',(-4.70774049217468,-0.0611214491085228,
379.114649523908));
#43304=CARTESIAN_POINT('Ctrl Pts',(-4.16694183125235,2.19160948806155,379.035521648449));
#43305=CARTESIAN_POINT('Ctrl Pts',(-2.61718809033458,3.91367894352783,378.956393772989));
#43306=CARTESIAN_POINT('Ctrl Pts',(-0.433726146618794,4.68811667974907,
378.877265897529));
#43307=CARTESIAN_POINT('Ctrl Pts',(1.85475530941073,4.32740558711739,378.798138022069));
#43308=CARTESIAN_POINT('Ctrl Pts',(3.69413887366186,2.91888580717067,378.71901014661));
#43309=CARTESIAN_POINT('Ctrl Pts',(4.63904866464471,0.803606782114387,378.63988227115));
#43310=CARTESIAN_POINT('Ctrl Pts',(4.46069062370475,-1.50625214781415,378.56075439569));
#43311=CARTESIAN_POINT('Ctrl Pts',(3.20225115918455,-3.45139738174314,378.48162652023));
#43312=CARTESIAN_POINT('Ctrl Pts',(1.16844028192984,-4.56084462361588,378.40249864477));
#43313=CARTESIAN_POINT('Ctrl Pts',(-1.14828881349689,-4.56595983052853,
378.323370769311));
#43314=CARTESIAN_POINT('Ctrl Pts',(-3.18697903086916,-3.46550444091513,
378.244242893851));
#43315=CARTESIAN_POINT('Ctrl Pts',(-4.45399572524721,-1.5259352714587,378.165115018391));
#43316=CARTESIAN_POINT('Ctrl Pts',(-4.64255205342532,0.783113532278959,
378.085987142931));
#43317=CARTESIAN_POINT('Ctrl Pts',(-3.7069922628433,2.90254452789652,378.006859267472));
#43318=CARTESIAN_POINT('Ctrl Pts',(-1.8738464663689,4.31917304511859,377.927731392012));
#43319=CARTESIAN_POINT('Ctrl Pts',(0.413019825360475,4.68998624700131,377.848603516552));
#43320=CARTESIAN_POINT('Ctrl Pts',(2.59988029319979,3.92519793567579,377.769475641092));
#43321=CARTESIAN_POINT('Ctrl Pts',(4.15722335104551,2.20998877434347,377.690347765632));
#43322=CARTESIAN_POINT('Ctrl Pts',(4.70796449588766,-0.0403321046239016,
377.611219890173));
#43323=CARTESIAN_POINT('Ctrl Pts',(4.11875099606982,-2.28088724087274,377.532092014713));
#43324=CARTESIAN_POINT('Ctrl Pts',(2.53225101877986,-3.9691637848658,377.452964139253));
#43325=CARTESIAN_POINT('Ctrl Pts',(0.332608926075814,-4.69637388582909,
377.373836263793));
#43326=CARTESIAN_POINT('Ctrl Pts',(-1.94756883984043,-4.28643581396986,
377.294708388333));
#43327=CARTESIAN_POINT('Ctrl Pts',(-3.75617547417524,-2.83860919825332,
377.215580512874));
#43328=CARTESIAN_POINT('Ctrl Pts',(-4.65528721285309,-0.703460971943434,
377.136452637414));
#43329=CARTESIAN_POINT('Ctrl Pts',(-4.42719922749879,1.60201853086424,377.057324761954));
#43330=CARTESIAN_POINT('Ctrl Pts',(-3.12713919846579,3.51959611413589,376.978196886494));
#43331=CARTESIAN_POINT('Ctrl Pts',(-1.06989485827222,4.58496252606164,376.899069011035));
#43332=CARTESIAN_POINT('Ctrl Pts',(1.24640657847665,4.54015715746168,376.819941135575));
#43333=CARTESIAN_POINT('Ctrl Pts',(3.26091156592763,3.39602887682211,376.740813260115));
#43334=CARTESIAN_POINT('Ctrl Pts',(4.48584150695881,1.4296091591174,376.661685384655));
#43335=CARTESIAN_POINT('Ctrl Pts',(4.62460015982963,-0.882966440516176,
376.582557509196));
#43336=CARTESIAN_POINT('Ctrl Pts',(3.64358944392086,-2.9817465244189,376.503429633736));
#43337=CARTESIAN_POINT('Ctrl Pts',(1.7803446513398,-4.35854669589912,376.424301758276));
#43338=CARTESIAN_POINT('Ctrl Pts',(-0.513980740029185,-4.67999788047178,
376.345173882816));
#43339=CARTESIAN_POINT('Ctrl Pts',(-2.68385431544624,-3.86826607229696,
376.266046007356));
#43340=CARTESIAN_POINT('Ctrl Pts',(-4.20387757931463,-2.11989849939269,
376.186918131897));
#43341=CARTESIAN_POINT('Ctrl Pts',(-4.7060023921165,0.141766919500427,376.107790256437));
#43342=CARTESIAN_POINT('Ctrl Pts',(-4.0686476489454,2.36910590400946,376.028662380977));
#43343=CARTESIAN_POINT('Ctrl Pts',(-2.44613811739875,4.02280552584175,375.949534505517));
#43344=CARTESIAN_POINT('Ctrl Pts',(-0.231337257081005,4.70245046971741,
375.870406630058));
#43345=CARTESIAN_POINT('Ctrl Pts',(2.03947802286674,4.24347544716049,375.791278754597));
#43346=CARTESIAN_POINT('Ctrl Pts',(3.81646794076225,2.75701496679917,375.712150879138));
#43347=CARTESIAN_POINT('Ctrl Pts',(4.66936407560377,0.602987532497468,375.633023003678));
#43348=CARTESIAN_POINT('Ctrl Pts',(4.39165217497973,-1.6970389500669,375.553895128218));
#43349=CARTESIAN_POINT('Ctrl Pts',(3.05057500604089,-3.58616494858208,375.474767252759));
#43350=CARTESIAN_POINT('Ctrl Pts',(0.970853006392586,-4.60694213867371,
375.395639377299));
#43351=CARTESIAN_POINT('Ctrl Pts',(-1.34394626652729,-4.51226606546036,
375.316511501839));
#43352=CARTESIAN_POINT('Ctrl Pts',(-3.33332776428957,-3.32493525307769,
375.23738362638));
#43353=CARTESIAN_POINT('Ctrl Pts',(-4.51560361732968,-1.33271151243227,
375.158255750919));
#43354=CARTESIAN_POINT('Ctrl Pts',(-4.60446635415931,0.982571567271653,
375.07912787546));
#43355=CARTESIAN_POINT('Ctrl Pts',(-3.92033033613572,2.36677696691101,375.026375958487));
#43356=CARTESIAN_POINT('Ctrl Pts',(-3.43378788736318,2.93584158412846,375.));
#43357=CARTESIAN_POINT('Ctrl Pts',(-4.51766328535307,-0.00011344722995056,
399.112583302492));
#43358=CARTESIAN_POINT('Ctrl Pts',(-4.51713673458649,0.545949625983492,
399.093346914919));
#43359=CARTESIAN_POINT('Ctrl Pts',(-4.41799450573444,1.09219871675483,399.074110527346));
#43360=CARTESIAN_POINT('Ctrl Pts',(-4.22436256903118,1.60260114106826,399.054874139773));
#43361=CARTESIAN_POINT('Ctrl Pts',(-3.95886428330821,2.3024390448317,399.028498181286));
#43362=CARTESIAN_POINT('Ctrl Pts',(-3.51572059597365,2.93488341331845,399.002122222799));
#43363=CARTESIAN_POINT('Ctrl Pts',(-2.94858141451404,3.42336635011963,398.975746264313));
#43364=CARTESIAN_POINT('Ctrl Pts',(-2.38144223305443,3.91184928692081,398.949370305826));
#43365=CARTESIAN_POINT('Ctrl Pts',(-1.69030755746978,4.25637079203641,398.92299434734));
#43366=CARTESIAN_POINT('Ctrl Pts',(-0.958850722305057,4.4152208122577,398.896618388853));
#43367=CARTESIAN_POINT('Ctrl Pts',(-0.227393887140339,4.57407083247899,
398.870242430366));
#43368=CARTESIAN_POINT('Ctrl Pts',(0.544385107604448,4.54724936780597,398.84386647188));
#43369=CARTESIAN_POINT('Ctrl Pts',(1.26304959160632,4.33800360262792,398.817490513393));
#43370=CARTESIAN_POINT('Ctrl Pts',(1.98171407560819,4.12875783744988,398.791114554907));
#43371=CARTESIAN_POINT('Ctrl Pts',(2.64726404886714,3.73708777176682,398.76473859642));
#43372=CARTESIAN_POINT('Ctrl Pts',(3.1791236295575,3.21041157417997,398.738362637933));
#43373=CARTESIAN_POINT('Ctrl Pts',(3.71098321024786,2.68373537659312,398.711986679447));
#43374=CARTESIAN_POINT('Ctrl Pts',(4.10915239836962,2.02205304710248,398.68561072096));
#43375=CARTESIAN_POINT('Ctrl Pts',(4.32542619827246,1.30547222526591,398.659234762474));
#43376=CARTESIAN_POINT('Ctrl Pts',(4.5416999981753,0.588891403429356,398.632858803987));
#43377=CARTESIAN_POINT('Ctrl Pts',(4.57607840985923,-0.182587910753133,
398.6064828455));
#43378=CARTESIAN_POINT('Ctrl Pts',(4.42439935544928,-0.915565328667223,
398.580106887014));
#43379=CARTESIAN_POINT('Ctrl Pts',(4.27272030103931,-1.64854274658133,398.553730928527));
#43380=CARTESIAN_POINT('Ctrl Pts',(3.93498378053545,-2.34301826822704,398.527354970041));
#43381=CARTESIAN_POINT('Ctrl Pts',(3.45207841102396,-2.91491409337733,398.500979011554));
#43382=CARTESIAN_POINT('Ctrl Pts',(2.96917304151247,-3.48680991852761,398.474603053068));
#43383=CARTESIAN_POINT('Ctrl Pts',(2.34109882299336,-3.93612604718246,398.448227094581));
#43384=CARTESIAN_POINT('Ctrl Pts',(1.64389457471586,-4.20846529685206,398.421851136094));
#43385=CARTESIAN_POINT('Ctrl Pts',(0.946690326438348,-4.48080454652167,
398.395475177608));
#43386=CARTESIAN_POINT('Ctrl Pts',(0.180356048402448,-4.57616691720601,
398.369099219121));
#43387=CARTESIAN_POINT('Ctrl Pts',(-0.562330762839376,-4.483007209538,398.342723260635));
#43388=CARTESIAN_POINT('Ctrl Pts',(-1.3050175740812,-4.38984750186999,398.316347302148));
#43389=CARTESIAN_POINT('Ctrl Pts',(-2.02405691852894,-4.10816571584963,
398.289971343661));
#43390=CARTESIAN_POINT('Ctrl Pts',(-2.63239713711321,-3.67206411165684,
398.263595385175));
#43391=CARTESIAN_POINT('Ctrl Pts',(-3.24073735569747,-3.23596250746405,
398.237219426688));
#43392=CARTESIAN_POINT('Ctrl Pts',(-3.73837844841825,-2.64544108509883,
398.210843468202));
#43393=CARTESIAN_POINT('Ctrl Pts',(-4.0650726929841,-1.97199227390868,398.184467509715));
#43394=CARTESIAN_POINT('Ctrl Pts',(-4.36186009740405,-1.36019354158502,
398.160506107307));
#43395=CARTESIAN_POINT('Ctrl Pts',(-4.51756632872819,-0.679955446831048,
398.1365447049));
#43396=CARTESIAN_POINT('Ctrl Pts',(-4.51805439081064,6.66898104614677E-5,
398.112583302492));
#43397=CARTESIAN_POINT('Ctrl Pts',(-1.31303618635555,-4.90075024188347,
400.));
#43398=CARTESIAN_POINT('Ctrl Pts',(-1.45291589482402,-4.85500689927294,
400.));
#43399=CARTESIAN_POINT('Ctrl Pts',(-1.59044602699472,-4.80315746369625,
400.));
#43400=CARTESIAN_POINT('Ctrl Pts',(-1.72529743087534,-4.74548509357023,
400.));
#43401=CARTESIAN_POINT('Ctrl Pts',(-1.86151474898354,-4.68722855814354,
400.));
#43402=CARTESIAN_POINT('Ctrl Pts',(-1.99499946782598,-4.62303013629637,
400.));
#43403=CARTESIAN_POINT('Ctrl Pts',(-2.12539163452376,-4.55313283560557,
400.));
#43404=CARTESIAN_POINT('Ctrl Pts',(-2.25520494367751,-4.48354583407488,
400.));
#43405=CARTESIAN_POINT('Ctrl Pts',(-2.38195370500541,-4.40830995570903,
400.));
#43406=CARTESIAN_POINT('Ctrl Pts',(-2.50525282411489,-4.32762357969483,
400.));
#43407=CARTESIAN_POINT('Ctrl Pts',(-2.6270809920476,-4.24789978736008,400.));
#43408=CARTESIAN_POINT('Ctrl Pts',(-2.74554186145885,-4.1628542844716,400.));
#43409=CARTESIAN_POINT('Ctrl Pts',(-2.86022634881304,-4.07264517835143,
400.));
#43410=CARTESIAN_POINT('Ctrl Pts',(-2.90206457395326,-4.03973585487948,
400.));
#43411=CARTESIAN_POINT('Ctrl Pts',(-2.94339980617641,-4.00613903342865,
400.));
#43412=CARTESIAN_POINT('Ctrl Pts',(-2.98421070502804,-3.97186145992605,
400.));
#43413=CARTESIAN_POINT('Ctrl Pts',(-3.00176471409307,-3.95711763283762,
400.));
#43414=CARTESIAN_POINT('Ctrl Pts',(-3.01922333710064,-3.94224634426854,
400.));
#43415=CARTESIAN_POINT('Ctrl Pts',(-3.0365678292172,-3.92726308267954,400.));
#43416=CARTESIAN_POINT('Ctrl Pts',(-3.14698675201001,-3.83187628245151,
400.));
#43417=CARTESIAN_POINT('Ctrl Pts',(-3.25293553514171,-3.73182827889012,
400.));
#43418=CARTESIAN_POINT('Ctrl Pts',(-3.35406834590596,-3.62734196551097,
400.));
#43419=CARTESIAN_POINT('Ctrl Pts',(-3.36860939901959,-3.61231873990287,
400.));
#43420=CARTESIAN_POINT('Ctrl Pts',(-3.3830508320319,-3.59720369462607,400.));
#43421=CARTESIAN_POINT('Ctrl Pts',(-3.3973915556082,-3.58199742790278,400.));
#43422=CARTESIAN_POINT('Ctrl Pts',(-3.49724054898418,-3.4761219874308,400.));
#43423=CARTESIAN_POINT('Ctrl Pts',(-3.59221081092533,-3.36582685075802,
400.));
#43424=CARTESIAN_POINT('Ctrl Pts',(-3.68210185106465,-3.25150412359693,
400.));
#43425=CARTESIAN_POINT('Ctrl Pts',(-3.77205159485829,-3.13710673758391,
400.));
#43426=CARTESIAN_POINT('Ctrl Pts',(-3.85691583765602,-3.01867577562728,
400.));
#43427=CARTESIAN_POINT('Ctrl Pts',(-3.93644802914845,-2.89657936297904,
400.));
#43428=CARTESIAN_POINT('Ctrl Pts',(-4.00696577927717,-2.78832176115549,
400.));
#43429=CARTESIAN_POINT('Ctrl Pts',(-4.07329120966267,-2.67718185514111,
400.));
#43430=CARTESIAN_POINT('Ctrl Pts',(-4.13521902572865,-2.56340683612714,
400.));
#43431=CARTESIAN_POINT('Ctrl Pts',(-4.14927174249539,-2.53758890455934,
400.));
#43432=CARTESIAN_POINT('Ctrl Pts',(-4.16309787710306,-2.511635261477,400.));
#43433=CARTESIAN_POINT('Ctrl Pts',(-4.17669478808166,-2.48554876582588,
400.));
#43434=CARTESIAN_POINT('Ctrl Pts',(-4.18567658693009,-2.46831664178184,
400.));
#43435=CARTESIAN_POINT('Ctrl Pts',(-4.19455855900594,-2.45102602806576,
400.));
#43436=CARTESIAN_POINT('Ctrl Pts',(-4.20333295387386,-2.43369188245622,
400.));
#43437=CARTESIAN_POINT('Ctrl Pts',(-4.26826574456287,-2.30541472311025,
400.));
#43438=CARTESIAN_POINT('Ctrl Pts',(-4.32740788322074,-2.17457173953832,
400.));
#43439=CARTESIAN_POINT('Ctrl Pts',(-4.38057216155237,-2.04153956135574,
400.));
#43440=CARTESIAN_POINT('Ctrl Pts',(-4.43343069026291,-1.90927245587513,
400.));
#43441=CARTESIAN_POINT('Ctrl Pts',(-4.48038018757078,-1.77484054207341,
400.));
#43442=CARTESIAN_POINT('Ctrl Pts',(-4.52118875294636,-1.63859604986007,
400.));
#43443=CARTESIAN_POINT('Ctrl Pts',(-4.53639547739945,-1.58782650105892,
400.));
#43444=CARTESIAN_POINT('Ctrl Pts',(-4.55074898869301,-1.53680513764063,
400.));
#43445=CARTESIAN_POINT('Ctrl Pts',(-4.56423545493657,-1.48554984951531,
400.));
#43446=CARTESIAN_POINT('Ctrl Pts',(-4.60065397684761,-1.34714132945246,
400.));
#43447=CARTESIAN_POINT('Ctrl Pts',(-4.63075368245775,-1.20702677925683,
400.));
#43448=CARTESIAN_POINT('Ctrl Pts',(-4.65449674508562,-1.06564398750406,
400.));
#43449=CARTESIAN_POINT('Ctrl Pts',(-4.6677938749007,-0.986463581630512,
400.));
#43450=CARTESIAN_POINT('Ctrl Pts',(-4.67909632529634,-0.906885415400295,
400.));
#43451=CARTESIAN_POINT('Ctrl Pts',(-4.68839036132626,-0.826987472477294,
400.));
#43452=CARTESIAN_POINT('Ctrl Pts',(-4.69350021378828,-0.783059656936131,
400.));
#43453=CARTESIAN_POINT('Ctrl Pts',(-4.69800287543295,-0.73903519996531,
400.));
#43454=CARTESIAN_POINT('Ctrl Pts',(-4.70189541038099,-0.69492725727482,
400.));
#43455=CARTESIAN_POINT('Ctrl Pts',(-4.70335699391325,-0.678365442534775,
400.));
#43456=CARTESIAN_POINT('Ctrl Pts',(-4.70473233460286,-0.661793969471143,
400.));
#43457=CARTESIAN_POINT('Ctrl Pts',(-4.70602072340745,-0.645222510455179,
400.));
#43458=CARTESIAN_POINT('Ctrl Pts',(-4.71697947907218,-0.504269275129255,
400.));
#43459=CARTESIAN_POINT('Ctrl Pts',(-4.72166837458957,-0.363132695636631,
400.));
#43460=CARTESIAN_POINT('Ctrl Pts',(-4.7201177742283,-0.222235244668839,
400.));
#43461=CARTESIAN_POINT('Ctrl Pts',(-4.71856870881553,-0.0814772689241232,
400.));
#43462=CARTESIAN_POINT('Ctrl Pts',(-4.71079242396856,0.0590428483946887,
400.));
#43463=CARTESIAN_POINT('Ctrl Pts',(-4.69676735600276,0.19890200600945,400.));
#43464=CARTESIAN_POINT('Ctrl Pts',(-4.68295624998761,0.33662751705272,400.));
#43465=CARTESIAN_POINT('Ctrl Pts',(-4.66308539592085,0.473712790055481,
400.));
#43466=CARTESIAN_POINT('Ctrl Pts',(-4.63708587274883,0.609740845579473,
400.));
#43467=CARTESIAN_POINT('Ctrl Pts',(-4.62194193613231,0.6889730775437,400.));
#43468=CARTESIAN_POINT('Ctrl Pts',(-4.60471782759541,0.767846329349665,
400.));
#43469=CARTESIAN_POINT('Ctrl Pts',(-4.58539250818854,0.846274698465189,
400.));
#43470=CARTESIAN_POINT('Ctrl Pts',(-4.57105296447468,0.904469184344614,
400.));
#43471=CARTESIAN_POINT('Ctrl Pts',(-4.55555640760633,0.962418671522469,
400.));
#43472=CARTESIAN_POINT('Ctrl Pts',(-4.53891410477628,1.02009082935325,400.));
#43473=CARTESIAN_POINT('Ctrl Pts',(-4.53055828962656,1.04904703181158,400.));
#43474=CARTESIAN_POINT('Ctrl Pts',(-4.52191362534324,1.07793330641511,400.));
#43475=CARTESIAN_POINT('Ctrl Pts',(-4.51298141319226,1.1067454537709,400.));
#43476=CARTESIAN_POINT('Ctrl Pts',(-4.50751626468392,1.12437408388872,400.));
#43477=CARTESIAN_POINT('Ctrl Pts',(-4.50194375351087,1.14197390912326,400.));
#43478=CARTESIAN_POINT('Ctrl Pts',(-4.49626740324529,1.15953444897625,400.));
#43479=CARTESIAN_POINT('Ctrl Pts',(-4.45341464273149,1.29210512795207,400.));
#43480=CARTESIAN_POINT('Ctrl Pts',(-4.4046021744809,1.42258699257377,400.));
#43481=CARTESIAN_POINT('Ctrl Pts',(-4.35004408840361,1.55060321390413,400.));
#43482=CARTESIAN_POINT('Ctrl Pts',(-4.29958883856276,1.66899245545036,400.));
#43483=CARTESIAN_POINT('Ctrl Pts',(-4.24421884943669,1.7852731960868,400.));
#43484=CARTESIAN_POINT('Ctrl Pts',(-4.18406982393872,1.89912668839153,400.));
#43485=CARTESIAN_POINT('Ctrl Pts',(-4.15968128005935,1.94529070966877,400.));
#43486=CARTESIAN_POINT('Ctrl Pts',(-4.13450669520302,1.99105541062324,400.));
#43487=CARTESIAN_POINT('Ctrl Pts',(-4.10855377241811,2.03639833327113,400.));
#43488=CARTESIAN_POINT('Ctrl Pts',(-4.09598731345164,2.05835347033207,400.));
#43489=CARTESIAN_POINT('Ctrl Pts',(-4.08323760980602,2.0802109712186,400.));
#43490=CARTESIAN_POINT('Ctrl Pts',(-4.07030781226104,2.10196429342508,400.));
#43491=CARTESIAN_POINT('Ctrl Pts',(-3.9998914613058,2.22043401931249,400.));
#43492=CARTESIAN_POINT('Ctrl Pts',(-3.92427608656828,2.33558378339706,400.));
#43493=CARTESIAN_POINT('Ctrl Pts',(-3.84364635340467,2.44703278518893,400.));
#43494=CARTESIAN_POINT('Ctrl Pts',(-3.76407407271829,2.55702014226977,400.));
#43495=CARTESIAN_POINT('Ctrl Pts',(-3.67961761227173,2.66340373121656,400.));
#43496=CARTESIAN_POINT('Ctrl Pts',(-3.59041821150276,2.76578232711007,400.));
#43497=CARTESIAN_POINT('Ctrl Pts',(-3.56727357293573,2.79234658178586,400.));
#43498=CARTESIAN_POINT('Ctrl Pts',(-3.5438094445685,2.81864098904491,400.));
#43499=CARTESIAN_POINT('Ctrl Pts',(-3.52002794801113,2.84465807439287,400.));
#43500=CARTESIAN_POINT('Ctrl Pts',(-3.49182454546321,2.87551274871592,400.));
#43501=CARTESIAN_POINT('Ctrl Pts',(-3.46317478144493,2.90597739162215,400.));
#43502=CARTESIAN_POINT('Ctrl Pts',(-3.43408816619831,2.93604416807489,400.));
#43503=CARTESIAN_POINT('Origin',(0.,0.,387.));
#43504=CARTESIAN_POINT('Origin',(0.,0.,374.));
#43505=CARTESIAN_POINT('',(-4.,-4.89858719658941E-16,374.));
#43506=CARTESIAN_POINT('Origin',(0.,0.,374.));
#43507=CARTESIAN_POINT('Origin',(-17.,5.,0.));
#43508=CARTESIAN_POINT('',(-16.,5.,400.));
#43509=CARTESIAN_POINT('',(-17.,4.,400.));
#43510=CARTESIAN_POINT('Origin',(-17.,5.,400.));
#43511=CARTESIAN_POINT('',(-17.,4.,0.));
#43512=CARTESIAN_POINT('',(-17.,4.,0.));
#43513=CARTESIAN_POINT('',(-16.,5.,0.));
#43514=CARTESIAN_POINT('Origin',(-17.,5.,0.));
#43515=CARTESIAN_POINT('',(-16.,5.,0.));
#43516=CARTESIAN_POINT('Origin',(-20.,4.,0.));
#43517=CARTESIAN_POINT('',(-19.,4.,400.));
#43518=CARTESIAN_POINT('',(-16.,4.,400.));
#43519=CARTESIAN_POINT('',(-19.,4.,0.));
#43520=CARTESIAN_POINT('',(-19.,4.,0.));
#43521=CARTESIAN_POINT('',(-16.,4.,0.));
#43522=CARTESIAN_POINT('Origin',(0.,0.,400.));
#43523=CARTESIAN_POINT('',(-16.,6.,400.));
#43524=CARTESIAN_POINT('',(-16.,7.,400.));
#43525=CARTESIAN_POINT('',(-15.,7.,400.));
#43526=CARTESIAN_POINT('Origin',(-15.,6.,400.));
#43527=CARTESIAN_POINT('',(-9.,7.,400.));
#43528=CARTESIAN_POINT('',(-8.,7.,400.));
#43529=CARTESIAN_POINT('',(-8.,6.,400.));
#43530=CARTESIAN_POINT('Origin',(-9.,6.,400.));
#43531=CARTESIAN_POINT('',(-8.,-6.,400.));
#43532=CARTESIAN_POINT('',(-8.,-7.,400.));
#43533=CARTESIAN_POINT('',(-9.,-7.,400.));
#43534=CARTESIAN_POINT('Origin',(-9.,-6.,400.));
#43535=CARTESIAN_POINT('',(-15.,-7.,400.));
#43536=CARTESIAN_POINT('',(-16.,-7.,400.));
#43537=CARTESIAN_POINT('',(-16.,-6.,400.));
#43538=CARTESIAN_POINT('Origin',(-15.,-6.,400.));
#43539=CARTESIAN_POINT('',(-16.,-5.,400.));
#43540=CARTESIAN_POINT('',(-16.,-4.,400.));
#43541=CARTESIAN_POINT('',(-17.,-4.,400.));
#43542=CARTESIAN_POINT('Origin',(-17.,-5.,400.));
#43543=CARTESIAN_POINT('',(-19.,-4.,400.));
#43544=CARTESIAN_POINT('',(-20.,-4.,400.));
#43545=CARTESIAN_POINT('',(-20.,-5.,400.));
#43546=CARTESIAN_POINT('Origin',(-19.,-5.,400.));
#43547=CARTESIAN_POINT('',(-20.,-19.,400.));
#43548=CARTESIAN_POINT('',(-20.,-20.,400.));
#43549=CARTESIAN_POINT('',(-19.,-20.,400.));
#43550=CARTESIAN_POINT('Origin',(-19.,-19.,400.));
#43551=CARTESIAN_POINT('',(-5.,-20.,400.));
#43552=CARTESIAN_POINT('',(-4.,-20.,400.));
#43553=CARTESIAN_POINT('',(-4.,-19.,400.));
#43554=CARTESIAN_POINT('Origin',(-5.,-19.,400.));
#43555=CARTESIAN_POINT('',(-4.,-17.,400.));
#43556=CARTESIAN_POINT('',(-4.,-16.,400.));
#43557=CARTESIAN_POINT('',(-5.,-16.,400.));
#43558=CARTESIAN_POINT('Origin',(-5.,-17.,400.));
#43559=CARTESIAN_POINT('',(-6.,-16.,400.));
#43560=CARTESIAN_POINT('',(-7.,-16.,400.));
#43561=CARTESIAN_POINT('',(-7.,-15.,400.));
#43562=CARTESIAN_POINT('Origin',(-6.,-15.,400.));
#43563=CARTESIAN_POINT('',(-7.,-9.,400.));
#43564=CARTESIAN_POINT('',(-7.,-8.,400.));
#43565=CARTESIAN_POINT('',(-6.,-8.,400.));
#43566=CARTESIAN_POINT('Origin',(-6.,-9.,400.));
#43567=CARTESIAN_POINT('',(6.,-8.,400.));
#43568=CARTESIAN_POINT('',(7.,-8.,400.));
#43569=CARTESIAN_POINT('',(7.,-9.,400.));
#43570=CARTESIAN_POINT('Origin',(6.,-9.,400.));
#43571=CARTESIAN_POINT('',(7.,-15.,400.));
#43572=CARTESIAN_POINT('',(7.,-16.,400.));
#43573=CARTESIAN_POINT('',(6.,-16.,400.));
#43574=CARTESIAN_POINT('Origin',(6.,-15.,400.));
#43575=CARTESIAN_POINT('',(5.,-16.,400.));
#43576=CARTESIAN_POINT('',(4.,-16.,400.));
#43577=CARTESIAN_POINT('',(4.,-17.,400.));
#43578=CARTESIAN_POINT('Origin',(5.,-17.,400.));
#43579=CARTESIAN_POINT('',(4.,-19.,400.));
#43580=CARTESIAN_POINT('',(4.,-20.,400.));
#43581=CARTESIAN_POINT('',(5.,-20.,400.));
#43582=CARTESIAN_POINT('Origin',(5.,-19.,400.));
#43583=CARTESIAN_POINT('',(19.,-20.,400.));
#43584=CARTESIAN_POINT('',(20.,-20.,400.));
#43585=CARTESIAN_POINT('',(20.,-19.,400.));
#43586=CARTESIAN_POINT('Origin',(19.,-19.,400.));
#43587=CARTESIAN_POINT('',(20.,-5.,400.));
#43588=CARTESIAN_POINT('',(20.,-4.,400.));
#43589=CARTESIAN_POINT('',(19.,-4.,400.));
#43590=CARTESIAN_POINT('Origin',(19.,-5.,400.));
#43591=CARTESIAN_POINT('',(17.,-4.,400.));
#43592=CARTESIAN_POINT('',(16.,-4.,400.));
#43593=CARTESIAN_POINT('',(16.,-5.,400.));
#43594=CARTESIAN_POINT('Origin',(17.,-5.,400.));
#43595=CARTESIAN_POINT('',(16.,-6.,400.));
#43596=CARTESIAN_POINT('',(16.,-7.,400.));
#43597=CARTESIAN_POINT('',(15.,-7.,400.));
#43598=CARTESIAN_POINT('Origin',(15.,-6.,400.));
#43599=CARTESIAN_POINT('',(9.,-7.,400.));
#43600=CARTESIAN_POINT('',(8.,-7.,400.));
#43601=CARTESIAN_POINT('',(8.,-6.,400.));
#43602=CARTESIAN_POINT('Origin',(9.,-6.,400.));
#43603=CARTESIAN_POINT('',(8.,6.,400.));
#43604=CARTESIAN_POINT('',(8.,7.,400.));
#43605=CARTESIAN_POINT('',(9.,7.,400.));
#43606=CARTESIAN_POINT('Origin',(9.,6.,400.));
#43607=CARTESIAN_POINT('',(15.,7.,400.));
#43608=CARTESIAN_POINT('',(16.,7.,400.));
#43609=CARTESIAN_POINT('',(16.,6.,400.));
#43610=CARTESIAN_POINT('Origin',(15.,6.,400.));
#43611=CARTESIAN_POINT('',(16.,5.,400.));
#43612=CARTESIAN_POINT('',(16.,4.,400.));
#43613=CARTESIAN_POINT('',(17.,4.,400.));
#43614=CARTESIAN_POINT('Origin',(17.,5.,400.));
#43615=CARTESIAN_POINT('',(19.,4.,400.));
#43616=CARTESIAN_POINT('',(20.,4.,400.));
#43617=CARTESIAN_POINT('',(20.,5.,400.));
#43618=CARTESIAN_POINT('Origin',(19.,5.,400.));
#43619=CARTESIAN_POINT('',(20.,19.,400.));
#43620=CARTESIAN_POINT('',(20.,20.,400.));
#43621=CARTESIAN_POINT('',(19.,20.,400.));
#43622=CARTESIAN_POINT('Origin',(19.,19.,400.));
#43623=CARTESIAN_POINT('',(5.,20.,400.));
#43624=CARTESIAN_POINT('',(4.,20.,400.));
#43625=CARTESIAN_POINT('',(4.,19.,400.));
#43626=CARTESIAN_POINT('Origin',(5.,19.,400.));
#43627=CARTESIAN_POINT('',(4.,17.,400.));
#43628=CARTESIAN_POINT('',(4.,16.,400.));
#43629=CARTESIAN_POINT('',(5.,16.,400.));
#43630=CARTESIAN_POINT('Origin',(5.,17.,400.));
#43631=CARTESIAN_POINT('',(6.,16.,400.));
#43632=CARTESIAN_POINT('',(7.,16.,400.));
#43633=CARTESIAN_POINT('',(7.,15.,400.));
#43634=CARTESIAN_POINT('Origin',(6.,15.,400.));
#43635=CARTESIAN_POINT('',(7.,9.,400.));
#43636=CARTESIAN_POINT('',(7.,8.,400.));
#43637=CARTESIAN_POINT('',(6.,8.,400.));
#43638=CARTESIAN_POINT('Origin',(6.,9.,400.));
#43639=CARTESIAN_POINT('',(-6.,8.,400.));
#43640=CARTESIAN_POINT('',(-7.,8.,400.));
#43641=CARTESIAN_POINT('',(-7.,9.,400.));
#43642=CARTESIAN_POINT('Origin',(-6.,9.,400.));
#43643=CARTESIAN_POINT('',(-7.,15.,400.));
#43644=CARTESIAN_POINT('',(-7.,16.,400.));
#43645=CARTESIAN_POINT('',(-6.,16.,400.));
#43646=CARTESIAN_POINT('Origin',(-6.,15.,400.));
#43647=CARTESIAN_POINT('',(-5.,16.,400.));
#43648=CARTESIAN_POINT('',(-4.,16.,400.));
#43649=CARTESIAN_POINT('',(-4.,17.,400.));
#43650=CARTESIAN_POINT('Origin',(-5.,17.,400.));
#43651=CARTESIAN_POINT('',(-4.,19.,400.));
#43652=CARTESIAN_POINT('',(-4.,20.,400.));
#43653=CARTESIAN_POINT('',(-5.,20.,400.));
#43654=CARTESIAN_POINT('Origin',(-5.,19.,400.));
#43655=CARTESIAN_POINT('',(-19.,20.,400.));
#43656=CARTESIAN_POINT('',(-20.,20.,400.));
#43657=CARTESIAN_POINT('',(-20.,19.,400.));
#43658=CARTESIAN_POINT('Origin',(-19.,19.,400.));
#43659=CARTESIAN_POINT('',(-20.,5.,400.));
#43660=CARTESIAN_POINT('',(-20.,4.,400.));
#43661=CARTESIAN_POINT('Origin',(-19.,5.,400.));
#43662=CARTESIAN_POINT('',(-15.,-12.,400.));
#43663=CARTESIAN_POINT('Origin',(-12.,-12.,400.));
#43664=CARTESIAN_POINT('',(9.,12.,400.));
#43665=CARTESIAN_POINT('Origin',(12.,12.,400.));
#43666=CARTESIAN_POINT('',(-15.,12.,400.));
#43667=CARTESIAN_POINT('Origin',(-12.,12.,400.));
#43668=CARTESIAN_POINT('',(9.,-12.,400.));
#43669=CARTESIAN_POINT('Origin',(12.,-12.,400.));
#43670=CARTESIAN_POINT('Origin',(-15.,6.,0.));
#43671=CARTESIAN_POINT('',(-16.,6.,0.));
#43672=CARTESIAN_POINT('',(-15.,7.,0.));
#43673=CARTESIAN_POINT('Origin',(-15.,6.,0.));
#43674=CARTESIAN_POINT('',(-15.,7.,0.));
#43675=CARTESIAN_POINT('',(-16.,6.,0.));
#43676=CARTESIAN_POINT('Origin',(-16.,7.,0.));
#43677=CARTESIAN_POINT('',(-9.,7.,0.));
#43678=CARTESIAN_POINT('',(-8.,7.,0.));
#43679=CARTESIAN_POINT('',(-9.,7.,0.));
#43680=CARTESIAN_POINT('Origin',(-9.,6.,0.));
#43681=CARTESIAN_POINT('',(-8.,6.,0.));
#43682=CARTESIAN_POINT('Origin',(-9.,6.,0.));
#43683=CARTESIAN_POINT('',(-8.,6.,0.));
#43684=CARTESIAN_POINT('Origin',(-8.,7.,0.));
#43685=CARTESIAN_POINT('',(-8.,-6.,0.));
#43686=CARTESIAN_POINT('',(-8.,-7.,0.));
#43687=CARTESIAN_POINT('',(-8.,-6.,0.));
#43688=CARTESIAN_POINT('Origin',(-9.,-6.,0.));
#43689=CARTESIAN_POINT('',(-9.,-7.,0.));
#43690=CARTESIAN_POINT('Origin',(-9.,-6.,0.));
#43691=CARTESIAN_POINT('',(-9.,-7.,0.));
#43692=CARTESIAN_POINT('Origin',(-8.,-7.,0.));
#43693=CARTESIAN_POINT('',(-15.,-7.,0.));
#43694=CARTESIAN_POINT('',(-16.,-7.,0.));
#43695=CARTESIAN_POINT('',(-15.,-7.,0.));
#43696=CARTESIAN_POINT('Origin',(-15.,-6.,0.));
#43697=CARTESIAN_POINT('',(-16.,-6.,0.));
#43698=CARTESIAN_POINT('Origin',(-15.,-6.,0.));
#43699=CARTESIAN_POINT('',(-16.,-6.,0.));
#43700=CARTESIAN_POINT('Origin',(-16.,-7.,0.));
#43701=CARTESIAN_POINT('',(-16.,-5.,0.));
#43702=CARTESIAN_POINT('',(-16.,-4.,0.));
#43703=CARTESIAN_POINT('',(-16.,-5.,0.));
#43704=CARTESIAN_POINT('Origin',(-17.,-5.,0.));
#43705=CARTESIAN_POINT('',(-17.,-4.,0.));
#43706=CARTESIAN_POINT('Origin',(-17.,-5.,0.));
#43707=CARTESIAN_POINT('',(-17.,-4.,0.));
#43708=CARTESIAN_POINT('Origin',(-19.,-5.,0.));
#43709=CARTESIAN_POINT('',(-19.,-4.,0.));
#43710=CARTESIAN_POINT('',(-19.,-4.,0.));
#43711=CARTESIAN_POINT('',(-20.,-5.,0.));
#43712=CARTESIAN_POINT('Origin',(-19.,-5.,0.));
#43713=CARTESIAN_POINT('',(-20.,-5.,0.));
#43714=CARTESIAN_POINT('Origin',(-20.,-4.,0.));
#43715=CARTESIAN_POINT('',(-20.,-19.,0.));
#43716=CARTESIAN_POINT('',(-20.,-20.,0.));
#43717=CARTESIAN_POINT('',(-20.,-19.,0.));
#43718=CARTESIAN_POINT('Origin',(-19.,-19.,0.));
#43719=CARTESIAN_POINT('',(-19.,-20.,0.));
#43720=CARTESIAN_POINT('Origin',(-19.,-19.,0.));
#43721=CARTESIAN_POINT('',(-19.,-20.,0.));
#43722=CARTESIAN_POINT('Origin',(-5.,-19.,0.));
#43723=CARTESIAN_POINT('',(-5.,-20.,0.));
#43724=CARTESIAN_POINT('',(-5.,-20.,0.));
#43725=CARTESIAN_POINT('',(-4.,-19.,0.));
#43726=CARTESIAN_POINT('Origin',(-5.,-19.,0.));
#43727=CARTESIAN_POINT('',(-4.,-19.,0.));
#43728=CARTESIAN_POINT('Origin',(-4.,-20.,0.));
#43729=CARTESIAN_POINT('',(-4.,-17.,0.));
#43730=CARTESIAN_POINT('',(-4.,-16.,0.));
#43731=CARTESIAN_POINT('',(-4.,-17.,0.));
#43732=CARTESIAN_POINT('Origin',(-5.,-17.,0.));
#43733=CARTESIAN_POINT('',(-5.,-16.,0.));
#43734=CARTESIAN_POINT('Origin',(-5.,-17.,0.));
#43735=CARTESIAN_POINT('',(-5.,-16.,0.));
#43736=CARTESIAN_POINT('Origin',(-6.,-15.,0.));
#43737=CARTESIAN_POINT('',(-6.,-16.,0.));
#43738=CARTESIAN_POINT('',(-7.,-15.,0.));
#43739=CARTESIAN_POINT('Origin',(-6.,-15.,0.));
#43740=CARTESIAN_POINT('',(-7.,-15.,0.));
#43741=CARTESIAN_POINT('',(-6.,-16.,0.));
#43742=CARTESIAN_POINT('Origin',(-7.,-16.,0.));
#43743=CARTESIAN_POINT('',(-7.,-9.,0.));
#43744=CARTESIAN_POINT('',(-7.,-8.,0.));
#43745=CARTESIAN_POINT('',(-7.,-9.,0.));
#43746=CARTESIAN_POINT('Origin',(-6.,-9.,0.));
#43747=CARTESIAN_POINT('',(-6.,-8.,0.));
#43748=CARTESIAN_POINT('Origin',(-6.,-9.,0.));
#43749=CARTESIAN_POINT('',(-6.,-8.,0.));
#43750=CARTESIAN_POINT('Origin',(-7.,-8.,0.));
#43751=CARTESIAN_POINT('',(6.,-8.,0.));
#43752=CARTESIAN_POINT('',(7.,-8.,0.));
#43753=CARTESIAN_POINT('',(6.,-8.,0.));
#43754=CARTESIAN_POINT('Origin',(6.,-9.,0.));
#43755=CARTESIAN_POINT('',(7.,-9.,0.));
#43756=CARTESIAN_POINT('Origin',(6.,-9.,0.));
#43757=CARTESIAN_POINT('',(7.,-9.,0.));
#43758=CARTESIAN_POINT('Origin',(7.,-8.,0.));
#43759=CARTESIAN_POINT('',(7.,-15.,0.));
#43760=CARTESIAN_POINT('',(7.,-16.,0.));
#43761=CARTESIAN_POINT('',(7.,-15.,0.));
#43762=CARTESIAN_POINT('Origin',(6.,-15.,0.));
#43763=CARTESIAN_POINT('',(6.,-16.,0.));
#43764=CARTESIAN_POINT('Origin',(6.,-15.,0.));
#43765=CARTESIAN_POINT('',(6.,-16.,0.));
#43766=CARTESIAN_POINT('Origin',(7.,-16.,0.));
#43767=CARTESIAN_POINT('',(5.,-16.,0.));
#43768=CARTESIAN_POINT('',(4.,-16.,0.));
#43769=CARTESIAN_POINT('',(5.,-16.,0.));
#43770=CARTESIAN_POINT('Origin',(5.,-17.,0.));
#43771=CARTESIAN_POINT('',(4.,-17.,0.));
#43772=CARTESIAN_POINT('Origin',(5.,-17.,0.));
#43773=CARTESIAN_POINT('',(4.,-17.,0.));
#43774=CARTESIAN_POINT('Origin',(5.,-19.,0.));
#43775=CARTESIAN_POINT('',(4.,-19.,0.));
#43776=CARTESIAN_POINT('',(4.,-19.,0.));
#43777=CARTESIAN_POINT('',(5.,-20.,0.));
#43778=CARTESIAN_POINT('Origin',(5.,-19.,0.));
#43779=CARTESIAN_POINT('',(5.,-20.,0.));
#43780=CARTESIAN_POINT('Origin',(4.,-20.,0.));
#43781=CARTESIAN_POINT('',(19.,-20.,0.));
#43782=CARTESIAN_POINT('',(20.,-20.,0.));
#43783=CARTESIAN_POINT('',(19.,-20.,0.));
#43784=CARTESIAN_POINT('Origin',(19.,-19.,0.));
#43785=CARTESIAN_POINT('',(20.,-19.,0.));
#43786=CARTESIAN_POINT('Origin',(19.,-19.,0.));
#43787=CARTESIAN_POINT('',(20.,-19.,0.));
#43788=CARTESIAN_POINT('Origin',(19.,-5.,0.));
#43789=CARTESIAN_POINT('',(20.,-5.,0.));
#43790=CARTESIAN_POINT('',(20.,-5.,0.));
#43791=CARTESIAN_POINT('',(19.,-4.,0.));
#43792=CARTESIAN_POINT('Origin',(19.,-5.,0.));
#43793=CARTESIAN_POINT('',(19.,-4.,0.));
#43794=CARTESIAN_POINT('Origin',(20.,-4.,0.));
#43795=CARTESIAN_POINT('',(17.,-4.,0.));
#43796=CARTESIAN_POINT('',(16.,-4.,0.));
#43797=CARTESIAN_POINT('',(17.,-4.,0.));
#43798=CARTESIAN_POINT('Origin',(17.,-5.,0.));
#43799=CARTESIAN_POINT('',(16.,-5.,0.));
#43800=CARTESIAN_POINT('Origin',(17.,-5.,0.));
#43801=CARTESIAN_POINT('',(16.,-5.,0.));
#43802=CARTESIAN_POINT('Origin',(15.,-6.,0.));
#43803=CARTESIAN_POINT('',(16.,-6.,0.));
#43804=CARTESIAN_POINT('',(15.,-7.,0.));
#43805=CARTESIAN_POINT('Origin',(15.,-6.,0.));
#43806=CARTESIAN_POINT('',(15.,-7.,0.));
#43807=CARTESIAN_POINT('',(16.,-6.,0.));
#43808=CARTESIAN_POINT('Origin',(16.,-7.,0.));
#43809=CARTESIAN_POINT('',(9.,-7.,0.));
#43810=CARTESIAN_POINT('',(8.,-7.,0.));
#43811=CARTESIAN_POINT('',(9.,-7.,0.));
#43812=CARTESIAN_POINT('Origin',(9.,-6.,0.));
#43813=CARTESIAN_POINT('',(8.,-6.,0.));
#43814=CARTESIAN_POINT('Origin',(9.,-6.,0.));
#43815=CARTESIAN_POINT('',(8.,-6.,0.));
#43816=CARTESIAN_POINT('Origin',(8.,-7.,0.));
#43817=CARTESIAN_POINT('',(8.,6.,0.));
#43818=CARTESIAN_POINT('',(8.,7.,0.));
#43819=CARTESIAN_POINT('',(8.,6.,0.));
#43820=CARTESIAN_POINT('Origin',(9.,6.,0.));
#43821=CARTESIAN_POINT('',(9.,7.,0.));
#43822=CARTESIAN_POINT('Origin',(9.,6.,0.));
#43823=CARTESIAN_POINT('',(9.,7.,0.));
#43824=CARTESIAN_POINT('Origin',(8.,7.,0.));
#43825=CARTESIAN_POINT('',(15.,7.,0.));
#43826=CARTESIAN_POINT('',(16.,7.,0.));
#43827=CARTESIAN_POINT('',(15.,7.,0.));
#43828=CARTESIAN_POINT('Origin',(15.,6.,0.));
#43829=CARTESIAN_POINT('',(16.,6.,0.));
#43830=CARTESIAN_POINT('Origin',(15.,6.,0.));
#43831=CARTESIAN_POINT('',(16.,6.,0.));
#43832=CARTESIAN_POINT('Origin',(16.,7.,0.));
#43833=CARTESIAN_POINT('',(16.,5.,0.));
#43834=CARTESIAN_POINT('',(16.,4.,0.));
#43835=CARTESIAN_POINT('',(16.,5.,0.));
#43836=CARTESIAN_POINT('Origin',(17.,5.,0.));
#43837=CARTESIAN_POINT('',(17.,4.,0.));
#43838=CARTESIAN_POINT('Origin',(17.,5.,0.));
#43839=CARTESIAN_POINT('',(17.,4.,0.));
#43840=CARTESIAN_POINT('Origin',(19.,5.,0.));
#43841=CARTESIAN_POINT('',(19.,4.,0.));
#43842=CARTESIAN_POINT('',(19.,4.,0.));
#43843=CARTESIAN_POINT('',(20.,5.,0.));
#43844=CARTESIAN_POINT('Origin',(19.,5.,0.));
#43845=CARTESIAN_POINT('',(20.,5.,0.));
#43846=CARTESIAN_POINT('Origin',(20.,4.,0.));
#43847=CARTESIAN_POINT('',(20.,19.,0.));
#43848=CARTESIAN_POINT('',(20.,20.,0.));
#43849=CARTESIAN_POINT('',(20.,19.,0.));
#43850=CARTESIAN_POINT('Origin',(19.,19.,0.));
#43851=CARTESIAN_POINT('',(19.,20.,0.));
#43852=CARTESIAN_POINT('Origin',(19.,19.,0.));
#43853=CARTESIAN_POINT('',(19.,20.,0.));
#43854=CARTESIAN_POINT('Origin',(5.,19.,0.));
#43855=CARTESIAN_POINT('',(5.,20.,0.));
#43856=CARTESIAN_POINT('',(5.,20.,0.));
#43857=CARTESIAN_POINT('',(4.,19.,0.));
#43858=CARTESIAN_POINT('Origin',(5.,19.,0.));
#43859=CARTESIAN_POINT('',(4.,19.,0.));
#43860=CARTESIAN_POINT('Origin',(4.,20.,0.));
#43861=CARTESIAN_POINT('',(4.,17.,0.));
#43862=CARTESIAN_POINT('',(4.,16.,0.));
#43863=CARTESIAN_POINT('',(4.,17.,0.));
#43864=CARTESIAN_POINT('Origin',(5.,17.,0.));
#43865=CARTESIAN_POINT('',(5.,16.,0.));
#43866=CARTESIAN_POINT('Origin',(5.,17.,0.));
#43867=CARTESIAN_POINT('',(5.,16.,0.));
#43868=CARTESIAN_POINT('Origin',(6.,15.,0.));
#43869=CARTESIAN_POINT('',(6.,16.,0.));
#43870=CARTESIAN_POINT('',(7.,15.,0.));
#43871=CARTESIAN_POINT('Origin',(6.,15.,0.));
#43872=CARTESIAN_POINT('',(7.,15.,0.));
#43873=CARTESIAN_POINT('',(6.,16.,0.));
#43874=CARTESIAN_POINT('Origin',(7.,16.,0.));
#43875=CARTESIAN_POINT('',(7.,9.,0.));
#43876=CARTESIAN_POINT('',(7.,8.,0.));
#43877=CARTESIAN_POINT('',(7.,9.,0.));
#43878=CARTESIAN_POINT('Origin',(6.,9.,0.));
#43879=CARTESIAN_POINT('',(6.,8.,0.));
#43880=CARTESIAN_POINT('Origin',(6.,9.,0.));
#43881=CARTESIAN_POINT('',(6.,8.,0.));
#43882=CARTESIAN_POINT('Origin',(7.,8.,0.));
#43883=CARTESIAN_POINT('',(-6.,8.,0.));
#43884=CARTESIAN_POINT('',(-7.,8.,0.));
#43885=CARTESIAN_POINT('',(-6.,8.,0.));
#43886=CARTESIAN_POINT('Origin',(-6.,9.,0.));
#43887=CARTESIAN_POINT('',(-7.,9.,0.));
#43888=CARTESIAN_POINT('Origin',(-6.,9.,0.));
#43889=CARTESIAN_POINT('',(-7.,9.,0.));
#43890=CARTESIAN_POINT('Origin',(-7.,8.,0.));
#43891=CARTESIAN_POINT('',(-7.,15.,0.));
#43892=CARTESIAN_POINT('',(-7.,16.,0.));
#43893=CARTESIAN_POINT('',(-7.,15.,0.));
#43894=CARTESIAN_POINT('Origin',(-6.,15.,0.));
#43895=CARTESIAN_POINT('',(-6.,16.,0.));
#43896=CARTESIAN_POINT('Origin',(-6.,15.,0.));
#43897=CARTESIAN_POINT('',(-6.,16.,0.));
#43898=CARTESIAN_POINT('Origin',(-7.,16.,0.));
#43899=CARTESIAN_POINT('',(-5.,16.,0.));
#43900=CARTESIAN_POINT('',(-4.,16.,0.));
#43901=CARTESIAN_POINT('',(-5.,16.,0.));
#43902=CARTESIAN_POINT('Origin',(-5.,17.,0.));
#43903=CARTESIAN_POINT('',(-4.,17.,0.));
#43904=CARTESIAN_POINT('Origin',(-5.,17.,0.));
#43905=CARTESIAN_POINT('',(-4.,17.,0.));
#43906=CARTESIAN_POINT('Origin',(-5.,19.,0.));
#43907=CARTESIAN_POINT('',(-4.,19.,0.));
#43908=CARTESIAN_POINT('',(-4.,19.,0.));
#43909=CARTESIAN_POINT('',(-5.,20.,0.));
#43910=CARTESIAN_POINT('Origin',(-5.,19.,0.));
#43911=CARTESIAN_POINT('',(-5.,20.,0.));
#43912=CARTESIAN_POINT('Origin',(-4.,20.,0.));
#43913=CARTESIAN_POINT('',(-19.,20.,0.));
#43914=CARTESIAN_POINT('',(-20.,20.,0.));
#43915=CARTESIAN_POINT('',(-19.,20.,0.));
#43916=CARTESIAN_POINT('Origin',(-19.,19.,0.));
#43917=CARTESIAN_POINT('',(-20.,19.,0.));
#43918=CARTESIAN_POINT('Origin',(-19.,19.,0.));
#43919=CARTESIAN_POINT('',(-20.,19.,0.));
#43920=CARTESIAN_POINT('Origin',(-19.,5.,0.));
#43921=CARTESIAN_POINT('',(-20.,5.,0.));
#43922=CARTESIAN_POINT('',(-20.,5.,0.));
#43923=CARTESIAN_POINT('Origin',(-19.,5.,0.));
#43924=CARTESIAN_POINT('Origin',(12.,-12.,0.));
#43925=CARTESIAN_POINT('',(9.,-12.,0.));
#43926=CARTESIAN_POINT('',(9.,-12.,0.));
#43927=CARTESIAN_POINT('Origin',(12.,-12.,0.));
#43928=CARTESIAN_POINT('Origin',(-12.,12.,0.));
#43929=CARTESIAN_POINT('',(-15.,12.,0.));
#43930=CARTESIAN_POINT('',(-15.,12.,0.));
#43931=CARTESIAN_POINT('Origin',(-12.,12.,0.));
#43932=CARTESIAN_POINT('Origin',(0.,0.,0.));
#43933=CARTESIAN_POINT('',(-4.,-4.89858719658941E-16,0.));
#43934=CARTESIAN_POINT('Origin',(12.,12.,0.));
#43935=CARTESIAN_POINT('',(9.,12.,0.));
#43936=CARTESIAN_POINT('',(9.,12.,0.));
#43937=CARTESIAN_POINT('Origin',(12.,12.,0.));
#43938=CARTESIAN_POINT('Origin',(-12.,-12.,0.));
#43939=CARTESIAN_POINT('',(-15.,-12.,0.));
#43940=CARTESIAN_POINT('',(-15.,-12.,0.));
#43941=CARTESIAN_POINT('Origin',(-12.,-12.,0.));
#43942=CARTESIAN_POINT('Origin',(-20.,20.,0.));
#43943=CARTESIAN_POINT('',(-20.,4.,0.));
#43944=CARTESIAN_POINT('Origin',(-4.,16.,0.));
#43945=CARTESIAN_POINT('',(-4.,20.,0.));
#43946=CARTESIAN_POINT('Origin',(4.,16.,0.));
#43947=CARTESIAN_POINT('',(7.,16.,0.));
#43948=CARTESIAN_POINT('Origin',(20.,20.,0.));
#43949=CARTESIAN_POINT('',(4.,20.,0.));
#43950=CARTESIAN_POINT('Origin',(16.,4.,0.));
#43951=CARTESIAN_POINT('',(20.,4.,0.));
#43952=CARTESIAN_POINT('Origin',(16.,-4.,0.));
#43953=CARTESIAN_POINT('',(16.,-7.,0.));
#43954=CARTESIAN_POINT('Origin',(20.,-20.,0.));
#43955=CARTESIAN_POINT('',(20.,-4.,0.));
#43956=CARTESIAN_POINT('Origin',(4.,-16.,0.));
#43957=CARTESIAN_POINT('',(4.,-20.,0.));
#43958=CARTESIAN_POINT('Origin',(-4.,-16.,0.));
#43959=CARTESIAN_POINT('',(-7.,-16.,0.));
#43960=CARTESIAN_POINT('Origin',(-20.,-20.,0.));
#43961=CARTESIAN_POINT('',(-4.,-20.,0.));
#43962=CARTESIAN_POINT('Origin',(-16.,-4.,0.));
#43963=CARTESIAN_POINT('',(-20.,-4.,0.));
#43964=CARTESIAN_POINT('Origin',(-16.,4.,0.));
#43965=CARTESIAN_POINT('',(-16.,7.,0.));
#43966=CARTESIAN_POINT('Origin',(0.,0.,0.));
#43967=CARTESIAN_POINT('',(0.,0.,0.));
#43968=CARTESIAN_POINT('Origin',(0.,0.,6.));
#43969=CARTESIAN_POINT('',(-8.5,1.04094977927525E-15,6.));
#43970=CARTESIAN_POINT('Origin',(0.,0.,6.));
#43971=CARTESIAN_POINT('',(-5.5,6.73555739531044E-16,6.));
#43972=CARTESIAN_POINT('Origin',(0.,0.,6.));
#43973=CARTESIAN_POINT('Origin',(0.,0.,11.));
#43974=CARTESIAN_POINT('',(-8.5,1.04094977927525E-15,16.));
#43975=CARTESIAN_POINT('Origin',(0.,0.,16.));
#43976=CARTESIAN_POINT('',(-8.5,1.04094977927525E-15,11.));
#43977=CARTESIAN_POINT('Origin',(0.,0.,8.));
#43978=CARTESIAN_POINT('',(-5.5,6.73555739531044E-16,0.));
#43979=CARTESIAN_POINT('',(-5.5,6.73555739531044E-16,8.));
#43980=CARTESIAN_POINT('Origin',(0.,0.,0.));
#43981=CARTESIAN_POINT('Origin',(35.,-35.,8.));
#43982=CARTESIAN_POINT('',(30.5,-35.,16.));
#43983=CARTESIAN_POINT('Origin',(35.,-35.,16.));
#43984=CARTESIAN_POINT('',(30.5,-35.,0.));
#43985=CARTESIAN_POINT('',(30.5,-35.,8.));
#43986=CARTESIAN_POINT('Origin',(35.,-35.,0.));
#43987=CARTESIAN_POINT('Origin',(-35.,-35.,8.));
#43988=CARTESIAN_POINT('',(-39.5,-35.,16.));
#43989=CARTESIAN_POINT('Origin',(-35.,-35.,16.));
#43990=CARTESIAN_POINT('',(-39.5,-35.,0.));
#43991=CARTESIAN_POINT('',(-39.5,-35.,8.));
#43992=CARTESIAN_POINT('Origin',(-35.,-35.,0.));
#43993=CARTESIAN_POINT('Origin',(-35.,35.,8.));
#43994=CARTESIAN_POINT('',(-39.5,35.,16.));
#43995=CARTESIAN_POINT('Origin',(-35.,35.,16.));
#43996=CARTESIAN_POINT('',(-39.5,35.,0.));
#43997=CARTESIAN_POINT('',(-39.5,35.,8.));
#43998=CARTESIAN_POINT('Origin',(-35.,35.,0.));
#43999=CARTESIAN_POINT('Origin',(35.,35.,8.));
#44000=CARTESIAN_POINT('',(30.5,35.,16.));
#44001=CARTESIAN_POINT('Origin',(35.,35.,16.));
#44002=CARTESIAN_POINT('',(30.5,35.,0.));
#44003=CARTESIAN_POINT('',(30.5,35.,8.));
#44004=CARTESIAN_POINT('Origin',(35.,35.,0.));
#44005=CARTESIAN_POINT('Origin',(50.,50.,0.));
#44006=CARTESIAN_POINT('',(50.,50.,0.));
#44007=CARTESIAN_POINT('',(-50.,50.,0.));
#44008=CARTESIAN_POINT('',(50.,50.,0.));
#44009=CARTESIAN_POINT('',(-50.,50.,16.));
#44010=CARTESIAN_POINT('',(-50.,50.,0.));
#44011=CARTESIAN_POINT('',(50.,50.,16.));
#44012=CARTESIAN_POINT('',(50.,50.,16.));
#44013=CARTESIAN_POINT('',(50.,50.,0.));
#44014=CARTESIAN_POINT('Origin',(50.,-50.,0.));
#44015=CARTESIAN_POINT('',(50.,-50.,0.));
#44016=CARTESIAN_POINT('',(50.,-50.,0.));
#44017=CARTESIAN_POINT('',(50.,-50.,16.));
#44018=CARTESIAN_POINT('',(50.,-50.,16.));
#44019=CARTESIAN_POINT('',(50.,-50.,0.));
#44020=CARTESIAN_POINT('Origin',(-50.,-50.,0.));
#44021=CARTESIAN_POINT('',(-50.,-50.,0.));
#44022=CARTESIAN_POINT('',(-50.,-50.,0.));
#44023=CARTESIAN_POINT('',(-50.,-50.,16.));
#44024=CARTESIAN_POINT('',(-50.,-50.,16.));
#44025=CARTESIAN_POINT('',(-50.,-50.,0.));
#44026=CARTESIAN_POINT('Origin',(-50.,50.,0.));
#44027=CARTESIAN_POINT('',(-50.,50.,0.));
#44028=CARTESIAN_POINT('',(-50.,50.,16.));
#44029=CARTESIAN_POINT('Origin',(0.,0.,16.));
#44030=CARTESIAN_POINT('Origin',(0.,0.,0.));
#44031=CARTESIAN_POINT('',(0.,0.,0.));
#44032=CARTESIAN_POINT('Origin',(0.,0.,0.));
#44033=CARTESIAN_POINT('',(-4.94697864382552,0.00278476180115707,0.322320454656892));
#44034=CARTESIAN_POINT('',(-4.94423617559418,0.00148231834052548,0.177679545343088));
#44035=CARTESIAN_POINT('',(-4.942,-6.05220448138622E-16,0.));
#44036=CARTESIAN_POINT('',(2.16917135428609,4.440502182833,0.));
#44037=CARTESIAN_POINT('Ctrl Pts',(-4.94697864382552,0.00278476180115707,
0.322320454656892));
#44038=CARTESIAN_POINT('Ctrl Pts',(-4.94837427497074,0.191084575140575,
0.316237515399425));
#44039=CARTESIAN_POINT('Ctrl Pts',(-4.93857638297692,0.379246871981659,
0.310154576141959));
#44040=CARTESIAN_POINT('Ctrl Pts',(-4.91710439111276,0.566072733558586,
0.304071636884492));
#44041=CARTESIAN_POINT('Ctrl Pts',(-4.73085624282078,2.18660104746097,0.251308196024277));
#44042=CARTESIAN_POINT('Ctrl Pts',(-3.66626808942587,3.70657817799375,0.198544755164062));
#44043=CARTESIAN_POINT('Ctrl Pts',(-2.20523483873771,4.43248249176653,0.145781314303847));
#44044=CARTESIAN_POINT('Ctrl Pts',(-0.85966080708188,5.10102168731156,0.097187542869231));
#44045=CARTESIAN_POINT('Ctrl Pts',(0.822175421307706,5.09603339682298,0.0485937714346156));
#44046=CARTESIAN_POINT('Ctrl Pts',(2.17571852337094,4.44456444733847,3.90312782094782E-17));
#44047=CARTESIAN_POINT('',(-2.16917135428615,4.44050218283297,0.));
#44048=CARTESIAN_POINT('Origin',(0.,0.,0.));
#44049=CARTESIAN_POINT('Ctrl Pts',(-2.16917135428615,4.44050218283297,1.94289029309402E-15));
#44050=CARTESIAN_POINT('Ctrl Pts',(-2.90569614448719,4.08071213863431,0.0263982667373533));
#44051=CARTESIAN_POINT('Ctrl Pts',(-3.54537901519776,3.53418981917855,0.0527965334747045));
#44052=CARTESIAN_POINT('Ctrl Pts',(-4.02261725675323,2.86672087533204,0.0791948002120558));
#44053=CARTESIAN_POINT('Ctrl Pts',(-4.49985549830871,2.1992519314855,0.105593066949408));
#44054=CARTESIAN_POINT('Ctrl Pts',(-4.81464911070909,1.41083636324821,0.13199133368676));
#44055=CARTESIAN_POINT('Ctrl Pts',(-4.91161341297729,0.598206782831744,
0.158389600424112));
#44056=CARTESIAN_POINT('Ctrl Pts',(-4.93523158039298,0.400269799547603,
0.164819582063771));
#44057=CARTESIAN_POINT('Ctrl Pts',(-4.94592610470609,0.200896217803435,
0.171249563703429));
#44058=CARTESIAN_POINT('Ctrl Pts',(-4.94423617559418,0.00148231834052548,
0.177679545343088));
#44059=CARTESIAN_POINT('Origin',(0.,0.,0.));
#44060=CARTESIAN_POINT('',(-4.93459216488855,0.00173983556611496,1.32232045465689));
#44061=CARTESIAN_POINT('',(-4.93449003509191,0.0016461999684793,1.17767954534309));
#44062=CARTESIAN_POINT('',(-4.942,-6.05220448138622E-16,0.));
#44063=CARTESIAN_POINT('Ctrl Pts',(-4.93459216488855,0.00173983556611496,
1.32232045465689));
#44064=CARTESIAN_POINT('Ctrl Pts',(-4.93685941200801,0.71330292763056,1.29948482722738));
#44065=CARTESIAN_POINT('Ctrl Pts',(-4.79300629668486,1.42399221307712,1.27664919979787));
#44066=CARTESIAN_POINT('Ctrl Pts',(-4.49846232996172,2.06549179869028,1.25381357236836));
#44067=CARTESIAN_POINT('Ctrl Pts',(-3.81789626200921,3.5477250130758,1.20105013150815));
#44068=CARTESIAN_POINT('Ctrl Pts',(-2.33282804601649,4.66057109067704,1.14828669064793));
#44069=CARTESIAN_POINT('Ctrl Pts',(-0.719110050159326,4.89750101325702,
1.09552324978772));
#44070=CARTESIAN_POINT('Ctrl Pts',(0.89460794569784,5.13443093583701,1.0427598089275));
#44071=CARTESIAN_POINT('Ctrl Pts',(2.63697572141945,4.49544470339575,0.989996368067287));
#44072=CARTESIAN_POINT('Ctrl Pts',(3.71488022775187,3.27143294682148,0.937232927207072));
#44073=CARTESIAN_POINT('Ctrl Pts',(4.79278473408429,2.04742119024721,0.884469486346857));
#44074=CARTESIAN_POINT('Ctrl Pts',(5.20622597102753,0.238383909539938,0.831706045486642));
#44075=CARTESIAN_POINT('Ctrl Pts',(4.76722694025552,-1.33245018266074,0.778942604626427));
#44076=CARTESIAN_POINT('Ctrl Pts',(4.32822790948351,-2.90328427486142,0.726179163766212));
#44077=CARTESIAN_POINT('Ctrl Pts',(3.03678861099627,-4.2359151785555,0.673415722905997));
#44078=CARTESIAN_POINT('Ctrl Pts',(1.48031593870399,-4.72357537917557,0.620652282045782));
#44079=CARTESIAN_POINT('Ctrl Pts',(-0.0761567335882804,-5.21123557979564,
0.567888841185567));
#44080=CARTESIAN_POINT('Ctrl Pts',(-1.89766277968558,-4.8539250773417,0.515125400325352));
#44081=CARTESIAN_POINT('Ctrl Pts',(-3.1544617311397,-3.81473007747874,0.462361959465137));
#44082=CARTESIAN_POINT('Ctrl Pts',(-4.26636809113457,-2.89534076044788,
0.415681457862388));
#44083=CARTESIAN_POINT('Ctrl Pts',(-4.93626856451128,-1.44222880258692,
0.36900095625964));
#44084=CARTESIAN_POINT('Ctrl Pts',(-4.94697864382552,0.00278476180115707,
0.322320454656892));
#44085=CARTESIAN_POINT('Ctrl Pts',(-4.94423617559418,0.00148231834052548,
0.177679545343088));
#44086=CARTESIAN_POINT('Ctrl Pts',(-4.93205010879707,-1.4364898912607,0.224046097178133));
#44087=CARTESIAN_POINT('Ctrl Pts',(-4.27589205183812,-2.87655855846778,
0.270412649013179));
#44088=CARTESIAN_POINT('Ctrl Pts',(-3.17793668728658,-3.7951739429827,0.316779200848224));
#44089=CARTESIAN_POINT('Ctrl Pts',(-1.92771999305178,-4.8411802984146,0.369575734322928));
#44090=CARTESIAN_POINT('Ctrl Pts',(-0.104675240574504,-5.21107779972881,
0.422372267797632));
#44091=CARTESIAN_POINT('Ctrl Pts',(1.45583984202071,-4.73188592100135,0.475168801272336));
#44092=CARTESIAN_POINT('Ctrl Pts',(3.01635492461593,-4.25269404227389,0.527965334747039));
#44093=CARTESIAN_POINT('Ctrl Pts',(4.31434033732908,-2.92441278350478,0.580761868221743));
#44094=CARTESIAN_POINT('Ctrl Pts',(4.76068268187915,-1.35442587380419,0.633558401696447));
#44095=CARTESIAN_POINT('Ctrl Pts',(5.20702502642923,0.215561035896397,0.686354935171151));
#44096=CARTESIAN_POINT('Ctrl Pts',(4.80172430281623,2.02725359652845,0.739151468645856));
#44097=CARTESIAN_POINT('Ctrl Pts',(3.72825744985575,3.25624139915875,0.791948002120559));
#44098=CARTESIAN_POINT('Ctrl Pts',(2.65479059689527,4.48522920178905,0.844744535595263));
#44099=CARTESIAN_POINT('Ctrl Pts',(0.9131576145873,5.13151224641759,0.897541069069967));
#44100=CARTESIAN_POINT('Ctrl Pts',(-0.702426516917608,4.90003317713487,
0.950337602544671));
#44101=CARTESIAN_POINT('Ctrl Pts',(-2.31801064842252,4.66855410785214,1.00313413601937));
#44102=CARTESIAN_POINT('Ctrl Pts',(-3.80754592912437,3.55931292465815,1.05593066949408));
#44103=CARTESIAN_POINT('Ctrl Pts',(-4.49264215512641,2.07804350324001,1.10872720296878));
#44104=CARTESIAN_POINT('Ctrl Pts',(-4.79088768013657,1.43319689701884,1.13171131709355));
#44105=CARTESIAN_POINT('Ctrl Pts',(-4.93667954029292,0.71784517544428,1.15469543121832));
#44106=CARTESIAN_POINT('Ctrl Pts',(-4.93449003509191,0.0016461999684793,
1.17767954534309));
#44107=CARTESIAN_POINT('Origin',(0.,0.,0.));
#44108=CARTESIAN_POINT('',(-4.9411817412373,-0.00444225127051057,2.32232045465689));
#44109=CARTESIAN_POINT('',(-4.94111085608669,-0.00445469630641156,2.17767954534309));
#44110=CARTESIAN_POINT('',(-4.942,-6.05220448138622E-16,0.));
#44111=CARTESIAN_POINT('Ctrl Pts',(-4.9411817412373,-0.00444225127051057,
2.32232045465689));
#44112=CARTESIAN_POINT('Ctrl Pts',(-4.93017412883888,1.22499555075574,2.28273213905534));
#44113=CARTESIAN_POINT('Ctrl Pts',(-4.46534239547945,2.46186324317617,2.24314382345379));
#44114=CARTESIAN_POINT('Ctrl Pts',(-3.63458175569093,3.36040592443024,2.20355550785224));
#44115=CARTESIAN_POINT('Ctrl Pts',(-2.52734116663296,4.55798664748753,2.15079206699202));
#44116=CARTESIAN_POINT('Ctrl Pts',(-0.770077330248272,5.15457871251208,
2.0980286261318));
#44117=CARTESIAN_POINT('Ctrl Pts',(0.837419729043101,4.87865187630481,2.04526518527159));
#44118=CARTESIAN_POINT('Ctrl Pts',(2.44491678833447,4.60272504009754,1.99250174441137));
#44119=CARTESIAN_POINT('Ctrl Pts',(3.90264707053253,3.45427930265847,1.93973830355116));
#44120=CARTESIAN_POINT('Ctrl Pts',(4.54714538443732,1.95601310903264,1.88697486269094));
#44121=CARTESIAN_POINT('Ctrl Pts',(5.19164369834212,0.45774691540682,1.83421142183073));
#44122=CARTESIAN_POINT('Ctrl Pts',(5.02291004395365,-1.39033973440576,1.78144798097051));
#44123=CARTESIAN_POINT('Ctrl Pts',(4.11774488359116,-2.74712173291455,1.7286845401103));
#44124=CARTESIAN_POINT('Ctrl Pts',(3.21257972322867,-4.10390373142335,1.67592109925008));
#44125=CARTESIAN_POINT('Ctrl Pts',(1.57098305689217,-4.96938107862837,1.62315765838987));
#44126=CARTESIAN_POINT('Ctrl Pts',(-0.0599057143251611,-4.94964036759779,
1.57039421752965));
#44127=CARTESIAN_POINT('Ctrl Pts',(-1.69079448554249,-4.92989965656721,
1.51763077666944));
#44128=CARTESIAN_POINT('Ctrl Pts',(-3.31097536164064,-4.02494088730103,
1.46486733580922));
#44129=CARTESIAN_POINT('Ctrl Pts',(-4.18303383973357,-2.64665132708304,
1.41210389494901));
#44130=CARTESIAN_POINT('Ctrl Pts',(-4.67767185058986,-1.86487530680844,
1.3821760815183));
#44131=CARTESIAN_POINT('Ctrl Pts',(-4.9316207664016,-0.930817306961143,
1.3522482680876));
#44132=CARTESIAN_POINT('Ctrl Pts',(-4.93459216488855,0.00173983556611496,
1.32232045465689));
#44133=CARTESIAN_POINT('Ctrl Pts',(-4.93449003509191,0.0016461999684793,
1.17767954534309));
#44134=CARTESIAN_POINT('Ctrl Pts',(-4.9316500541004,-0.927326919420464,
1.20749196469302));
#44135=CARTESIAN_POINT('Ctrl Pts',(-4.67984069516382,-1.85772549042789,
1.23730438404296));
#44136=CARTESIAN_POINT('Ctrl Pts',(-4.18882172046978,-2.63753729589231,
1.26711680339289));
#44137=CARTESIAN_POINT('Ctrl Pts',(-3.31924788850886,-4.01855101396421,
1.3199133368676));
#44138=CARTESIAN_POINT('Ctrl Pts',(-1.69944305328478,-4.92728079046571,
1.3727098703423));
#44139=CARTESIAN_POINT('Ctrl Pts',(-0.0675730918879967,-4.94957507244757,
1.42550640381701));
#44140=CARTESIAN_POINT('Ctrl Pts',(1.56429686950879,-4.97186935442943,1.47830293729171));
#44141=CARTESIAN_POINT('Ctrl Pts',(3.20823195707828,-4.10772814189165,1.53109947076641));
#44142=CARTESIAN_POINT('Ctrl Pts',(4.11520771620268,-2.7509467593832,1.58389600424112));
#44143=CARTESIAN_POINT('Ctrl Pts',(5.02218347532707,-1.39416537687474,1.63669253771582));
#44144=CARTESIAN_POINT('Ctrl Pts',(5.19219990600637,0.455256175604397,1.68948907119053));
#44145=CARTESIAN_POINT('Ctrl Pts',(4.54776321553941,1.95463753781542,1.74228560466523));
#44146=CARTESIAN_POINT('Ctrl Pts',(3.90332652507246,3.45401890002643,1.79508213813993));
#44147=CARTESIAN_POINT('Ctrl Pts',(2.44443671345924,4.60336007196933,1.84787867161464));
#44148=CARTESIAN_POINT('Ctrl Pts',(0.835860696338233,4.878943390804,1.90067520508934));
#44149=CARTESIAN_POINT('Ctrl Pts',(-0.772715320782773,5.15452670963867,
1.95347173856405));
#44150=CARTESIAN_POINT('Ctrl Pts',(-2.53097754341157,4.55635217536511,2.00626827203875));
#44151=CARTESIAN_POINT('Ctrl Pts',(-3.63776731536415,3.3569886406566,2.05906480551345));
#44152=CARTESIAN_POINT('Ctrl Pts',(-4.4666195916167,2.45880976243686,2.09860305212333));
#44153=CARTESIAN_POINT('Ctrl Pts',(-4.93011266597958,1.22347167947137,2.13814129873321));
#44154=CARTESIAN_POINT('Ctrl Pts',(-4.94111085608669,-0.00445469630641156,
2.17767954534309));
#44155=CARTESIAN_POINT('Origin',(0.,0.,0.));
#44156=CARTESIAN_POINT('',(-4.94903399601206,0.00195803074323202,3.32232045465689));
#44157=CARTESIAN_POINT('',(-4.94919334226918,0.00181972978148383,3.17767954534309));
#44158=CARTESIAN_POINT('',(-4.942,-6.05220448138622E-16,0.));
#44159=CARTESIAN_POINT('Ctrl Pts',(-4.94903399601206,0.00195803074323202,
3.32232045465689));
#44160=CARTESIAN_POINT('Ctrl Pts',(-4.949593728633,0.112604296590692,3.31874289174351));
#44161=CARTESIAN_POINT('Ctrl Pts',(-4.94620248790589,0.223215646212416,
3.31516532883013));
#44162=CARTESIAN_POINT('Ctrl Pts',(-4.93875055399973,0.333552745210412,
3.31158776591675));
#44163=CARTESIAN_POINT('Ctrl Pts',(-4.82884621871006,1.96085186995656,3.25882432505653));
#44164=CARTESIAN_POINT('Ctrl Pts',(-3.83567522857514,3.52849703407851,3.20606088419632));
#44165=CARTESIAN_POINT('Ctrl Pts',(-2.41126381713223,4.32299910001284,3.15329744333611));
#44166=CARTESIAN_POINT('Ctrl Pts',(-0.986852405689299,5.11750116594718,
3.10053400247589));
#44167=CARTESIAN_POINT('Ctrl Pts',(0.868799427061646,5.13886013369387,3.04777056161567));
#44168=CARTESIAN_POINT('Ctrl Pts',(2.31112083361857,4.37735478907724,2.99500712075546));
#44169=CARTESIAN_POINT('Ctrl Pts',(3.75344224017549,3.61584944446061,2.94224367989524));
#44170=CARTESIAN_POINT('Ctrl Pts',(4.78243322053839,2.07147978748068,2.88948023903503));
#44171=CARTESIAN_POINT('Ctrl Pts',(4.92976460259391,0.447141508486386,2.83671679817481));
#44172=CARTESIAN_POINT('Ctrl Pts',(5.07709598464943,-1.17719677050791,2.7839533573146));
#44173=CARTESIAN_POINT('Ctrl Pts',(4.34276776839756,-2.88150367151656,2.73118991645438));
#44174=CARTESIAN_POINT('Ctrl Pts',(3.06099802257449,-3.89009065317052,2.67842647559417));
#44175=CARTESIAN_POINT('Ctrl Pts',(1.77922827675142,-4.89867763482448,2.62566303473395));
#44176=CARTESIAN_POINT('Ctrl Pts',(-0.0499829986428499,-5.21154469712375,
2.57289959387374));
#44177=CARTESIAN_POINT('Ctrl Pts',(-1.59409909536903,-4.68629519517074,
2.52013615301352));
#44178=CARTESIAN_POINT('Ctrl Pts',(-3.13821519209522,-4.16104569321773,
2.46737271215331));
#44179=CARTESIAN_POINT('Ctrl Pts',(-4.39723611015331,-2.79767962701243,
2.41460927129309));
#44180=CARTESIAN_POINT('Ctrl Pts',(-4.79813789831673,-1.21671190336476,
2.36184583043288));
#44181=CARTESIAN_POINT('Ctrl Pts',(-4.89824378961878,-0.821941443944892,
2.34867070517422));
#44182=CARTESIAN_POINT('Ctrl Pts',(-4.94484511185421,-0.413603307842339,
2.33549557991555));
#44183=CARTESIAN_POINT('Ctrl Pts',(-4.9411817412373,-0.00444225127051057,
2.32232045465689));
#44184=CARTESIAN_POINT('Ctrl Pts',(-4.94111085608669,-0.00445469630641156,
2.17767954534309));
#44185=CARTESIAN_POINT('Ctrl Pts',(-4.94479885876604,-0.416212969241057,
2.19093783220791));
#44186=CARTESIAN_POINT('Ctrl Pts',(-4.89760609031032,-0.8271378330251,2.20419611907274));
#44187=CARTESIAN_POINT('Ctrl Pts',(-4.79624701605789,-1.22423691020985,
2.21745440593756));
#44188=CARTESIAN_POINT('Ctrl Pts',(-4.39261962352267,-2.80554639122433,
2.27025093941227));
#44189=CARTESIAN_POINT('Ctrl Pts',(-3.13004751717586,-4.16761281810985,
2.32304747288697));
#44190=CARTESIAN_POINT('Ctrl Pts',(-1.58383298272376,-4.68979872834667,
2.37584400636168));
#44191=CARTESIAN_POINT('Ctrl Pts',(-0.0376184482716604,-5.21198463858349,
2.42864053983638));
#44192=CARTESIAN_POINT('Ctrl Pts',(1.79223851428572,-4.89429003217164,2.48143707331108));
#44193=CARTESIAN_POINT('Ctrl Pts',(3.07195081718679,-3.88147571791622,2.53423360678579));
#44194=CARTESIAN_POINT('Ctrl Pts',(4.35166312008787,-2.86866140366079,2.58703014026049));
#44195=CARTESIAN_POINT('Ctrl Pts',(5.08123076333263,-1.1607273815618,2.6398266737352));
#44196=CARTESIAN_POINT('Ctrl Pts',(4.92822027622649,0.464093861851888,2.6926232072099));
#44197=CARTESIAN_POINT('Ctrl Pts',(4.77520978912036,2.08891510526557,2.7454197406846));
#44198=CARTESIAN_POINT('Ctrl Pts',(3.73962117166333,3.63062356999396,2.79821627415931));
#44199=CARTESIAN_POINT('Ctrl Pts',(2.29332840687238,4.38672799125455,2.85101280763401));
#44200=CARTESIAN_POINT('Ctrl Pts',(0.847035642081437,5.14283241251514,2.90380934110872));
#44201=CARTESIAN_POINT('Ctrl Pts',(-1.00996127004341,5.11333279030795,2.95660587458342));
#44202=CARTESIAN_POINT('Ctrl Pts',(-2.4315078970232,4.31167097450304,3.00940240805812));
#44203=CARTESIAN_POINT('Ctrl Pts',(-3.853054524003,3.51000915869812,3.06219894153283));
#44204=CARTESIAN_POINT('Ctrl Pts',(-4.83915086583772,1.93618514929547,3.11499547500753));
#44205=CARTESIAN_POINT('Ctrl Pts',(-4.94047465700387,0.307323593631802,
3.16779200848224));
#44206=CARTESIAN_POINT('Ctrl Pts',(-4.94679983692322,0.205641231723391,
3.17108785410252));
#44207=CARTESIAN_POINT('Ctrl Pts',(-4.94967711776464,0.103744392201655,
3.17438369972281));
#44208=CARTESIAN_POINT('Ctrl Pts',(-4.94919334226918,0.00181972978148383,
3.17767954534309));
#44209=CARTESIAN_POINT('Origin',(0.,0.,0.));
#44210=CARTESIAN_POINT('',(-4.93570031758673,0.00282778719561921,4.32232045465689));
#44211=CARTESIAN_POINT('',(-4.93596067211196,0.00302686994969232,4.17767954534309));
#44212=CARTESIAN_POINT('',(-4.942,-6.05220448138622E-16,0.));
#44213=CARTESIAN_POINT('Ctrl Pts',(-4.93570031758673,0.00282778719561921,
4.32232045465689));
#44214=CARTESIAN_POINT('Ctrl Pts',(-4.93901975399819,0.635970529567334,
4.30199020357146));
#44215=CARTESIAN_POINT('Ctrl Pts',(-4.82594024125747,1.26797266957629,4.28165995248604));
#44216=CARTESIAN_POINT('Ctrl Pts',(-4.59096240198504,1.85083188703807,4.26132970140062));
#44217=CARTESIAN_POINT('Ctrl Pts',(-3.98112048346584,3.36353616802088,4.2085662605404));
#44218=CARTESIAN_POINT('Ctrl Pts',(-2.55021179152983,4.54522999135323,4.15580281968019));
#44219=CARTESIAN_POINT('Ctrl Pts',(-0.94949200772219,4.85808392031181,4.10303937881998));
#44220=CARTESIAN_POINT('Ctrl Pts',(0.651227776085471,5.17093784927039,4.05027593795976));
#44221=CARTESIAN_POINT('Ctrl Pts',(2.42175865176475,4.61495188385518,3.99751249709954));
#44222=CARTESIAN_POINT('Ctrl Pts',(3.55627122044722,3.44317432848828,3.94474905623933));
#44223=CARTESIAN_POINT('Ctrl Pts',(4.69078378912967,2.27139677312141,3.89198561537911));
#44224=CARTESIAN_POINT('Ctrl Pts',(5.18927805081532,0.483827627802874,3.8392221745189));
#44225=CARTESIAN_POINT('Ctrl Pts',(4.82487214846976,-1.10594900598695,3.78645873365868));
#44226=CARTESIAN_POINT('Ctrl Pts',(4.46046624612419,-2.6957256397768,3.73369529279847));
#44227=CARTESIAN_POINT('Ctrl Pts',(3.23316017974738,-4.08770976203793,3.68093185193825));
#44228=CARTESIAN_POINT('Ctrl Pts',(1.7015430859675,-4.6483616008314,3.62816841107804));
#44229=CARTESIAN_POINT('Ctrl Pts',(0.169925992187646,-5.20901343962485,
3.57540497021783));
#44230=CARTESIAN_POINT('Ctrl Pts',(-1.66600212899526,-4.93833299495065,
3.52264152935761));
#44231=CARTESIAN_POINT('Ctrl Pts',(-2.97064734936451,-3.95951622992839,
3.4698780884974));
#44232=CARTESIAN_POINT('Ctrl Pts',(-4.18683263839842,-3.04706698189228,
3.42069221055056));
#44233=CARTESIAN_POINT('Ctrl Pts',(-4.94133855052495,-1.51925455419597,
3.37150633260372));
#44234=CARTESIAN_POINT('Ctrl Pts',(-4.94903399601206,0.00195803074323202,
3.32232045465689));
#44235=CARTESIAN_POINT('Ctrl Pts',(-4.94919334226918,0.00181972978148383,
3.17767954534309));
#44236=CARTESIAN_POINT('Ctrl Pts',(-4.94192746196068,-1.52899860347891,
3.22718023319751));
#44237=CARTESIAN_POINT('Ctrl Pts',(-4.17649517400323,-3.06609305497157,
3.27668092105193));
#44238=CARTESIAN_POINT('Ctrl Pts',(-2.94711271903068,-3.97709242316291,
3.32618160890635));
#44239=CARTESIAN_POINT('Ctrl Pts',(-1.63587574939375,-4.94874778236929,
3.37897814238105));
#44240=CARTESIAN_POINT('Ctrl Pts',(0.203149430377691,-5.20815939885737,
3.43177467585576));
#44241=CARTESIAN_POINT('Ctrl Pts',(1.73199722462222,-4.63712444206039,3.48457120933046));
#44242=CARTESIAN_POINT('Ctrl Pts',(3.26084501886676,-4.06608948526341,3.53736774280516));
#44243=CARTESIAN_POINT('Ctrl Pts',(4.47951542758438,-2.66460795518137,3.59016427627987));
#44244=CARTESIAN_POINT('Ctrl Pts',(4.83271212906113,-1.07127541230128,3.64296080975457));
#44245=CARTESIAN_POINT('Ctrl Pts',(5.18590883053788,0.522057130578818,3.69575734322927));
#44246=CARTESIAN_POINT('Ctrl Pts',(4.67363182477377,2.30724068625696,3.74855387670398));
#44247=CARTESIAN_POINT('Ctrl Pts',(3.52930397676422,3.47084297428374,3.80135041017868));
#44248=CARTESIAN_POINT('Ctrl Pts',(2.38497612875467,4.63444526231052,3.85414694365339));
#44249=CARTESIAN_POINT('Ctrl Pts',(0.6085974384997,5.17646628268592,3.90694347712809));
#44250=CARTESIAN_POINT('Ctrl Pts',(-0.990411824257063,4.84993009504558,
3.95974001060279));
#44251=CARTESIAN_POINT('Ctrl Pts',(-2.58942108701383,4.52339390740524,4.0125365440775));
#44252=CARTESIAN_POINT('Ctrl Pts',(-4.01106092227238,3.32830051174915,4.0653330775522));
#44253=CARTESIAN_POINT('Ctrl Pts',(-4.60755047572122,1.80920317532792,4.11812961102691));
#44254=CARTESIAN_POINT('Ctrl Pts',(-4.831813392182,1.23806626759189,4.1379795891323));
#44255=CARTESIAN_POINT('Ctrl Pts',(-4.93943770829377,0.621129986103563,
4.1578295672377));
#44256=CARTESIAN_POINT('Ctrl Pts',(-4.93596067211196,0.00302686994969232,
4.17767954534309));
#44257=CARTESIAN_POINT('Origin',(0.,0.,0.));
#44258=CARTESIAN_POINT('',(-4.93897027655035,-0.00418490057281118,5.32232045465689));
#44259=CARTESIAN_POINT('',(-4.93838471541483,-0.00406162586984615,5.17767954534309));
#44260=CARTESIAN_POINT('',(-4.942,-6.05220448138622E-16,0.));
#44261=CARTESIAN_POINT('Ctrl Pts',(-4.93897027655035,-0.00418490057281118,
5.32232045465689));
#44262=CARTESIAN_POINT('Ctrl Pts',(-4.92960049919577,1.1487585810669,5.28523751539942));
#44263=CARTESIAN_POINT('Ctrl Pts',(-4.5267508630109,2.30760372029857,5.24815457614196));
#44264=CARTESIAN_POINT('Ctrl Pts',(-3.78916668346253,3.18507932319436,5.21107163688449));
#44265=CARTESIAN_POINT('Ctrl Pts',(-2.73969541672107,4.43359502898083,5.15830819602428));
#44266=CARTESIAN_POINT('Ctrl Pts',(-1.01255385125843,5.11247792715855,5.10554475516406));
#44267=CARTESIAN_POINT('Ctrl Pts',(0.606176578608286,4.91274509878472,5.05278131430385));
#44268=CARTESIAN_POINT('Ctrl Pts',(2.224907008475,4.71301227041089,5.00001787344363));
#44269=CARTESIAN_POINT('Ctrl Pts',(3.73522630274578,3.63466371548551,4.94725443258342));
#44270=CARTESIAN_POINT('Ctrl Pts',(4.44973628814144,2.16849289048282,4.8944909917232));
#44271=CARTESIAN_POINT('Ctrl Pts',(5.1642462735371,0.702322065480126,4.84172755086299));
#44272=CARTESIAN_POINT('Ctrl Pts',(5.08294695005765,-1.15167102959988,4.78896411000277));
#44273=CARTESIAN_POINT('Ctrl Pts',(4.24284043151724,-2.54967047338244,4.73620066914256));
#44274=CARTESIAN_POINT('Ctrl Pts',(3.40273391297681,-3.94766991716502,4.68343722828234));
#44275=CARTESIAN_POINT('Ctrl Pts',(1.80382019937538,-4.88967570965013,4.63067378742212));
#44276=CARTESIAN_POINT('Ctrl Pts',(0.173819826494171,-4.94694866740537,
4.57791034656191));
#44277=CARTESIAN_POINT('Ctrl Pts',(-1.45618054638702,-5.0042216251606,4.5251469057017));
#44278=CARTESIAN_POINT('Ctrl Pts',(-3.11726757854798,-4.17676174818597,
4.47238346484148));
#44279=CARTESIAN_POINT('Ctrl Pts',(-4.05342352207729,-2.84117444038203,
4.41962002398127));
#44280=CARTESIAN_POINT('Ctrl Pts',(-4.62886975682389,-2.02020151085742,
4.38718683420648));
#44281=CARTESIAN_POINT('Ctrl Pts',(-4.93040476513016,-1.00723542508793,
4.35475364443168));
#44282=CARTESIAN_POINT('Ctrl Pts',(-4.93570031758673,0.00282778719561921,
4.32232045465689));
#44283=CARTESIAN_POINT('Ctrl Pts',(-4.93596067211196,0.00302686994969232,
4.17767954534309));
#44284=CARTESIAN_POINT('Ctrl Pts',(-4.9301895642308,-1.0228870344476,4.2106261007124));
#44285=CARTESIAN_POINT('Ctrl Pts',(-4.61834948018582,-2.05201540819261,
4.24357265608171));
#44286=CARTESIAN_POINT('Ctrl Pts',(-4.02575926717865,-2.88027773583012,
4.27651921145102));
#44287=CARTESIAN_POINT('Ctrl Pts',(-3.07613923354808,-4.20756003338059,
4.32931574492572));
#44288=CARTESIAN_POINT('Ctrl Pts',(-1.40555989464781,-5.01902335129515,
4.38211227840043));
#44289=CARTESIAN_POINT('Ctrl Pts',(0.224766745275694,-4.94491834338594,
4.43490881187513));
#44290=CARTESIAN_POINT('Ctrl Pts',(1.85509338519918,-4.87081333547673,4.48770534534984));
#44291=CARTESIAN_POINT('Ctrl Pts',(3.44516732614589,-3.91114000174376,4.54050187882454));
#44292=CARTESIAN_POINT('Ctrl Pts',(4.270459451601,-2.50318069379225,4.59329841229924));
#44293=CARTESIAN_POINT('Ctrl Pts',(5.09575157705613,-1.09522138584072,4.64609494577394));
#44294=CARTESIAN_POINT('Ctrl Pts',(5.15626188701963,0.761023896329388,4.69889147924865));
#44295=CARTESIAN_POINT('Ctrl Pts',(4.42441840505647,2.21974306847382,4.75168801272335));
#44296=CARTESIAN_POINT('Ctrl Pts',(3.69257492309331,3.67846224061823,4.80448454619806));
#44297=CARTESIAN_POINT('Ctrl Pts',(2.16837764920352,4.73965530273698,4.85728107967276));
#44298=CARTESIAN_POINT('Ctrl Pts',(0.54633850223222,4.91978167747611,4.91007761314747));
#44299=CARTESIAN_POINT('Ctrl Pts',(-1.0757006447391,5.09990805221523,4.96287414662217));
#44300=CARTESIAN_POINT('Ctrl Pts',(-2.79558166479192,4.39896773957469,5.01567068009687));
#44301=CARTESIAN_POINT('Ctrl Pts',(-3.82962787248045,3.13634944983863,5.06846721357158));
#44302=CARTESIAN_POINT('Ctrl Pts',(-4.54262037450559,2.26575259758193,5.10487132416208));
#44303=CARTESIAN_POINT('Ctrl Pts',(-4.92954384104421,1.12811506301544,5.14127543475258));
#44304=CARTESIAN_POINT('Ctrl Pts',(-4.93838471541483,-0.00406162586984614,
5.17767954534309));
#44305=CARTESIAN_POINT('Origin',(0.,0.,0.));
#44306=CARTESIAN_POINT('',(-4.94990673126105,0.000609106175146774,6.32232045465689));
#44307=CARTESIAN_POINT('',(-4.95002176789587,9.24615926348992E-5,6.1776795453431));
#44308=CARTESIAN_POINT('',(-4.942,-6.05220448138622E-16,0.));
#44309=CARTESIAN_POINT('Ctrl Pts',(-4.94990673126105,0.000609106175146774,
6.32232045465689));
#44310=CARTESIAN_POINT('Ctrl Pts',(-4.94996465668772,0.0337538979231002,
6.3212482680876));
#44311=CARTESIAN_POINT('Ctrl Pts',(-4.94966035453883,0.0668975980773335,
6.3201760815183));
#44312=CARTESIAN_POINT('Ctrl Pts',(-4.94899057048952,0.100033910748547,
6.31910389494901));
#44313=CARTESIAN_POINT('Ctrl Pts',(-4.91602978541085,1.73070708277234,6.26634045408879));
#44314=CARTESIAN_POINT('Ctrl Pts',(-3.99797098316147,3.34348977495136,6.21357701322858));
#44315=CARTESIAN_POINT('Ctrl Pts',(-2.61265424963019,4.20434920314469,6.16081357236836));
#44316=CARTESIAN_POINT('Ctrl Pts',(-1.22733751609891,5.06520863133802,6.10805013150815));
#44317=CARTESIAN_POINT('Ctrl Pts',(0.625237148714281,5.17414479554567,6.05528669064793));
#44318=CARTESIAN_POINT('Ctrl Pts',(2.10189939976769,4.48157710670587,6.00252324978771));
#44319=CARTESIAN_POINT('Ctrl Pts',(3.57856165082109,3.78900941786606,5.9497598089275));
#44320=CARTESIAN_POINT('Ctrl Pts',(4.67931148811471,2.29493787597879,5.89699636806729));
#44321=CARTESIAN_POINT('Ctrl Pts',(4.90315986233076,0.679365744295384,5.84423292720707));
#44322=CARTESIAN_POINT('Ctrl Pts',(5.12700823654681,-0.936206387388013,
5.79146948634686));
#44323=CARTESIAN_POINT('Ctrl Pts',(4.4739551476853,-2.67327910886755,5.73870604548664));
#44324=CARTESIAN_POINT('Ctrl Pts',(3.24122748150885,-3.74125097570411,5.68594260462643));
#44325=CARTESIAN_POINT('Ctrl Pts',(2.00849981533238,-4.80922284254067,5.63317916376621));
#44326=CARTESIAN_POINT('Ctrl Pts',(0.196097571840956,-5.20809385473422,
5.580415722906));
#44327=CARTESIAN_POINT('Ctrl Pts',(-1.37109275233711,-4.7563241179068,5.52765228204578));
#44328=CARTESIAN_POINT('Ctrl Pts',(-2.93828307651517,-4.30455438107937,
5.47488884118557));
#44329=CARTESIAN_POINT('Ctrl Pts',(-4.26026148137987,-3.00214389523098,
5.42212540032535));
#44330=CARTESIAN_POINT('Ctrl Pts',(-4.73535019980207,-1.44186439560917,
5.36936195946513));
#44331=CARTESIAN_POINT('Ctrl Pts',(-4.87653942645625,-0.978172778920024,
5.35368145786239));
#44332=CARTESIAN_POINT('Ctrl Pts',(-4.94293228203772,-0.49170645290201,
5.33800095625964));
#44333=CARTESIAN_POINT('Ctrl Pts',(-4.93897027655035,-0.00418490057281118,
5.32232045465689));
#44334=CARTESIAN_POINT('Ctrl Pts',(-4.93838471541483,-0.00406162586984614,
5.17767954534309));
#44335=CARTESIAN_POINT('Ctrl Pts',(-4.94236567660296,-0.513869962422989,
5.19407196822729));
#44336=CARTESIAN_POINT('Ctrl Pts',(-4.86968605256145,-1.02257104983416,
5.21046439111149));
#44337=CARTESIAN_POINT('Ctrl Pts',(-4.71559692470099,-1.50528507494596,
5.22685681399569));
#44338=CARTESIAN_POINT('Ctrl Pts',(-4.21930837390877,-3.06000504316299,
5.27965334747039));
#44339=CARTESIAN_POINT('Ctrl Pts',(-2.8785198770001,-4.34514871276549,5.3324498809451));
#44340=CARTESIAN_POINT('Ctrl Pts',(-1.30417176812337,-4.7751307324871,5.3852464144198));
#44341=CARTESIAN_POINT('Ctrl Pts',(0.270176340753341,-5.2051127522087,5.4380429478945));
#44342=CARTESIAN_POINT('Ctrl Pts',(2.07808406159809,-4.77993312204945,5.49083948136921));
#44343=CARTESIAN_POINT('Ctrl Pts',(3.29576468259939,-3.69332812921623,5.54363601484391));
#44344=CARTESIAN_POINT('Ctrl Pts',(4.51344530360071,-2.606723136383,5.59643254831862));
#44345=CARTESIAN_POINT('Ctrl Pts',(5.14089882475856,-0.858692780875764,
5.64922908179332));
#44346=CARTESIAN_POINT('Ctrl Pts',(4.892221343433,0.754259796075777,5.70202561526803));
#44347=CARTESIAN_POINT('Ctrl Pts',(4.64354386210744,2.36721237302732,5.75482214874273));
#44348=CARTESIAN_POINT('Ctrl Pts',(3.51873537829851,3.84508717142316,5.80761868221743));
#44349=CARTESIAN_POINT('Ctrl Pts',(2.03032331340283,4.51447945572607,5.86041521569213));
#44350=CARTESIAN_POINT('Ctrl Pts',(0.54191124850715,5.18387174002898,5.91321174916684));
#44351=CARTESIAN_POINT('Ctrl Pts',(-1.31010439747531,5.04478151023892,5.96600828264154));
#44352=CARTESIAN_POINT('Ctrl Pts',(-2.68183880585053,4.16058627269715,6.01880481611625));
#44353=CARTESIAN_POINT('Ctrl Pts',(-4.05357321422575,3.27639103515538,6.07160134959095));
#44354=CARTESIAN_POINT('Ctrl Pts',(-4.94502638499377,1.6470907898619,6.12439788306566));
#44355=CARTESIAN_POINT('Ctrl Pts',(-4.95000099524402,0.0150884128829395,
6.17719441654037));
#44356=CARTESIAN_POINT('Ctrl Pts',(-4.95001623189281,0.0100897806679753,
6.17735612614128));
#44357=CARTESIAN_POINT('Ctrl Pts',(-4.950023152263,0.00509112310363388,
6.17751783574219));
#44358=CARTESIAN_POINT('Ctrl Pts',(-4.95002176789587,9.24615926348992E-5,
6.1776795453431));
#44359=CARTESIAN_POINT('Origin',(0.,0.,0.));
#44360=CARTESIAN_POINT('',(-4.93729272679059,0.00368592931905526,7.32232045465689));
#44361=CARTESIAN_POINT('',(-4.93812703863464,0.00398950918922817,7.17767954534309));
#44362=CARTESIAN_POINT('',(-4.942,-6.05220448138622E-16,0.));
#44363=CARTESIAN_POINT('Ctrl Pts',(-4.93729272679059,0.00368592931905526,
7.32232045465689));
#44364=CARTESIAN_POINT('Ctrl Pts',(-4.94116559210242,0.558353954818944,
7.30449557991555));
#44365=CARTESIAN_POINT('Ctrl Pts',(-4.85488370936681,1.1118525040865,7.28667070517422));
#44366=CARTESIAN_POINT('Ctrl Pts',(-4.67321739836765,1.63203970469098,7.26884583043288));
#44367=CARTESIAN_POINT('Ctrl Pts',(-4.13546665420853,3.17184668755196,7.21608238957266));
#44368=CARTESIAN_POINT('Ctrl Pts',(-2.76193831173125,4.41977291493536,7.16331894871245));
#44369=CARTESIAN_POINT('Ctrl Pts',(-1.17777228483381,4.80784430854112,7.11055550785224));
#44370=CARTESIAN_POINT('Ctrl Pts',(0.406393742063621,5.19591570214688,7.05779206699202));
#44371=CARTESIAN_POINT('Ctrl Pts',(2.2011974533812,4.72413226197502,7.0050286261318));
#44372=CARTESIAN_POINT('Ctrl Pts',(3.38976204879511,3.60721883209798,6.95226518527158));
#44373=CARTESIAN_POINT('Ctrl Pts',(4.57832664420902,2.49030540222094,6.89950174441137));
#44374=CARTESIAN_POINT('Ctrl Pts',(5.16065212371926,0.728261982638741,6.84673830355116));
#44375=CARTESIAN_POINT('Ctrl Pts',(4.8717021652758,-0.876944960040814,6.79397486269094));
#44376=CARTESIAN_POINT('Ctrl Pts',(4.58275220683234,-2.48215190272036,6.74121142183073));
#44377=CARTESIAN_POINT('Ctrl Pts',(3.4225268104352,-3.93052236849726,6.68844798097051));
#44378=CARTESIAN_POINT('Ctrl Pts',(1.91908439466629,-4.56285322317541,6.63568454011029));
#44379=CARTESIAN_POINT('Ctrl Pts',(0.415641978897348,-5.19518407785358,
6.58292109925008));
#44380=CARTESIAN_POINT('Ctrl Pts',(-1.43101745624338,-5.01147532143298,
6.53015765838987));
#44381=CARTESIAN_POINT('Ctrl Pts',(-2.78041578985976,-4.09533911728839,
6.47739421752966));
#44382=CARTESIAN_POINT('Ctrl Pts',(-4.10239349384425,-3.1978193816249,6.42570296323874));
#44383=CARTESIAN_POINT('Ctrl Pts',(-4.94711408486409,-1.59733653848074,
6.37401170894781));
#44384=CARTESIAN_POINT('Ctrl Pts',(-4.94990673126105,0.000609106175146774,
6.32232045465689));
#44385=CARTESIAN_POINT('Ctrl Pts',(-4.95002176789587,9.24615926348992E-5,
6.1776795453431));
#44386=CARTESIAN_POINT('Ctrl Pts',(-4.94957117052949,-1.62692081873173,
6.23031436921689));
#44387=CARTESIAN_POINT('Ctrl Pts',(-4.06928678123987,-3.25435222218023,
6.28294919309067));
#44388=CARTESIAN_POINT('Ctrl Pts',(-2.70715303041471,-4.14415974390912,
6.33558401696446));
#44389=CARTESIAN_POINT('Ctrl Pts',(-1.34083440560272,-5.03670101505779,
6.38838055043917));
#44390=CARTESIAN_POINT('Ctrl Pts',(0.510298893753757,-5.18707904869072,
6.44117708391388));
#44391=CARTESIAN_POINT('Ctrl Pts',(2.00276409681877,-4.52677296598962,6.49397361738859));
#44392=CARTESIAN_POINT('Ctrl Pts',(3.49522929988377,-3.86646688328851,6.54677015086329));
#44393=CARTESIAN_POINT('Ctrl Pts',(4.62902640665733,-2.39547668425338,6.59956668433799));
#44394=CARTESIAN_POINT('Ctrl Pts',(4.88753226227565,-0.784070085091338,
6.65236321781269));
#44395=CARTESIAN_POINT('Ctrl Pts',(5.14603811789397,0.827336514070738,6.7051597512874));
#44396=CARTESIAN_POINT('Ctrl Pts',(4.52925272235704,2.57915951335971,6.7579562847621));
#44397=CARTESIAN_POINT('Ctrl Pts',(3.31821896685987,3.67316762496513,6.81075281823681));
#44398=CARTESIAN_POINT('Ctrl Pts',(2.10718521136272,4.76717573657052,6.86354935171151));
#44399=CARTESIAN_POINT('Ctrl Pts',(0.301903095905328,5.20336896049236,6.91634588518622));
#44400=CARTESIAN_POINT('Ctrl Pts',(-1.27503704449112,4.78299258292295,6.96914241866092));
#44401=CARTESIAN_POINT('Ctrl Pts',(-2.85197718488759,4.36261620535354,7.02193895213562));
#44402=CARTESIAN_POINT('Ctrl Pts',(-4.20057535022311,3.0856702262929,7.07473548561032));
#44403=CARTESIAN_POINT('Ctrl Pts',(-4.70633267235205,1.53400465783913,7.12753201908503));
#44404=CARTESIAN_POINT('Ctrl Pts',(-4.86645984309908,1.04273383179117,7.14424786117105));
#44405=CARTESIAN_POINT('Ctrl Pts',(-4.94209974418837,0.523924819599999,
7.16096370325707));
#44406=CARTESIAN_POINT('Ctrl Pts',(-4.93812703863464,0.00398950918922817,
7.17767954534309));
#44407=CARTESIAN_POINT('Origin',(0.,0.,0.));
#44408=CARTESIAN_POINT('',(-4.9370364718937,-0.00357917755902493,8.32232045465689));
#44409=CARTESIAN_POINT('',(-4.93615302863258,-0.00314627141571121,8.17767954534309));
#44410=CARTESIAN_POINT('',(-4.942,-6.05220448138622E-16,0.));
#44411=CARTESIAN_POINT('Ctrl Pts',(-4.9370364718937,-0.00357917755902493,
8.32232045465689));
#44412=CARTESIAN_POINT('Ctrl Pts',(-4.92976643593387,1.07253365977557,8.28774289174351));
#44413=CARTESIAN_POINT('Ctrl Pts',(-4.58366254169201,2.15290343310709,8.25316532883013));
#44414=CARTESIAN_POINT('Ctrl Pts',(-3.93530233070663,3.00265049848112,8.21858776591675));
#44415=CARTESIAN_POINT('Ctrl Pts',(-2.94594065318929,4.29931733247173,8.16582432505654));
#44416=CARTESIAN_POINT('Ctrl Pts',(-1.25277317118212,5.05897768713911,8.11306088419632));
#44417=CARTESIAN_POINT('Ctrl Pts',(0.373581453010537,4.93588404929253,8.06029744333611));
#44418=CARTESIAN_POINT('Ctrl Pts',(1.99993607720318,4.81279041144596,8.00753400247589));
#44419=CARTESIAN_POINT('Ctrl Pts',(3.55947784358134,3.80694278108544,7.95477056161567));
#44420=CARTESIAN_POINT('Ctrl Pts',(4.34240574156256,2.37613695433122,7.90200712075546));
#44421=CARTESIAN_POINT('Ctrl Pts',(5.12533363954378,0.945331127576992,7.84924367989524));
#44422=CARTESIAN_POINT('Ctrl Pts',(5.13164766912806,-0.910432895570919,
7.79648023903503));
#44423=CARTESIAN_POINT('Ctrl Pts',(4.35847409863575,-2.34653318357428,7.74371679817482));
#44424=CARTESIAN_POINT('Ctrl Pts',(3.58530052814345,-3.78263347157761,7.6909533573146));
#44425=CARTESIAN_POINT('Ctrl Pts',(2.03263935757455,-4.7990700244364,7.63818991645438));
#44426=CARTESIAN_POINT('Ctrl Pts',(0.407160002087725,-4.93322766379111,
7.58542647559417));
#44427=CARTESIAN_POINT('Ctrl Pts',(-1.21831935339912,-5.06738530314582,
7.53266303473395));
#44428=CARTESIAN_POINT('Ctrl Pts',(-2.91661689380388,-4.31926402899647,
7.47989959387374));
#44429=CARTESIAN_POINT('Ctrl Pts',(-3.9147790910858,-3.02935952275251,7.42713615301352));
#44430=CARTESIAN_POINT('Ctrl Pts',(-4.57573590812677,-2.1752186035157,7.39219758689465));
#44431=CARTESIAN_POINT('Ctrl Pts',(-4.92970151716189,-1.08351977418085,
7.35725902077577));
#44432=CARTESIAN_POINT('Ctrl Pts',(-4.93729272679059,0.00368592931905526,
7.32232045465689));
#44433=CARTESIAN_POINT('Ctrl Pts',(-4.93812703863464,0.00398950918922817,
7.17767954534309));
#44434=CARTESIAN_POINT('Ctrl Pts',(-4.9295520615366,-1.11827674461206,7.21376023673177));
#44435=CARTESIAN_POINT('Ctrl Pts',(-4.55006154683992,-2.24579042752333,
7.24984092812046));
#44436=CARTESIAN_POINT('Ctrl Pts',(-3.84867674353058,-3.11294472114867,
7.28592161950915));
#44437=CARTESIAN_POINT('Ctrl Pts',(-2.82234701365785,-4.38184337383585,
7.33871815298385));
#44438=CARTESIAN_POINT('Ctrl Pts',(-1.10677107499002,-5.09325552136332,
7.39151468645855));
#44439=CARTESIAN_POINT('Ctrl Pts',(0.516336029677229,-4.92302088331724,
7.44431121993325));
#44440=CARTESIAN_POINT('Ctrl Pts',(2.13944313434447,-4.75278624527117,7.49710775340795));
#44441=CARTESIAN_POINT('Ctrl Pts',(3.67008140501115,-3.70090482165158,7.54990428688267));
#44442=CARTESIAN_POINT('Ctrl Pts',(4.41080403428737,-2.24667427194838,7.60270082035737));
#44443=CARTESIAN_POINT('Ctrl Pts',(5.15152666356361,-0.792443722245162,
7.65549735383208));
#44444=CARTESIAN_POINT('Ctrl Pts',(5.10233365144936,1.06413595354166,7.70829388730677));
#44445=CARTESIAN_POINT('Ctrl Pts',(4.28564016284837,2.47710030230944,7.76109042078147));
#44446=CARTESIAN_POINT('Ctrl Pts',(3.46894667424739,3.89006465107721,7.81388695425618));
#44447=CARTESIAN_POINT('Ctrl Pts',(1.88475270915971,4.85941367282593,7.86668348773089));
#44448=CARTESIAN_POINT('Ctrl Pts',(0.254908128790928,4.94345621594819,7.91948002120559));
#44449=CARTESIAN_POINT('Ctrl Pts',(-1.37493645157786,5.02749875907046,7.9722765546803));
#44450=CARTESIAN_POINT('Ctrl Pts',(-3.05043164722777,4.22623482356622,8.02507308815499));
#44451=CARTESIAN_POINT('Ctrl Pts',(-4.00812550651364,2.90476633090432,8.0778696216297));
#44452=CARTESIAN_POINT('Ctrl Pts',(-4.61162062728013,2.07203697816232,8.11113959620083));
#44453=CARTESIAN_POINT('Ctrl Pts',(-4.93008062183261,1.03273713844183,8.14440957077196));
#44454=CARTESIAN_POINT('Ctrl Pts',(-4.93615302863258,-0.00314627141571121,
8.17767954534309));
#44455=CARTESIAN_POINT('Origin',(0.,0.,0.));
#44456=CARTESIAN_POINT('',(-4.94983422880388,-0.000811751590238941,9.32232045465689));
#44457=CARTESIAN_POINT('',(-4.94934061074693,-0.00165165342605634,9.1776795453431));
#44458=CARTESIAN_POINT('',(-4.942,-6.05220448138622E-16,0.));
#44459=CARTESIAN_POINT('Ctrl Pts',(-4.94983422880388,-0.000811751590238941,
9.32232045465689));
#44460=CARTESIAN_POINT('Ctrl Pts',(-4.94619904315733,1.58603660082692,9.27099020357146));
#44461=CARTESIAN_POINT('Ctrl Pts',(-4.11486910012118,3.17616060693066,9.21965995248604));
#44462=CARTESIAN_POINT('Ctrl Pts',(-2.80821896129528,4.07632441244751,9.16832970140062));
#44463=CARTESIAN_POINT('Ctrl Pts',(-1.46508589907443,5.00162165359779,9.1155662605404));
#44464=CARTESIAN_POINT('Ctrl Pts',(0.38028069926283,5.19789211576897,9.06280281968019));
#44465=CARTESIAN_POINT('Ctrl Pts',(1.88799112724405,4.575806371946,9.01003937881998));
#44466=CARTESIAN_POINT('Ctrl Pts',(3.39570155522527,3.95372062812305,8.95727593795976));
#44467=CARTESIAN_POINT('Ctrl Pts',(4.56575581285046,2.51327867830594,8.90451249709954));
#44468=CARTESIAN_POINT('Ctrl Pts',(4.86562202928207,0.910075116822231,8.85174905623933));
#44469=CARTESIAN_POINT('Ctrl Pts',(5.16548824571368,-0.693128444661515,
8.79898561537912));
#44470=CARTESIAN_POINT('Ctrl Pts',(4.5951664209517,-2.45909361781186,8.7462221745189));
#44471=CARTESIAN_POINT('Ctrl Pts',(3.4142296015798,-3.58406901130408,8.69345873365869));
#44472=CARTESIAN_POINT('Ctrl Pts',(2.23329278220791,-4.70904440479628,8.64069529279847));
#44473=CARTESIAN_POINT('Ctrl Pts',(0.441740968226092,-5.19303001863033,
8.58793185193825));
#44474=CARTESIAN_POINT('Ctrl Pts',(-1.14502909018537,-4.81574738049279,
8.53516841107804));
#44475=CARTESIAN_POINT('Ctrl Pts',(-2.73179914859682,-4.43846474235526,
8.48240497021782));
#44476=CARTESIAN_POINT('Ctrl Pts',(-4.11378745143793,-3.19991385224615,
8.42964152935761));
#44477=CARTESIAN_POINT('Ctrl Pts',(-4.66200366634471,-1.66380175053471,
8.3768780884974));
#44478=CARTESIAN_POINT('Ctrl Pts',(-4.85095633907095,-1.1343528226608,8.35869221055056));
#44479=CARTESIAN_POINT('Ctrl Pts',(-4.94086010709221,-0.569554771785043,
8.34050633260373));
#44480=CARTESIAN_POINT('Ctrl Pts',(-4.9370364718937,-0.00357917755902493,
8.32232045465689));
#44481=CARTESIAN_POINT('Ctrl Pts',(-4.93615302863258,-0.00314627141571121,
8.17767954534309));
#44482=CARTESIAN_POINT('Ctrl Pts',(-4.93971699916741,-0.611119036064889,
8.19720610424667));
#44483=CARTESIAN_POINT('Ctrl Pts',(-4.83567403422615,-1.21791495642756,
8.21673266315024));
#44484=CARTESIAN_POINT('Ctrl Pts',(-4.61849424808279,-1.78108068136924,
8.23625922205381));
#44485=CARTESIAN_POINT('Ctrl Pts',(-4.03127660744421,-3.30378615116137,
8.28905575552852));
#44486=CARTESIAN_POINT('Ctrl Pts',(-2.61694880324517,-4.50752404092604,
8.34185228900322));
#44487=CARTESIAN_POINT('Ctrl Pts',(-1.01995990653351,-4.84380215349313,
8.39464882247793));
#44488=CARTESIAN_POINT('Ctrl Pts',(0.57702899017813,-5.18008026606022,8.44744535595263));
#44489=CARTESIAN_POINT('Ctrl Pts',(2.35667897940238,-4.64889860142975,8.50024188942734));
#44490=CARTESIAN_POINT('Ctrl Pts',(3.50807919667006,-3.4922940688051,8.55303842290204));
#44491=CARTESIAN_POINT('Ctrl Pts',(4.65947941393775,-2.33568953618045,8.60583495637674));
#44492=CARTESIAN_POINT('Ctrl Pts',(5.18262985924886,-0.553662135561577,
8.65863148985144));
#44493=CARTESIAN_POINT('Ctrl Pts',(4.83915310871477,1.04179398325038,8.71142802332615));
#44494=CARTESIAN_POINT('Ctrl Pts',(4.49567635818068,2.63725010206233,8.76422455680085));
#44495=CARTESIAN_POINT('Ctrl Pts',(3.28557241180142,4.04613493906739,8.81702109027556));
#44496=CARTESIAN_POINT('Ctrl Pts',(1.76023420818717,4.62647955204043,8.86981762375026));
#44497=CARTESIAN_POINT('Ctrl Pts',(0.234896004572933,5.20682416501346,8.92261415722497));
#44498=CARTESIAN_POINT('Ctrl Pts',(-1.60567645627628,4.95862855395447,8.97541069069966));
#44499=CARTESIAN_POINT('Ctrl Pts',(-2.9228125287938,3.99498491044041,9.02820722417436));
#44500=CARTESIAN_POINT('Ctrl Pts',(-4.16579429986394,3.0855940679239,9.07803133123061));
#44501=CARTESIAN_POINT('Ctrl Pts',(-4.9426191442377,1.53904642191653,9.12785543828685));
#44502=CARTESIAN_POINT('Ctrl Pts',(-4.94934061074693,-0.00165165342605634,
9.1776795453431));
#44503=CARTESIAN_POINT('Origin',(0.,0.,0.));
#44504=CARTESIAN_POINT('',(-4.93927523449924,0.00424456982664218,10.3223204546569));
#44505=CARTESIAN_POINT('',(-4.94081497674544,0.00444099958366976,10.1776795453431));
#44506=CARTESIAN_POINT('',(-4.942,-6.05220448138622E-16,0.));
#44507=CARTESIAN_POINT('Ctrl Pts',(-4.93927523449924,0.00424456982664218,
10.3223204546569));
#44508=CARTESIAN_POINT('Ctrl Pts',(-4.94321947186548,0.480467662900444,
10.3070009562597));
#44509=CARTESIAN_POINT('Ctrl Pts',(-4.8799048924926,0.955663934034991,10.2916814578624));
#44510=CARTESIAN_POINT('Ctrl Pts',(-4.7450520171049,1.40960838712838,10.2763619594652));
#44511=CARTESIAN_POINT('Ctrl Pts',(-4.28059152820107,2.97308459787111,10.2235985186049));
#44512=CARTESIAN_POINT('Ctrl Pts',(-2.96750623957443,4.28446059329433,10.1708350777447));
#44513=CARTESIAN_POINT('Ctrl Pts',(-1.40342635577711,4.74688412687777,10.1180716368845));
#44514=CARTESIAN_POINT('Ctrl Pts',(0.160653528020168,5.2093076604612,10.0653081960243));
#44515=CARTESIAN_POINT('Ctrl Pts',(1.9757280069881,4.82277873220489,10.0125447551641));
#44516=CARTESIAN_POINT('Ctrl Pts',(3.21569435837255,3.76321993027579,9.95978131430385));
#44517=CARTESIAN_POINT('Ctrl Pts',(4.455660709757,2.70366112834667,9.90701787344364));
#44518=CARTESIAN_POINT('Ctrl Pts',(5.12051893355795,0.971072452744719,9.85425443258342));
#44519=CARTESIAN_POINT('Ctrl Pts',(4.90766922172796,-0.64598549534651,9.8014909917232));
#44520=CARTESIAN_POINT('Ctrl Pts',(4.69481950989796,-2.26304344343773,9.74872755086298));
#44521=CARTESIAN_POINT('Ctrl Pts',(3.60426186243706,-3.76457066401824,9.69596411000277));
#44522=CARTESIAN_POINT('Ctrl Pts',(2.13234651308336,-4.4671705584447,9.64320066914255));
#44523=CARTESIAN_POINT('Ctrl Pts',(0.660431163729675,-5.16977045287116,
9.59043722828234));
#44524=CARTESIAN_POINT('Ctrl Pts',(-1.19284188751682,-5.07344302114356,
9.53767378742213));
#44525=CARTESIAN_POINT('Ctrl Pts',(-2.58398443596702,-4.22203018520405,
9.48491034656191));
#44526=CARTESIAN_POINT('Ctrl Pts',(-3.97512698441724,-3.37061734926452,
9.43214690570169));
#44527=CARTESIAN_POINT('Ctrl Pts',(-4.90413903007116,-1.76411910911306,
9.37938346484148));
#44528=CARTESIAN_POINT('Ctrl Pts',(-4.94819528984589,-0.133707978972622,
9.32662002398126));
#44529=CARTESIAN_POINT('Ctrl Pts',(-4.94939197035033,-0.089421849745139,
9.32518683420647));
#44530=CARTESIAN_POINT('Ctrl Pts',(-4.94993572666894,-0.0451180774845514,
9.32375364443168));
#44531=CARTESIAN_POINT('Ctrl Pts',(-4.94983422880388,-0.000811751590238941,
9.32232045465689));
#44532=CARTESIAN_POINT('Ctrl Pts',(-4.94934061074693,-0.00165165342605634,
9.1776795453431));
#44533=CARTESIAN_POINT('Ctrl Pts',(-4.94974160267239,-0.0935672327028531,
9.18065197176156));
#44534=CARTESIAN_POINT('Ctrl Pts',(-4.94740170081727,-0.185461992629528,
9.18362439818002));
#44535=CARTESIAN_POINT('Ctrl Pts',(-4.9422563677255,-0.277199402591944,
9.18659682459849));
#44536=CARTESIAN_POINT('Ctrl Pts',(-4.85086444995379,-1.90664839614095,
9.23939335807319));
#44537=CARTESIAN_POINT('Ctrl Pts',(-3.87438093022463,-3.48645470726985,
9.29218989154789));
#44538=CARTESIAN_POINT('Ctrl Pts',(-2.45774784765697,-4.29676774220554,
9.34498642502259));
#44539=CARTESIAN_POINT('Ctrl Pts',(-1.04111476508925,-5.10708077714125,
9.3977829584973));
#44540=CARTESIAN_POINT('Ctrl Pts',(0.815667880316977,-5.14790053588371,
9.450579491972));
#44541=CARTESIAN_POINT('Ctrl Pts',(2.2665431508298,-4.40062718922509,9.50337602544671));
#44542=CARTESIAN_POINT('Ctrl Pts',(3.71741842134259,-3.65335384256648,9.55617255892141));
#44543=CARTESIAN_POINT('Ctrl Pts',(4.76238631696197,-2.11798739050681,9.60896909239612));
#44544=CARTESIAN_POINT('Ctrl Pts',(4.92529937908085,-0.494129071747753,
9.66176562587082));
#44545=CARTESIAN_POINT('Ctrl Pts',(5.08821244119973,1.12972924701132,9.71456215934552));
#44546=CARTESIAN_POINT('Ctrl Pts',(4.36907066981809,2.8420794324698,9.76735869282023));
#44547=CARTESIAN_POINT('Ctrl Pts',(3.09555640642893,3.86267628047412,9.82015522629493));
#44548=CARTESIAN_POINT('Ctrl Pts',(1.82204214303977,4.88327312847843,9.87295175976963));
#44549=CARTESIAN_POINT('Ctrl Pts',(-0.00584461235687284,5.21211663902861,
9.92574829324434));
#44550=CARTESIAN_POINT('Ctrl Pts',(-1.55521355102309,4.69936680030775,9.97854482671904));
#44551=CARTESIAN_POINT('Ctrl Pts',(-3.10458248968932,4.18661696158688,10.0313413601937));
#44552=CARTESIAN_POINT('Ctrl Pts',(-4.37543361162511,2.83227377359494,10.0841378936684));
#44553=CARTESIAN_POINT('Ctrl Pts',(-4.78869407209101,1.25345386713711,10.1369344271432));
#44554=CARTESIAN_POINT('Ctrl Pts',(-4.89500374307923,0.847308491854974,
10.1505161332098));
#44555=CARTESIAN_POINT('Ctrl Pts',(-4.9445618440258,0.426308236753005,10.1640978392764));
#44556=CARTESIAN_POINT('Ctrl Pts',(-4.94081497674544,0.00444099958366976,
10.1776795453431));
#44557=CARTESIAN_POINT('Origin',(0.,0.,0.));
#44558=CARTESIAN_POINT('',(-4.93550942083981,-0.00268364051190351,11.3223204546569));
#44559=CARTESIAN_POINT('',(-4.93464332849729,-0.00183839903596135,11.1776795453431));
#44560=CARTESIAN_POINT('',(-4.942,-6.05220448138622E-16,0.));
#44561=CARTESIAN_POINT('Ctrl Pts',(-4.93550942083981,-0.00268364051190351,
11.3223204546569));
#44562=CARTESIAN_POINT('Ctrl Pts',(-4.93055147786098,0.996233778963576,
11.2902482680876));
#44563=CARTESIAN_POINT('Ctrl Pts',(-4.63616667462007,1.99783803363001,11.2581760815183));
#44564=CARTESIAN_POINT('Ctrl Pts',(-4.07266300921302,2.81352633957493,11.226103894949));
#44565=CARTESIAN_POINT('Ctrl Pts',(-3.14561700753245,4.15545298365024,11.1733404540888));
#44566=CARTESIAN_POINT('Ctrl Pts',(-1.49019904742592,4.99419689804637,11.1205770132286));
#44567=CARTESIAN_POINT('Ctrl Pts',(0.140153312490383,4.94801692591001,11.0678135723684));
#44568=CARTESIAN_POINT('Ctrl Pts',(1.77050567240668,4.90183695377364,11.0150501315081));
#44569=CARTESIAN_POINT('Ctrl Pts',(3.37579243213274,3.97073309510478,10.9622866906479));
#44570=CARTESIAN_POINT('Ctrl Pts',(4.22539246378791,2.57848268891964,10.9095232497877));
#44571=CARTESIAN_POINT('Ctrl Pts',(5.07499249544306,1.18623228273452,10.8567598089275));
#44572=CARTESIAN_POINT('Ctrl Pts',(5.16890579902736,-0.667164670966868,
10.8039963680673));
#44573=CARTESIAN_POINT('Ctrl Pts',(4.46438920521479,-2.13816357523356,10.7512329272071));
#44574=CARTESIAN_POINT('Ctrl Pts',(3.75987261140222,-3.60916247950026,10.6984694863469));
#44575=CARTESIAN_POINT('Ctrl Pts',(2.25692612019279,-4.69776333433226,10.6457060454866));
#44576=CARTESIAN_POINT('Ctrl Pts',(0.639592289029041,-4.90850650951066,
10.5929426046264));
#44577=CARTESIAN_POINT('Ctrl Pts',(-0.977741542134707,-5.11924968468906,
10.5401791637662));
#44578=CARTESIAN_POINT('Ctrl Pts',(-2.70946271325277,-4.45213518021386,
10.487415722906));
#44579=CARTESIAN_POINT('Ctrl Pts',(-3.76740545422127,-3.21078971494518,
10.4346522820458));
#44580=CARTESIAN_POINT('Ctrl Pts',(-4.51818187206105,-2.32986027932856,
10.3972083395828));
#44581=CARTESIAN_POINT('Ctrl Pts',(-4.92963472322582,-1.15974067526383,
10.3597643971199));
#44582=CARTESIAN_POINT('Ctrl Pts',(-4.93927523449924,0.00424456982664218,
10.3223204546569));
#44583=CARTESIAN_POINT('Ctrl Pts',(-4.94081497674544,0.00444099958366976,
10.1776795453431));
#44584=CARTESIAN_POINT('Ctrl Pts',(-4.92999654546744,-1.21362768880717,
10.2168943727512));
#44585=CARTESIAN_POINT('Ctrl Pts',(-4.47479284917987,-2.43892410978247,
10.2561092001592));
#44586=CARTESIAN_POINT('Ctrl Pts',(-3.65816585751927,-3.33475037626519,
10.2953240275673));
#44587=CARTESIAN_POINT('Ctrl Pts',(-2.5587073834856,-4.54083808828599,10.348120561042));
#44588=CARTESIAN_POINT('Ctrl Pts',(-0.804120636422241,-5.14971688740386,
10.4009170945167));
#44589=CARTESIAN_POINT('Ctrl Pts',(0.806103773459557,-4.88394658237934,
10.4537136279914));
#44590=CARTESIAN_POINT('Ctrl Pts',(2.41632818334133,-4.61817627735482,10.5065101614661));
#44591=CARTESIAN_POINT('Ctrl Pts',(3.88219025604155,-3.47775686818796,10.5593066949408));
#44592=CARTESIAN_POINT('Ctrl Pts',(4.53575894457716,-1.9823290114935,10.6121032284155));
#44593=CARTESIAN_POINT('Ctrl Pts',(5.18932763311279,-0.486901154799003,
10.6648997618902));
#44594=CARTESIAN_POINT('Ctrl Pts',(5.03060293748377,1.3635351494231,10.7176962953649));
#44595=CARTESIAN_POINT('Ctrl Pts',(4.13190895564446,2.72581472139719,10.7704928288396));
#44596=CARTESIAN_POINT('Ctrl Pts',(3.23321497380518,4.08809429337122,10.8232893623143));
#44597=CARTESIAN_POINT('Ctrl Pts',(1.5945517057557,4.96221713309726,10.876085895789));
#44598=CARTESIAN_POINT('Ctrl Pts',(-0.0374116408992591,4.94988261297637,
10.9288824292637));
#44599=CARTESIAN_POINT('Ctrl Pts',(-1.66937498755429,4.93754809285548,10.9816789627384));
#44600=CARTESIAN_POINT('Ctrl Pts',(-3.29463841281478,4.03875621288757,11.0344754962131));
#44601=CARTESIAN_POINT('Ctrl Pts',(-4.17263844793783,2.66304823386876,11.0872720296878));
#44602=CARTESIAN_POINT('Ctrl Pts',(-4.67379383761091,1.87780513509723,11.1174078682396));
#44603=CARTESIAN_POINT('Ctrl Pts',(-4.93148820012105,0.937181102537252,
11.1475437067913));
#44604=CARTESIAN_POINT('Ctrl Pts',(-4.93464332849729,-0.00183839903596135,
11.1776795453431));
#44605=CARTESIAN_POINT('Origin',(0.,0.,0.));
#44606=CARTESIAN_POINT('',(-4.9488440041135,-0.00213750530709822,12.3223204546569));
#44607=CARTESIAN_POINT('',(-4.94745353480859,-0.00311052193284108,12.1776795453431));
#44608=CARTESIAN_POINT('',(-4.942,-6.05220448138622E-16,0.));
#44609=CARTESIAN_POINT('Ctrl Pts',(-4.9488440041135,-0.00213750530709822,
12.3223204546569));
#44610=CARTESIAN_POINT('Ctrl Pts',(-4.94061448411462,1.50806390763245,12.2734955799156));
#44611=CARTESIAN_POINT('Ctrl Pts',(-4.19858957372796,3.0252638763299,12.2246707051742));
#44612=CARTESIAN_POINT('Ctrl Pts',(-2.99752188376984,3.93921020084163,12.1758458304329));
#44613=CARTESIAN_POINT('Ctrl Pts',(-1.69956742174719,4.92688201973019,12.1230823895727));
#44614=CARTESIAN_POINT('Ctrl Pts',(0.13447629685455,5.21004913441221,12.0703189487124));
#44615=CARTESIAN_POINT('Ctrl Pts',(1.669872996944,4.65983246739314,12.0175555078522));
#44616=CARTESIAN_POINT('Ctrl Pts',(3.20526969703341,4.10961580037408,11.964792066992));
#44617=CARTESIAN_POINT('Ctrl Pts',(4.44201937861055,2.72601535165399,11.9120286261318));
#44618=CARTESIAN_POINT('Ctrl Pts',(4.81723479316035,1.13875519654544,11.8592651852716));
#44619=CARTESIAN_POINT('Ctrl Pts',(5.19245020771016,-0.44850495856316,11.8065017444114));
#44620=CARTESIAN_POINT('Ctrl Pts',(4.70613135523258,-2.23942482006024,11.7537383035512));
#44621=CARTESIAN_POINT('Ctrl Pts',(3.57961864506819,-3.4188952610418,11.7009748626909));
#44622=CARTESIAN_POINT('Ctrl Pts',(2.45310593490382,-4.59836570202334,11.6482114218307));
#44623=CARTESIAN_POINT('Ctrl Pts',(0.686399367052665,-5.16638672248939,
11.5954479809705));
#44624=CARTESIAN_POINT('Ctrl Pts',(-0.916412232973623,-4.86443245089807,
11.5426845401103));
#44625=CARTESIAN_POINT('Ctrl Pts',(-2.51922383299994,-4.56247817930674,
11.4899210992501));
#44626=CARTESIAN_POINT('Ctrl Pts',(-3.95814046520138,-3.39054861565802,
11.4371576583899));
#44627=CARTESIAN_POINT('Ctrl Pts',(-4.57826175967478,-1.88202914695641,
11.3843942175297));
#44628=CARTESIAN_POINT('Ctrl Pts',(-4.82144315925703,-1.29046120861066,
11.3637029632387));
#44629=CARTESIAN_POINT('Ctrl Pts',(-4.93870801968536,-0.647131573531266,
11.3430117089478));
#44630=CARTESIAN_POINT('Ctrl Pts',(-4.93550942083981,-0.00268364051190351,
11.3223204546569));
#44631=CARTESIAN_POINT('Ctrl Pts',(-4.93464332849729,-0.00183839903596135,
11.1776795453431));
#44632=CARTESIAN_POINT('Ctrl Pts',(-4.93701583263233,-0.707935706243941,
11.200340240266));
#44633=CARTESIAN_POINT('Ctrl Pts',(-4.79546387301719,-1.41312576132387,
11.223000935189));
#44634=CARTESIAN_POINT('Ctrl Pts',(-4.50527725011862,-2.05066194500317,
11.2456616301119));
#44635=CARTESIAN_POINT('Ctrl Pts',(-3.82917937219074,-3.53604006678678,
11.2984581635866));
#44636=CARTESIAN_POINT('Ctrl Pts',(-2.34624697134931,-4.65417223228435,
11.3512546970613));
#44637=CARTESIAN_POINT('Ctrl Pts',(-0.732189317617651,-4.89557313460714,
11.404051230536));
#44638=CARTESIAN_POINT('Ctrl Pts',(0.881868336113988,-5.13697403692992,
11.4568477640108));
#44639=CARTESIAN_POINT('Ctrl Pts',(2.62705124273586,-4.50164367607793,11.5096442974855));
#44640=CARTESIAN_POINT('Ctrl Pts',(3.70815372246008,-3.27907509577412,11.5624408309602));
#44641=CARTESIAN_POINT('Ctrl Pts',(4.78925620218431,-2.05650651547028,11.6152373644349));
#44642=CARTESIAN_POINT('Ctrl Pts',(5.20627825501086,-0.246699715714593,
11.6680338979096));
#44643=CARTESIAN_POINT('Ctrl Pts',(4.76920065502008,1.32569326213742,11.7208304313843));
#44644=CARTESIAN_POINT('Ctrl Pts',(4.33212305502932,2.89808623998941,11.773626964859));
#44645=CARTESIAN_POINT('Ctrl Pts',(3.04094580222125,4.23306539593773,11.8264234983337));
#44646=CARTESIAN_POINT('Ctrl Pts',(1.48400349530759,4.72233746560275,11.8792200318084));
#44647=CARTESIAN_POINT('Ctrl Pts',(-0.0729388116060994,5.21160953526778,
11.9320165652831));
#44648=CARTESIAN_POINT('Ctrl Pts',(-1.89564617262539,4.85517451864949,11.9848130987578));
#44649=CARTESIAN_POINT('Ctrl Pts',(-3.15358830890438,3.81544470423333,12.0376096322325));
#44650=CARTESIAN_POINT('Ctrl Pts',(-4.26603410872305,2.89597231227191,12.0842996032694));
#44651=CARTESIAN_POINT('Ctrl Pts',(-4.93680336098554,1.44212692063929,12.1309895743062));
#44652=CARTESIAN_POINT('Ctrl Pts',(-4.94745353480859,-0.00311052193284108,
12.1776795453431));
#44653=CARTESIAN_POINT('Origin',(0.,0.,0.));
#44654=CARTESIAN_POINT('',(-4.94151427280004,0.00444821020356132,13.3223204546569));
#44655=CARTESIAN_POINT('',(-4.94372929093918,0.00429917225691094,13.1776795453431));
#44656=CARTESIAN_POINT('',(-4.942,-6.05220448138622E-16,0.));
#44657=CARTESIAN_POINT('Ctrl Pts',(-4.94151427280004,0.00444821020356132,
13.3223204546569));
#44658=CARTESIAN_POINT('Ctrl Pts',(-4.94510334294322,0.402329751972593,
13.3095063326037));
#44659=CARTESIAN_POINT('Ctrl Pts',(-4.90105411066494,0.799426659282486,
13.2966922105506));
#44660=CARTESIAN_POINT('Ctrl Pts',(-4.80630608075059,1.18403391346491,13.2838780884974));
#44661=CARTESIAN_POINT('Ctrl Pts',(-4.41617150483,2.76769310027955,13.2311146476372));
#44662=CARTESIAN_POINT('Ctrl Pts',(-3.16645719817481,4.13959474701713,13.178351206777));
#44663=CARTESIAN_POINT('Ctrl Pts',(-1.62595105536246,4.67533930486966,13.1255877659167));
#44664=CARTESIAN_POINT('Ctrl Pts',(-0.0854449125500667,5.21108386272221,
13.0728243250565));
#44665=CARTESIAN_POINT('Ctrl Pts',(1.74585306641946,4.91067133168968,13.0200608841963));
#44666=CARTESIAN_POINT('Ctrl Pts',(3.03445628684691,3.91082977043353,12.9672974433361));
#44667=CARTESIAN_POINT('Ctrl Pts',(4.3230595072743,2.91098820917742,12.9145340024759));
#44668=CARTESIAN_POINT('Ctrl Pts',(5.06896796915959,1.21171761769772,12.8617705616157));
#44669=CARTESIAN_POINT('Ctrl Pts',(4.9326931179398,-0.41358560700714,12.8090071207555));
#44670=CARTESIAN_POINT('Ctrl Pts',(4.79641826672,-2.03888883171205,12.7562436798952));
#44671=CARTESIAN_POINT('Ctrl Pts',(3.77796010239502,-3.59022468964221,12.703480239035));
#44672=CARTESIAN_POINT('Ctrl Pts',(2.34085390812233,-4.36152696093034,12.6507167981748));
#44673=CARTESIAN_POINT('Ctrl Pts',(0.903747713849633,-5.13282923221848,
12.5979533573146));
#44674=CARTESIAN_POINT('Ctrl Pts',(-0.952006510370724,-5.12409791686467,
12.5451899164544));
#44675=CARTESIAN_POINT('Ctrl Pts',(-2.38179129282902,-4.33930693630882,
12.4924264755942));
#44676=CARTESIAN_POINT('Ctrl Pts',(-3.81157607528729,-3.55451595575297,
12.4396630347339));
#44677=CARTESIAN_POINT('Ctrl Pts',(-4.81539141598345,-1.99366530999509,
12.3868995938737));
#44678=CARTESIAN_POINT('Ctrl Pts',(-4.93636648360977,-0.367151725568608,
12.3341361530135));
#44679=CARTESIAN_POINT('Ctrl Pts',(-4.94539675712518,-0.245739414485935,
12.3301975868946));
#44680=CARTESIAN_POINT('Ctrl Pts',(-4.94950785648002,-0.123961230389695,
12.3262590207758));
#44681=CARTESIAN_POINT('Ctrl Pts',(-4.9488440041135,-0.00213750530709822,
12.3223204546569));
#44682=CARTESIAN_POINT('Ctrl Pts',(-4.94745353480859,-0.00311052193284108,
12.1776795453431));
#44683=CARTESIAN_POINT('Ctrl Pts',(-4.94884646673765,-0.192132542820318,
12.1837861077809));
#44684=CARTESIAN_POINT('Ctrl Pts',(-4.93894745560412,-0.381007316833933,
12.1898926702188));
#44685=CARTESIAN_POINT('Ctrl Pts',(-4.91726778514412,-0.568520045648731,
12.1959992326566));
#44686=CARTESIAN_POINT('Ctrl Pts',(-4.72982821356618,-2.18973036890068,
12.2487957661313));
#44687=CARTESIAN_POINT('Ctrl Pts',(-3.6617721588716,-3.70912640319057,12.301592299606));
#44688=CARTESIAN_POINT('Ctrl Pts',(-2.19976737250484,-4.4343839504472,12.3543888330807));
#44689=CARTESIAN_POINT('Ctrl Pts',(-0.737762586138102,-5.15964149770382,
12.4071853665554));
#44690=CARTESIAN_POINT('Ctrl Pts',(1.1181909319008,-5.09076055792721,12.4599819000301));
#44691=CARTESIAN_POINT('Ctrl Pts',(2.52241404198307,-4.25912724791444,12.5127784335048));
#44692=CARTESIAN_POINT('Ctrl Pts',(3.92663715206537,-3.42749393790165,12.5655749669795));
#44693=CARTESIAN_POINT('Ctrl Pts',(4.87912985419102,-1.83310825765268,12.6183715004542));
#44694=CARTESIAN_POINT('Ctrl Pts',(4.94588170520655,-0.202463999821435,
12.6711680339289));
#44695=CARTESIAN_POINT('Ctrl Pts',(5.01263355622208,1.42818025800979,12.7239645674036));
#44696=CARTESIAN_POINT('Ctrl Pts',(4.1936445561275,3.09508309342328,12.7767611008784));
#44697=CARTESIAN_POINT('Ctrl Pts',(2.86209318500527,4.03870772815599,12.8295576343531));
#44698=CARTESIAN_POINT('Ctrl Pts',(1.53054181388302,4.98233236288871,12.8823541678278));
#44699=CARTESIAN_POINT('Ctrl Pts',(-0.313571928266912,5.20267879694063,
12.9351507013025));
#44700=CARTESIAN_POINT('Ctrl Pts',(-1.82996378449454,4.59934452509909,12.9879472347772));
#44701=CARTESIAN_POINT('Ctrl Pts',(-3.34635564072214,3.99601025325757,13.0407437682519));
#44702=CARTESIAN_POINT('Ctrl Pts',(-4.53502561102745,2.56899527552262,13.0935403017266));
#44703=CARTESIAN_POINT('Ctrl Pts',(-4.85434730874721,0.968529668713999,
13.1463368352013));
#44704=CARTESIAN_POINT('Ctrl Pts',(-4.917535847558,0.651823714081653,13.1567844052486));
#44705=CARTESIAN_POINT('Ctrl Pts',(-4.94668250438369,0.328325791222804,
13.1672319752958));
#44706=CARTESIAN_POINT('Ctrl Pts',(-4.94372929093918,0.00429917225691095,
13.1776795453431));
#44707=CARTESIAN_POINT('Origin',(0.,0.,0.));
#44708=CARTESIAN_POINT('',(-4.93448587773112,-0.00157506815688546,14.3223204546569));
#44709=CARTESIAN_POINT('',(-4.93400159721632,-0.000305393655117946,14.1776795453431));
#44710=CARTESIAN_POINT('',(-4.942,-6.05220448138622E-16,0.));
#44711=CARTESIAN_POINT('Ctrl Pts',(-4.93448587773112,-0.00157506815688546,
14.3223204546569));
#44712=CARTESIAN_POINT('Ctrl Pts',(-4.9318360603942,0.919788438910237,14.2927536444317));
#44713=CARTESIAN_POINT('Ctrl Pts',(-4.68434909382344,1.84247391790569,14.2631868342065));
#44714=CARTESIAN_POINT('Ctrl Pts',(-4.20094243104244,2.61812855704659,14.2336200239813));
#44715=CARTESIAN_POINT('Ctrl Pts',(-3.3382792398224,4.00232277240241,14.180856583121));
#44716=CARTESIAN_POINT('Ctrl Pts',(-1.72430206586684,4.91828000860559,14.1280931422608));
#44717=CARTESIAN_POINT('Ctrl Pts',(-0.0935873430086671,4.94911667465072,
14.0753297014006));
#44718=CARTESIAN_POINT('Ctrl Pts',(1.53712737984951,4.97995334069586,14.0225662605404));
#44719=CARTESIAN_POINT('Ctrl Pts',(3.18457965161027,4.12566943658293,13.9698028196802));
#44720=CARTESIAN_POINT('Ctrl Pts',(4.09895737196505,2.77507890210349,13.91703937882));
#44721=CARTESIAN_POINT('Ctrl Pts',(5.01333509231982,1.42448836762405,13.8642759379598));
#44722=CARTESIAN_POINT('Ctrl Pts',(5.19463826126858,-0.422408797221965,
13.8115124970995));
#44723=CARTESIAN_POINT('Ctrl Pts',(4.56034958089476,-1.92502627258323,13.7587490562393));
#44724=CARTESIAN_POINT('Ctrl Pts',(3.92606090052093,-3.42764374794451,13.7059856153791));
#44725=CARTESIAN_POINT('Ctrl Pts',(2.47618037082453,-4.58598153382108,13.6532221745189));
#44726=CARTESIAN_POINT('Ctrl Pts',(0.870598407947765,-4.87284032799863,
13.6004587336587));
#44727=CARTESIAN_POINT('Ctrl Pts',(-0.734983554928979,-5.15969912217617,
13.5476952927985));
#44728=CARTESIAN_POINT('Ctrl Pts',(-2.49626695098606,-4.57507892465472,
13.4949318519383));
#44729=CARTESIAN_POINT('Ctrl Pts',(-3.61163122642161,-3.38506046244813,
13.442168411078));
#44730=CARTESIAN_POINT('Ctrl Pts',(-4.45611828600162,-2.48404972171741,
13.402219092271));
#44731=CARTESIAN_POINT('Ctrl Pts',(-4.93032498439027,-1.23598765372993,
13.3622697734639));
#44732=CARTESIAN_POINT('Ctrl Pts',(-4.94151427280004,0.00444821020356132,
13.3223204546569));
#44733=CARTESIAN_POINT('Ctrl Pts',(-4.94372929093918,0.00429917225691095,
13.1776795453431));
#44734=CARTESIAN_POINT('Ctrl Pts',(-4.93175851423331,-1.30913460937943,
13.2200285087705));
#44735=CARTESIAN_POINT('Ctrl Pts',(-4.39236571089229,-2.63125521653574,
13.262377472198));
#44736=CARTESIAN_POINT('Ctrl Pts',(-3.45489131803353,-3.54492080217556,
13.3047264356254));
#44737=CARTESIAN_POINT('Ctrl Pts',(-2.28614020446586,-4.68398943037421,
13.3575229691001));
#44738=CARTESIAN_POINT('Ctrl Pts',(-0.498664552196314,-5.18821045088918,
13.4103195025748));
#44739=CARTESIAN_POINT('Ctrl Pts',(1.09305895224904,-4.82783177420557,13.4631160360495));
#44740=CARTESIAN_POINT('Ctrl Pts',(2.68478245669437,-4.46745309752197,13.5159125695242));
#44741=CARTESIAN_POINT('Ctrl Pts',(4.08075381331552,-3.2424747236398,13.5687091029989));
#44742=CARTESIAN_POINT('Ctrl Pts',(4.64488820407174,-1.71106723561516,13.6215056364736));
#44743=CARTESIAN_POINT('Ctrl Pts',(5.20902259482797,-0.179659747590474,
13.6743021699483));
#44744=CARTESIAN_POINT('Ctrl Pts',(4.94132001971923,1.6581768545767,13.727098703423));
#44745=CARTESIAN_POINT('Ctrl Pts',(3.9637611647886,2.96501853984655,13.7798952368977));
#44746=CARTESIAN_POINT('Ctrl Pts',(2.98620230985801,4.27186022511634,13.8326917703724));
#44747=CARTESIAN_POINT('Ctrl Pts',(1.29878717510559,5.04770699348884,13.8854883038471));
#44748=CARTESIAN_POINT('Ctrl Pts',(-0.32960087817538,4.93903844632007,13.9382848373218));
#44749=CARTESIAN_POINT('Ctrl Pts',(-1.95798893145639,4.8303698991513,13.9910813707965));
#44750=CARTESIAN_POINT('Ctrl Pts',(-3.52734990326595,3.8371860364412,14.0438779042712));
#44751=CARTESIAN_POINT('Ctrl Pts',(-4.32259269702876,2.41203853383676,14.0966744377459));
#44752=CARTESIAN_POINT('Ctrl Pts',(-4.72930328852039,1.68317611811527,14.1236761402783));
#44753=CARTESIAN_POINT('Ctrl Pts',(-4.93353545879958,0.841329253368597,
14.1506778428107));
#44754=CARTESIAN_POINT('Ctrl Pts',(-4.93400159721632,-0.000305393655117946,
14.1776795453431));
#44755=CARTESIAN_POINT('Origin',(0.,0.,0.));
#44756=CARTESIAN_POINT('',(-4.94718090754756,-0.00323194414963146,15.3223204546569));
#44757=CARTESIAN_POINT('',(-4.9448369857261,-0.0040807615555026,15.1776795453431));
#44758=CARTESIAN_POINT('',(-4.942,-6.05220448138622E-16,0.));
#44759=CARTESIAN_POINT('Ctrl Pts',(-4.94718090754756,-0.00323194414963146,
15.3223204546569));
#44760=CARTESIAN_POINT('Ctrl Pts',(-4.93629962156844,1.4307451373895,15.2760009562597));
#44761=CARTESIAN_POINT('Ctrl Pts',(-4.27737587184649,2.87344030248637,15.2296814578624));
#44762=CARTESIAN_POINT('Ctrl Pts',(-3.18014090814091,3.79331230684891,15.1833619594651));
#44763=CARTESIAN_POINT('Ctrl Pts',(-1.93025923583274,4.84115638505733,15.1305985186049));
#44764=CARTESIAN_POINT('Ctrl Pts',(-0.111627961864901,5.21058874364864,
15.0778350777447));
#44765=CARTESIAN_POINT('Ctrl Pts',(1.44803137056367,4.73346803090561,15.0250716368845));
#44766=CARTESIAN_POINT('Ctrl Pts',(3.00769070299228,4.25634731816257,14.9723081960243));
#44767=CARTESIAN_POINT('Ctrl Pts',(4.30837809388161,2.93267353408514,14.9195447551641));
#44768=CARTESIAN_POINT('Ctrl Pts',(4.75810604814116,1.36489607082845,14.8667813143038));
#44769=CARTESIAN_POINT('Ctrl Pts',(5.20783400240071,-0.202881392428214,
14.8140178734436));
#44770=CARTESIAN_POINT('Ctrl Pts',(4.80660252003052,-2.01476253486414,14.7612544325834));
#44771=CARTESIAN_POINT('Ctrl Pts',(3.73702582619445,-3.2460980306936,14.7084909917232));
#44772=CARTESIAN_POINT('Ctrl Pts',(2.66744913235836,-4.47743352652308,14.655727550863));
#44773=CARTESIAN_POINT('Ctrl Pts',(0.929527227056376,-5.12822337574609,
14.6029641100028));
#44774=CARTESIAN_POINT('Ctrl Pts',(-0.685751952425607,-4.90227077075043,
14.5502006691425));
#44775=CARTESIAN_POINT('Ctrl Pts',(-2.30103113190757,-4.67631816575478,
14.4974372282823));
#44776=CARTESIAN_POINT('Ctrl Pts',(-3.79366758556953,-3.57362310654048,
14.4446737874221));
#44777=CARTESIAN_POINT('Ctrl Pts',(-4.48431120815826,-2.09605997967911,
14.3919103465619));
#44778=CARTESIAN_POINT('Ctrl Pts',(-4.78794199402862,-1.44647220574097,
14.3687137159269));
#44779=CARTESIAN_POINT('Ctrl Pts',(-4.93656479099726,-0.724430485809702,
14.3455170852919));
#44780=CARTESIAN_POINT('Ctrl Pts',(-4.93448587773112,-0.00157506815688546,
14.3223204546569));
#44781=CARTESIAN_POINT('Ctrl Pts',(-4.93400159721632,-0.000305393655117946,
14.1776795453431));
#44782=CARTESIAN_POINT('Ctrl Pts',(-4.93444690105008,-0.804322229598714,
14.2034743762854));
#44783=CARTESIAN_POINT('Ctrl Pts',(-4.74893420650715,-1.60814539448429,
14.2292692072277));
#44784=CARTESIAN_POINT('Ctrl Pts',(-4.37634095459745,-2.31308827376533,
14.2550640381701));
#44785=CARTESIAN_POINT('Ctrl Pts',(-3.61372180268731,-3.75595643626419,
14.3078605716448));
#44786=CARTESIAN_POINT('Ctrl Pts',(-2.06735888315097,-4.78458161876317,
14.3606571051195));
#44787=CARTESIAN_POINT('Ctrl Pts',(-0.44186405756573,-4.93026304245127,
14.4134536385942));
#44788=CARTESIAN_POINT('Ctrl Pts',(1.18363076801951,-5.07594446613938,14.4662501720689));
#44789=CARTESIAN_POINT('Ctrl Pts',(2.88825749965368,-4.33868213101661,14.5190467055436));
#44790=CARTESIAN_POINT('Ctrl Pts',(3.89529018284092,-3.05441514934954,14.5718432390183));
#44791=CARTESIAN_POINT('Ctrl Pts',(4.90232286602818,-1.77014816768244,14.624639772493));
#44792=CARTESIAN_POINT('Ctrl Pts',(5.21176150076849,0.0611234605289337,
14.6774363059677));
#44793=CARTESIAN_POINT('Ctrl Pts',(4.682608052441,1.60496708387405,14.7302328394424));
#44794=CARTESIAN_POINT('Ctrl Pts',(4.15345460411353,3.1488107072191,14.7830293729171));
#44795=CARTESIAN_POINT('Ctrl Pts',(2.78570907271829,4.40522632569788,14.8358259063918));
#44796=CARTESIAN_POINT('Ctrl Pts',(1.20259496734194,4.80171873996239,14.8886224398665));
#44797=CARTESIAN_POINT('Ctrl Pts',(-0.380519138034476,5.19821115422692,
14.9414189733412));
#44798=CARTESIAN_POINT('Ctrl Pts',(-2.17900181739205,4.73478036427711,14.9942155068159));
#44799=CARTESIAN_POINT('Ctrl Pts',(-3.3733609497546,3.62259208519558,15.0470120402906));
#44800=CARTESIAN_POINT('Ctrl Pts',(-4.35867771010103,2.70506424759102,15.0905678753081));
#44801=CARTESIAN_POINT('Ctrl Pts',(-4.93283752130763,1.34600230443831,15.1341237103256));
#44802=CARTESIAN_POINT('Ctrl Pts',(-4.9448369857261,-0.0040807615555026,
15.1776795453431));
#44803=CARTESIAN_POINT('Origin',(0.,0.,0.));
#44804=CARTESIAN_POINT('',(-4.94384666289092,0.00426556420662083,16.3223204546569));
#44805=CARTESIAN_POINT('',(-4.94650740111161,0.00354971811832453,16.1776795453431));
#44806=CARTESIAN_POINT('',(-4.942,-6.05220448138622E-16,0.));
#44807=CARTESIAN_POINT('Ctrl Pts',(-4.94384666289092,0.00426556420662083,
16.3223204546569));
#44808=CARTESIAN_POINT('Ctrl Pts',(-4.94674943417405,0.323967179430384,
16.3120117089478));
#44809=CARTESIAN_POINT('Ctrl Pts',(-4.91837466800284,0.643155833620532,
16.3017029632387));
#44810=CARTESIAN_POINT('Ctrl Pts',(-4.85684297990262,0.955819257318147,
16.2913942175296));
#44811=CARTESIAN_POINT('Ctrl Pts',(-4.5419042203555,2.55613015167716,16.2386307766694));
#44812=CARTESIAN_POINT('Ctrl Pts',(-3.35834756654112,3.98549839996768,16.1858673358092));
#44813=CARTESIAN_POINT('Ctrl Pts',(-1.84485020909617,4.59336938114029,16.133103894949));
#44814=CARTESIAN_POINT('Ctrl Pts',(-0.331352851651252,5.20124036231289,
16.0803404540888));
#44815=CARTESIAN_POINT('Ctrl Pts',(1.51208520942422,4.98761407636759,16.0275770132286));
#44816=CARTESIAN_POINT('Ctrl Pts',(2.84645196705723,4.04971920709069,15.9748135723683));
#44817=CARTESIAN_POINT('Ctrl Pts',(4.18081872469025,3.11182433781378,15.9220501315081));
#44818=CARTESIAN_POINT('Ctrl Pts',(5.00611417888079,1.44966088520527,15.8692866906479));
#44819=CARTESIAN_POINT('Ctrl Pts',(4.94671805190497,-0.180263500133812,
15.8165232497877));
#44820=CARTESIAN_POINT('Ctrl Pts',(4.88732192492914,-1.81018788547292,15.7637598089275));
#44821=CARTESIAN_POINT('Ctrl Pts',(3.94323421678691,-3.40787320354259,15.7109963680673));
#44822=CARTESIAN_POINT('Ctrl Pts',(2.54414165016166,-4.24615799663446,15.6582329272071));
#44823=CARTESIAN_POINT('Ctrl Pts',(1.14504908353641,-5.08444278972633,15.6054694863468));
#44824=CARTESIAN_POINT('Ctrl Pts',(-0.709048341571857,-5.16332705784039,
15.5527060454866));
#44825=CARTESIAN_POINT('Ctrl Pts',(-2.17428721330366,-4.44690786540681,
15.4999426046264));
#44826=CARTESIAN_POINT('Ctrl Pts',(-3.63952608503543,-3.73048867297323,
15.4471791637662));
#44827=CARTESIAN_POINT('Ctrl Pts',(-4.71590640339076,-2.21876601999203,
15.394415722906));
#44828=CARTESIAN_POINT('Ctrl Pts',(-4.91353052724419,-0.59977679458864,
15.3416522820458));
#44829=CARTESIAN_POINT('Ctrl Pts',(-4.93766614961155,-0.402051376257967,
15.3352083395828));
#44830=CARTESIAN_POINT('Ctrl Pts',(-4.94869470590891,-0.202726026045579,
15.3287643971199));
#44831=CARTESIAN_POINT('Ctrl Pts',(-4.94718090754756,-0.00323194414963146,
15.3223204546569));
#44832=CARTESIAN_POINT('Ctrl Pts',(-4.9448369857261,-0.0040807615555026,
15.1776795453431));
#44833=CARTESIAN_POINT('Ctrl Pts',(-4.94738276248126,-0.290511052698514,
15.1869202438003));
#44834=CARTESIAN_POINT('Ctrl Pts',(-4.92462524198781,-0.576537197232804,
15.1961609422575));
#44835=CARTESIAN_POINT('Ctrl Pts',(-4.8751224347969,-0.857857073631679,
15.2054016407147));
#44836=CARTESIAN_POINT('Ctrl Pts',(-4.59228920210912,-2.46517218516427,
15.2581981741894));
#44837=CARTESIAN_POINT('Ctrl Pts',(-3.436387151366,-3.91885664001626,15.3109947076642));
#44838=CARTESIAN_POINT('Ctrl Pts',(-1.93411172090367,-4.55652821395913,
15.3637912411389));
#44839=CARTESIAN_POINT('Ctrl Pts',(-0.431836290441309,-5.19419978790203,
15.4165877746136));
#44840=CARTESIAN_POINT('Ctrl Pts',(1.41681251974025,-5.01585848093576,15.4693843080882));
#44841=CARTESIAN_POINT('Ctrl Pts',(2.76948401487652,-4.1027668473702,15.522180841563));
#44842=CARTESIAN_POINT('Ctrl Pts',(4.12215551001273,-3.18967521380468,15.5749773750377));
#44843=CARTESIAN_POINT('Ctrl Pts',(4.97884969010367,-1.54183325363995,15.6277739085124));
#44844=CARTESIAN_POINT('Ctrl Pts',(4.94920742712676,0.0899074861556964,
15.6805704419871));
#44845=CARTESIAN_POINT('Ctrl Pts',(4.91956516414985,1.72164822595137,15.7333669754618));
#44846=CARTESIAN_POINT('Ctrl Pts',(4.00358645810502,3.33728774537801,15.7861635089365));
#44847=CARTESIAN_POINT('Ctrl Pts',(2.61864387578884,4.200647779537,15.8389600424112));
#44848=CARTESIAN_POINT('Ctrl Pts',(1.23370129347265,5.06400781369599,15.8917565758859));
#44849=CARTESIAN_POINT('Ctrl Pts',(-0.620205165114908,5.17508836258739,
15.9445531093606));
#44850=CARTESIAN_POINT('Ctrl Pts',(-2.09832911795802,4.48327474299608,15.9973496428353));
#44851=CARTESIAN_POINT('Ctrl Pts',(-3.57645307080114,3.79146112340477,16.05014617631));
#44852=CARTESIAN_POINT('Ctrl Pts',(-4.67879451789979,2.29675333533074,16.1029427097847));
#44853=CARTESIAN_POINT('Ctrl Pts',(-4.90306331235317,0.680226188554136,
16.1557392432594));
#44854=CARTESIAN_POINT('Ctrl Pts',(-4.93412927302912,0.456303065875542,
16.1630526772873));
#44855=CARTESIAN_POINT('Ctrl Pts',(-4.94834669148062,0.23004246166547,16.1703661113152));
#44856=CARTESIAN_POINT('Ctrl Pts',(-4.94650740111161,0.00354971811832453,
16.1776795453431));
#44857=CARTESIAN_POINT('Origin',(0.,0.,0.));
#44858=CARTESIAN_POINT('',(-4.93403031428168,-0.000341981052076612,17.3223204546569));
#44859=CARTESIAN_POINT('',(-4.93428824426153,0.00126466874552048,17.1776795453431));
#44860=CARTESIAN_POINT('',(-4.942,-6.05220448138622E-16,0.));
#44861=CARTESIAN_POINT('Ctrl Pts',(-4.93403031428168,-0.000341981052076612,
17.3223204546569));
#44862=CARTESIAN_POINT('Ctrl Pts',(-4.93350394108414,0.843143514252388,
17.2952590207758));
#44863=CARTESIAN_POINT('Ctrl Pts',(-4.72829119907115,1.68686850434222,17.2681975868947));
#44864=CARTESIAN_POINT('Ctrl Pts',(-4.31985335744029,2.41689215977968,17.2411361530135));
#44865=CARTESIAN_POINT('Ctrl Pts',(-3.52349548532491,3.84026684640702,17.1883727121533));
#44866=CARTESIAN_POINT('Ctrl Pts',(-1.9545602926493,4.83139633972401,17.1356092712931));
#44867=CARTESIAN_POINT('Ctrl Pts',(-0.327119944589159,4.9391812045894,17.0828458304329));
#44868=CARTESIAN_POINT('Ctrl Pts',(1.30032040347096,5.04696606945479,17.0300823895727));
#44869=CARTESIAN_POINT('Ctrl Pts',(2.98626590691563,4.2714063058686,16.9773189487124));
#44870=CARTESIAN_POINT('Ctrl Pts',(3.96338272054503,2.96548703306019,16.9245555078522));
#44871=CARTESIAN_POINT('Ctrl Pts',(4.94049953417446,1.65956776025175,16.871792066992));
#44872=CARTESIAN_POINT('Ctrl Pts',(5.20878765798859,-0.176711021778891,
16.8190286261318));
#44873=CARTESIAN_POINT('Ctrl Pts',(4.64614108062899,-1.70759643201752,16.7662651852716));
#44874=CARTESIAN_POINT('Ctrl Pts',(4.0834945032694,-3.2384818422561,16.7135017444114));
#44875=CARTESIAN_POINT('Ctrl Pts',(2.68991322473609,-4.46397388070265,16.6607383035511));
#44876=CARTESIAN_POINT('Ctrl Pts',(1.09966334943406,-4.82630869971703,16.6079748626909));
#44877=CARTESIAN_POINT('Ctrl Pts',(-0.490586525867957,-5.18864351873141,
16.5552114218307));
#44878=CARTESIAN_POINT('Ctrl Pts',(-2.27750499793871,-4.68782111831362,
16.5024479809705));
#44879=CARTESIAN_POINT('Ctrl Pts',(-3.44780380133416,-3.551783147891,16.4496845401103));
#44880=CARTESIAN_POINT('Ctrl Pts',(-4.38945351416312,-2.63770050035899,
16.4072298449592));
#44881=CARTESIAN_POINT('Ctrl Pts',(-4.93189212706316,-1.31236741876541,
16.364775149808));
#44882=CARTESIAN_POINT('Ctrl Pts',(-4.94384666289092,0.00426556420662083,
16.3223204546569));
#44883=CARTESIAN_POINT('Ctrl Pts',(-4.94650740111161,0.00354971811832453,
16.1776795453431));
#44884=CARTESIAN_POINT('Ctrl Pts',(-4.93506863972457,-1.40503507794796,
16.2231626447899));
#44885=CARTESIAN_POINT('Ctrl Pts',(-4.30259793428105,-2.82259842281934,
16.2686457442367));
#44886=CARTESIAN_POINT('Ctrl Pts',(-3.23956236772638,-3.74272269838241,
16.3141288436835));
#44887=CARTESIAN_POINT('Ctrl Pts',(-2.00559648683807,-4.81079793306321,
16.3669253771582));
#44888=CARTESIAN_POINT('Ctrl Pts',(-0.191468583253334,-5.20860189694556,
16.4197219106329));
#44889=CARTESIAN_POINT('Ctrl Pts',(1.37620035566145,-4.75487224416495,16.4725184441076));
#44890=CARTESIAN_POINT('Ctrl Pts',(2.94386929457619,-4.30114259138436,16.5253149775823));
#44891=CARTESIAN_POINT('Ctrl Pts',(4.265079268821,-2.99587932194087,16.578111511057));
#44892=CARTESIAN_POINT('Ctrl Pts',(4.73781104997921,-1.43383540748133,16.6309080445317));
#44893=CARTESIAN_POINT('Ctrl Pts',(5.21054283113743,0.128208506978224,16.6837045780064));
#44894=CARTESIAN_POINT('Ctrl Pts',(4.83479641920902,1.94703306645383,16.7365011114811));
#44895=CARTESIAN_POINT('Ctrl Pts',(3.78178347511922,3.19387716968194,16.7892976449558));
#44896=CARTESIAN_POINT('Ctrl Pts',(2.72877053102942,4.44072127291004,16.8420941784306));
#44897=CARTESIAN_POINT('Ctrl Pts',(0.998491054778278,5.11558491989063,16.8948907119053));
#44898=CARTESIAN_POINT('Ctrl Pts',(-0.620640115192454,4.91096152429156,
16.94768724538));
#44899=CARTESIAN_POINT('Ctrl Pts',(-2.23977128516316,4.70633812869249,17.0004837788547));
#44900=CARTESIAN_POINT('Ctrl Pts',(-3.74775414885348,3.62222769051368,17.0532803123294));
#44901=CARTESIAN_POINT('Ctrl Pts',(-4.45746504028889,2.1526130784761,17.1060768458041));
#44902=CARTESIAN_POINT('Ctrl Pts',(-4.77830186027552,1.48824892058866,17.1299444123171));
#44903=CARTESIAN_POINT('Ctrl Pts',(-4.93600022440261,0.745101393327629,
17.1538119788301));
#44904=CARTESIAN_POINT('Ctrl Pts',(-4.93428824426153,0.00126466874552048,
17.1776795453431));
#44905=CARTESIAN_POINT('Origin',(0.,0.,0.));
#44906=CARTESIAN_POINT('',(-4.94522242777803,-0.0039236424385497,18.3223204546569));
#44907=CARTESIAN_POINT('',(-4.94192999916445,-0.00446510791632448,18.1776795453431));
#44908=CARTESIAN_POINT('',(-4.942,-6.05220448138622E-16,0.));
#44909=CARTESIAN_POINT('Ctrl Pts',(-4.94522242777803,-0.0039236424385497,
18.3223204546569));
#44910=CARTESIAN_POINT('Ctrl Pts',(-4.93329330491003,1.35399213993734,18.2785063326037));
#44911=CARTESIAN_POINT('Ctrl Pts',(-4.3513066594067,2.72080403156538,18.2346922105506));
#44912=CARTESIAN_POINT('Ctrl Pts',(-3.35561026819536,3.63892235657103,18.1908780884974));
#44913=CARTESIAN_POINT('Ctrl Pts',(-2.15653642646331,4.74457230855067,18.1381146476372));
#44914=CARTESIAN_POINT('Ctrl Pts',(-0.35748677154393,5.19951173147208,18.085351206777));
#44915=CARTESIAN_POINT('Ctrl Pts',(1.22293027595834,4.79656649826054,18.0325877659168));
#44916=CARTESIAN_POINT('Ctrl Pts',(2.80334732346066,4.39362126504898,17.9798243250565));
#44917=CARTESIAN_POINT('Ctrl Pts',(4.16513176354582,3.13279137570437,17.9270608841963));
#44918=CARTESIAN_POINT('Ctrl Pts',(4.68838366687364,1.58798426669984,17.8742974433361));
#44919=CARTESIAN_POINT('Ctrl Pts',(5.21163557020145,0.0431771576953521,
17.8215340024759));
#44920=CARTESIAN_POINT('Ctrl Pts',(4.89635493677199,-1.78560717096906,17.7687705616157));
#44921=CARTESIAN_POINT('Ctrl Pts',(3.88609177304056,-3.06605780050668,17.7160071207555));
#44922=CARTESIAN_POINT('Ctrl Pts',(2.87582860930912,-4.34650843004432,17.6632436798953));
#44923=CARTESIAN_POINT('Ctrl Pts',(1.17058291527568,-5.07862536045516,17.610480239035));
#44924=CARTESIAN_POINT('Ctrl Pts',(-0.453558190725748,-4.92918049163674,
17.5577167981748));
#44925=CARTESIAN_POINT('Ctrl Pts',(-2.0776992967272,-4.77973562281832,17.5049533573146));
#44926=CARTESIAN_POINT('Ctrl Pts',(-3.62073581469659,-3.74872895477065,
17.4521899164544));
#44927=CARTESIAN_POINT('Ctrl Pts',(-4.38036379790372,-2.30541568077795,
17.3994264755942));
#44928=CARTESIAN_POINT('Ctrl Pts',(-4.75039204866972,-1.6023522103828,17.3737244686151));
#44929=CARTESIAN_POINT('Ctrl Pts',(-4.93453024520391,-0.801455114314277,
17.348022461636));
#44930=CARTESIAN_POINT('Ctrl Pts',(-4.93403031428168,-0.000341981052076612,
17.3223204546569));
#44931=CARTESIAN_POINT('Ctrl Pts',(-4.93428824426153,0.00126466874552048,
17.1776795453431));
#44932=CARTESIAN_POINT('Ctrl Pts',(-4.93221321843459,-0.900311452079429,
17.2066085123048));
#44933=CARTESIAN_POINT('Ctrl Pts',(-4.69594942149747,-1.80290006851385,
17.2355374792665));
#44934=CARTESIAN_POINT('Ctrl Pts',(-4.23213525097133,-2.56744414176908,
17.2644664462282));
#44935=CARTESIAN_POINT('Ctrl Pts',(-3.38565565103777,-3.96276796408032,
17.3172629797029));
#44936=CARTESIAN_POINT('Ctrl Pts',(-1.78125753199004,-4.89829682280636,
17.3700595131776));
#44937=CARTESIAN_POINT('Ctrl Pts',(-0.149997058388728,-4.94775064594635,
17.4228560466523));
#44938=CARTESIAN_POINT('Ctrl Pts',(1.48126341521252,-4.99720446908635,17.475652580127));
#44939=CARTESIAN_POINT('Ctrl Pts',(3.13938624336737,-4.16058325664038,17.5284491136017));
#44940=CARTESIAN_POINT('Ctrl Pts',(4.06883557073125,-2.81909846013186,17.5812456470764));
#44941=CARTESIAN_POINT('Ctrl Pts',(4.99828489809513,-1.47761366362332,17.6340421805511));
#44942=CARTESIAN_POINT('Ctrl Pts',(5.19906072466804,0.368734716947733,17.6868387140258));
#44943=CARTESIAN_POINT('Ctrl Pts',(4.57967756755998,1.87864175098721,17.7396352475005));
#44944=CARTESIAN_POINT('Ctrl Pts',(3.9602944104519,3.38854878502672,17.7924317809752));
#44945=CARTESIAN_POINT('Ctrl Pts',(2.52075226966277,4.56201447253459,17.8452283144499));
#44946=CARTESIAN_POINT('Ctrl Pts',(0.916990219673444,4.86434504442812,17.8980248479246));
#44947=CARTESIAN_POINT('Ctrl Pts',(-0.68677183031584,5.16667561632164,17.9508213813993));
#44948=CARTESIAN_POINT('Ctrl Pts',(-2.45475378950534,4.59787107260088,18.003617914874));
#44949=CARTESIAN_POINT('Ctrl Pts',(-3.58136314295608,3.4171025376229,18.0564144483487));
#44950=CARTESIAN_POINT('Ctrl Pts',(-4.44390962426003,2.51309109660283,18.0968361473469));
#44951=CARTESIAN_POINT('Ctrl Pts',(-4.93050729338922,1.25036908149785,18.137257846345));
#44952=CARTESIAN_POINT('Ctrl Pts',(-4.94192999916445,-0.00446510791632448,
18.1776795453431));
#44953=CARTESIAN_POINT('Origin',(0.,0.,-1.84858989190501));
#44954=CARTESIAN_POINT('',(-4.37485075966118,-0.00347109768167049,18.651410108095));
#44955=CARTESIAN_POINT('',(-4.37798451307649,0.0018411544964702,18.848589891905));
#44956=CARTESIAN_POINT('',(-4.372,-4.40683631492666E-13,-1.84858989190501));
#44957=CARTESIAN_POINT('',(-4.32479004603203,0.640761311052912,19.628));
#44958=CARTESIAN_POINT('Ctrl Pts',(-4.37485075966118,-0.00347109768167011,
18.651410108095));
#44959=CARTESIAN_POINT('Ctrl Pts',(-4.37700632796887,-0.248843725443851,
18.660359426902));
#44960=CARTESIAN_POINT('Ctrl Pts',(-4.24678226663423,-1.93862138449445,
18.7220721865693));
#44961=CARTESIAN_POINT('Ctrl Pts',(-2.04533412033072,-4.73987705500777,
18.8365483870968));
#44962=CARTESIAN_POINT('Ctrl Pts',(2.85792925831606,-4.29723869811459,18.9948387096774));
#44963=CARTESIAN_POINT('Ctrl Pts',(5.16462833680317,0.0542185969503185,
19.1531290322581));
#44964=CARTESIAN_POINT('Ctrl Pts',(2.76051461044002,4.36178489183685,19.3114193548387));
#44965=CARTESIAN_POINT('Ctrl Pts',(-1.32005059452733,4.63359119197125,19.4433279569892));
#44966=CARTESIAN_POINT('Ctrl Pts',(-3.63987183575178,2.72812739966123,19.5488548387097));
#44967=CARTESIAN_POINT('Ctrl Pts',(-4.21857665773145,1.35764386397051,19.6016182795699));
#44968=CARTESIAN_POINT('Ctrl Pts',(-4.32479004603219,0.640761311051878,
19.628));
#44969=CARTESIAN_POINT('',(-0.803308159453264,4.29756675351946,19.628));
#44970=CARTESIAN_POINT('Origin',(0.,0.,19.628));
#44971=CARTESIAN_POINT('Ctrl Pts',(-4.37798451307649,0.00184115449647014,
18.848589891905));
#44972=CARTESIAN_POINT('Ctrl Pts',(-4.37034287302321,-1.32832166361097,
18.8972071273712));
#44973=CARTESIAN_POINT('Ctrl Pts',(-3.01402217294637,-4.11556359956004,
18.9986208963121));
#44974=CARTESIAN_POINT('Ctrl Pts',(1.72525842040716,-4.86940713488401,19.1528311987277));
#44975=CARTESIAN_POINT('Ctrl Pts',(5.02276837180745,-1.19521866677756,19.3112207991518));
#44976=CARTESIAN_POINT('Ctrl Pts',(3.95306672650205,2.75529758855723,19.4432121328385));
#44977=CARTESIAN_POINT('Ctrl Pts',(1.3947178009747,4.32991044428859,19.548805199788));
#44978=CARTESIAN_POINT('Ctrl Pts',(-0.0904913830656236,4.43080762341373,
19.6016017332627));
#44979=CARTESIAN_POINT('Ctrl Pts',(-0.803308159453631,4.29756675351939,
19.628));
#44980=CARTESIAN_POINT('Origin',(0.,0.,-1.84858989190501));
#44981=CARTESIAN_POINT('',(-4.36494952125445,-0.000302537669007011,17.651410108095));
#44982=CARTESIAN_POINT('',(-4.37193807291522,-0.0039501116577445,17.848589891905));
#44983=CARTESIAN_POINT('',(-4.372,-4.40683631492666E-13,-1.84858989190501));
#44984=CARTESIAN_POINT('Ctrl Pts',(-4.36494952125446,-0.000302537669007175,
17.651410108095));
#44985=CARTESIAN_POINT('Ctrl Pts',(-4.36539179118401,-0.709016948559791,
17.6771121150741));
#44986=CARTESIAN_POINT('Ctrl Pts',(-3.86807546336294,-2.87206193474975,
17.7555775629134));
#44987=CARTESIAN_POINT('Ctrl Pts',(-0.472995886023615,-5.14054336213398,
17.8868064516129));
#44988=CARTESIAN_POINT('Ctrl Pts',(4.05270272242283,-3.19751510246813,18.0450967741935));
#44989=CARTESIAN_POINT('Ctrl Pts',(4.88945318540557,1.65605334244537,18.2033870967742));
#44990=CARTESIAN_POINT('Ctrl Pts',(1.27529601904452,5.00227852023644,18.3616774193548));
#44991=CARTESIAN_POINT('Ctrl Pts',(-3.22941067771149,3.86313894204385,18.5110184231284));
#44992=CARTESIAN_POINT('Ctrl Pts',(-4.36429751701074,1.19782550299575,18.6075959860418));
#44993=CARTESIAN_POINT('Ctrl Pts',(-4.37485075966118,-0.00347109768167011,
18.651410108095));
#44994=CARTESIAN_POINT('Ctrl Pts',(-4.37193807291522,-0.00395011165774454,
17.848589891905));
#44995=CARTESIAN_POINT('Ctrl Pts',(-4.37503172333717,-0.34380114135277,
17.8609647263816));
#44996=CARTESIAN_POINT('Ctrl Pts',(-4.18383382909851,-2.13016311819971,
17.9261360943329));
#44997=CARTESIAN_POINT('Ctrl Pts',(-1.7333097832156,-4.86367572142824,18.0441039957589));
#44998=CARTESIAN_POINT('Ctrl Pts',(3.13645552043595,-4.10159948955856,18.202493596183));
#44999=CARTESIAN_POINT('Ctrl Pts',(5.14796384574126,0.398543369117654,18.3608831966071));
#45000=CARTESIAN_POINT('Ctrl Pts',(2.46797524199195,4.53507188733415,18.5192727970312));
#45001=CARTESIAN_POINT('Ctrl Pts',(-2.46096278237594,4.53951629179981,18.6776623974553));
#45002=CARTESIAN_POINT('Ctrl Pts',(-4.32286248336998,1.67443240118537,18.7874347624133));
#45003=CARTESIAN_POINT('Ctrl Pts',(-4.37864141367461,0.116186340178791,
18.8444105938965));
#45004=CARTESIAN_POINT('Ctrl Pts',(-4.37798451307649,0.00184115449647014,
18.848589891905));
#45005=CARTESIAN_POINT('Origin',(0.,0.,-1.84858989190501));
#45006=CARTESIAN_POINT('',(-4.37363367263438,0.00377358290378073,16.651410108095));
#45007=CARTESIAN_POINT('',(-4.36517770212695,0.0011188044825361,16.848589891905));
#45008=CARTESIAN_POINT('',(-4.372,-4.40683631492666E-13,-1.84858989190501));
#45009=CARTESIAN_POINT('Ctrl Pts',(-4.37363367263438,0.00377358290378063,
16.651410108095));
#45010=CARTESIAN_POINT('Ctrl Pts',(-4.36305794810196,-1.16100169057931,
16.6938648032461));
#45011=CARTESIAN_POINT('Ctrl Pts',(-3.28678615689719,-3.7906423093463,16.7890829392575));
#45012=CARTESIAN_POINT('Ctrl Pts',(1.14681571606612,-5.03325475486043,16.937064516129));
#45013=CARTESIAN_POINT('Ctrl Pts',(4.84536125415653,-1.78081574711759,17.0953548387097));
#45014=CARTESIAN_POINT('Ctrl Pts',(4.13332826509411,3.09264287390914,17.2536451612903));
#45015=CARTESIAN_POINT('Ctrl Pts',(-0.341147903092961,5.15096781506579,
17.411935483871));
#45016=CARTESIAN_POINT('Ctrl Pts',(-3.82897189620604,2.94763574423766,17.5445237994725));
#45017=CARTESIAN_POINT('Ctrl Pts',(-4.36448385884661,0.745897095166127,
17.6243486742139));
#45018=CARTESIAN_POINT('Ctrl Pts',(-4.36494952125446,-0.000302537669007175,
17.651410108095));
#45019=CARTESIAN_POINT('Ctrl Pts',(-4.36517770212695,0.0011188044825361,
16.848589891905));
#45020=CARTESIAN_POINT('Ctrl Pts',(-4.36334200546248,-0.796471401961387,
16.8775188588667));
#45021=CARTESIAN_POINT('Ctrl Pts',(-3.77287007871479,-3.05222639411641,
16.9592443593031));
#45022=CARTESIAN_POINT('Ctrl Pts',(-0.156460816144074,-5.16096436253732,
17.0937663932142));
#45023=CARTESIAN_POINT('Ctrl Pts',(4.24417435465306,-2.94058317628852,17.2521559936383));
#45024=CARTESIAN_POINT('Ctrl Pts',(4.7770306357801,1.95960002071087,17.4105455940624));
#45025=CARTESIAN_POINT('Ctrl Pts',(0.956505601666415,5.07396180892462,17.5689351944865));
#45026=CARTESIAN_POINT('Ctrl Pts',(-3.36909691713057,3.68230599805327,17.7149499604341));
#45027=CARTESIAN_POINT('Ctrl Pts',(-4.36183283826352,1.10615411256716,17.8081681929069));
#45028=CARTESIAN_POINT('Ctrl Pts',(-4.37193807291522,-0.00395011165774454,
17.848589891905));
#45029=CARTESIAN_POINT('Origin',(0.,0.,-1.84858989190501));
#45030=CARTESIAN_POINT('',(-4.37658335244799,-0.00285917843438755,15.651410108095));
#45031=CARTESIAN_POINT('',(-4.37598752684337,0.00314030101388529,15.848589891905));
#45032=CARTESIAN_POINT('',(-4.372,-4.40683631492666E-13,-1.84858989190501));
#45033=CARTESIAN_POINT('Ctrl Pts',(-4.37658335244799,-0.00285917843438723,
15.651410108095));
#45034=CARTESIAN_POINT('Ctrl Pts',(-4.37792255245523,-0.179344027897961,
15.657854050558));
#45035=CARTESIAN_POINT('Ctrl Pts',(-4.28827874574891,-1.79952736688815,
15.7170614338811));
#45036=CARTESIAN_POINT('Ctrl Pts',(-2.26751786562628,-4.63758557609733,
15.8290322580645));
#45037=CARTESIAN_POINT('Ctrl Pts',(2.65323118895075,-4.42822781393943,15.9873225806452));
#45038=CARTESIAN_POINT('Ctrl Pts',(5.15882697608013,-0.187992963311806,
16.1456129032258));
#45039=CARTESIAN_POINT('Ctrl Pts',(2.96850419640318,4.22336596918787,16.3039032258064));
#45040=CARTESIAN_POINT('Ctrl Pts',(-1.92395505269964,4.79032719267193,16.4621935483871));
#45041=CARTESIAN_POINT('Ctrl Pts',(-4.22261913325801,2.01425606870238,16.5780291758166));
#45042=CARTESIAN_POINT('Ctrl Pts',(-4.37620164431587,0.286601478848438,
16.6411013623859));
#45043=CARTESIAN_POINT('Ctrl Pts',(-4.37363367263438,0.00377358290378063,
16.651410108095));
#45044=CARTESIAN_POINT('Ctrl Pts',(-4.37598752684337,0.00314030101388495,
15.848589891905));
#45045=CARTESIAN_POINT('Ctrl Pts',(-4.36586808840044,-1.24298125471277,
15.8940729913518));
#45046=CARTESIAN_POINT('Ctrl Pts',(-3.15685416964687,-3.95275705920985,
15.9923526242733));
#45047=CARTESIAN_POINT('Ctrl Pts',(1.43550516966593,-4.9597746708902,16.1434287906695));
#45048=CARTESIAN_POINT('Ctrl Pts',(4.94197826197569,-1.49562391370258,16.3018183910937));
#45049=CARTESIAN_POINT('Ctrl Pts',(3.94475245484231,3.3315114408263,16.4602079915177));
#45050=CARTESIAN_POINT('Ctrl Pts',(-0.647385467154988,5.12259027405121,
16.6185975919419));
#45051=CARTESIAN_POINT('Ctrl Pts',(-3.91857823830144,2.77088302731469,16.7480582254043));
#45052=CARTESIAN_POINT('Ctrl Pts',(-4.36669222603978,0.659162948528226,
16.824722325392));
#45053=CARTESIAN_POINT('Ctrl Pts',(-4.36517770212695,0.0011188044825361,
16.848589891905));
#45054=CARTESIAN_POINT('Origin',(0.,0.,-1.84858989190501));
#45055=CARTESIAN_POINT('',(-4.36535254096326,-0.00139340307212889,14.651410108095));
#45056=CARTESIAN_POINT('',(-4.37450977369375,-0.00361009500681242,14.848589891905));
#45057=CARTESIAN_POINT('',(-4.372,-4.40683631492666E-13,-1.84858989190501));
#45058=CARTESIAN_POINT('Ctrl Pts',(-4.36535254096326,-0.00139340307212868,
14.651410108095));
#45059=CARTESIAN_POINT('Ctrl Pts',(-4.36719167669768,-0.640876180485729,
14.67460673873));
#45060=CARTESIAN_POINT('Ctrl Pts',(-3.93664196772952,-2.73257986740296,
14.7505668102252));
#45061=CARTESIAN_POINT('Ctrl Pts',(-0.715156117622299,-5.11247386069707,
14.8792903225806));
#45062=CARTESIAN_POINT('Ctrl Pts',(3.89726470591888,-3.38528655547465,15.0375806451613));
#45063=CARTESIAN_POINT('Ctrl Pts',(4.96212753934002,1.42342106576975,15.1958709677419));
#45064=CARTESIAN_POINT('Ctrl Pts',(1.5101211008729,4.93643307547415,15.3541612903226));
#45065=CARTESIAN_POINT('Ctrl Pts',(-3.1200112045152,3.99587919704142,15.5060076704403));
#45066=CARTESIAN_POINT('Ctrl Pts',(-4.36695709135924,1.26572596937806,15.6050906096977));
#45067=CARTESIAN_POINT('Ctrl Pts',(-4.37658335244799,-0.00285917843438723,
15.651410108095));
#45068=CARTESIAN_POINT('Ctrl Pts',(-4.37450977369375,-0.00361009500681263,
14.848589891905));
#45069=CARTESIAN_POINT('Ctrl Pts',(-4.37676192585348,-0.2570041121813,14.8578305903622));
#45070=CARTESIAN_POINT('Ctrl Pts',(-4.24160137044629,-1.95575914866763,
14.9198678222941));
#45071=CARTESIAN_POINT('Ctrl Pts',(-2.01745869282129,-4.75288338056742,
15.0347015877008));
#45072=CARTESIAN_POINT('Ctrl Pts',(2.88882981271105,-4.27956800578602,15.1930911881249));
#45073=CARTESIAN_POINT('Ctrl Pts',(5.16248437889336,0.0937818828261288,
15.351480788549));
#45074=CARTESIAN_POINT('Ctrl Pts',(2.73148949656154,4.38166693681219,15.5098703889731));
#45075=CARTESIAN_POINT('Ctrl Pts',(-2.18875273549729,4.67647318514471,15.6682599893972));
#45076=CARTESIAN_POINT('Ctrl Pts',(-4.27423782525496,1.84868256384714,15.7811664903745));
#45077=CARTESIAN_POINT('Ctrl Pts',(-4.37761467728721,0.203509842654685,
15.8412764578771));
#45078=CARTESIAN_POINT('Ctrl Pts',(-4.37598752684337,0.00314030101388495,
15.848589891905));
#45079=CARTESIAN_POINT('Origin',(0.,0.,-1.84858989190501));
#45080=CARTESIAN_POINT('',(-4.3715702955649,0.00393516289142377,13.651410108095));
#45081=CARTESIAN_POINT('',(-4.36492411635568,-0.000270170186619789,13.848589891905));
#45082=CARTESIAN_POINT('',(-4.372,-4.40683631492666E-13,-1.84858989190501));
#45083=CARTESIAN_POINT('Ctrl Pts',(-4.3715702955649,0.00393516289142415,
13.651410108095));
#45084=CARTESIAN_POINT('Ctrl Pts',(-4.36167155640512,-1.09343140876319,
13.691359426902));
#45085=CARTESIAN_POINT('Ctrl Pts',(-3.38808352462445,-3.65581253168041,
13.7840721865693));
#45086=CARTESIAN_POINT('Ctrl Pts',(0.907928552289056,-5.08178147829179,
13.9295483870968));
#45087=CARTESIAN_POINT('Ctrl Pts',(4.75589152831045,-2.00756893285326,14.0878387096774));
#45088=CARTESIAN_POINT('Ctrl Pts',(4.2747154125816,2.89407073006048,14.2461290322581));
#45089=CARTESIAN_POINT('Ctrl Pts',(-0.0976002483683332,5.16132845696157,
14.4044193548387));
#45090=CARTESIAN_POINT('Ctrl Pts',(-3.75335254656528,3.08663197095523,14.5395130467844));
#45091=CARTESIAN_POINT('Ctrl Pts',(-4.36300834804604,0.813701953645304,
14.6218432978698));
#45092=CARTESIAN_POINT('Ctrl Pts',(-4.36535254096326,-0.00139340307212868,
14.651410108095));
#45093=CARTESIAN_POINT('Ctrl Pts',(-4.36492411635568,-0.000270170186619789,
13.848589891905));
#45094=CARTESIAN_POINT('Ctrl Pts',(-4.36531805977148,-0.711553376731479,
13.8743847228474));
#45095=CARTESIAN_POINT('Ctrl Pts',(-3.86529136737144,-2.8781600308068,13.9529760872644));
#45096=CARTESIAN_POINT('Ctrl Pts',(-0.460905372910369,-5.14272362102755,
14.0843639851561));
#45097=CARTESIAN_POINT('Ctrl Pts',(4.06315051784514,-3.18603952805496,14.2427535855802));
#45098=CARTESIAN_POINT('Ctrl Pts',(4.88439639669049,1.67413017563193,14.4011431860043));
#45099=CARTESIAN_POINT('Ctrl Pts',(1.25441857601452,5.00863993928383,14.5595327864284));
#45100=CARTESIAN_POINT('Ctrl Pts',(-3.24025672884045,3.85045757200017,14.7086816883953));
#45101=CARTESIAN_POINT('Ctrl Pts',(-4.36389430254103,1.19075719850307,14.8050340568875));
#45102=CARTESIAN_POINT('Ctrl Pts',(-4.37450977369375,-0.00361009500681263,
14.848589891905));
#45103=CARTESIAN_POINT('Origin',(0.,0.,-1.84858989190501));
#45104=CARTESIAN_POINT('',(-4.37805463091546,-0.00189096989131645,12.651410108095));
#45105=CARTESIAN_POINT('',(-4.3735298381194,0.00380331467108683,12.848589891905));
#45106=CARTESIAN_POINT('',(-4.372,-4.40683631492666E-13,-1.84858989190501));
#45107=CARTESIAN_POINT('Ctrl Pts',(-4.37805463091546,-0.00189096989131629,
12.651410108095));
#45108=CARTESIAN_POINT('Ctrl Pts',(-4.37864191593093,-0.109663799931991,
12.6553486742139));
#45109=CARTESIAN_POINT('Ctrl Pts',(-4.32628239365674,-1.66064736718339,
12.7120506811929));
#45110=CARTESIAN_POINT('Ctrl Pts',(-2.4839194519693,-4.5253708583176,12.8215161290323));
#45111=CARTESIAN_POINT('Ctrl Pts',(2.44122672465452,-4.54854364912704,12.9798064516129));
#45112=CARTESIAN_POINT('Ctrl Pts',(5.14420067918421,-0.431319627959304,
13.1380967741936));
#45113=CARTESIAN_POINT('Ctrl Pts',(3.16456988475122,4.07852114052473,13.2963870967742));
#45114=CARTESIAN_POINT('Ctrl Pts',(-1.69566975348524,4.87581186432528,13.4546774193548));
#45115=CARTESIAN_POINT('Ctrl Pts',(-4.17531922896613,2.15372155886245,13.5730184231284));
#45116=CARTESIAN_POINT('Ctrl Pts',(-4.37474540982351,0.355925875277971,
13.6385959860418));
#45117=CARTESIAN_POINT('Ctrl Pts',(-4.3715702955649,0.00393516289142415,
13.651410108095));
#45118=CARTESIAN_POINT('Ctrl Pts',(-4.3735298381194,0.00380331467108686,
12.848589891905));
#45119=CARTESIAN_POINT('Ctrl Pts',(-4.36293974589787,-1.15814174670351,
12.8909388553325));
#45120=CARTESIAN_POINT('Ctrl Pts',(-3.29085772231164,-3.78595162322649,
12.9860843522346));
#45121=CARTESIAN_POINT('Ctrl Pts',(1.14016230868481,-5.03587826648703,13.1340263826114));
#45122=CARTESIAN_POINT('Ctrl Pts',(4.84505108113381,-1.78480251743019,13.2924159830355));
#45123=CARTESIAN_POINT('Ctrl Pts',(4.13457213027864,3.09279053680373,13.4508055834596));
#45124=CARTESIAN_POINT('Ctrl Pts',(-0.343804419177731,5.15187718471428,
13.6091951838838));
#45125=CARTESIAN_POINT('Ctrl Pts',(-3.8305579098897,2.94525464061577,13.7417899533655));
#45126=CARTESIAN_POINT('Ctrl Pts',(-4.36451174137436,0.744292087358565,
13.8215881893726));
#45127=CARTESIAN_POINT('Ctrl Pts',(-4.36492411635568,-0.000270170186619789,
13.848589891905));
#45128=CARTESIAN_POINT('Origin',(0.,0.,-1.84858989190501));
#45129=CARTESIAN_POINT('',(-4.3662580307389,-0.00237411499775451,11.651410108095));
#45130=CARTESIAN_POINT('',(-4.37682453544783,-0.00275176080394124,11.848589891905));
#45131=CARTESIAN_POINT('',(-4.372,-4.40683631492666E-13,-1.84858989190501));
#45132=CARTESIAN_POINT('Ctrl Pts',(-4.3662580307389,-0.00237411499775443,
11.651410108095));
#45133=CARTESIAN_POINT('Ctrl Pts',(-4.36908770984708,-0.57249276395778,
11.6721013623859));
#45134=CARTESIAN_POINT('Ctrl Pts',(-4.00080778508103,-2.59292231754593,
11.745556057537));
#45135=CARTESIAN_POINT('Ctrl Pts',(-0.955706815437237,-5.07301308219371,
11.8717741935484));
#45136=CARTESIAN_POINT('Ctrl Pts',(3.73310810644377,-3.5654931096253,12.030064516129));
#45137=CARTESIAN_POINT('Ctrl Pts',(5.02379164936073,1.1875835604264,12.1883548387097));
#45138=CARTESIAN_POINT('Ctrl Pts',(1.74147501164997,4.85964011352491,12.3466451612903));
#45139=CARTESIAN_POINT('Ctrl Pts',(-3.00493840101716,4.12681778354368,12.5009969177521));
#45140=CARTESIAN_POINT('Ctrl Pts',(-4.3707742866348,1.33412695349428,12.6025852333536));
#45141=CARTESIAN_POINT('Ctrl Pts',(-4.37805463091546,-0.00189096989131629,
12.651410108095));
#45142=CARTESIAN_POINT('Ctrl Pts',(-4.37682453544783,-0.0027517608039412,
11.848589891905));
#45143=CARTESIAN_POINT('Ctrl Pts',(-4.37805680950565,-0.169972374992373,
11.8546964543429));
#45144=CARTESIAN_POINT('Ctrl Pts',(-4.29358524369388,-1.7817038588778,11.9135995502554));
#45145=CARTESIAN_POINT('Ctrl Pts',(-2.29456228398659,-4.62547553554524,
12.0252991796426));
#45146=CARTESIAN_POINT('Ctrl Pts',(2.63111281568934,-4.44266646915302,12.1836887800668));
#45147=CARTESIAN_POINT('Ctrl Pts',(5.15901534120123,-0.211188811899807,
12.3420783804909));
#45148=CARTESIAN_POINT('Ctrl Pts',(2.98542980392062,4.2127483773522,12.500467980915));
#45149=CARTESIAN_POINT('Ctrl Pts',(-1.90882269345658,4.79754478144462,12.6588575813391));
#45150=CARTESIAN_POINT('Ctrl Pts',(-4.22005393336117,2.0228792487521,12.7748982183358));
#45151=CARTESIAN_POINT('Ctrl Pts',(-4.37614243406833,0.290457377422949,
12.8381423218578));
#45152=CARTESIAN_POINT('Ctrl Pts',(-4.3735298381194,0.00380331467108686,
12.848589891905));
#45153=CARTESIAN_POINT('Origin',(0.,0.,-1.84858989190501));
#45154=CARTESIAN_POINT('',(-4.36958950328423,0.00375500997191766,10.651410108095));
#45155=CARTESIAN_POINT('',(-4.36549183168559,-0.00162636191587406,10.848589891905));
#45156=CARTESIAN_POINT('',(-4.372,-4.40683631492666E-13,-1.84858989190501));
#45157=CARTESIAN_POINT('Ctrl Pts',(-4.36958950328423,0.00375500997191747,
10.651410108095));
#45158=CARTESIAN_POINT('Ctrl Pts',(-4.36106090852754,-1.0259785981898,10.688854050558));
#45159=CARTESIAN_POINT('Ctrl Pts',(-3.48414488794968,-3.51981628552574,
10.7790614338811));
#45160=CARTESIAN_POINT('Ctrl Pts',(0.667017186951725,-5.11897697997292,
10.9220322580645));
#45161=CARTESIAN_POINT('Ctrl Pts',(4.65581649466175,-2.22984528997355,11.0803225806452));
#45162=CARTESIAN_POINT('Ctrl Pts',(4.40657187915952,2.68904472312794,11.2386129032258));
#45163=CARTESIAN_POINT('Ctrl Pts',(0.14616290696869,5.16018155240764,11.3969032258064));
#45164=CARTESIAN_POINT('Ctrl Pts',(-3.67299362448513,3.22514497791193,11.5345022940962));
#45165=CARTESIAN_POINT('Ctrl Pts',(-4.36187192659012,0.881330247193059,
11.6193379215257));
#45166=CARTESIAN_POINT('Ctrl Pts',(-4.3662580307389,-0.00237411499775443,
11.651410108095));
#45167=CARTESIAN_POINT('Ctrl Pts',(-4.36549183168559,-0.00162636191587386,
10.848589891905));
#45168=CARTESIAN_POINT('Ctrl Pts',(-4.36759069612872,-0.626283874484138,
10.871250586828));
#45169=CARTESIAN_POINT('Ctrl Pts',(-3.95060522485931,-2.70364125089475,
10.9467078152256));
#45170=CARTESIAN_POINT('Ctrl Pts',(-0.763741663751577,-5.10653881568242,
11.074961577098));
#45171=CARTESIAN_POINT('Ctrl Pts',(3.86794975738412,-3.42038077988013,11.2333511775221));
#45172=CARTESIAN_POINT('Ctrl Pts',(4.97472054752429,1.38282156443299,11.3917407779462));
#45173=CARTESIAN_POINT('Ctrl Pts',(1.54795388466898,4.92583787552529,11.5501303783703));
#45174=CARTESIAN_POINT('Ctrl Pts',(-3.10298340129681,4.01633537157594,11.7024134163566));
#45175=CARTESIAN_POINT('Ctrl Pts',(-4.36740273051995,1.27579500142313,11.8018999208682));
#45176=CARTESIAN_POINT('Ctrl Pts',(-4.37682453544783,-0.0027517608039412,
11.848589891905));
#45177=CARTESIAN_POINT('Origin',(0.,0.,-1.84858989190501));
#45178=CARTESIAN_POINT('',(-4.37893064514985,-0.000718125850480163,9.65141010809499));
#45179=CARTESIAN_POINT('',(-4.37095165486262,0.00392878392899476,9.84858989190502));
#45180=CARTESIAN_POINT('',(-4.372,-4.40683631492666E-13,-1.84858989190501));
#45181=CARTESIAN_POINT('Ctrl Pts',(-4.37893064514985,-0.000718125850479884,
9.65141010809498));
#45182=CARTESIAN_POINT('Ctrl Pts',(-4.37902043646228,-0.0399142522790172,
9.65284329786977));
#45183=CARTESIAN_POINT('Ctrl Pts',(-4.36082969860212,-1.52204564057694,
9.70703992850478));
#45184=CARTESIAN_POINT('Ctrl Pts',(-2.69478237803987,-4.40306543037773,
9.81399999999999));
#45185=CARTESIAN_POINT('Ctrl Pts',(2.22377879965116,-4.65871710875468,9.97229032258064));
#45186=CARTESIAN_POINT('Ctrl Pts',(5.11810379036282,-0.67368452576514,10.1305806451613));
#45187=CARTESIAN_POINT('Ctrl Pts',(3.35357921258595,3.92458197953528,10.2888709677419));
#45188=CARTESIAN_POINT('Ctrl Pts',(-1.46360347987537,4.95042443663959,10.4471612903226));
#45189=CARTESIAN_POINT('Ctrl Pts',(-4.12415016732119,2.29334108429437,10.5680076704403));
#45190=CARTESIAN_POINT('Ctrl Pts',(-4.37307882051719,0.425051522096353,
10.6360906096977));
#45191=CARTESIAN_POINT('Ctrl Pts',(-4.36958950328423,0.00375500997191747,
10.651410108095));
#45192=CARTESIAN_POINT('Ctrl Pts',(-4.37095165486262,0.00392878392899445,
9.84858989190502));
#45193=CARTESIAN_POINT('Ctrl Pts',(-4.36138099894435,-1.0736503956833,9.88780471931308));
#45194=CARTESIAN_POINT('Ctrl Pts',(-3.41650604254828,-3.61702144425598,
9.97981608019584));
#45195=CARTESIAN_POINT('Ctrl Pts',(0.840841326532404,-5.09441123866306,
10.1246239745533));
#45196=CARTESIAN_POINT('Ctrl Pts',(4.73121909778617,-2.06775381846214,10.2830135749774));
#45197=CARTESIAN_POINT('Ctrl Pts',(4.30996593957687,2.84327867165857,10.4414031754015));
#45198=CARTESIAN_POINT('Ctrl Pts',(-0.0390238264566685,5.16318866070086,
10.5997927758256));
#45199=CARTESIAN_POINT('Ctrl Pts',(-3.7353314916358,3.11908229388608,10.7355216813268));
#45200=CARTESIAN_POINT('Ctrl Pts',(-4.36270060925329,0.829088583628261,
10.8184540533533));
#45201=CARTESIAN_POINT('Ctrl Pts',(-4.36549183168559,-0.00162636191587386,
10.848589891905));
#45202=CARTESIAN_POINT('Origin',(0.,0.,-1.84858989190501));
#45203=CARTESIAN_POINT('',(-4.3676089549007,-0.00316636266463396,8.65141010809498));
#45204=CARTESIAN_POINT('',(-4.3784939599728,-0.00146115515596901,8.84858989190502));
#45205=CARTESIAN_POINT('',(-4.372,-4.40683631492666E-13,-1.84858989190501));
#45206=CARTESIAN_POINT('Ctrl Pts',(-4.3676089549007,-0.0031663626646336,
8.65141010809498));
#45207=CARTESIAN_POINT('Ctrl Pts',(-4.37099157996906,-0.503863509155134,
8.66959598604181));
#45208=CARTESIAN_POINT('Ctrl Pts',(-4.0607005189635,-2.45318988687306,8.74054530484886));
#45209=CARTESIAN_POINT('Ctrl Pts',(-1.19412647058753,-5.02224045834365,
8.86425806451613));
#45210=CARTESIAN_POINT('Ctrl Pts',(3.56062739266322,-3.73774929868204,9.02254838709676));
#45211=CARTESIAN_POINT('Ctrl Pts',(5.07425366817473,0.949097971864315,9.18083870967742));
#45212=CARTESIAN_POINT('Ctrl Pts',(1.96894576792944,4.77201108675727,9.33912903225805));
#45213=CARTESIAN_POINT('Ctrl Pts',(-2.88428822201713,4.2558282973375,9.49598616506391));
#45214=CARTESIAN_POINT('Ctrl Pts',(-4.37571473425415,1.40310643844898,9.60007985700956));
#45215=CARTESIAN_POINT('Ctrl Pts',(-4.37893064514985,-0.000718125850479884,
9.65141010809498));
#45216=CARTESIAN_POINT('Ctrl Pts',(-4.3784939599728,-0.00146115515596968,
8.84858989190502));
#45217=CARTESIAN_POINT('Ctrl Pts',(-4.37884870232368,-0.0827753827151446,
8.85156231832348));
#45218=CARTESIAN_POINT('Ctrl Pts',(-4.34001073551865,-1.6080554399903,8.90733127821665));
#45219=CARTESIAN_POINT('Ctrl Pts',(-2.56365995117077,-4.48192901101572,
9.01589677158451));
#45220=CARTESIAN_POINT('Ctrl Pts',(2.36421564112952,-4.59026408905411,9.17428637200862));
#45221=CARTESIAN_POINT('Ctrl Pts',(5.13754605775107,-0.515422651333577,
9.33267597243274));
#45222=CARTESIAN_POINT('Ctrl Pts',(3.22895369161553,4.02913117959985,9.49106557285684));
#45223=CARTESIAN_POINT('Ctrl Pts',(-1.62223260619563,4.90187733184103,9.64945517328097));
#45224=CARTESIAN_POINT('Ctrl Pts',(-4.15999532952882,2.19738929405191,9.76862994629701));
#45225=CARTESIAN_POINT('Ctrl Pts',(-4.37426636626487,0.377138731501872,
9.83500818583837));
#45226=CARTESIAN_POINT('Ctrl Pts',(-4.37095165486262,0.00392878392899445,
9.84858989190502));
#45227=CARTESIAN_POINT('Origin',(0.,0.,-1.84858989190501));
#45228=CARTESIAN_POINT('',(-4.36783565389082,0.00326080189849165,7.65141010809498));
#45229=CARTESIAN_POINT('',(-4.36682740614764,-0.00278338701585445,7.84858989190503));
#45230=CARTESIAN_POINT('',(-4.372,-4.40683631492666E-13,-1.84858989190501));
#45231=CARTESIAN_POINT('Ctrl Pts',(-4.36783565389082,0.0032608018984915,
7.65141010809498));
#45232=CARTESIAN_POINT('Ctrl Pts',(-4.36111999858997,-0.958548857288375,
7.68634867421386));
#45233=CARTESIAN_POINT('Ctrl Pts',(-3.57508309710888,-3.38283964502905,
7.77405068119295));
#45234=CARTESIAN_POINT('Ctrl Pts',(0.424618501333285,-5.14475814567673,
7.91451612903225));
#45235=CARTESIAN_POINT('Ctrl Pts',(4.54535988400859,-2.44714952016159,8.0728064516129));
#45236=CARTESIAN_POINT('Ctrl Pts',(4.52860253637045,2.47802266268103,8.23109677419354));
#45237=CARTESIAN_POINT('Ctrl Pts',(0.389600147091602,5.14752843358518,8.38938709677419));
#45238=CARTESIAN_POINT('Ctrl Pts',(-3.58777114537366,3.36303202741965,8.52949154140801));
#45239=CARTESIAN_POINT('Ctrl Pts',(-4.36117742976588,0.948829858465871,
8.6168325451816));
#45240=CARTESIAN_POINT('Ctrl Pts',(-4.3676089549007,-0.0031663626646336,
8.65141010809498));
#45241=CARTESIAN_POINT('Ctrl Pts',(-4.36682740614764,-0.00278338701585466,
7.84858989190503));
#45242=CARTESIAN_POINT('Ctrl Pts',(-4.36998031573444,-0.540633837652302,
7.8681164508086));
#45243=CARTESIAN_POINT('Ctrl Pts',(-4.02906901036793,-2.52888541639766,
7.94043954318687));
#45244=CARTESIAN_POINT('Ctrl Pts',(-1.06391319462353,-5.05253685976928,
8.06555916903983));
#45245=CARTESIAN_POINT('Ctrl Pts',(3.65925338948522,-3.64278803069328,8.22394876946396));
#45246=CARTESIAN_POINT('Ctrl Pts',(5.04768747299395,1.08668817054443,8.38233836988805));
#45247=CARTESIAN_POINT('Ctrl Pts',(1.83608824986349,4.82584914224785,8.54072797031219));
#45248=CARTESIAN_POINT('Ctrl Pts',(-2.95709387717496,4.17950307750852,8.69614514431782));
#45249=CARTESIAN_POINT('Ctrl Pts',(-4.37254773342937,1.36153600902825,8.79876578484878));
#45250=CARTESIAN_POINT('Ctrl Pts',(-4.3784939599728,-0.00146115515596968,
8.84858989190502));
#45251=CARTESIAN_POINT('Origin',(0.,0.,-1.84858989190501));
#45252=CARTESIAN_POINT('',(-4.37899478532443,0.000538853135781114,6.65141010809498));
#45253=CARTESIAN_POINT('',(-4.36857373794226,0.00352936749739713,6.84858989190502));
#45254=CARTESIAN_POINT('',(-4.372,-4.40683631492666E-13,-1.84858989190501));
#45255=CARTESIAN_POINT('Ctrl Pts',(-4.37899478532443,0.00053885313578114,
6.65141010809498));
#45256=CARTESIAN_POINT('Ctrl Pts',(-4.37652423695377,-1.41310306479934,
6.7031013623859));
#45257=CARTESIAN_POINT('Ctrl Pts',(-2.86643925520047,-4.27424452468468,
6.80755605753705));
#45258=CARTESIAN_POINT('Ctrl Pts',(2.00137227482285,-4.75850252356265,6.96477419354837));
#45259=CARTESIAN_POINT('Ctrl Pts',(5.08059451261016,-0.914547236405604,
7.12306451612904));
#45260=CARTESIAN_POINT('Ctrl Pts',(3.53511070256229,3.76189175413264,7.28135483870967));
#45261=CARTESIAN_POINT('Ctrl Pts',(-1.22827365147281,5.01399851279189,7.43964516129032));
#45262=CARTESIAN_POINT('Ctrl Pts',(-4.06898604612617,2.43305468214084,7.56299691775209));
#45263=CARTESIAN_POINT('Ctrl Pts',(-4.37126183097366,0.493954571118568,
7.63358523335364));
#45264=CARTESIAN_POINT('Ctrl Pts',(-4.36783565389082,0.0032608018984915,
7.65141010809498));
#45265=CARTESIAN_POINT('Ctrl Pts',(-4.36857373794226,0.00352936749739713,
6.84858989190502));
#45266=CARTESIAN_POINT('Ctrl Pts',(-4.3609877808655,-0.989297031049394,
6.8846705832937));
#45267=CARTESIAN_POINT('Ctrl Pts',(-3.53400975081915,-3.4463519724339,6.97354780815709));
#45268=CARTESIAN_POINT('Ctrl Pts',(0.538586577094185,-5.13516937442138,
7.11522156649516));
#45269=CARTESIAN_POINT('Ctrl Pts',(4.60087948645563,-2.34349054961462,7.27361116691928));
#45270=CARTESIAN_POINT('Ctrl Pts',(4.47032190918109,2.58384636410851,7.43200076734339));
#45271=CARTESIAN_POINT('Ctrl Pts',(0.26589292373178,5.15648532996368,7.59039036776751));
#45272=CARTESIAN_POINT('Ctrl Pts',(-3.63264590427038,3.29210602756316,7.72925340928804));
#45273=CARTESIAN_POINT('Ctrl Pts',(-4.3614553781167,0.913623385120531,7.81531991733389));
#45274=CARTESIAN_POINT('Ctrl Pts',(-4.36682740614764,-0.00278338701585466,
7.84858989190503));
#45275=CARTESIAN_POINT('Origin',(0.,0.,-1.84858989190501));
#45276=CARTESIAN_POINT('',(-4.36931971855082,-0.00370222284602327,5.65141010809498));
#45277=CARTESIAN_POINT('',(-4.37909655387308,8.17972643269707E-5,5.84858989190502));
#45278=CARTESIAN_POINT('',(-4.372,-4.40683631492666E-13,-1.84858989190501));
#45279=CARTESIAN_POINT('Ctrl Pts',(-4.36931971855082,-0.00370222284602335,
5.65141010809498));
#45280=CARTESIAN_POINT('Ctrl Pts',(-4.37282475456675,-0.434994053437505,
5.66709060969773));
#45281=CARTESIAN_POINT('Ctrl Pts',(-4.11645084466375,-2.3134683703663,5.73553455216068));
#45282=CARTESIAN_POINT('Ctrl Pts',(-1.42988345294528,-4.96026920238937,
5.85674193548387));
#45283=CARTESIAN_POINT('Ctrl Pts',(3.38020716333018,-3.90167102433782,6.01503225806451));
#45284=CARTESIAN_POINT('Ctrl Pts',(5.11340107541181,0.708496077023162,6.17332258064516));
#45285=CARTESIAN_POINT('Ctrl Pts',(2.19202615312461,4.67374139134797,6.3316129032258));
#45286=CARTESIAN_POINT('Ctrl Pts',(-2.72468151658193,4.38462631046011,6.48990322580645));
#45287=CARTESIAN_POINT('Ctrl Pts',(-4.36552898201431,1.50209810391025,6.59650229409617));
#45288=CARTESIAN_POINT('Ctrl Pts',(-4.37904602975287,0.0298607935490157,
6.65033792152568));
#45289=CARTESIAN_POINT('Ctrl Pts',(-4.37899478532443,0.00053885313578114,
6.65141010809498));
#45290=CARTESIAN_POINT('Ctrl Pts',(-4.37909655387308,8.17972643267733E-5,
5.84858989190502));
#45291=CARTESIAN_POINT('Ctrl Pts',(-4.37869792746944,-1.43927515570558,
5.90122471577881));
#45292=CARTESIAN_POINT('Ctrl Pts',(-2.8187969284654,-4.3231521197151,6.0066560731273));
#45293=CARTESIAN_POINT('Ctrl Pts',(2.08906951604171,-4.72184588505036,6.16488396395049));
#45294=CARTESIAN_POINT('Ctrl Pts',(5.098151436811,-0.817858137064712,6.32327356437462));
#45295=CARTESIAN_POINT('Ctrl Pts',(3.46121148378334,3.83145599864432,6.48166316479871));
#45296=CARTESIAN_POINT('Ctrl Pts',(-1.32998241066,4.98910681308353,6.64005276522284));
#45297=CARTESIAN_POINT('Ctrl Pts',(-4.09382090065572,2.37211345116906,6.76236167425826));
#45298=CARTESIAN_POINT('Ctrl Pts',(-4.37208823990123,0.463496420738366,
6.831874049819));
#45299=CARTESIAN_POINT('Ctrl Pts',(-4.36857373794226,0.00352936749739713,
6.84858989190502));
#45300=CARTESIAN_POINT('Origin',(0.,0.,-1.84858989190501));
#45301=CARTESIAN_POINT('',(-4.36642690985212,0.00250163610255838,4.65141010809498));
#45302=CARTESIAN_POINT('',(-4.36880169481863,-0.00359316639133633,4.84858989190502));
#45303=CARTESIAN_POINT('',(-4.372,-4.40683631492666E-13,-1.84858989190501));
#45304=CARTESIAN_POINT('Ctrl Pts',(-4.36642690985212,0.00250163610255878,
4.65141010809498));
#45305=CARTESIAN_POINT('Ctrl Pts',(-4.36174213540044,-0.891062986338486,
4.68384329786977));
#45306=CARTESIAN_POINT('Ctrl Pts',(-3.66101665548786,-3.24505548151499,
4.76903992850477));
#45307=CARTESIAN_POINT('Ctrl Pts',(0.181272997936893,-5.15906748833169,
4.907));
#45308=CARTESIAN_POINT('Ctrl Pts',(4.4247679934035,-2.65899707670991,5.06529032258064));
#45309=CARTESIAN_POINT('Ctrl Pts',(4.64053527927078,2.26147508740778,5.22358064516129));
#45310=CARTESIAN_POINT('Ctrl Pts',(0.63216865368283,5.12339731452249,5.38187096774192));
#45311=CARTESIAN_POINT('Ctrl Pts',(-3.49756148837773,3.50013537491244,5.52448078871984));
#45312=CARTESIAN_POINT('Ctrl Pts',(-4.361030631826,1.01626315589314,5.61432716883751));
#45313=CARTESIAN_POINT('Ctrl Pts',(-4.36931971855082,-0.00370222284602335,
5.65141010809498));
#45314=CARTESIAN_POINT('Ctrl Pts',(-4.36880169481863,-0.00359316639133644,
4.84858989190502));
#45315=CARTESIAN_POINT('Ctrl Pts',(-4.37232350022417,-0.454601269873613,
4.86498231478922));
#45316=CARTESIAN_POINT('Ctrl Pts',(-4.10093982798236,-2.35407682434418,
4.93417127114812));
#45317=CARTESIAN_POINT('Ctrl Pts',(-1.36037264139205,-4.98090617072295,
5.05615676098171));
#45318=CARTESIAN_POINT('Ctrl Pts',(3.43778957362211,-3.85248528258675,5.21454636140584));
#45319=CARTESIAN_POINT('Ctrl Pts',(5.10304258525828,0.786763228710822,5.37293596182993));
#45320=CARTESIAN_POINT('Ctrl Pts',(2.11781634615703,4.70902260867037,5.53132556225406));
#45321=CARTESIAN_POINT('Ctrl Pts',(-2.79740769526454,4.33987905263503,5.68971516267816));
#45322=CARTESIAN_POINT('Ctrl Pts',(-4.37709282415761,1.45270398568835,5.79546993922849));
#45323=CARTESIAN_POINT('Ctrl Pts',(-4.37909777857019,0.00450392355468565,
5.84842818230411));
#45324=CARTESIAN_POINT('Ctrl Pts',(-4.37909655387308,8.17972643267733E-5,
5.84858989190502));
#45325=CARTESIAN_POINT('Origin',(0.,0.,-1.84858989190501));
#45326=CARTESIAN_POINT('',(-4.37822270954365,0.00173219555018226,3.65141010809498));
#45327=CARTESIAN_POINT('',(-4.36665723562798,0.00267775706545931,3.84858989190502));
#45328=CARTESIAN_POINT('',(-4.372,-4.40683631492666E-13,-1.84858989190501));
#45329=CARTESIAN_POINT('Ctrl Pts',(-4.37822270954365,0.00173219555018251,
3.65141010809498));
#45330=CARTESIAN_POINT('Ctrl Pts',(-4.37141484073147,-1.3440268941613,3.70059598604181));
#45331=CARTESIAN_POINT('Ctrl Pts',(-2.98789956101879,-4.1455315666631,3.80254530484886));
#45332=CARTESIAN_POINT('Ctrl Pts',(1.77450307237079,-4.84767739015689,3.95725806451612));
#45333=CARTESIAN_POINT('Ctrl Pts',(5.03175648528012,-1.15337068283656,4.11554838709677));
#45334=CARTESIAN_POINT('Ctrl Pts',(3.7087595738537,3.5908132325819,4.27383870967742));
#45335=CARTESIAN_POINT('Ctrl Pts',(-0.990205008382098,5.06639233464293,
4.43212903225806));
#45336=CARTESIAN_POINT('Ctrl Pts',(-4.00969822487022,2.57279053906618,4.55798616506392));
#45337=CARTESIAN_POINT('Ctrl Pts',(-4.36936348937275,0.562619011588028,
4.63107985700956));
#45338=CARTESIAN_POINT('Ctrl Pts',(-4.36642690985212,0.00250163610255878,
4.65141010809498));
#45339=CARTESIAN_POINT('Ctrl Pts',(-4.36665723562798,0.00267775706545938,
3.84858989190502));
#45340=CARTESIAN_POINT('Ctrl Pts',(-4.36155175532508,-0.904909371632279,
3.88153644727432));
#45341=CARTESIAN_POINT('Ctrl Pts',(-3.64359471136329,-3.27429676880991,
3.96727953611833));
#45342=CARTESIAN_POINT('Ctrl Pts',(0.234452652827207,-5.15801046495039,
4.10581915843705));
#45343=CARTESIAN_POINT('Ctrl Pts',(4.4544870133001,-2.61105064195526,4.26420875886115));
#45344=CARTESIAN_POINT('Ctrl Pts',(4.61508054334482,2.31539879571022,4.42259835928526));
#45345=CARTESIAN_POINT('Ctrl Pts',(0.56988195080356,5.13179058096912,4.58098795970938));
#45346=CARTESIAN_POINT('Ctrl Pts',(-3.52225462180705,3.46403365178023,4.72298513724929));
#45347=CARTESIAN_POINT('Ctrl Pts',(-4.36098050850789,0.998000618272236,
4.81218578131451));
#45348=CARTESIAN_POINT('Ctrl Pts',(-4.36880169481863,-0.00359316639133644,
4.84858989190502));
#45349=CARTESIAN_POINT('Origin',(0.,0.,-1.84858989190501));
#45350=CARTESIAN_POINT('',(-4.3712761175009,-0.0039298912494793,2.65141010809498));
#45351=CARTESIAN_POINT('',(-4.37836367713493,0.00160984593324705,2.84858989190502));
#45352=CARTESIAN_POINT('',(-4.372,-4.40683631492666E-13,-1.84858989190501));
#45353=CARTESIAN_POINT('Ctrl Pts',(-4.3712761175009,-0.00392989124947909,
2.65141010809498));
#45354=CARTESIAN_POINT('Ctrl Pts',(-4.37451696257115,-0.365899162664298,
2.66458523335364));
#45355=CARTESIAN_POINT('Ctrl Pts',(-4.16818790357475,-2.17383119834201,
2.73052379947252));
#45356=CARTESIAN_POINT('Ctrl Pts',(-1.66245191543707,-4.88723759858308,
2.84922580645161));
#45357=CARTESIAN_POINT('Ctrl Pts',(3.19224964022283,-4.05689272016998,3.00751612903226));
#45358=CARTESIAN_POINT('Ctrl Pts',(5.14114662208426,0.466314344506177,3.1658064516129));
#45359=CARTESIAN_POINT('Ctrl Pts',(2.41021871871718,4.56505016420442,3.32409677419355));
#45360=CARTESIAN_POINT('Ctrl Pts',(-2.5146557123555,4.50836375769575,3.48238709677419));
#45361=CARTESIAN_POINT('Ctrl Pts',(-4.33147098232467,1.64065849811777,3.591491541408));
#45362=CARTESIAN_POINT('Ctrl Pts',(-4.37871788376841,0.0996167512533684,
3.6478325451816));
#45363=CARTESIAN_POINT('Ctrl Pts',(-4.37822270954365,0.00173219555018251,
3.65141010809498));
#45364=CARTESIAN_POINT('Ctrl Pts',(-4.37836367713493,0.00160984593324717,
2.84858989190502));
#45365=CARTESIAN_POINT('Ctrl Pts',(-4.37193582834707,-1.35264708506912,
2.89809057975943));
#45366=CARTESIAN_POINT('Ctrl Pts',(-2.9725521843832,-4.16280399703585,3.00038780108855));
#45367=CARTESIAN_POINT('Ctrl Pts',(1.80663443860224,-4.83695274769126,3.15548155589238));
#45368=CARTESIAN_POINT('Ctrl Pts',(5.04096893490742,-1.11744005069485,3.31387115631648));
#45369=CARTESIAN_POINT('Ctrl Pts',(3.68139281034196,3.62041254264275,3.4722607567406));
#45370=CARTESIAN_POINT('Ctrl Pts',(-1.03309179131411,5.05892887272037,3.63065035716471));
#45371=CARTESIAN_POINT('Ctrl Pts',(-4.0212815682019,2.54692422938098,3.75609340221952));
#45372=CARTESIAN_POINT('Ctrl Pts',(-4.36973323768933,0.549490145536826,
3.82873991379962));
#45373=CARTESIAN_POINT('Ctrl Pts',(-4.36665723562798,0.00267775706545938,
3.84858989190502));
#45374=CARTESIAN_POINT('Origin',(0.,0.,-1.84858989190501));
#45375=CARTESIAN_POINT('',(-4.36544656918105,0.00153916655095219,1.65141010809498));
#45376=CARTESIAN_POINT('',(-4.37121340809612,-0.00394090090135357,1.84858989190502));
#45377=CARTESIAN_POINT('',(-4.372,-4.40683631492666E-13,-1.84858989190501));
#45378=CARTESIAN_POINT('Ctrl Pts',(-4.36544656918105,0.00153916655095176,
1.65141010809498));
#45379=CARTESIAN_POINT('Ctrl Pts',(-4.36281788561468,-0.823458774996837,
1.68133792152568));
#45380=CARTESIAN_POINT('Ctrl Pts',(-3.74207983653693,-3.10661615213039,
1.76402917581661));
#45381=CARTESIAN_POINT('Ctrl Pts',(-0.0624691826164238,-5.16187799225891,
1.89948387096774));
#45382=CARTESIAN_POINT('Ctrl Pts',(4.29430578210828,-2.8649130214088,2.05777419354839));
#45383=CARTESIAN_POINT('Ctrl Pts',(4.74212257914569,2.03988351823947,2.21606451612903));
#45384=CARTESIAN_POINT('Ctrl Pts',(0.873326467994359,5.08784270323556,2.37435483870968));
#45385=CARTESIAN_POINT('Ctrl Pts',(-3.40224500791429,3.63628377215307,2.51947003603166));
#45386=CARTESIAN_POINT('Ctrl Pts',(-4.36153810021927,1.08370711208091,2.61182179249343));
#45387=CARTESIAN_POINT('Ctrl Pts',(-4.3712761175009,-0.00392989124947909,
2.65141010809498));
#45388=CARTESIAN_POINT('Ctrl Pts',(-4.37121340809612,-0.00394090090135399,
1.84858989190502));
#45389=CARTESIAN_POINT('Ctrl Pts',(-4.37447604421791,-0.368207831146071,
1.86184817876984));
#45390=CARTESIAN_POINT('Ctrl Pts',(-4.16647286574876,-2.17936832407669,
1.92790299910937));
#45391=CARTESIAN_POINT('Ctrl Pts',(-1.65208468153467,-4.89189754332655,
2.04675435292359));
#45392=CARTESIAN_POINT('Ctrl Pts',(3.20433051897175,-4.04874042926377,2.20514395334771));
#45393=CARTESIAN_POINT('Ctrl Pts',(5.14059300557593,0.484092964878372,2.36353355377181));
#45394=CARTESIAN_POINT('Ctrl Pts',(2.392155064142,4.57576601695794,2.52192315419593));
#45395=CARTESIAN_POINT('Ctrl Pts',(-2.53628918908134,4.49747442552335,2.68031275462004));
#45396=CARTESIAN_POINT('Ctrl Pts',(-4.33547083524805,1.62595452236117,2.78920166718974));
#45397=CARTESIAN_POINT('Ctrl Pts',(-4.37879165497107,0.0917787298065273,
2.84529404628473));
#45398=CARTESIAN_POINT('Ctrl Pts',(-4.37836367713493,0.00160984593324717,
2.84858989190502));
#45399=CARTESIAN_POINT('Origin',(0.,0.,-1.84858989190501));
#45400=CARTESIAN_POINT('',(-4.37640441740291,0.00246357316762604,0.651410108094979));
#45401=CARTESIAN_POINT('',(-4.36535621882271,0.00145633068789036,0.848589891905021));
#45402=CARTESIAN_POINT('',(-4.372,-4.40683631492666E-13,-1.84858989190501));
#45403=CARTESIAN_POINT('Ctrl Pts',(-4.37640441740291,0.00246357316762608,
0.651410108094978));
#45404=CARTESIAN_POINT('Ctrl Pts',(-4.3669296163584,-1.27588513251927,0.698090609697727));
#45405=CARTESIAN_POINT('Ctrl Pts',(-3.10443214653608,-4.01442651751147,
0.79753455216069));
#45406=CARTESIAN_POINT('Ctrl Pts',(1.54404435335689,-4.92628156041988,0.949741935483869));
#45407=CARTESIAN_POINT('Ctrl Pts',(4.97150648183897,-1.38949747849925,1.10803225806451));
#45408=CARTESIAN_POINT('Ctrl Pts',(3.87423912778238,3.41166257284768,1.26632258064516));
#45409=CARTESIAN_POINT('Ctrl Pts',(-0.749980974679123,5.10752324154442,
1.42461290322581));
#45410=CARTESIAN_POINT('Ctrl Pts',(-3.94614385852298,2.71245661069425,1.55297541237574));
#45411=CARTESIAN_POINT('Ctrl Pts',(-4.36745231673392,0.631032051720065,
1.62857448066547));
#45412=CARTESIAN_POINT('Ctrl Pts',(-4.36544656918105,0.00153916655095176,
1.65141010809498));
#45413=CARTESIAN_POINT('Ctrl Pts',(-4.36535621882271,0.0014563306878905,
0.848589891905021));
#45414=CARTESIAN_POINT('Ctrl Pts',(-4.36284379533113,-0.820370961494963,
0.87840231125495));
#45415=CARTESIAN_POINT('Ctrl Pts',(-3.74556810328531,-3.1011139180804,0.961011264079584));
#45416=CARTESIAN_POINT('Ctrl Pts',(-0.0704529116473286,-5.16289724783097,
1.09641675037892));
#45417=CARTESIAN_POINT('Ctrl Pts',(4.29252819085395,-2.86947836000301,1.25480635080303));
#45418=CARTESIAN_POINT('Ctrl Pts',(4.74374945851672,2.03886099295457,1.41319595122714));
#45419=CARTESIAN_POINT('Ctrl Pts',(0.87187597225223,5.08919664880298,1.57158555165126));
#45420=CARTESIAN_POINT('Ctrl Pts',(-3.4039180408651,3.63453814591924,1.71671686521054));
#45421=CARTESIAN_POINT('Ctrl Pts',(-4.36148372635845,1.08235900094027,1.80905164529514));
#45422=CARTESIAN_POINT('Ctrl Pts',(-4.37121340809612,-0.00394090090135399,
1.84858989190502));
#45423=CARTESIAN_POINT('Origin',(0.,0.,19.5));
#45424=CARTESIAN_POINT('',(-4.87237116524908,0.00192128708900893,19.1338737912933));
#45425=CARTESIAN_POINT('Ctrl Pts',(-0.803308159453631,4.29756675351939,
19.628));
#45426=CARTESIAN_POINT('Ctrl Pts',(-0.673853669232168,4.32487002581643,
19.6249474412138));
#45427=CARTESIAN_POINT('Ctrl Pts',(-0.543485635434045,4.34604385579072,
19.621903094994));
#45428=CARTESIAN_POINT('Ctrl Pts',(-0.412569255997991,4.3612238307311,19.6188638308603));
#45429=CARTESIAN_POINT('Ctrl Pts',(-0.27984336996821,4.37661362101213,19.6157825584728));
#45430=CARTESIAN_POINT('Ctrl Pts',(-0.146553204834455,4.38584275860783,
19.6127065096298));
#45431=CARTESIAN_POINT('Ctrl Pts',(-0.0130667331008604,4.38900056457998,
19.6096324222416));
#45432=CARTESIAN_POINT('Ctrl Pts',(0.102479072721167,4.39173395943972,19.6069714941353));
#45433=CARTESIAN_POINT('Ctrl Pts',(0.218172435996331,4.38991749290017,19.6043120356729));
#45434=CARTESIAN_POINT('Ctrl Pts',(0.333776183320261,4.38357806344137,19.6016519311904));
#45435=CARTESIAN_POINT('Ctrl Pts',(0.379031782704649,4.38109635600062,19.6006105754768));
#45436=CARTESIAN_POINT('Ctrl Pts',(0.424273632554427,4.37792119522461,19.5995691207606));
#45437=CARTESIAN_POINT('Ctrl Pts',(0.469487373095433,4.37405300814147,19.5985274401165));
#45438=CARTESIAN_POINT('Ctrl Pts',(0.491900142232015,4.37213552060263,19.598011071696));
#45439=CARTESIAN_POINT('Ctrl Pts',(0.514298864495916,4.37004829843513,19.5974948121273));
#45440=CARTESIAN_POINT('Ctrl Pts',(0.536673783628106,4.36779258854753,19.5969788310225));
#45441=CARTESIAN_POINT('Ctrl Pts',(0.67587029099505,4.35375960205351,19.5937688633242));
#45442=CARTESIAN_POINT('Ctrl Pts',(0.814241659431173,4.33320254529649,19.5905674515573));
#45443=CARTESIAN_POINT('Ctrl Pts',(0.951373424482021,4.30622334317185,19.5873709472848));
#45444=CARTESIAN_POINT('Ctrl Pts',(1.08850518953287,4.2792441410472,19.5841744430122));
#45445=CARTESIAN_POINT('Ctrl Pts',(1.22439822554137,4.24584269855803,19.580982846234));
#45446=CARTESIAN_POINT('Ctrl Pts',(1.35863436321977,4.20606161338018,19.5777925085132));
#45447=CARTESIAN_POINT('Ctrl Pts',(1.44718365537814,4.1798198949077,19.57568799216));
#45448=CARTESIAN_POINT('Ctrl Pts',(1.53501187237287,4.15080088353343,19.573584023676));
#45449=CARTESIAN_POINT('Ctrl Pts',(1.62197697724057,4.11905814350536,19.5714795558027));
#45450=CARTESIAN_POINT('Ctrl Pts',(1.66029004733011,4.10507366288661,19.5705524181278));
#45451=CARTESIAN_POINT('Ctrl Pts',(1.69843554242665,4.09056039562537,19.5696251835263));
#45452=CARTESIAN_POINT('Ctrl Pts',(1.73640102301099,4.07552228846135,19.5686977624494));
#45453=CARTESIAN_POINT('Ctrl Pts',(1.75436952443725,4.06840497436797,19.5682588277464));
#45454=CARTESIAN_POINT('Ctrl Pts',(1.77228816141992,4.061173866115,19.5678200842298));
#45455=CARTESIAN_POINT('Ctrl Pts',(1.79015508413385,4.05383000141309,19.5673815385189));
#45456=CARTESIAN_POINT('Ctrl Pts',(1.91574464850677,4.00220875787305,19.5642989279495));
#45457=CARTESIAN_POINT('Ctrl Pts',(2.03879019285953,3.94501636210332,19.561225830935));
#45458=CARTESIAN_POINT('Ctrl Pts',(2.15887237555029,3.88249361470115,19.5581590360687));
#45459=CARTESIAN_POINT('Ctrl Pts',(2.27969637656572,3.81958462748645,19.5550732958053));
#45460=CARTESIAN_POINT('Ctrl Pts',(2.39752111769151,3.75127894449634,19.5519939357949));
#45461=CARTESIAN_POINT('Ctrl Pts',(2.51190593036526,3.67777150955579,19.5489176847461));
#45462=CARTESIAN_POINT('Ctrl Pts',(2.62522809247125,3.60494696874821,19.5458700124906));
#45463=CARTESIAN_POINT('Ctrl Pts',(2.73517470696147,3.52701649641376,19.5428253916997));
#45464=CARTESIAN_POINT('Ctrl Pts',(2.84129224832913,3.44412553804493,19.5397806414099));
#45465=CARTESIAN_POINT('Ctrl Pts',(2.91209516263097,3.38881968242346,19.5377491469835));
#45466=CARTESIAN_POINT('Ctrl Pts',(2.98119295340959,3.33130466078434,19.5357175949077));
#45467=CARTESIAN_POINT('Ctrl Pts',(3.04844206982076,3.27161381566964,19.5336850403595));
#45468=CARTESIAN_POINT('Ctrl Pts',(3.08425226424725,3.23982840519718,19.5326027038555));
#45469=CARTESIAN_POINT('Ctrl Pts',(3.1195381208217,3.20742589648737,19.5315200830935));
#45470=CARTESIAN_POINT('Ctrl Pts',(3.15427695670459,3.17441047942531,19.5304370354107));
#45471=CARTESIAN_POINT('Ctrl Pts',(3.16725486117647,3.16207641819842,19.5300324251523));
#45472=CARTESIAN_POINT('Ctrl Pts',(3.18015812731145,3.14965513440157,19.5296277011351));
#45473=CARTESIAN_POINT('Ctrl Pts',(3.19297991753168,3.13715232569191,19.5292230337074));
#45474=CARTESIAN_POINT('Ctrl Pts',(3.21028959746143,3.12027327734767,19.5286767243753));
#45475=CARTESIAN_POINT('Ctrl Pts',(3.22744427955767,3.10325207454711,19.5281307247594));
#45476=CARTESIAN_POINT('Ctrl Pts',(3.24444163127926,3.08608990264034,19.5275850170264));
#45477=CARTESIAN_POINT('Ctrl Pts',(3.33717764080849,2.99245464912803,19.5246076851246));
#45478=CARTESIAN_POINT('Ctrl Pts',(3.42523294755332,2.89462674101026,19.5216390416869));
#45479=CARTESIAN_POINT('Ctrl Pts',(3.50859096128539,2.79305369138356,19.5186761904996));
#45480=CARTESIAN_POINT('Ctrl Pts',(3.59397640033088,2.68901019215335,19.5156412771407));
#45481=CARTESIAN_POINT('Ctrl Pts',(3.67443362705331,2.58103662340854,19.5126124412155));
#45482=CARTESIAN_POINT('Ctrl Pts',(3.74990902226373,2.46957232453757,19.5095865700048));
#45483=CARTESIAN_POINT('Ctrl Pts',(3.82667993619766,2.35619476524857,19.5065087603736));
#45484=CARTESIAN_POINT('Ctrl Pts',(3.89829689144343,2.23920494837555,19.5034340181076));
#45485=CARTESIAN_POINT('Ctrl Pts',(3.96466142958627,2.11903192999767,19.5003590674328));
#45486=CARTESIAN_POINT('Ctrl Pts',(4.0309620923612,1.99897457724446,19.4972870763748));
#45487=CARTESIAN_POINT('Ctrl Pts',(4.09202070623594,1.87573937136613,19.4942148773091));
#45488=CARTESIAN_POINT('Ctrl Pts',(4.14769296331372,1.74973219296001,19.4911392039111));
#45489=CARTESIAN_POINT('Ctrl Pts',(4.15491534612853,1.73338523439156,19.4907401956463));
#45490=CARTESIAN_POINT('Ctrl Pts',(4.16204794028702,1.71698942368025,19.490341076027));
#45491=CARTESIAN_POINT('Ctrl Pts',(4.1690873140012,1.70055278577387,19.4899420115644));
#45492=CARTESIAN_POINT('Ctrl Pts',(4.2235955422653,1.57327839358026,19.4868519217777));
#45493=CARTESIAN_POINT('Ctrl Pts',(4.27240340036226,1.44383040880503,19.4837717143479));
#45494=CARTESIAN_POINT('Ctrl Pts',(4.31545919855678,1.31266698606642,19.4806981622917));
#45495=CARTESIAN_POINT('Ctrl Pts',(4.35892069590576,1.18026765801579,19.4775956492703));
#45496=CARTESIAN_POINT('Ctrl Pts',(4.39652153701043,1.04611964222381,19.4744999176358));
#45497=CARTESIAN_POINT('Ctrl Pts',(4.42816288898243,0.910666566444117,19.4714076483225));
#45498=CARTESIAN_POINT('Ctrl Pts',(4.45971763719553,0.775584231634271,19.4683238426851));
#45499=CARTESIAN_POINT('Ctrl Pts',(4.48534571134421,0.639203155572113,19.4652434804418));
#45500=CARTESIAN_POINT('Ctrl Pts',(4.50489988856683,0.501947997482608,19.4621632697058));
#45501=CARTESIAN_POINT('Ctrl Pts',(4.5234656283834,0.371630903362032,19.4592387594872));
#45502=CARTESIAN_POINT('Ctrl Pts',(4.53655584516878,0.240525160569636,19.456314385846));
#45503=CARTESIAN_POINT('Ctrl Pts',(4.5440002395032,0.108991400598333,19.453387331288));
#45504=CARTESIAN_POINT('Ctrl Pts',(4.54553145652646,0.0819365827912304,
19.4527852734757));
#45505=CARTESIAN_POINT('Ctrl Pts',(4.54682366211308,0.0548636663001908,
19.4521831022411));
#45506=CARTESIAN_POINT('Ctrl Pts',(4.54787513450369,0.0277758132908992,
19.4515807930663));
#45507=CARTESIAN_POINT('Ctrl Pts',(4.54880630338109,0.00378719894119923,
19.4510473966946));
#45508=CARTESIAN_POINT('Ctrl Pts',(4.54954867988174,-0.0202170615304457,
19.450513804788));
#45509=CARTESIAN_POINT('Ctrl Pts',(4.5501006277934,-0.0442070954676754,
19.4499806150988));
#45510=CARTESIAN_POINT('Ctrl Pts',(4.55331420062987,-0.183882814458235,
19.4468762571225));
#45511=CARTESIAN_POINT('Ctrl Pts',(4.55008558494902,-0.323251293541528,
19.443781616557));
#45512=CARTESIAN_POINT('Ctrl Pts',(4.54031186270851,-0.461877411739,19.4406934171861));
#45513=CARTESIAN_POINT('Ctrl Pts',(4.53067866021077,-0.598510460562132,
19.4376496177859));
#45514=CARTESIAN_POINT('Ctrl Pts',(4.51468731171393,-0.734423134579881,
19.4346120756979));
#45515=CARTESIAN_POINT('Ctrl Pts',(4.49218947310497,-0.869204596926774,
19.4315776539935));
#45516=CARTESIAN_POINT('Ctrl Pts',(4.48129191999887,-0.934490341445224,
19.430107834059));
#45517=CARTESIAN_POINT('Ctrl Pts',(4.46886701290829,-0.999510687886201,
19.4286387462481));
#45518=CARTESIAN_POINT('Ctrl Pts',(4.45489347098868,-1.06421861098155,19.4271700340528));
#45519=CARTESIAN_POINT('Ctrl Pts',(4.42601008140308,-1.19797025124501,19.4241341977007));
#45520=CARTESIAN_POINT('Ctrl Pts',(4.39051333916906,-1.33038812058978,19.421099966171));
#45521=CARTESIAN_POINT('Ctrl Pts',(4.34872071354063,-1.46115895479143,19.4180641910325));
#45522=CARTESIAN_POINT('Ctrl Pts',(4.32227027711835,-1.54392345173146,19.416142857398));
#45523=CARTESIAN_POINT('Ctrl Pts',(4.29329690956391,-1.62602796166861,19.4142209054574));
#45524=CARTESIAN_POINT('Ctrl Pts',(4.26187123440312,-1.70738903830258,19.4122975370436));
#45525=CARTESIAN_POINT('Ctrl Pts',(4.25321767430855,-1.72979310639049,19.4117679069221));
#45526=CARTESIAN_POINT('Ctrl Pts',(4.24437655206198,-1.75214443843245,19.4112380817814));
#45527=CARTESIAN_POINT('Ctrl Pts',(4.23535981723739,-1.7744158038722,19.4107086515302));
#45528=CARTESIAN_POINT('Ctrl Pts',(4.18439432237877,-1.90030074813356,19.4077161409069));
#45529=CARTESIAN_POINT('Ctrl Pts',(4.12776551664013,-2.02378469411099,19.4047326389142));
#45530=CARTESIAN_POINT('Ctrl Pts',(4.06584469055636,-2.14458841387499,19.4017552111055));
#45531=CARTESIAN_POINT('Ctrl Pts',(4.00036068062891,-2.2723436859638,19.3986064496223));
#45532=CARTESIAN_POINT('Ctrl Pts',(3.92895803265593,-2.39710220266129,19.3954644815049));
#45533=CARTESIAN_POINT('Ctrl Pts',(3.85201703329039,-2.51851897272141,19.392325836016));
#45534=CARTESIAN_POINT('Ctrl Pts',(3.77655716323104,-2.63759844617919,19.3892476100675));
#45535=CARTESIAN_POINT('Ctrl Pts',(3.69576939240684,-2.75346420580146,19.3861725800561));
#45536=CARTESIAN_POINT('Ctrl Pts',(3.60996439826952,-2.86576656284731,19.3830974718481));
#45537=CARTESIAN_POINT('Ctrl Pts',(3.54413699183306,-2.95192207133902,19.3807383271401));
#45538=CARTESIAN_POINT('Ctrl Pts',(3.47535563877055,-3.03597991726489,19.3783791364089));
#45539=CARTESIAN_POINT('Ctrl Pts',(3.40374469167589,-3.11776882943693,19.3760184212987));
#45540=CARTESIAN_POINT('Ctrl Pts',(3.38306291872267,-3.14139007423622,19.3753366292557));
#45541=CARTESIAN_POINT('Ctrl Pts',(3.36214505086869,-3.16482198260282,19.3746547100648));
#45542=CARTESIAN_POINT('Ctrl Pts',(3.34099389843024,-3.18806021076517,19.3739726281131));
#45543=CARTESIAN_POINT('Ctrl Pts',(3.32373515295353,-3.20702195132993,19.3734160684253));
#45544=CARTESIAN_POINT('Ctrl Pts',(3.30632108269655,-3.22585473586077,19.3728594003699));
#45545=CARTESIAN_POINT('Ctrl Pts',(3.28875317708965,-3.24455615157313,19.372302604599));
#45546=CARTESIAN_POINT('Ctrl Pts',(3.27637002727884,-3.25773828253526,19.3719101340564));
#45547=CARTESIAN_POINT('Ctrl Pts',(3.26391669904378,-3.27084847479794,19.3715177984306));
#45548=CARTESIAN_POINT('Ctrl Pts',(3.25139510554647,-3.28388487669204,19.3711256274074));
#45549=CARTESIAN_POINT('Ctrl Pts',(3.15282448543269,-3.38650809465787,19.3680384371903));
#45550=CARTESIAN_POINT('Ctrl Pts',(3.05000398947139,-3.48458548857025,19.3649607083322));
#45551=CARTESIAN_POINT('Ctrl Pts',(2.94328170324704,-3.57779502158214,19.3618892172301));
#45552=CARTESIAN_POINT('Ctrl Pts',(2.83673480189425,-3.67085137626031,19.3588227737435));
#45553=CARTESIAN_POINT('Ctrl Pts',(2.72629835158367,-3.75905650319765,19.3557625475278));
#45554=CARTESIAN_POINT('Ctrl Pts',(2.61227793614804,-3.84205888933313,19.3527053308466));
#45555=CARTESIAN_POINT('Ctrl Pts',(2.49975879118773,-3.92396840950061,19.3496883675631));
#45556=CARTESIAN_POINT('Ctrl Pts',(2.38374884571102,-4.0008118415243,19.3466743350847));
#45557=CARTESIAN_POINT('Ctrl Pts',(2.26451075890163,-4.07221233820177,19.3436601507197));
#45558=CARTESIAN_POINT('Ctrl Pts',(2.15307182587664,-4.13894265382576,19.3408431188587));
#45559=CARTESIAN_POINT('Ctrl Pts',(2.03881261846325,-4.20091883876065,19.3380259543306));
#45560=CARTESIAN_POINT('Ctrl Pts',(1.92192917555825,-4.2577952663979,19.3352061406412));
#45561=CARTESIAN_POINT('Ctrl Pts',(1.89885610409831,-4.26902280938128,19.334649502668));
#45562=CARTESIAN_POINT('Ctrl Pts',(1.87568072700257,-4.28005149894805,19.3340927614631));
#45563=CARTESIAN_POINT('Ctrl Pts',(1.85240449004643,-4.29087848232892,19.3335358976687));
#45564=CARTESIAN_POINT('Ctrl Pts',(1.83464431921192,-4.29913965765674,19.3331110009753));
#45565=CARTESIAN_POINT('Ctrl Pts',(1.81682357432143,-4.30728417370212,19.3326859893584));
#45566=CARTESIAN_POINT('Ctrl Pts',(1.79895912167073,-4.315303623104,19.3322612385723));
#45567=CARTESIAN_POINT('Ctrl Pts',(1.72163150021165,-4.35001641054753,19.3304226729781));
#45568=CARTESIAN_POINT('Ctrl Pts',(1.64342321773675,-4.38241577414544,19.3285875039126));
#45569=CARTESIAN_POINT('Ctrl Pts',(1.56440032675076,-4.41242911636972,19.3267550510791));
#45570=CARTESIAN_POINT('Ctrl Pts',(1.43711047143297,-4.46077452542352,19.3238033410982));
#45571=CARTESIAN_POINT('Ctrl Pts',(1.30770822291801,-4.50293181836922,19.3208586788369));
#45572=CARTESIAN_POINT('Ctrl Pts',(1.17662145504096,-4.53906398417229,19.3179182210069));
#45573=CARTESIAN_POINT('Ctrl Pts',(1.04250946942332,-4.57603000735673,19.3149099033514));
#45574=CARTESIAN_POINT('Ctrl Pts',(0.906633655370345,-4.60668969161992,
19.3119059864259));
#45575=CARTESIAN_POINT('Ctrl Pts',(0.769431097467203,-4.63116704578967,
19.308903425512));
#45576=CARTESIAN_POINT('Ctrl Pts',(0.630182204159468,-4.65600947242755,
19.3058560822937));
#45577=CARTESIAN_POINT('Ctrl Pts',(0.489565915681568,-4.67448381748104,
19.3028101358377));
#45578=CARTESIAN_POINT('Ctrl Pts',(0.348028745832047,-4.68666735853543,
19.2997624031501));
#45579=CARTESIAN_POINT('Ctrl Pts',(0.276401735269172,-4.69283302247179,
19.2982200522494));
#45580=CARTESIAN_POINT('Ctrl Pts',(0.204538794597775,-4.69738677129886,
19.2966772438915));
#45581=CARTESIAN_POINT('Ctrl Pts',(0.132497794988,-4.70033357743951,19.2951335655473));
#45582=CARTESIAN_POINT('Ctrl Pts',(0.112510249077041,-4.70115115941847,
19.2947052769069));
#45583=CARTESIAN_POINT('Ctrl Pts',(0.092508998863809,-4.70184502431764,
19.2942769212978));
#45584=CARTESIAN_POINT('Ctrl Pts',(0.0724952864131179,-4.70241523264229,
19.2938484899096));
#45585=CARTESIAN_POINT('Ctrl Pts',(0.0524053747538238,-4.70298761194961,
19.2934184273332));
#45586=CARTESIAN_POINT('Ctrl Pts',(0.0323102430098365,-4.70343515128597,
19.2929884454936));
#45587=CARTESIAN_POINT('Ctrl Pts',(0.0122186816347883,-4.70375813703399,
19.2925586960882));
#45588=CARTESIAN_POINT('Ctrl Pts',(-0.130279647047385,-4.70604889624492,
19.2895107213251));
#45589=CARTESIAN_POINT('Ctrl Pts',(-0.272714799094277,-4.70208198168319,
19.2864719199788));
#45590=CARTESIAN_POINT('Ctrl Pts',(-0.414633190928799,-4.69200784465072,
19.2834391901245));
#45591=CARTESIAN_POINT('Ctrl Pts',(-0.558078433367512,-4.68182532348272,
19.2803738321848));
#45592=CARTESIAN_POINT('Ctrl Pts',(-0.70099656213896,-4.66540343587715,
19.277314677082));
#45593=CARTESIAN_POINT('Ctrl Pts',(-0.842927293052888,-4.64284438111864,
19.2742585216926));
#45594=CARTESIAN_POINT('Ctrl Pts',(-0.984668741071393,-4.62031541176288,
19.2712064420796));
#45595=CARTESIAN_POINT('Ctrl Pts',(-1.12542627120009,-4.59166551790643,
19.2681573541844));
#45596=CARTESIAN_POINT('Ctrl Pts',(-1.26473685825812,-4.5569449834536,19.2651080676816));
#45597=CARTESIAN_POINT('Ctrl Pts',(-1.40219852797764,-4.52268525675062,
19.2620992510297));
#45598=CARTESIAN_POINT('Ctrl Pts',(-1.53825218997399,-4.48251476703442,
19.259090241007));
#45599=CARTESIAN_POINT('Ctrl Pts',(-1.6724364842164,-4.43643407027143,19.2560779726351));
#45600=CARTESIAN_POINT('Ctrl Pts',(-1.69577574030498,-4.42841905488856,
19.2555540357366));
#45601=CARTESIAN_POINT('Ctrl Pts',(-1.71905838453956,-4.42022512285657,
19.2550300002629));
#45602=CARTESIAN_POINT('Ctrl Pts',(-1.74228191014027,-4.41185213332152,
19.2545058500857));
#45603=CARTESIAN_POINT('Ctrl Pts',(-1.76035515482698,-4.40533602154642,
19.2540979406852));
#45604=CARTESIAN_POINT('Ctrl Pts',(-1.77838477372036,-4.39871426481839,
19.2536901381687));
#45605=CARTESIAN_POINT('Ctrl Pts',(-1.79636551936284,-4.3919886694264,19.2532825296376));
#45606=CARTESIAN_POINT('Ctrl Pts',(-1.93187451941972,-4.34130230054732,
19.2502106534458));
#45607=CARTESIAN_POINT('Ctrl Pts',(-2.06468449537211,-4.28469503542289,
19.2471480732848));
#45608=CARTESIAN_POINT('Ctrl Pts',(-2.19433977491624,-4.22226508755719,
19.2440916139197));
#45609=CARTESIAN_POINT('Ctrl Pts',(-2.32196725551768,-4.1608115394395,19.2410829573521));
#45610=CARTESIAN_POINT('Ctrl Pts',(-2.44653872111971,-4.09371577322205,
19.23808023162));
#45611=CARTESIAN_POINT('Ctrl Pts',(-2.56760656005401,-4.02102358517923,
19.235080408152));
#45612=CARTESIAN_POINT('Ctrl Pts',(-2.68526160349352,-3.95038052574101,
19.2321651470591));
#45613=CARTESIAN_POINT('Ctrl Pts',(-2.79960837675168,-3.87445182317372,
19.229252626912));
#45614=CARTESIAN_POINT('Ctrl Pts',(-2.91021369160128,-3.79323796763903,
19.2263400681055));
#45615=CARTESIAN_POINT('Ctrl Pts',(-2.98399388261748,-3.73906359290253,
19.2243972216394));
#45616=CARTESIAN_POINT('Ctrl Pts',(-3.05610871619606,-3.68253657740801,
19.2224543579711));
#45617=CARTESIAN_POINT('Ctrl Pts',(-3.12651483591522,-3.62376762555295,
19.2205106520618));
#45618=CARTESIAN_POINT('Ctrl Pts',(-3.16741234664924,-3.58962991353437,
19.2193815920652));
#45619=CARTESIAN_POINT('Ctrl Pts',(-3.20773318569702,-3.55473559432281,
19.2182522478782));
#45620=CARTESIAN_POINT('Ctrl Pts',(-3.24746784403176,-3.51910539807467,
19.217122457792));
#45621=CARTESIAN_POINT('Ctrl Pts',(-3.26700401396051,-3.50158725150764,
19.2165669787208));
#45622=CARTESIAN_POINT('Ctrl Pts',(-3.28639847163628,-3.48389120743249,
19.21601139186));
#45623=CARTESIAN_POINT('Ctrl Pts',(-3.30565001708697,-3.46601967389373,
19.2154556779901));
#45624=CARTESIAN_POINT('Ctrl Pts',(-3.31923733798883,-3.45340633530117,
19.2150634672609));
#45625=CARTESIAN_POINT('Ctrl Pts',(-3.33275239972697,-3.44070650564925,
19.2146712232022));
#45626=CARTESIAN_POINT('Ctrl Pts',(-3.34618584616149,-3.42792978435657,
19.2142792032619));
#45627=CARTESIAN_POINT('Ctrl Pts',(-3.44713342315095,-3.33191726347047,
19.2113333126973));
#45628=CARTESIAN_POINT('Ctrl Pts',(-3.54361479719668,-3.23143681477532,
19.2083960349772));
#45629=CARTESIAN_POINT('Ctrl Pts',(-3.63553433126932,-3.126940879262,19.2054645714511));
#45630=CARTESIAN_POINT('Ctrl Pts',(-3.73049026986206,-3.01899309932707,
19.2024362720435));
#45631=CARTESIAN_POINT('Ctrl Pts',(-3.82057851236323,-2.90675969406161,
19.1994141772984));
#45632=CARTESIAN_POINT('Ctrl Pts',(-3.90566064499467,-2.79069444962541,
19.1963952019566));
#45633=CARTESIAN_POINT('Ctrl Pts',(-3.99147592842286,-2.67362907362455,
19.1933502121733));
#45634=CARTESIAN_POINT('Ctrl Pts',(-4.07219888206677,-2.55266483623709,
19.1903083957846));
#45635=CARTESIAN_POINT('Ctrl Pts',(-4.14764752468129,-2.42823151976782,
19.1872665870857));
#45636=CARTESIAN_POINT('Ctrl Pts',(-4.20306739838779,-2.33683055555379,
19.1850322638681));
#45637=CARTESIAN_POINT('Ctrl Pts',(-4.25564073821494,-2.24355706942676,
19.1827979447995));
#45638=CARTESIAN_POINT('Ctrl Pts',(-4.30527982057198,-2.14857260904585,
19.1805623752584));
#45639=CARTESIAN_POINT('Ctrl Pts',(-4.32699691910319,-2.10701690762921,
19.1795843135842));
#45640=CARTESIAN_POINT('Ctrl Pts',(-4.3481522027174,-2.06513363702578,19.1786060125617));
#45641=CARTESIAN_POINT('Ctrl Pts',(-4.36873745807105,-2.02293601505909,
19.1776273671286));
#45642=CARTESIAN_POINT('Ctrl Pts',(-4.38086243818899,-1.99808107308335,
19.1770509323837));
#45643=CARTESIAN_POINT('Ctrl Pts',(-4.39278964467502,-1.97311706816874,
19.1764743781503));
#45644=CARTESIAN_POINT('Ctrl Pts',(-4.40451730909724,-1.9480466787424,19.175897682959));
#45645=CARTESIAN_POINT('Ctrl Pts',(-4.4127985002692,-1.93034386255322,19.1754904643556));
#45646=CARTESIAN_POINT('Ctrl Pts',(-4.42097601800018,-1.91259691029446,
19.1750833804788));
#45647=CARTESIAN_POINT('Ctrl Pts',(-4.42904852534276,-1.89480918199437,
19.1746764755087));
#45648=CARTESIAN_POINT('Ctrl Pts',(-4.48950921559979,-1.76158436280397,
19.1716288777402));
#45649=CARTESIAN_POINT('Ctrl Pts',(-4.54410184606152,-1.62603381239176,
19.1685903704127));
#45650=CARTESIAN_POINT('Ctrl Pts',(-4.59268280744846,-1.48860776987399,
19.1655578531078));
#45651=CARTESIAN_POINT('Ctrl Pts',(-4.64144650306992,-1.35066480793007,
19.1625139291796));
#45652=CARTESIAN_POINT('Ctrl Pts',(-4.68415360775462,-1.21083146528599,
19.1594760404209));
#45653=CARTESIAN_POINT('Ctrl Pts',(-4.72061445405524,-1.06953622768658,
19.1564410512956));
#45654=CARTESIAN_POINT('Ctrl Pts',(-4.75671346962216,-0.929643178041525,
19.1534361808442));
#45655=CARTESIAN_POINT('Ctrl Pts',(-4.78668986944038,-0.78831633896503,
19.1504341527609));
#45656=CARTESIAN_POINT('Ctrl Pts',(-4.81031125214298,-0.645956691618861,
19.1474319239356));
#45657=CARTESIAN_POINT('Ctrl Pts',(-4.82807965738957,-0.538871347096197,
19.1451735964244));
#45658=CARTESIAN_POINT('Ctrl Pts',(-4.84225125518576,-0.431201234879474,
19.1429151553273));
#45659=CARTESIAN_POINT('Ctrl Pts',(-4.85270728658022,-0.32311529964396,
19.1406553054137));
#45660=CARTESIAN_POINT('Ctrl Pts',(-4.85885127437678,-0.259603758599947,
19.1393274124716));
#45661=CARTESIAN_POINT('Ctrl Pts',(-4.86371203457958,-0.195948633814534,
19.1379990330984));
#45662=CARTESIAN_POINT('Ctrl Pts',(-4.86726251019289,-0.132184380886881,
19.136669904511));
#45663=CARTESIAN_POINT('Ctrl Pts',(-4.86838059639054,-0.112104273637358,
19.1362513464105));
#45664=CARTESIAN_POINT('Ctrl Pts',(-4.86936819801155,-0.0920224658990377,
19.1358329041084));
#45665=CARTESIAN_POINT('Ctrl Pts',(-4.87022464687506,-0.0719445408679467,
19.1354146627671));
#45666=CARTESIAN_POINT('Ctrl Pts',(-4.87127693233824,-0.0472755739962392,
19.1349007858712));
#45667=CARTESIAN_POINT('Ctrl Pts',(-4.87213135174695,-0.0226102934020704,
19.134387167001));
#45668=CARTESIAN_POINT('Ctrl Pts',(-4.8727870952798,0.00204924970852941,
19.1338737912933));
#45669=CARTESIAN_POINT('',(0.446113671359645,4.91412736825422,19.058));
#45670=CARTESIAN_POINT('Ctrl Pts',(0.44649414690178,4.91265885279919,19.058));
#45671=CARTESIAN_POINT('Ctrl Pts',(0.299727560449543,4.91447193481392,19.0691244126311));
#45672=CARTESIAN_POINT('Ctrl Pts',(0.153167317909177,4.91005959431981,19.0802626720314));
#45673=CARTESIAN_POINT('Ctrl Pts',(0.00725046426545532,4.89944030839442,
19.0914270753353));
#45674=CARTESIAN_POINT('Ctrl Pts',(-0.137909608980915,4.88887609813179,
19.10253357579));
#45675=CARTESIAN_POINT('Ctrl Pts',(-0.282433758712205,4.87216902002991,
19.1136659496671));
#45676=CARTESIAN_POINT('Ctrl Pts',(-0.425882683147369,4.84928678485378,
19.1248363037588));
#45677=CARTESIAN_POINT('Ctrl Pts',(-0.565675808016648,4.82698770403557,
19.1357219810862));
#45678=CARTESIAN_POINT('Ctrl Pts',(-0.704448457143253,4.79882393308609,
19.1466437274425));
#45679=CARTESIAN_POINT('Ctrl Pts',(-0.841774914873059,4.76472078486696,
19.1576127473831));
#45680=CARTESIAN_POINT('Ctrl Pts',(-0.940805834192305,4.74012781002693,
19.1655228919155));
#45681=CARTESIAN_POINT('Ctrl Pts',(-1.0390843184423,4.71244522520194,19.1734576204009));
#45682=CARTESIAN_POINT('Ctrl Pts',(-1.13644149966956,4.68163105513636,19.181421134727));
#45683=CARTESIAN_POINT('Ctrl Pts',(-1.16730557623662,4.6718623776514,19.1839457201022));
#45684=CARTESIAN_POINT('Ctrl Pts',(-1.198076992637,4.66177888532038,19.1864731984846));
#45685=CARTESIAN_POINT('Ctrl Pts',(-1.22875016771071,4.65137899873876,19.1890037037495));
#45686=CARTESIAN_POINT('Ctrl Pts',(-1.24841289336978,4.644712257645,19.190625858309));
#45687=CARTESIAN_POINT('Ctrl Pts',(-1.26802854233492,4.6379177328912,19.1922487049096));
#45688=CARTESIAN_POINT('Ctrl Pts',(-1.28758810772402,4.63099805128267,19.1938716419773));
#45689=CARTESIAN_POINT('Ctrl Pts',(-1.41973360557623,4.58424830235176,19.204836293928));
#45690=CARTESIAN_POINT('Ctrl Pts',(-1.54943066798541,4.53175252800649,19.2158141351685));
#45691=CARTESIAN_POINT('Ctrl Pts',(-1.67628513679076,4.47348474855613,19.2268170475339));
#45692=CARTESIAN_POINT('Ctrl Pts',(-1.77854477370016,4.42651405823497,19.2356866903145));
#45693=CARTESIAN_POINT('Ctrl Pts',(-1.87895707987582,4.37579165399884,19.2445726249588));
#45694=CARTESIAN_POINT('Ctrl Pts',(-1.97730366067652,4.32128226154577,19.2534810756009));
#45695=CARTESIAN_POINT('Ctrl Pts',(-2.10058309475894,4.25295363233385,19.2646479991967));
#45696=CARTESIAN_POINT('Ctrl Pts',(-2.22061803115919,4.17867506623871,19.275850302475));
#45697=CARTESIAN_POINT('Ctrl Pts',(-2.3371003873209,4.09882401061829,19.2871002449437));
#45698=CARTESIAN_POINT('Ctrl Pts',(-2.45349352336119,4.01903411722977,19.2983415704744));
#45699=CARTESIAN_POINT('Ctrl Pts',(-2.56634003134295,3.93367951832198,19.3096304622446));
#45700=CARTESIAN_POINT('Ctrl Pts',(-2.67529062823455,3.84310647943015,19.3209791516131));
#45701=CARTESIAN_POINT('Ctrl Pts',(-2.71693531724479,3.80848632915125,19.3253170134781));
#45702=CARTESIAN_POINT('Ctrl Pts',(-2.75801032451888,3.77310349110297,19.3296636119694));
#45703=CARTESIAN_POINT('Ctrl Pts',(-2.79849428295858,3.73697648238141,19.3340196301562));
#45704=CARTESIAN_POINT('Ctrl Pts',(-2.81294818526249,3.72407813264686,19.335574850143));
#45705=CARTESIAN_POINT('Ctrl Pts',(-2.82732736116309,3.71108427106867,19.3371313434063));
#45706=CARTESIAN_POINT('Ctrl Pts',(-2.84161861583708,3.69800711896962,19.3386877998622));
#45707=CARTESIAN_POINT('Ctrl Pts',(-2.94391515755751,3.60440110145739,19.34982888694));
#45708=CARTESIAN_POINT('Ctrl Pts',(-3.04186033803071,3.50639786607989,19.3609841912936));
#45709=CARTESIAN_POINT('Ctrl Pts',(-3.13519298587128,3.40438402939327,19.3721662582028));
#45710=CARTESIAN_POINT('Ctrl Pts',(-3.22998005288867,3.30078049302696,19.3835225772406));
#45711=CARTESIAN_POINT('Ctrl Pts',(-3.32001032606879,3.19303967930977,19.3949064994243));
#45712=CARTESIAN_POINT('Ctrl Pts',(-3.4049668301135,3.08153340439932,19.4063311657064));
#45713=CARTESIAN_POINT('Ctrl Pts',(-3.48992333415822,2.97002712948888,19.4177558319884));
#45714=CARTESIAN_POINT('Ctrl Pts',(-3.56980658085615,2.85475460919877,19.4292212423689));
#45715=CARTESIAN_POINT('Ctrl Pts',(-3.64424819284547,2.73606613269444,19.4407405378004));
#45716=CARTESIAN_POINT('Ctrl Pts',(-3.69362849951562,2.65733498741996,19.4483817793834));
#45717=CARTESIAN_POINT('Ctrl Pts',(-3.74061319511361,2.57710031760525,19.4560467316635));
#45718=CARTESIAN_POINT('Ctrl Pts',(-3.78513614038734,2.49546231597417,19.463739230308));
#45719=CARTESIAN_POINT('Ctrl Pts',(-3.80567440292713,2.4578030214146,19.4672877501953));
#45720=CARTESIAN_POINT('Ctrl Pts',(-3.82568866999261,2.41984508871949,19.470842131787));
#45721=CARTESIAN_POINT('Ctrl Pts',(-3.84517166765662,2.38159830576804,19.4744027515965));
#45722=CARTESIAN_POINT('Ctrl Pts',(-3.85722034167954,2.35794573298872,19.4766047098446));
#45723=CARTESIAN_POINT('Ctrl Pts',(-3.86906582550741,2.33418269113951,19.4788090538567));
#45724=CARTESIAN_POINT('Ctrl Pts',(-3.88070630194933,2.310311496771,19.4810158726822));
#45725=CARTESIAN_POINT('Ctrl Pts',(-3.8885082527386,2.29431198982011,19.4824949781091));
#45726=CARTESIAN_POINT('Ctrl Pts',(-3.8962165975453,2.27826690602767,19.4839749160027));
#45727=CARTESIAN_POINT('Ctrl Pts',(-3.90382674774023,2.26218599112426,19.4854548878754));
#45728=CARTESIAN_POINT('Ctrl Pts',(-3.96414789534232,2.13472211503535,19.4971857472531));
#45729=CARTESIAN_POINT('Ctrl Pts',(-4.01838481417725,2.00484470453858,19.5089339279855));
#45730=CARTESIAN_POINT('Ctrl Pts',(-4.06640211675339,1.87293521419554,19.5207141703003));
#45731=CARTESIAN_POINT('Ctrl Pts',(-4.11224826252183,1.74699016109889,19.5319617555951));
#45732=CARTESIAN_POINT('Ctrl Pts',(-4.15242432683241,1.61919178653392,19.5432385686204));
#45733=CARTESIAN_POINT('Ctrl Pts',(-4.18676153681696,1.4898597689249,19.554557439162));
#45734=CARTESIAN_POINT('Ctrl Pts',(-4.2207524598163,1.36183205048544,19.5657621601394));
#45735=CARTESIAN_POINT('Ctrl Pts',(-4.24902179998014,1.23230080216518,19.5770080946197));
#45736=CARTESIAN_POINT('Ctrl Pts',(-4.27135507448881,1.1015746586975,19.588307688129));
#45737=CARTESIAN_POINT('Ctrl Pts',(-4.29323252438759,0.973516650317833,
19.5993766556815));
#45738=CARTESIAN_POINT('Ctrl Pts',(-4.30941374767392,0.844311453337346,
19.6104971142425));
#45739=CARTESIAN_POINT('Ctrl Pts',(-4.31964759244882,0.714256825545012,
19.621680762742));
#45740=CARTESIAN_POINT('Ctrl Pts',(-4.32157304106312,0.689787673591424,
19.6237849123534));
#45741=CARTESIAN_POINT('Ctrl Pts',(-4.32328781702124,0.665288489028016,
19.6258912988008));
#45742=CARTESIAN_POINT('Ctrl Pts',(-4.32479004603219,0.640761311051878,
19.628));
#45743=CARTESIAN_POINT('',(-3.60367707498796,3.37571982724537,19.058));
#45744=CARTESIAN_POINT('Origin',(0.,0.,19.058));
#45745=CARTESIAN_POINT('Ctrl Pts',(-4.8727870952798,0.00204924970852941,
19.1338737912933));
#45746=CARTESIAN_POINT('Ctrl Pts',(-4.87617886814195,0.129598459003725,
19.1312184028586));
#45747=CARTESIAN_POINT('Ctrl Pts',(-4.87425769241846,0.256993603559053,
19.1285695196845));
#45748=CARTESIAN_POINT('Ctrl Pts',(-4.86689403436298,0.383955746440246,
19.1259250851319));
#45749=CARTESIAN_POINT('Ctrl Pts',(-4.85865401760772,0.526027822131655,
19.1229659329201));
#45750=CARTESIAN_POINT('Ctrl Pts',(-4.84360044272571,0.667558209996482,
19.1200123512114));
#45751=CARTESIAN_POINT('Ctrl Pts',(-4.82205180462592,0.808202442374607,
19.117061458221));
#45752=CARTESIAN_POINT('Ctrl Pts',(-4.80012826355871,0.951293601552751,
19.1140592256271));
#45753=CARTESIAN_POINT('Ctrl Pts',(-4.77148144982624,1.09346818380839,19.1110597761218));
#45754=CARTESIAN_POINT('Ctrl Pts',(-4.73639180273002,1.23435901743,19.1080600748768));
#45755=CARTESIAN_POINT('Ctrl Pts',(-4.71189105823817,1.33273362650888,19.1059655849107));
#45756=CARTESIAN_POINT('Ctrl Pts',(-4.68424808585656,1.43048229055225,19.1038709722142));
#45757=CARTESIAN_POINT('Ctrl Pts',(-4.6535439006576,1.52747603119476,19.1017752037047));
#45758=CARTESIAN_POINT('Ctrl Pts',(-4.64011081963306,1.56991079272586,19.1008583049818));
#45759=CARTESIAN_POINT('Ctrl Pts',(-4.62609165763282,1.61220100164168,19.099941185029));
#45760=CARTESIAN_POINT('Ctrl Pts',(-4.61149254035212,1.65433555918283,19.0990237573359));
#45761=CARTESIAN_POINT('Ctrl Pts',(-4.60425406248102,1.6752265525563,19.098568881885));
#45762=CARTESIAN_POINT('Ctrl Pts',(-4.59687300609065,1.69607927843875,19.0981139307812));
#45763=CARTESIAN_POINT('Ctrl Pts',(-4.58935008303519,1.71689236429986,19.0976588934799));
#45764=CARTESIAN_POINT('Ctrl Pts',(-4.58288926961042,1.73476699408821,19.0972680997573));
#45765=CARTESIAN_POINT('Ctrl Pts',(-4.57632388063936,1.75261206193917,19.0968772491973));
#45766=CARTESIAN_POINT('Ctrl Pts',(-4.56965942251531,1.77041363655401,19.0964866227106));
#45767=CARTESIAN_POINT('Ctrl Pts',(-4.51879838731399,1.90626962008207,19.0935054849917));
#45768=CARTESIAN_POINT('Ctrl Pts',(-4.4621015938381,2.03978869153619,19.090533120728));
#45769=CARTESIAN_POINT('Ctrl Pts',(-4.39988991481362,2.17062521779186,19.0875666304161));
#45770=CARTESIAN_POINT('Ctrl Pts',(-4.33631291127845,2.304333139242,19.0845350362203));
#45771=CARTESIAN_POINT('Ctrl Pts',(-4.26697605411688,2.4352402172723,19.08150957663));
#45772=CARTESIAN_POINT('Ctrl Pts',(-4.19216902199247,2.5629660482269,19.0784871570202));
#45773=CARTESIAN_POINT('Ctrl Pts',(-4.11721282278043,2.69094656767373,19.0754587106304));
#45774=CARTESIAN_POINT('Ctrl Pts',(-4.03676418963347,2.81573387820879,19.0724333163567));
#45775=CARTESIAN_POINT('Ctrl Pts',(-3.95106744680097,2.93692273562437,19.0694078610249));
#45776=CARTESIAN_POINT('Ctrl Pts',(-3.86644065662709,3.05659850939287,19.0664201795206));
#45777=CARTESIAN_POINT('Ctrl Pts',(-3.77669549591118,3.17276577294219,19.0634324384734));
#45778=CARTESIAN_POINT('Ctrl Pts',(-3.68202832948565,3.28500209019142,19.0604416398662));
#45779=CARTESIAN_POINT('Ctrl Pts',(-3.65627454507218,3.31553548447098,19.0596280063176));
#45780=CARTESIAN_POINT('Ctrl Pts',(-3.63015628737134,3.34577773744076,19.0588141464826));
#45781=CARTESIAN_POINT('Ctrl Pts',(-3.60367707498796,3.37571982724537,19.058));
#45782=CARTESIAN_POINT('',(-4.,-4.89858719658941E-16,20.));
#45783=CARTESIAN_POINT('',(-4.5,-5.51091059616309E-16,19.5));
#45784=CARTESIAN_POINT('Origin',(0.,0.,20.));
#45785=CARTESIAN_POINT('Ctrl Pts',(2.86929757049748,-4.02374147429196,-0.329089653438089));
#45786=CARTESIAN_POINT('Ctrl Pts',(3.53627793941073,-3.54812315628632,-0.302707933007981));
#45787=CARTESIAN_POINT('Ctrl Pts',(4.61815699384527,-2.26074102389229,-0.249944492147766));
#45788=CARTESIAN_POINT('Ctrl Pts',(5.34305681190694,1.0543831002385,-0.144417610427336));
#45789=CARTESIAN_POINT('Ctrl Pts',(2.97075510791326,5.02204979956487,-0.0125090082767979));
#45790=CARTESIAN_POINT('Ctrl Pts',(-2.60167993603097,5.22655530852652,0.145781314303847));
#45791=CARTESIAN_POINT('Ctrl Pts',(-5.79544439621568,0.666623916928201,
0.304071636884492));
#45792=CARTESIAN_POINT('Ctrl Pts',(-3.71916882578288,-4.49661457488776,
0.462361959465137));
#45793=CARTESIAN_POINT('Ctrl Pts',(1.74534931250902,-5.56854608224957,0.620652282045782));
#45794=CARTESIAN_POINT('Ctrl Pts',(5.61966720797076,-1.57065337116734,0.778942604626428));
#45795=CARTESIAN_POINT('Ctrl Pts',(4.37934349714106,3.85645847095449,0.937232927207072));
#45796=CARTESIAN_POINT('Ctrl Pts',(-0.84775983002377,5.77341716827827,1.09552324978772));
#45797=CARTESIAN_POINT('Ctrl Pts',(-5.30296447800194,2.43487893547456,1.25381357236836));
#45798=CARTESIAN_POINT('Ctrl Pts',(-4.93115623773879,-3.11998211803485,
1.41210389494901));
#45799=CARTESIAN_POINT('Ctrl Pts',(-0.0706136094443395,-5.83485842583339,
1.57039421752965));
#45800=CARTESIAN_POINT('Ctrl Pts',(4.85417638956518,-3.23842638421833,1.7286845401103));
#45801=CARTESIAN_POINT('Ctrl Pts',(5.36037735273058,2.3058335652194,1.88697486269095));
#45802=CARTESIAN_POINT('Ctrl Pts',(0.98718650613642,5.75117077753662,2.04526518527159));
#45803=CARTESIAN_POINT('Ctrl Pts',(-4.28460500301765,3.96139458246299,2.20355550785224));
#45804=CARTESIAN_POINT('Ctrl Pts',(-5.65625702821141,-1.43431356080714,
2.36184583043288));
#45805=CARTESIAN_POINT('Ctrl Pts',(-1.87919427403712,-5.52441175942303,
2.52013615301353));
#45806=CARTESIAN_POINT('Ctrl Pts',(3.60843955214569,-4.58581057252521,2.67842647559417));
#45807=CARTESIAN_POINT('Ctrl Pts',(5.81142420090129,0.527110130500736,2.83671679817481));
#45808=CARTESIAN_POINT('Ctrl Pts',(2.72445125981257,5.16021910144056,2.99500712075546));
#45809=CARTESIAN_POINT('Ctrl Pts',(-2.84250423844022,5.09614219820049,3.15329744333611));
#45810=CARTESIAN_POINT('Ctrl Pts',(-5.82201720884499,0.393206705834578,
3.31158776591675));
#45811=CARTESIAN_POINT('Ctrl Pts',(-3.50193025017819,-4.66765255027645,
3.4698780884974));
#45812=CARTESIAN_POINT('Ctrl Pts',(2.00585411337058,-5.47969388429905,3.62816841107804));
#45813=CARTESIAN_POINT('Ctrl Pts',(5.68777231250098,-1.30374151751568,3.78645873365868));
#45814=CARTESIAN_POINT('Ctrl Pts',(4.19228952744401,4.05896591843996,3.94474905623933));
#45815=CARTESIAN_POINT('Ctrl Pts',(-1.11930309959379,5.72692381468561,4.10303937881998));
#45816=CARTESIAN_POINT('Ctrl Pts',(-5.41202917540188,2.18184234468851,4.26132970140061));
#45817=CARTESIAN_POINT('Ctrl Pts',(-4.77835461070898,-3.34930187121133,
4.41962002398127));
#45818=CARTESIAN_POINT('Ctrl Pts',(0.204906485773977,-5.83168150213524,
4.57791034656191));
#45819=CARTESIAN_POINT('Ctrl Pts',(5.00164762657821,-3.00566412467992,4.73620066914256));
#45820=CARTESIAN_POINT('Ctrl Pts',(5.24554559701654,2.55631516056015,4.8944909917232));
#45821=CARTESIAN_POINT('Ctrl Pts',(0.714587714204218,5.79136082533626,5.05278131430385));
#45822=CARTESIAN_POINT('Ctrl Pts',(-4.46683698218372,3.75471213080312,5.21107163688449));
#45823=CARTESIAN_POINT('Ctrl Pts',(-5.58223988624457,-1.69973340938259,
5.36936195946513));
#45824=CARTESIAN_POINT('Ctrl Pts',(-1.61630467165047,-5.60696486692776,
5.52765228204579));
#45825=CARTESIAN_POINT('Ctrl Pts',(3.82090205882377,-4.41035183034713,5.68594260462642));
#45826=CARTESIAN_POINT('Ctrl Pts',(5.78006132540833,0.800866334091529,5.84423292720708));
#45827=CARTESIAN_POINT('Ctrl Pts',(2.47781181352747,5.28308095975332,6.00252324978771));
#45828=CARTESIAN_POINT('Ctrl Pts',(-3.07991218091209,4.95627246713037,6.16081357236837));
#45829=CARTESIAN_POINT('Ctrl Pts',(-5.83408858766023,0.117924390593317,
6.319103894949));
#45830=CARTESIAN_POINT('Ctrl Pts',(-3.27767689138409,-4.82776656501236,
6.47739421752966));
#45831=CARTESIAN_POINT('Ctrl Pts',(2.26230141403803,-5.37889283427418,6.63568454011029));
#45832=CARTESIAN_POINT('Ctrl Pts',(5.7429776032295,-1.03378143694346,6.79397486269095));
#45833=CARTESIAN_POINT('Ctrl Pts',(3.99600116469878,4.25234882180315,6.95226518527158));
#45834=CARTESIAN_POINT('Ctrl Pts',(-1.38840996925396,5.66769914231875,7.11055550785224));
#45835=CARTESIAN_POINT('Ctrl Pts',(-5.50899499668582,1.92392046016856,7.26884583043288));
#45836=CARTESIAN_POINT('Ctrl Pts',(-4.61491443420867,-3.57114275484712,
7.42713615301353));
#45837=CARTESIAN_POINT('Ctrl Pts',(0.47997818700567,-5.81550657729517,7.58542647559416));
#45838=CARTESIAN_POINT('Ctrl Pts',(5.13796169871233,-2.76619691871885,7.74371679817482));
#45839=CARTESIAN_POINT('Ctrl Pts',(5.1190196099595,2.80109515072493,7.90200712075546));
#45840=CARTESIAN_POINT('Ctrl Pts',(0.440394310825021,5.81863804180648,8.06029744333611));
#45841=CARTESIAN_POINT('Ctrl Pts',(-4.63910813519642,3.53965697780435,8.21858776591675));
#45842=CARTESIAN_POINT('Ctrl Pts',(-5.49577575427904,-1.96136296213705,
8.3768780884974));
#45843=CARTESIAN_POINT('Ctrl Pts',(-1.34981084575569,-5.67701563246438,
8.53516841107803));
#45844=CARTESIAN_POINT('Ctrl Pts',(4.02484459618971,-4.22505879096223,8.69345873365869));
#45845=CARTESIAN_POINT('Ctrl Pts',(5.73581007047566,1.07283672848883,8.85174905623933));
#45846=CARTESIAN_POINT('Ctrl Pts',(2.22564729760008,5.39416257794014,9.01003937881998));
#45847=CARTESIAN_POINT('Ctrl Pts',(-3.31045249741171,4.80535119142661,9.16832970140062));
#45848=CARTESIAN_POINT('Ctrl Pts',(-5.83315107572507,-0.157620868961595,
9.32662002398126));
#45849=CARTESIAN_POINT('Ctrl Pts',(-3.04611493876333,-4.97711558941596,
9.48491034656191));
#45850=CARTESIAN_POINT('Ctrl Pts',(2.51370421497615,-5.26609788459876,9.64320066914256));
#45851=CARTESIAN_POINT('Ctrl Pts',(5.78537715735888,-0.761516222857186,
9.8014909917232));
#45852=CARTESIAN_POINT('Ctrl Pts',(3.79080248595607,4.43624980394858,9.95978131430386));
#45853=CARTESIAN_POINT('Ctrl Pts',(-1.6544209509478,5.59583658871751,10.1180716368845));
#45854=CARTESIAN_POINT('Ctrl Pts',(-5.59367681682763,1.66170860244797,10.2763619594652));
#45855=CARTESIAN_POINT('Ctrl Pts',(-4.44118388437089,-3.78502067573863,
10.4346522820458));
#45856=CARTESIAN_POINT('Ctrl Pts',(0.753979628983335,-5.78636418916428,
10.5929426046264));
#45857=CARTESIAN_POINT('Ctrl Pts',(5.26281910261167,-2.52056162466824,10.7512329272071));
#45858=CARTESIAN_POINT('Ctrl Pts',(4.98107919185876,3.03962923643596,10.9095232497877));
#45859=CARTESIAN_POINT('Ctrl Pts',(0.165218912680596,5.83294081244249,11.0678135723684));
#45860=CARTESIAN_POINT('Ctrl Pts',(-4.80103496763896,3.31670906925412,11.226103894949));
#45861=CARTESIAN_POINT('Ctrl Pts',(-5.3970570974028,-2.21861905200931,11.3843942175297));
#45862=CARTESIAN_POINT('Ctrl Pts',(-1.08030720079852,-5.73440774295545,
11.5426845401103));
#45863=CARTESIAN_POINT('Ctrl Pts',(4.219812502755,-4.03034468155729,11.7009748626909));
#45864=CARTESIAN_POINT('Ctrl Pts',(5.67876906018774,1.34241490293389,11.8592651852716));
#45865=CARTESIAN_POINT('Ctrl Pts',(1.96852001545618,5.49321624909424,12.0175555078522));
#45866=CARTESIAN_POINT('Ctrl Pts',(-3.53361114034896,4.64371490504813,12.1758458304329));
#45867=CARTESIAN_POINT('Ctrl Pts',(-5.81920675667964,-0.432814664237157,
12.3341361530135));
#45868=CARTESIAN_POINT('Ctrl Pts',(-2.80776073459116,-5.11536660151085,
12.4924264755942));
#45869=CARTESIAN_POINT('Ctrl Pts',(2.75950193807008,-5.14156054757227,12.6507167981748));
#45870=CARTESIAN_POINT('Ctrl Pts',(5.81487643104491,-0.487552973782061,
12.8090071207555));
#45871=CARTESIAN_POINT('Ctrl Pts',(3.57715104538901,4.61025880065714,12.9672974433361));
#45872=CARTESIAN_POINT('Ctrl Pts',(-1.91674289151962,5.51149639375472,13.1255877659167));
#45873=CARTESIAN_POINT('Ctrl Pts',(-5.66588581148519,1.39579145354196,13.2838780884974));
#45874=CARTESIAN_POINT('Ctrl Pts',(-4.25755034704318,-3.99045872713326,
13.442168411078));
#45875=CARTESIAN_POINT('Ctrl Pts',(1.02629984112814,-5.74431931969763,13.6004587336587));
#45876=CARTESIAN_POINT('Ctrl Pts',(5.37594143021732,-2.26930596206795,13.7587490562393));
#45877=CARTESIAN_POINT('Ctrl Pts',(4.8320319233711,3.27138553246996,13.91703937882));
#45878=CARTESIAN_POINT('Ctrl Pts',(-0.110324891911251,5.8342372448088,14.0753297014006));
#45879=CARTESIAN_POINT('Ctrl Pts',(-4.95225641377798,3.0863655361992,14.2336200239813));
#45880=CARTESIAN_POINT('Ctrl Pts',(-5.28630403923151,-2.47092804732617,
14.3919103465619));
#45881=CARTESIAN_POINT('Ctrl Pts',(-0.808394678245584,-5.77901322496909,
14.5502006691425));
#45882=CARTESIAN_POINT('Ctrl Pts',(4.40537103766032,-3.82664367730009,14.7084909917232));
#45883=CARTESIAN_POINT('Ctrl Pts',(5.60906548477092,1.60899975000773,14.8667813143038));
#45884=CARTESIAN_POINT('Ctrl Pts',(1.70700331210297,5.58002110223998,15.0250716368845));
#45885=CARTESIAN_POINT('Ctrl Pts',(-3.74889050980069,4.47172402646598,15.1833619594651));
#45886=CARTESIAN_POINT('Ctrl Pts',(-5.7922867217461,-0.707043367010812,
15.3416522820458));
#45887=CARTESIAN_POINT('Ctrl Pts',(-2.56314576668009,-5.24221132595445,
15.4999426046264));
#45888=CARTESIAN_POINT('Ctrl Pts',(2.99914650864464,-5.00555852161226,15.658232927207));
#45889=CARTESIAN_POINT('Ctrl Pts',(5.83140963307135,-0.2125025674033,15.8165232497877));
#45890=CARTESIAN_POINT('Ctrl Pts',(3.35552327049972,4.77398779042229,15.9748135723683));
#45891=CARTESIAN_POINT('Ctrl Pts',(-2.17479091272675,5.41486664825819,16.133103894949));
#45892=CARTESIAN_POINT('Ctrl Pts',(-5.72546087416986,1.12676190338666,16.2913942175296));
#45893=CARTESIAN_POINT('Ctrl Pts',(-4.06442347000951,-4.18699871789581,
16.4496845401103));
#45894=CARTESIAN_POINT('Ctrl Pts',(1.29633194620277,-5.68946591914921,16.6079748626909));
#45895=CARTESIAN_POINT('Ctrl Pts',(5.47707578180272,-2.01298980380955,16.7662651852716));
#45896=CARTESIAN_POINT('Ctrl Pts',(4.67221141036031,3.49584654228241,16.9245555078522));
#45897=CARTESIAN_POINT('Ctrl Pts',(-0.385625099973721,5.82252583304098,
17.0828458304329));
#45898=CARTESIAN_POINT('Ctrl Pts',(-5.09243067800049,2.84913735309004,17.2411361530135));
#45899=CARTESIAN_POINT('Ctrl Pts',(-5.163772332666,-2.71772228672297,17.3994264755942));
#45900=CARTESIAN_POINT('Ctrl Pts',(-0.534662778757779,-5.81074229086598,
17.5577167981748));
#45901=CARTESIAN_POINT('Ctrl Pts',(4.58107430334251,-3.61439149963352,17.7160071207555));
#45902=CARTESIAN_POINT('Ctrl Pts',(5.52691620363093,1.87196148635973,17.8742974433361));
#45903=CARTESIAN_POINT('Ctrl Pts',(1.44156288337564,5.6544511543935,18.0325877659168));
#45904=CARTESIAN_POINT('Ctrl Pts',(-3.95558608138272,4.2896328856293,18.1908780884974));
#45905=CARTESIAN_POINT('Ctrl Pts',(-5.75288016701676,-0.979448557484372,
18.349168411078));
#45906=CARTESIAN_POINT('Ctrl Pts',(-2.31199479018177,-5.35783906812632,
18.5074587336587));
#45907=CARTESIAN_POINT('Ctrl Pts',(3.23053211221357,-4.8574916848313,18.6657490562393));
#45908=CARTESIAN_POINT('Ctrl Pts',(5.83796734686214,0.0612873527283092,
18.82403937882));
#45909=CARTESIAN_POINT('Ctrl Pts',(3.12041701848007,4.9304530959418,18.9823297014006));
#45910=CARTESIAN_POINT('Ctrl Pts',(-1.49215234175522,5.23769617354117,19.1142383035512));
#45911=CARTESIAN_POINT('Ctrl Pts',(-4.11442054260868,3.08380732139205,19.2197651852716));
#45912=CARTESIAN_POINT('Ctrl Pts',(-4.76857407193705,1.53464683800148,19.2725286261318));
#45913=CARTESIAN_POINT('Ctrl Pts',(-4.8886350428845,0.724300640260437,19.2989103465619));
#45914=CARTESIAN_POINT('Ctrl Pts',(2.75898463274061,-3.86904481704479,-0.21939310229206));
#45915=CARTESIAN_POINT('Ctrl Pts',(3.40032229220555,-3.4117121081895,-0.193011381861952));
#45916=CARTESIAN_POINT('Ctrl Pts',(4.44060745341011,-2.17382463487172,-0.140247941001737));
#45917=CARTESIAN_POINT('Ctrl Pts',(5.13763779242852,1.01384631572915,-0.0347210592813072));
#45918=CARTESIAN_POINT('Ctrl Pts',(2.85654153638278,4.82897220710893,0.0971875428692309));
#45919=CARTESIAN_POINT('Ctrl Pts',(-2.50165581870078,5.02561530273532,0.255477865449875));
#45920=CARTESIAN_POINT('Ctrl Pts',(-5.57263289575413,0.640994911623377,
0.413768188030522));
#45921=CARTESIAN_POINT('Ctrl Pts',(-3.5761817604452,-4.32373785104547,0.572058510611166));
#45922=CARTESIAN_POINT('Ctrl Pts',(1.67824765945831,-5.35445790830635,0.730348833191812));
#45923=CARTESIAN_POINT('Ctrl Pts',(5.4036136325935,-1.51026807361131,0.888639155772457));
#45924=CARTESIAN_POINT('Ctrl Pts',(4.2109753740215,3.70819317158555,1.0469294783531));
#45925=CARTESIAN_POINT('Ctrl Pts',(-0.815166878242221,5.55145252603366,
1.20521980093375));
#45926=CARTESIAN_POINT('Ctrl Pts',(-5.09908684732198,2.3412676449565,1.36351012351439));
#45927=CARTESIAN_POINT('Ctrl Pts',(-4.74157313673304,-3.0000313688591,1.52180044609504));
#45928=CARTESIAN_POINT('Ctrl Pts',(-0.0678988005016982,-5.6105316146419,
1.68009076867568));
#45929=CARTESIAN_POINT('Ctrl Pts',(4.66755285374621,-3.11392192994849,1.83838109125633));
#45930=CARTESIAN_POINT('Ctrl Pts',(5.15429242820228,2.21718354955942,1.99667141383697));
#45931=CARTESIAN_POINT('Ctrl Pts',(0.94923316008907,5.53006141943627,2.15496173641762));
#45932=CARTESIAN_POINT('Ctrl Pts',(-4.11987919351274,3.8090949121538,2.31325205899827));
#45933=CARTESIAN_POINT('Ctrl Pts',(-5.43879672158246,-1.37916997995865,
2.47154238157891));
#45934=CARTESIAN_POINT('Ctrl Pts',(-1.80694682117044,-5.31202037247638,
2.62983270415955));
#45935=CARTESIAN_POINT('Ctrl Pts',(3.46970958150474,-4.40950462174014,2.7881230267402));
#45936=CARTESIAN_POINT('Ctrl Pts',(5.58799834129561,0.506844868502552,2.94641334932084));
#45937=CARTESIAN_POINT('Ctrl Pts',(2.61970707944744,4.96182945569518,3.10470367190149));
#45938=CARTESIAN_POINT('Ctrl Pts',(-2.73322139641198,4.90021605136558,3.26299399448213));
#45939=CARTESIAN_POINT('Ctrl Pts',(-5.59818409073885,0.378089491324522,
3.42128431706278));
#45940=CARTESIAN_POINT('Ctrl Pts',(-3.3672951333158,-4.48820010500075,3.57957463964342));
#45941=CARTESIAN_POINT('Ctrl Pts',(1.92873709970399,-5.269021719585,3.73786496222407));
#45942=CARTESIAN_POINT('Ctrl Pts',(5.46910037009403,-1.25361790595597,3.89615528480471));
#45943=CARTESIAN_POINT('Ctrl Pts',(4.03111287624724,3.90291502315395,4.05444560738536));
#45944=CARTESIAN_POINT('Ctrl Pts',(-1.07627040252322,5.50674665467138,4.21273592996601));
#45945=CARTESIAN_POINT('Ctrl Pts',(-5.20395844627879,2.09795929218125,4.37102625254665));
#45946=CARTESIAN_POINT('Ctrl Pts',(-4.5946461169747,-3.22053470093006,4.5293165751273));
#45947=CARTESIAN_POINT('Ctrl Pts',(0.197028656494944,-5.60747683086738,
4.68760689770794));
#45948=CARTESIAN_POINT('Ctrl Pts',(4.80935441551997,-2.89010844202325,4.84589722028858));
#45949=CARTESIAN_POINT('Ctrl Pts',(5.04387549110129,2.45803513617603,5.00418754286923));
#45950=CARTESIAN_POINT('Ctrl Pts',(0.687114694030425,5.56870632173167,5.16247786544987));
#45951=CARTESIAN_POINT('Ctrl Pts',(-4.29510508687517,3.61035856850998,5.32076818803052));
#45952=CARTESIAN_POINT('Ctrl Pts',(-5.3676252406787,-1.63438550412508,5.47905851061116));
#45953=CARTESIAN_POINT('Ctrl Pts',(-1.55416426541541,-5.39139964541496,
5.63734883319181));
#45954=CARTESIAN_POINT('Ctrl Pts',(3.67400376032591,-4.24079156167736,5.79563915577246));
#45955=CARTESIAN_POINT('Ctrl Pts',(5.55784124207616,0.770076248402076,5.95392947835309));
#45956=CARTESIAN_POINT('Ctrl Pts',(2.38254992672651,5.07996777028487,6.11221980093375));
#45957=CARTESIAN_POINT('Ctrl Pts',(-2.9615019594687,4.76572374824029,6.27051012351439));
#45958=CARTESIAN_POINT('Ctrl Pts',(-5.60979137364659,0.113390672622288,
6.42880044609503));
#45959=CARTESIAN_POINT('Ctrl Pts',(-3.15166341316413,-4.64215838060276,
6.58709076867568));
#45960=CARTESIAN_POINT('Ctrl Pts',(2.17532503429963,-5.17209606403701,6.74538109125632));
#45961=CARTESIAN_POINT('Ctrl Pts',(5.52218323968972,-0.994036703430842,
6.90367141383697));
#45962=CARTESIAN_POINT('Ctrl Pts',(3.84237101065328,4.08886313257964,7.06196173641762));
#45963=CARTESIAN_POINT('Ctrl Pts',(-1.33503119666024,5.44979893247647,7.22025205899827));
#45964=CARTESIAN_POINT('Ctrl Pts',(-5.29719632218758,1.84995346554449,7.3785423815789));
#45965=CARTESIAN_POINT('Ctrl Pts',(-4.43748955713467,-3.43384669587891,
7.53683270415955));
#45966=CARTESIAN_POINT('Ctrl Pts',(0.461524958448211,-5.59192376675569,
7.6951230267402));
#45967=CARTESIAN_POINT('Ctrl Pts',(4.94042776047775,-2.65984778586643,7.85341334932084));
#45968=CARTESIAN_POINT('Ctrl Pts',(4.92221391876315,2.69340432137696,8.01170367190149));
#45969=CARTESIAN_POINT('Ctrl Pts',(0.42346292291388,5.59493483906605,8.16999399448214));
#45970=CARTESIAN_POINT('Ctrl Pts',(-4.46075310774047,3.40357142017932,8.32828431706278));
#45971=CARTESIAN_POINT('Ctrl Pts',(-5.28448530642128,-1.88595645408243,
8.48657463964342));
#45972=CARTESIAN_POINT('Ctrl Pts',(-1.29791605403297,-5.4587572410908,8.64486496222408));
#45973=CARTESIAN_POINT('Ctrl Pts',(3.87010552834755,-4.0626222935355,8.8031552848047));
#45974=CARTESIAN_POINT('Ctrl Pts',(5.51529126970868,1.03159047628066,8.96144560738537));
#45975=CARTESIAN_POINT('Ctrl Pts',(2.1400801210432,5.18677874754585,9.11973592996599));
#45976=CARTESIAN_POINT('Ctrl Pts',(-3.18317892911787,4.62060478787114,9.27802625254666));
#45977=CARTESIAN_POINT('Ctrl Pts',(-5.60888990527024,-0.151560981243543,
9.43631657512728));
#45978=CARTESIAN_POINT('Ctrl Pts',(-2.92900408518884,-4.78576553640322,
9.59460689770795));
#45979=CARTESIAN_POINT('Ctrl Pts',(2.41706240986782,-5.06363762598407,9.75289722028857));
#45980=CARTESIAN_POINT('Ctrl Pts',(5.56295270169353,-0.732238990493172,
9.91118754286925));
#45981=CARTESIAN_POINT('Ctrl Pts',(3.6450613948327,4.26569386247748,10.0694778654499));
#45982=CARTESIAN_POINT('Ctrl Pts',(-1.59081512725699,5.38069920469153,10.2277681880305));
#45983=CARTESIAN_POINT('Ctrl Pts',(-5.37862246733407,1.5978225979022,10.3860585106112));
#45984=CARTESIAN_POINT('Ctrl Pts',(-4.27043824737563,-3.63950187193647,
10.5443488331918));
#45985=CARTESIAN_POINT('Ctrl Pts',(0.724992148306133,-5.56390178610049,
10.7026391557725));
#45986=CARTESIAN_POINT('Ctrl Pts',(5.0604848999617,-2.42365617977001,10.8609294783531));
#45987=CARTESIAN_POINT('Ctrl Pts',(4.78957675429235,2.92276773199996,11.0192198009338));
#45988=CARTESIAN_POINT('Ctrl Pts',(0.158866910776627,5.60868772576421,11.1775101235144));
#45989=CARTESIAN_POINT('Ctrl Pts',(-4.61645450550797,3.18919496096631,11.335800446095));
#45990=CARTESIAN_POINT('Ctrl Pts',(-5.18956198439054,-2.13332208319472,
11.4940907686757));
#45991=CARTESIAN_POINT('Ctrl Pts',(-1.03877373901142,-5.51394285603487,
11.6523810912563));
#45992=CARTESIAN_POINT('Ctrl Pts',(4.05757770398459,-3.87539415757996,11.810671413837));
#45993=CARTESIAN_POINT('Ctrl Pts',(5.46044325657874,1.29080445543139,11.9689617364176));
#45994=CARTESIAN_POINT('Ctrl Pts',(1.89283834752078,5.28202420390446,12.1272520589983));
#45995=CARTESIAN_POINT('Ctrl Pts',(-3.39775802082929,4.4651827658415,12.2855423815789));
#45996=CARTESIAN_POINT('Ctrl Pts',(-5.59548168914238,-0.416174683216324,
12.4438327041595));
#45997=CARTESIAN_POINT('Ctrl Pts',(-2.69981364038388,-4.91870135377977,
12.6021230267402));
#45998=CARTESIAN_POINT('Ctrl Pts',(2.65341020026489,-4.94388824809053,12.7604133493208));
#45999=CARTESIAN_POINT('Ctrl Pts',(5.59131784709134,-0.468808525174477,
12.9187036719015));
#46000=CARTESIAN_POINT('Ctrl Pts',(3.43962399184309,4.43301291394634,13.0769939944821));
#46001=CARTESIAN_POINT('Ctrl Pts',(-1.84305184550816,5.29960155061157,13.2352843170628));
#46002=CARTESIAN_POINT('Ctrl Pts',(-5.44805531691171,1.34212889260043,13.3935746396434));
#46003=CARTESIAN_POINT('Ctrl Pts',(-4.0938646801192,-3.8370416574944,13.5518649622241));
#46004=CARTESIAN_POINT('Ctrl Pts',(0.986842744848443,-5.52347337256235,
13.7101552848047));
#46005=CARTESIAN_POINT('Ctrl Pts',(5.1692581295817,-2.18206028566305,13.8684456073854));
#46006=CARTESIAN_POINT('Ctrl Pts',(4.64625975310793,3.1456139316668,14.026735929966));
#46007=CARTESIAN_POINT('Ctrl Pts',(-0.106083344063608,5.60993431552639,
14.1850262525467));
#46008=CARTESIAN_POINT('Ctrl Pts',(-4.76186209596784,2.96770720923078,14.3433165751273));
#46009=CARTESIAN_POINT('Ctrl Pts',(-5.08306693533551,-2.37593081361676,
14.5016068977079));
#46010=CARTESIAN_POINT('Ctrl Pts',(-0.777315158037826,-5.55683343687841,
14.6598972202886));
#46011=CARTESIAN_POINT('Ctrl Pts',(4.23600226041317,-3.67952463669161,14.8181875428692));
#46012=CARTESIAN_POINT('Ctrl Pts',(5.39341950296062,1.54714018859507,14.9764778654499));
#46013=CARTESIAN_POINT('Ctrl Pts',(1.64137590835962,5.3654917599847,15.1347681880305));
#46014=CARTESIAN_POINT('Ctrl Pts',(-3.60476076539315,4.29980424398346,15.2930585106112));
#46015=CARTESIAN_POINT('Ctrl Pts',(-5.56959662115286,-0.679860396607744,
15.4513488331918));
#46016=CARTESIAN_POINT('Ctrl Pts',(-2.46460313299549,-5.04066940933542,
15.6096391557725));
#46017=CARTESIAN_POINT('Ctrl Pts',(2.88384140208001,-4.81311495238798,15.7679294783531));
#46018=CARTESIAN_POINT('Ctrl Pts',(5.60721541407427,-0.204332699372805,
15.9262198009337));
#46019=CARTESIAN_POINT('Ctrl Pts',(3.22651691246755,4.59044718334415,16.0845101235144));
#46020=CARTESIAN_POINT('Ctrl Pts',(-2.09117895938438,5.20668682972943,16.242800446095));
#46021=CARTESIAN_POINT('Ctrl Pts',(-5.50533995832764,1.08344244534466,16.4010907686757));
#46022=CARTESIAN_POINT('Ctrl Pts',(-3.90816275384159,-4.02602547702165,
16.5593810912563));
#46023=CARTESIAN_POINT('Ctrl Pts',(1.24649320282389,-5.47072886438628,16.717671413837));
#46024=CARTESIAN_POINT('Ctrl Pts',(5.26650427258732,-1.9355984515789,16.8759617364176));
#46025=CARTESIAN_POINT('Ctrl Pts',(4.49258369527158,3.36144531949132,17.0342520589983));
#46026=CARTESIAN_POINT('Ctrl Pts',(-0.370799367680139,5.59867316038258,
17.1925423815789));
#46027=CARTESIAN_POINT('Ctrl Pts',(-4.89664722417207,2.73959949451312,17.3508327041595));
#46028=CARTESIAN_POINT('Ctrl Pts',(-4.96524607948782,-2.61323680827755,
17.5091230267402));
#46029=CARTESIAN_POINT('Ctrl Pts',(-0.51410714784639,-5.58734264795531,
17.6674133493208));
#46030=CARTESIAN_POINT('Ctrl Pts',(4.40495044303595,-3.47543270057839,17.8257036719015));
#46031=CARTESIAN_POINT('Ctrl Pts',(5.31442853088914,1.79999210505495,17.9839939944821));
#46032=CARTESIAN_POINT('Ctrl Pts',(1.38614059526527,5.43706027634114,18.1422843170628));
#46033=CARTESIAN_POINT('Ctrl Pts',(-3.80350972455094,4.12471377428376,18.3005746396434));
#46034=CARTESIAN_POINT('Ctrl Pts',(-5.53170508977411,-0.941792704404255,
18.4588649622241));
#46035=CARTESIAN_POINT('Ctrl Pts',(-2.22310790023142,-5.15185173042014,
18.6171552848047));
#46036=CARTESIAN_POINT('Ctrl Pts',(3.1063311609144,-4.67074068925906,18.7754456073854));
#46037=CARTESIAN_POINT('Ctrl Pts',(5.61352101017582,0.0589311008023047,
18.933735929966));
#46038=CARTESIAN_POINT('Ctrl Pts',(3.00044954913339,4.74089702790683,19.0920262525466));
#46039=CARTESIAN_POINT('Ctrl Pts',(-1.43478509267926,5.03632784635119,19.2239348546972));
#46040=CARTESIAN_POINT('Ctrl Pts',(-3.95623764032305,2.96524734748178,19.3294617364176));
#46041=CARTESIAN_POINT('Ctrl Pts',(-4.58524160053518,1.47564584665783,19.3822251772778));
#46042=CARTESIAN_POINT('Ctrl Pts',(-4.70068671060039,0.696454197190917,
19.4086068977079));
#46043=CARTESIAN_POINT('Ctrl Pts',(2.64867169498374,-3.71434815979762,-0.109696551146031));
#46044=CARTESIAN_POINT('Ctrl Pts',(3.26436664500038,-3.27530106009269,-0.0833148307159233));
#46045=CARTESIAN_POINT('Ctrl Pts',(4.26305791297495,-2.08690824585116,-0.0305513898557082));
#46046=CARTESIAN_POINT('Ctrl Pts',(4.93221877295011,0.973309531219794,0.0749754918647217));
#46047=CARTESIAN_POINT('Ctrl Pts',(2.74232796485231,4.63589461465298,0.20688409401526));
#46048=CARTESIAN_POINT('Ctrl Pts',(-2.40163170137059,4.82467529694413,0.365174416595904));
#46049=CARTESIAN_POINT('Ctrl Pts',(-5.34982139529258,0.615365906318545,
0.52346473917655));
#46050=CARTESIAN_POINT('Ctrl Pts',(-3.43319469510752,-4.15086112720317,
0.681755061757195));
#46051=CARTESIAN_POINT('Ctrl Pts',(1.6111460064076,-5.14036973436311,0.84004538433784));
#46052=CARTESIAN_POINT('Ctrl Pts',(5.18756005721624,-1.44988277605528,0.998335706918485));
#46053=CARTESIAN_POINT('Ctrl Pts',(4.04260725090194,3.55992787221662,1.15662602949913));
#46054=CARTESIAN_POINT('Ctrl Pts',(-0.782573926460673,5.32948788378904,
1.31491635207978));
#46055=CARTESIAN_POINT('Ctrl Pts',(-4.89520921664203,2.24765635443844,1.47320667466042));
#46056=CARTESIAN_POINT('Ctrl Pts',(-4.55199003572729,-2.88008061968337,
1.63149699724107));
#46057=CARTESIAN_POINT('Ctrl Pts',(-0.065183991559061,-5.3862048034504,
1.78978731982171));
#46058=CARTESIAN_POINT('Ctrl Pts',(4.48092931792725,-2.98941747567865,1.94807764240236));
#46059=CARTESIAN_POINT('Ctrl Pts',(4.94820750367398,2.12853353389945,2.106367964983));
#46060=CARTESIAN_POINT('Ctrl Pts',(0.911279814041717,5.30895206133591,2.26465828756365));
#46061=CARTESIAN_POINT('Ctrl Pts',(-3.95515338400782,3.6567952418446,2.42294861014429));
#46062=CARTESIAN_POINT('Ctrl Pts',(-5.22133641495353,-1.32402639911015,
2.58123893272494));
#46063=CARTESIAN_POINT('Ctrl Pts',(-1.73469936830376,-5.09962898552972,
2.73952925530558));
#46064=CARTESIAN_POINT('Ctrl Pts',(3.33097961086378,-4.23319867095506,2.89781957788623));
#46065=CARTESIAN_POINT('Ctrl Pts',(5.36457248168994,0.486579606504366,3.05610990046687));
#46066=CARTESIAN_POINT('Ctrl Pts',(2.51496289908231,4.7634398099498,3.21440022304752));
#46067=CARTESIAN_POINT('Ctrl Pts',(-2.62393855438374,4.70428990453067,3.37269054562815));
#46068=CARTESIAN_POINT('Ctrl Pts',(-5.37435097263271,0.362972276814471,
3.53098086820881));
#46069=CARTESIAN_POINT('Ctrl Pts',(-3.23266001645341,-4.30874765972506,
3.68927119078945));
#46070=CARTESIAN_POINT('Ctrl Pts',(1.85162008603739,-5.05834955487095,3.8475615133701));
#46071=CARTESIAN_POINT('Ctrl Pts',(5.25042842768707,-1.20349429439626,4.00585183595074));
#46072=CARTESIAN_POINT('Ctrl Pts',(3.86993622505047,3.74686412786792,4.16414215853139));
#46073=CARTESIAN_POINT('Ctrl Pts',(-1.03323770545266,5.28656949465716,4.32243248111203));
#46074=CARTESIAN_POINT('Ctrl Pts',(-4.9958877171557,2.01407623967397,4.48072280369268));
#46075=CARTESIAN_POINT('Ctrl Pts',(-4.41093762324043,-3.09176753064878,
4.63901312627333));
#46076=CARTESIAN_POINT('Ctrl Pts',(0.18915082721592,-5.38327215959954,4.79730344885396));
#46077=CARTESIAN_POINT('Ctrl Pts',(4.61706120446174,-2.77455275936658,4.95559377143462));
#46078=CARTESIAN_POINT('Ctrl Pts',(4.84220538518603,2.3597551117919,5.11388409401526));
#46079=CARTESIAN_POINT('Ctrl Pts',(0.65964167385663,5.34605181812708,5.2721744165959));
#46080=CARTESIAN_POINT('Ctrl Pts',(-4.12337319156663,3.46600500621685,5.43046473917655));
#46081=CARTESIAN_POINT('Ctrl Pts',(-5.15301059511283,-1.56903759886758,
5.58875506175719));
#46082=CARTESIAN_POINT('Ctrl Pts',(-1.49202385918035,-5.17583442390216,
5.74704538433784));
#46083=CARTESIAN_POINT('Ctrl Pts',(3.52710546182805,-4.07123129300759,5.90533570691848));
#46084=CARTESIAN_POINT('Ctrl Pts',(5.33562115874398,0.739286162712621,6.06362602949913));
#46085=CARTESIAN_POINT('Ctrl Pts',(2.28728803992556,4.87685458081641,6.22191635207978));
#46086=CARTESIAN_POINT('Ctrl Pts',(-2.84309173802532,4.5751750293502,6.38020667466042));
#46087=CARTESIAN_POINT('Ctrl Pts',(-5.38549415963294,0.108856954651256,
6.53849699724107));
#46088=CARTESIAN_POINT('Ctrl Pts',(-3.02564993494416,-4.45655019619314,
6.6967873198217));
#46089=CARTESIAN_POINT('Ctrl Pts',(2.08834865456124,-4.96529929379983,6.85507764240235));
#46090=CARTESIAN_POINT('Ctrl Pts',(5.30138887614994,-0.954291969918219,
7.013367964983));
#46091=CARTESIAN_POINT('Ctrl Pts',(3.68874085660779,3.92537744335614,7.17165828756364));
#46092=CARTESIAN_POINT('Ctrl Pts',(-1.28165242406652,5.23189872263419,7.32994861014429));
#46093=CARTESIAN_POINT('Ctrl Pts',(-5.08539764768935,1.77598647092042,7.48823893272493));
#46094=CARTESIAN_POINT('Ctrl Pts',(-4.26006468006067,-3.2965506369107,7.64652925530558));
#46095=CARTESIAN_POINT('Ctrl Pts',(0.443071729890745,-5.36834095621621,
7.80481957788623));
#46096=CARTESIAN_POINT('Ctrl Pts',(4.74289382224317,-2.55349865301401,7.96310990046686));
#46097=CARTESIAN_POINT('Ctrl Pts',(4.7254082275668,2.58571349202899,8.12140022304752));
#46098=CARTESIAN_POINT('Ctrl Pts',(0.406531535002743,5.37123163632562,8.27969054562816));
#46099=CARTESIAN_POINT('Ctrl Pts',(-4.28239808028453,3.26748586255429,8.43798086820882));
#46100=CARTESIAN_POINT('Ctrl Pts',(-5.07319485856352,-1.81054994602781,
8.59627119078944));
#46101=CARTESIAN_POINT('Ctrl Pts',(-1.24602126231025,-5.24049884971722,
8.7545615133701));
#46102=CARTESIAN_POINT('Ctrl Pts',(3.71536646050538,-3.90018579610877,8.91285183595074));
#46103=CARTESIAN_POINT('Ctrl Pts',(5.29477246894171,0.99034422407249,9.07114215853139));
#46104=CARTESIAN_POINT('Ctrl Pts',(2.05451294448632,4.97939491715156,9.22943248111203));
#46105=CARTESIAN_POINT('Ctrl Pts',(-3.05590536082404,4.43585838431568,9.38772280369268));
#46106=CARTESIAN_POINT('Ctrl Pts',(-5.38462873481541,-0.145501093525492,
9.54601312627332));
#46107=CARTESIAN_POINT('Ctrl Pts',(-2.81189323161436,-4.59441548339048,
9.70430344885398));
#46108=CARTESIAN_POINT('Ctrl Pts',(2.32042060475949,-4.86117736736937,9.8625937714346));
#46109=CARTESIAN_POINT('Ctrl Pts',(5.34052824602817,-0.702961758129157,
10.0208840940153));
#46110=CARTESIAN_POINT('Ctrl Pts',(3.49932030370932,4.09513792100639,10.1791744165959));
#46111=CARTESIAN_POINT('Ctrl Pts',(-1.52720930356618,5.16556182066556,10.3374647391766));
#46112=CARTESIAN_POINT('Ctrl Pts',(-5.16356811784049,1.53393659335643,10.4957550617572));
#46113=CARTESIAN_POINT('Ctrl Pts',(-4.09969261038038,-3.49398306813431,
10.6540453843378));
#46114=CARTESIAN_POINT('Ctrl Pts',(0.69600466762893,-5.34143938303671,10.8123357069185));
#46115=CARTESIAN_POINT('Ctrl Pts',(4.85815069731172,-2.32675073487178,10.9706260294991));
#46116=CARTESIAN_POINT('Ctrl Pts',(4.59807431672593,2.80590622756395,11.1289163520798));
#46117=CARTESIAN_POINT('Ctrl Pts',(0.152514908872657,5.38443463908592,11.2872066746604));
#46118=CARTESIAN_POINT('Ctrl Pts',(-4.43187404337698,3.0616808526785,11.4454969972411));
#46119=CARTESIAN_POINT('Ctrl Pts',(-4.98206687137828,-2.04802511438014,
11.6037873198217));
#46120=CARTESIAN_POINT('Ctrl Pts',(-0.997240277224328,-5.29347796911429,
11.7620776424023));
#46121=CARTESIAN_POINT('Ctrl Pts',(3.89534290521418,-3.72044363360263,11.920367964983));
#46122=CARTESIAN_POINT('Ctrl Pts',(5.24211745296974,1.2391940079289,12.0786582875636));
#46123=CARTESIAN_POINT('Ctrl Pts',(1.81715667958537,5.07083215871469,12.2369486101443));
#46124=CARTESIAN_POINT('Ctrl Pts',(-3.26190490130962,4.28665062663486,12.3952389327249));
#46125=CARTESIAN_POINT('Ctrl Pts',(-5.37175662160512,-0.399534702195488,
12.5535292553056));
#46126=CARTESIAN_POINT('Ctrl Pts',(-2.59186654617659,-4.72203610604869,
12.7118195778862));
#46127=CARTESIAN_POINT('Ctrl Pts',(2.5473184624597,-4.74621594860878,12.8701099004669));
#46128=CARTESIAN_POINT('Ctrl Pts',(5.36775926313778,-0.450064076566892,
13.0284002230475));
#46129=CARTESIAN_POINT('Ctrl Pts',(3.30209693829715,4.25576702723554,13.1866905456282));
#46130=CARTESIAN_POINT('Ctrl Pts',(-1.76936079949669,5.08770670746843,13.3449808682088));
#46131=CARTESIAN_POINT('Ctrl Pts',(-5.23022482233823,1.28846633165889,13.5032711907894));
#46132=CARTESIAN_POINT('Ctrl Pts',(-3.93017901319522,-3.68362458785553,
13.6615615133701));
#46133=CARTESIAN_POINT('Ctrl Pts',(0.947385648568746,-5.30262742542707,
13.8198518359507));
#46134=CARTESIAN_POINT('Ctrl Pts',(4.96257482894607,-2.09481460925815,13.9781421585314));
#46135=CARTESIAN_POINT('Ctrl Pts',(4.46048758284477,3.01984233086364,14.136432481112));
#46136=CARTESIAN_POINT('Ctrl Pts',(-0.101841796215968,5.38563138624398,
14.2947228036927));
#46137=CARTESIAN_POINT('Ctrl Pts',(-4.57146777815769,2.84904888226236,14.4530131262733));
#46138=CARTESIAN_POINT('Ctrl Pts',(-4.87982983143951,-2.28093357990735,
14.611303448854));
#46139=CARTESIAN_POINT('Ctrl Pts',(-0.746235637830062,-5.33465364878775,
14.7695937714346));
#46140=CARTESIAN_POINT('Ctrl Pts',(4.06663348316603,-3.53240559608313,14.9278840940153));
#46141=CARTESIAN_POINT('Ctrl Pts',(5.17777352115031,1.48528062718241,15.0861744165959));
#46142=CARTESIAN_POINT('Ctrl Pts',(1.57574850461626,5.15096241772943,15.2444647391765));
#46143=CARTESIAN_POINT('Ctrl Pts',(-3.46063102098561,4.12788446150094,15.4027550617572));
#46144=CARTESIAN_POINT('Ctrl Pts',(-5.34690652055963,-0.652677426204677,
15.5610453843378));
#46145=CARTESIAN_POINT('Ctrl Pts',(-2.36606049931089,-4.83912749271637,
15.7193357069185));
#46146=CARTESIAN_POINT('Ctrl Pts',(2.76853629551539,-4.62067138316371,15.8776260294991));
#46147=CARTESIAN_POINT('Ctrl Pts',(5.3830211950772,-0.196162831342301,16.0359163520798));
#46148=CARTESIAN_POINT('Ctrl Pts',(3.09751055443537,4.406906576266,16.1942066746604));
#46149=CARTESIAN_POINT('Ctrl Pts',(-2.00756700604201,4.99850701120068,16.3524969972411));
#46150=CARTESIAN_POINT('Ctrl Pts',(-5.28521904248542,1.04012298730266,16.5107873198217));
#46151=CARTESIAN_POINT('Ctrl Pts',(-3.75190203767367,-3.86505223614748,
16.6690776424023));
#46152=CARTESIAN_POINT('Ctrl Pts',(1.19665445944501,-5.25199180962336,16.827367964983));
#46153=CARTESIAN_POINT('Ctrl Pts',(5.05593276337192,-1.85820709934824,16.9856582875636));
#46154=CARTESIAN_POINT('Ctrl Pts',(4.31295598018285,3.22704409670023,17.1439486101443));
#46155=CARTESIAN_POINT('Ctrl Pts',(-0.355973635386551,5.37482048772419,
17.3022389327249));
#46156=CARTESIAN_POINT('Ctrl Pts',(-4.70086377034365,2.63006163593618,17.4605292553056));
#46157=CARTESIAN_POINT('Ctrl Pts',(-4.76671982630963,-2.50875132983212,
17.6188195778862));
#46158=CARTESIAN_POINT('Ctrl Pts',(-0.493551516935001,-5.36394300504465,
17.7771099004669));
#46159=CARTESIAN_POINT('Ctrl Pts',(4.22882658272939,-3.33647390152326,17.9354002230475));
#46160=CARTESIAN_POINT('Ctrl Pts',(5.10194085814736,1.72802272375016,18.0936905456282));
#46161=CARTESIAN_POINT('Ctrl Pts',(1.3307183071549,5.21966939828879,18.2519808682088));
#46162=CARTESIAN_POINT('Ctrl Pts',(-3.65143336771916,3.95979466293823,18.4102711907895));
#46163=CARTESIAN_POINT('Ctrl Pts',(-5.31053001253145,-0.904136851324141,
18.5685615133701));
#46164=CARTESIAN_POINT('Ctrl Pts',(-2.13422101028107,-4.94586439271395,
18.7268518359507));
#46165=CARTESIAN_POINT('Ctrl Pts',(2.98213020961523,-4.48398969368682,18.8851421585314));
#46166=CARTESIAN_POINT('Ctrl Pts',(5.3890746734895,0.056574848876316,19.043432481112));
#46167=CARTESIAN_POINT('Ctrl Pts',(2.88048207978671,4.55134095987183,19.2017228036927));
#46168=CARTESIAN_POINT('Ctrl Pts',(-1.3774178436033,4.83495951916122,19.3336314058432));
#46169=CARTESIAN_POINT('Ctrl Pts',(-3.79805473803742,2.8466873735715,19.4391582875636));
#46170=CARTESIAN_POINT('Ctrl Pts',(-4.40190912913332,1.41664485531417,19.4919217284239));
#46171=CARTESIAN_POINT('Ctrl Pts',(-4.51273837831629,0.668607754121397,
19.518303448854));
#46172=CARTESIAN_POINT('Ctrl Pts',(2.53835875722687,-3.55965150255045,-1.94289029309402E-15));
#46173=CARTESIAN_POINT('Ctrl Pts',(3.1284109977952,-3.13889001199587,0.0263817204301056));
#46174=CARTESIAN_POINT('Ctrl Pts',(4.08550837253979,-1.9999918568306,0.0791451612903207));
#46175=CARTESIAN_POINT('Ctrl Pts',(4.72679975347169,0.932772746710439,0.184672043010751));
#46176=CARTESIAN_POINT('Ctrl Pts',(2.62811439332184,4.44281702219704,0.316580645161289));
#46177=CARTESIAN_POINT('Ctrl Pts',(-2.3016075840404,4.62373529115294,0.474870967741933));
#46178=CARTESIAN_POINT('Ctrl Pts',(-5.12700989483103,0.589736901013719,
0.633161290322578));
#46179=CARTESIAN_POINT('Ctrl Pts',(-3.29020762976984,-3.97798440336088,
0.791451612903224));
#46180=CARTESIAN_POINT('Ctrl Pts',(1.54404435335689,-4.92628156041988,0.949741935483869));
#46181=CARTESIAN_POINT('Ctrl Pts',(4.97150648183897,-1.38949747849925,1.10803225806451));
#46182=CARTESIAN_POINT('Ctrl Pts',(3.87423912778238,3.41166257284768,1.26632258064516));
#46183=CARTESIAN_POINT('Ctrl Pts',(-0.749980974679123,5.10752324154442,
1.42461290322581));
#46184=CARTESIAN_POINT('Ctrl Pts',(-4.69133158596208,2.15404506392038,1.58290322580645));
#46185=CARTESIAN_POINT('Ctrl Pts',(-4.36240693472153,-2.76012987050762,
1.7411935483871));
#46186=CARTESIAN_POINT('Ctrl Pts',(-0.0624691826164238,-5.16187799225891,
1.89948387096774));
#46187=CARTESIAN_POINT('Ctrl Pts',(4.29430578210828,-2.8649130214088,2.05777419354839));
#46188=CARTESIAN_POINT('Ctrl Pts',(4.74212257914569,2.03988351823947,2.21606451612903));
#46189=CARTESIAN_POINT('Ctrl Pts',(0.873326467994359,5.08784270323556,2.37435483870968));
#46190=CARTESIAN_POINT('Ctrl Pts',(-3.7904275745029,3.50449557153541,2.53264516129032));
#46191=CARTESIAN_POINT('Ctrl Pts',(-5.00387610832461,-1.26888281826166,
2.69093548387097));
#46192=CARTESIAN_POINT('Ctrl Pts',(-1.66245191543707,-4.88723759858308,
2.84922580645161));
#46193=CARTESIAN_POINT('Ctrl Pts',(3.19224964022283,-4.05689272016998,3.00751612903226));
#46194=CARTESIAN_POINT('Ctrl Pts',(5.14114662208426,0.466314344506177,3.1658064516129));
#46195=CARTESIAN_POINT('Ctrl Pts',(2.41021871871718,4.56505016420442,3.32409677419355));
#46196=CARTESIAN_POINT('Ctrl Pts',(-2.5146557123555,4.50836375769575,3.48238709677419));
#46197=CARTESIAN_POINT('Ctrl Pts',(-5.15051785452657,0.347855062304423,
3.64067741935484));
#46198=CARTESIAN_POINT('Ctrl Pts',(-3.09802489959102,-4.12929521444937,
3.79896774193548));
#46199=CARTESIAN_POINT('Ctrl Pts',(1.77450307237079,-4.84767739015689,3.95725806451612));
#46200=CARTESIAN_POINT('Ctrl Pts',(5.03175648528012,-1.15337068283656,4.11554838709677));
#46201=CARTESIAN_POINT('Ctrl Pts',(3.7087595738537,3.5908132325819,4.27383870967742));
#46202=CARTESIAN_POINT('Ctrl Pts',(-0.990205008382098,5.06639233464293,
4.43212903225806));
#46203=CARTESIAN_POINT('Ctrl Pts',(-4.7878169880326,1.93019318716672,4.59041935483871));
#46204=CARTESIAN_POINT('Ctrl Pts',(-4.22722912950617,-2.96300036036751,
4.74870967741935));
#46205=CARTESIAN_POINT('Ctrl Pts',(0.181272997936893,-5.15906748833169,
4.907));
#46206=CARTESIAN_POINT('Ctrl Pts',(4.4247679934035,-2.65899707670991,5.06529032258064));
#46207=CARTESIAN_POINT('Ctrl Pts',(4.64053527927078,2.26147508740778,5.22358064516129));
#46208=CARTESIAN_POINT('Ctrl Pts',(0.63216865368283,5.12339731452249,5.38187096774192));
#46209=CARTESIAN_POINT('Ctrl Pts',(-3.95164129625807,3.32165144392371,5.54016129032259));
#46210=CARTESIAN_POINT('Ctrl Pts',(-4.93839594954698,-1.50368969361007,
5.69845161290321));
#46211=CARTESIAN_POINT('Ctrl Pts',(-1.42988345294528,-4.96026920238937,
5.85674193548387));
#46212=CARTESIAN_POINT('Ctrl Pts',(3.38020716333018,-3.90167102433782,6.01503225806451));
#46213=CARTESIAN_POINT('Ctrl Pts',(5.11340107541181,0.708496077023162,6.17332258064516));
#46214=CARTESIAN_POINT('Ctrl Pts',(2.19202615312461,4.67374139134797,6.3316129032258));
#46215=CARTESIAN_POINT('Ctrl Pts',(-2.72468151658193,4.38462631046011,6.48990322580645));
#46216=CARTESIAN_POINT('Ctrl Pts',(-5.16119694561929,0.104323236680228,
6.64819354838708));
#46217=CARTESIAN_POINT('Ctrl Pts',(-2.8996364567242,-4.27094201178353,6.80648387096775));
#46218=CARTESIAN_POINT('Ctrl Pts',(2.00137227482285,-4.75850252356265,6.96477419354837));
#46219=CARTESIAN_POINT('Ctrl Pts',(5.08059451261016,-0.914547236405604,
7.12306451612904));
#46220=CARTESIAN_POINT('Ctrl Pts',(3.53511070256229,3.76189175413264,7.28135483870967));
#46221=CARTESIAN_POINT('Ctrl Pts',(-1.22827365147281,5.01399851279189,7.43964516129032));
#46222=CARTESIAN_POINT('Ctrl Pts',(-4.87359897319111,1.70201947629637,7.59793548387097));
#46223=CARTESIAN_POINT('Ctrl Pts',(-4.08263980298667,-3.1592545779425,7.75622580645161));
#46224=CARTESIAN_POINT('Ctrl Pts',(0.424618501333285,-5.14475814567673,
7.91451612903225));
#46225=CARTESIAN_POINT('Ctrl Pts',(4.54535988400859,-2.44714952016159,8.0728064516129));
#46226=CARTESIAN_POINT('Ctrl Pts',(4.52860253637045,2.47802266268103,8.23109677419354));
#46227=CARTESIAN_POINT('Ctrl Pts',(0.389600147091602,5.14752843358518,8.38938709677419));
#46228=CARTESIAN_POINT('Ctrl Pts',(-4.10404305282859,3.13140030492926,8.54767741935484));
#46229=CARTESIAN_POINT('Ctrl Pts',(-4.86190441070575,-1.73514343797319,
8.70596774193548));
#46230=CARTESIAN_POINT('Ctrl Pts',(-1.19412647058753,-5.02224045834365,
8.86425806451613));
#46231=CARTESIAN_POINT('Ctrl Pts',(3.56062739266322,-3.73774929868204,9.02254838709676));
#46232=CARTESIAN_POINT('Ctrl Pts',(5.07425366817473,0.949097971864315,9.18083870967742));
#46233=CARTESIAN_POINT('Ctrl Pts',(1.96894576792944,4.77201108675727,9.33912903225805));
#46234=CARTESIAN_POINT('Ctrl Pts',(-2.9286317925302,4.25111198076021,9.4974193548387));
#46235=CARTESIAN_POINT('Ctrl Pts',(-5.16036756436058,-0.139441205807441,
9.65570967741936));
#46236=CARTESIAN_POINT('Ctrl Pts',(-2.69478237803987,-4.40306543037773,
9.81399999999999));
#46237=CARTESIAN_POINT('Ctrl Pts',(2.22377879965116,-4.65871710875468,9.97229032258064));
#46238=CARTESIAN_POINT('Ctrl Pts',(5.11810379036282,-0.67368452576514,10.1305806451613));
#46239=CARTESIAN_POINT('Ctrl Pts',(3.35357921258595,3.92458197953528,10.2888709677419));
#46240=CARTESIAN_POINT('Ctrl Pts',(-1.46360347987537,4.95042443663959,10.4471612903226));
#46241=CARTESIAN_POINT('Ctrl Pts',(-4.94851376834693,1.47005058881065,10.6054516129032));
#46242=CARTESIAN_POINT('Ctrl Pts',(-3.92894697338513,-3.34846426433215,
10.7637419354839));
#46243=CARTESIAN_POINT('Ctrl Pts',(0.667017186951725,-5.11897697997292,
10.9220322580645));
#46244=CARTESIAN_POINT('Ctrl Pts',(4.65581649466175,-2.22984528997355,11.0803225806452));
#46245=CARTESIAN_POINT('Ctrl Pts',(4.40657187915952,2.68904472312794,11.2386129032258));
#46246=CARTESIAN_POINT('Ctrl Pts',(0.14616290696869,5.16018155240764,11.3969032258064));
#46247=CARTESIAN_POINT('Ctrl Pts',(-4.24729358124599,2.93416674439068,11.5551935483871));
#46248=CARTESIAN_POINT('Ctrl Pts',(-4.77457175836603,-1.96272814556555,
11.7134838709677));
#46249=CARTESIAN_POINT('Ctrl Pts',(-0.955706815437237,-5.07301308219371,
11.8717741935484));
#46250=CARTESIAN_POINT('Ctrl Pts',(3.73310810644377,-3.5654931096253,12.030064516129));
#46251=CARTESIAN_POINT('Ctrl Pts',(5.02379164936073,1.1875835604264,12.1883548387097));
#46252=CARTESIAN_POINT('Ctrl Pts',(1.74147501164997,4.85964011352491,12.3466451612903));
#46253=CARTESIAN_POINT('Ctrl Pts',(-3.12605178178994,4.10811848742822,12.504935483871));
#46254=CARTESIAN_POINT('Ctrl Pts',(-5.14803155406786,-0.382894721174656,
12.6632258064516));
#46255=CARTESIAN_POINT('Ctrl Pts',(-2.4839194519693,-4.5253708583176,12.8215161290323));
#46256=CARTESIAN_POINT('Ctrl Pts',(2.44122672465452,-4.54854364912704,12.9798064516129));
#46257=CARTESIAN_POINT('Ctrl Pts',(5.14420067918421,-0.431319627959304,
13.1380967741936));
#46258=CARTESIAN_POINT('Ctrl Pts',(3.16456988475122,4.07852114052473,13.2963870967742));
#46259=CARTESIAN_POINT('Ctrl Pts',(-1.69566975348524,4.87581186432528,13.4546774193548));
#46260=CARTESIAN_POINT('Ctrl Pts',(-5.01239432776474,1.23480377071736,13.6129677419355));
#46261=CARTESIAN_POINT('Ctrl Pts',(-3.76649334627126,-3.53020751821668,
13.7712580645161));
#46262=CARTESIAN_POINT('Ctrl Pts',(0.907928552289056,-5.08178147829179,
13.9295483870968));
#46263=CARTESIAN_POINT('Ctrl Pts',(4.75589152831045,-2.00756893285326,14.0878387096774));
#46264=CARTESIAN_POINT('Ctrl Pts',(4.2747154125816,2.89407073006048,14.2461290322581));
#46265=CARTESIAN_POINT('Ctrl Pts',(-0.0976002483683332,5.16132845696157,
14.4044193548387));
#46266=CARTESIAN_POINT('Ctrl Pts',(-4.38107346034753,2.73039055529394,14.5627096774194));
#46267=CARTESIAN_POINT('Ctrl Pts',(-4.67659272754351,-2.18593634619795,
14.721));
#46268=CARTESIAN_POINT('Ctrl Pts',(-0.715156117622299,-5.11247386069707,
14.8792903225806));
#46269=CARTESIAN_POINT('Ctrl Pts',(3.89726470591888,-3.38528655547465,15.0375806451613));
#46270=CARTESIAN_POINT('Ctrl Pts',(4.96212753934002,1.42342106576975,15.1958709677419));
#46271=CARTESIAN_POINT('Ctrl Pts',(1.5101211008729,4.93643307547415,15.3541612903226));
#46272=CARTESIAN_POINT('Ctrl Pts',(-3.31650127657807,3.95596467901843,15.5124516129032));
#46273=CARTESIAN_POINT('Ctrl Pts',(-5.1242164199664,-0.62549445580161,15.6707419354839));
#46274=CARTESIAN_POINT('Ctrl Pts',(-2.26751786562628,-4.63758557609733,
15.8290322580645));
#46275=CARTESIAN_POINT('Ctrl Pts',(2.65323118895075,-4.42822781393943,15.9873225806452));
#46276=CARTESIAN_POINT('Ctrl Pts',(5.15882697608013,-0.187992963311806,
16.1456129032258));
#46277=CARTESIAN_POINT('Ctrl Pts',(2.96850419640318,4.22336596918787,16.3039032258064));
#46278=CARTESIAN_POINT('Ctrl Pts',(-1.92395505269964,4.79032719267193,16.4621935483871));
#46279=CARTESIAN_POINT('Ctrl Pts',(-5.06509812664321,0.99680352926066,16.6204838709677));
#46280=CARTESIAN_POINT('Ctrl Pts',(-3.59564132150574,-3.70407899527331,
16.7787741935484));
#46281=CARTESIAN_POINT('Ctrl Pts',(1.14681571606612,-5.03325475486043,16.937064516129));
#46282=CARTESIAN_POINT('Ctrl Pts',(4.84536125415653,-1.78081574711759,17.0953548387097));
#46283=CARTESIAN_POINT('Ctrl Pts',(4.13332826509411,3.09264287390914,17.2536451612903));
#46284=CARTESIAN_POINT('Ctrl Pts',(-0.341147903092961,5.15096781506579,
17.411935483871));
#46285=CARTESIAN_POINT('Ctrl Pts',(-4.50508031651524,2.52052377735926,17.5702258064516));
#46286=CARTESIAN_POINT('Ctrl Pts',(-4.56819357313145,-2.40426585138671,
17.7285161290323));
#46287=CARTESIAN_POINT('Ctrl Pts',(-0.472995886023615,-5.14054336213398,
17.8868064516129));
#46288=CARTESIAN_POINT('Ctrl Pts',(4.05270272242283,-3.19751510246813,18.0450967741935));
#46289=CARTESIAN_POINT('Ctrl Pts',(4.88945318540557,1.65605334244537,18.2033870967742));
#46290=CARTESIAN_POINT('Ctrl Pts',(1.27529601904452,5.00227852023644,18.3616774193548));
#46291=CARTESIAN_POINT('Ctrl Pts',(-3.49935701088739,3.79487555159269,18.5199677419355));
#46292=CARTESIAN_POINT('Ctrl Pts',(-5.0893549352888,-0.866480998244023,
18.6782580645161));
#46293=CARTESIAN_POINT('Ctrl Pts',(-2.04533412033072,-4.73987705500777,
18.8365483870968));
#46294=CARTESIAN_POINT('Ctrl Pts',(2.85792925831606,-4.29723869811459,18.9948387096774));
#46295=CARTESIAN_POINT('Ctrl Pts',(5.16462833680317,0.0542185969503185,
19.1531290322581));
#46296=CARTESIAN_POINT('Ctrl Pts',(2.76051461044002,4.36178489183685,19.3114193548387));
#46297=CARTESIAN_POINT('Ctrl Pts',(-1.32005059452733,4.63359119197125,19.4433279569892));
#46298=CARTESIAN_POINT('Ctrl Pts',(-3.63987183575178,2.72812739966123,19.5488548387097));
#46299=CARTESIAN_POINT('Ctrl Pts',(-4.21857665773145,1.35764386397051,19.6016182795699));
#46300=CARTESIAN_POINT('Ctrl Pts',(-4.32479004603219,0.640761311051878,
19.628));
#46301=CARTESIAN_POINT('',(2.53835875722687,-3.55965150255045,0.));
#46302=CARTESIAN_POINT('Ctrl Pts',(2.53835875722687,-3.55965150255045,-1.94289029309402E-15));
#46303=CARTESIAN_POINT('Ctrl Pts',(3.1284109977952,-3.13889001199587,0.0263817204301056));
#46304=CARTESIAN_POINT('Ctrl Pts',(4.08550837253979,-1.9999918568306,0.0791451612903207));
#46305=CARTESIAN_POINT('Ctrl Pts',(4.72679975347169,0.932772746710439,0.184672043010751));
#46306=CARTESIAN_POINT('Ctrl Pts',(2.62811439332184,4.44281702219704,0.316580645161289));
#46307=CARTESIAN_POINT('Ctrl Pts',(-2.3016075840404,4.62373529115294,0.474870967741933));
#46308=CARTESIAN_POINT('Ctrl Pts',(-4.29378651801925,1.77938049543143,0.58648078871983));
#46309=CARTESIAN_POINT('Ctrl Pts',(-4.37763907935493,0.169045277724475,
0.645327168837512));
#46310=CARTESIAN_POINT('Ctrl Pts',(-4.37640441740291,0.00246357316762608,
0.651410108094978));
#46311=CARTESIAN_POINT('Ctrl Pts',(2.17571852337094,4.44456444733847,4.16333634234434E-17));
#46312=CARTESIAN_POINT('Ctrl Pts',(2.288553758881,4.38223977042994,4.80899030934479E-17));
#46313=CARTESIAN_POINT('Ctrl Pts',(2.39856816217823,4.31535914976362,1.26999648448827E-16));
#46314=CARTESIAN_POINT('Ctrl Pts',(2.50544378309707,4.24391302988421,1.37043154602168E-16));
#46315=CARTESIAN_POINT('Ctrl Pts',(2.62554044419194,4.16362867343386,1.45788230031228E-16));
#46316=CARTESIAN_POINT('Ctrl Pts',(2.7416747038151,4.07757963945051,2.86902645733316E-16));
#46317=CARTESIAN_POINT('Ctrl Pts',(2.85366454038282,3.98618686426695,3.64291929955129E-16));
#46318=CARTESIAN_POINT('Ctrl Pts',(2.9232629976869,3.92938888726778,4.12387140724083E-16));
#46319=CARTESIAN_POINT('Ctrl Pts',(2.99126006746036,3.87052620415169,6.62527936102846E-16));
#46320=CARTESIAN_POINT('Ctrl Pts',(3.05760444128136,3.80969336998723,7.21644966006352E-16));
#46321=CARTESIAN_POINT('Ctrl Pts',(3.09753791324214,3.7730773596537,7.57228213237312E-16));
#46322=CARTESIAN_POINT('Ctrl Pts',(3.13687250045182,3.73574748028041,-2.48343235400226E-16));
#46323=CARTESIAN_POINT('Ctrl Pts',(3.17559590361344,3.69772367591327,-3.60822483003176E-16));
#46324=CARTESIAN_POINT('Ctrl Pts',(3.19355313598542,3.68009086900739,-4.12982567637309E-16));
#46325=CARTESIAN_POINT('Ctrl Pts',(3.21137384475144,3.66231375739153,2.85386760819859E-16));
#46326=CARTESIAN_POINT('Ctrl Pts',(3.22905135321198,3.64440041383412,2.77555756156289E-16));
#46327=CARTESIAN_POINT('Ctrl Pts',(3.33032953777236,3.54177108012739,2.32690274271181E-16));
#46328=CARTESIAN_POINT('Ctrl Pts',(3.42697009782031,3.4346145361773,1.17947475774344E-16));
#46329=CARTESIAN_POINT('Ctrl Pts',(3.51879473621821,3.32334962039163,1.38777878078145E-16));
#46330=CARTESIAN_POINT('Ctrl Pts',(3.60865605635445,3.21446367875555,1.59162901995989E-16));
#46331=CARTESIAN_POINT('Ctrl Pts',(3.69390536375717,3.10164237133953,1.64416256607793E-16));
#46332=CARTESIAN_POINT('Ctrl Pts',(3.77433601631748,2.9852523894932,1.52655665885959E-16));
#46333=CARTESIAN_POINT('Ctrl Pts',(3.80952442681261,2.93433177243543,1.47510407445157E-16));
#46334=CARTESIAN_POINT('Ctrl Pts',(3.84378998451378,2.88272782098782,-1.03604202083645E-16));
#46335=CARTESIAN_POINT('Ctrl Pts',(3.87711279910771,2.83047021492504,-1.52655665885959E-16));
#46336=CARTESIAN_POINT('Ctrl Pts',(3.90167945166607,2.79194422402902,-1.88817985407716E-16));
#46337=CARTESIAN_POINT('Ctrl Pts',(3.92573367987553,2.75306295204808,1.37038491228682E-16));
#46338=CARTESIAN_POINT('Ctrl Pts',(3.94926693181774,2.71383814709955,1.2490009027033E-16));
#46339=CARTESIAN_POINT('Ctrl Pts',(3.95979885299727,2.69628372856808,1.19467747878689E-16));
#46340=CARTESIAN_POINT('Ctrl Pts',(3.97022193097802,2.67866796640904,3.81603872600368E-16));
#46341=CARTESIAN_POINT('Ctrl Pts',(3.98053410416003,2.66099477842828,3.7470027081099E-16));
#46342=CARTESIAN_POINT('Ctrl Pts',(4.05311436653015,2.53660541859884,3.26110587499023E-16));
#46343=CARTESIAN_POINT('Ctrl Pts',(4.12023044721824,2.40933003202768,5.80264781591426E-16));
#46344=CARTESIAN_POINT('Ctrl Pts',(4.1817056161975,2.27957303631144,5.41233724504764E-16));
#46345=CARTESIAN_POINT('Ctrl Pts',(4.24306352883745,2.15006353613803,5.02277114368784E-16));
#46346=CARTESIAN_POINT('Ctrl Pts',(4.29880233786649,2.01808110524174,-2.01806554237873E-16));
#46347=CARTESIAN_POINT('Ctrl Pts',(4.34869895497134,1.88400727320529,-2.08166817117217E-16));
#46348=CARTESIAN_POINT('Ctrl Pts',(4.3987130094648,1.74961788308838,-2.14542049601851E-16));
#46349=CARTESIAN_POINT('Ctrl Pts',(4.44285769397013,1.61312648052743,2.07700331834603E-16));
#46350=CARTESIAN_POINT('Ctrl Pts',(4.48085566800584,1.47490808725521,2.22044604925031E-16));
#46351=CARTESIAN_POINT('Ctrl Pts',(4.50935414853263,1.37124429230104,2.32802809742852E-16));
#46352=CARTESIAN_POINT('Ctrl Pts',(4.53439405643066,1.26660880723853,3.27090126933202E-16));
#46353=CARTESIAN_POINT('Ctrl Pts',(4.55583718119808,1.16116031586893,3.33066907387547E-16));
#46354=CARTESIAN_POINT('Ctrl Pts',(4.5647459632839,1.1173505800641,3.35550026579367E-16));
#46355=CARTESIAN_POINT('Ctrl Pts',(4.57303368750873,1.073400536371,3.93488937669688E-16));
#46356=CARTESIAN_POINT('Ctrl Pts',(4.58068946156208,1.02932171064127,4.16333634234434E-16));
#46357=CARTESIAN_POINT('Ctrl Pts',(4.58528213032192,1.00287899635937,4.3003807790138E-16));
#46358=CARTESIAN_POINT('Ctrl Pts',(4.58964820129846,0.976383975558462,1.1911498064296E-16));
#46359=CARTESIAN_POINT('Ctrl Pts',(4.59378028021791,0.949872636571533,1.38777878078145E-16));
#46360=CARTESIAN_POINT('Ctrl Pts',(4.61514939077547,0.812768833647209,2.40464858739661E-16));
#46361=CARTESIAN_POINT('Ctrl Pts',(4.63029132458926,0.675091193156248,-6.4053354410212E-17));
#46362=CARTESIAN_POINT('Ctrl Pts',(4.63900152451931,0.537186451104229,-1.38777878078145E-16));
#46363=CARTESIAN_POINT('Ctrl Pts',(4.64607280433788,0.42523000611001,-1.99442159083017E-16));
#46364=CARTESIAN_POINT('Ctrl Pts',(4.64890419840177,0.313123505052828,4.93108554065338E-16));
#46365=CARTESIAN_POINT('Ctrl Pts',(4.64736094433393,0.20105139156818,4.71844785465692E-16));
#46366=CARTESIAN_POINT('Ctrl Pts',(4.64544832051237,0.0621554064876461,
4.17736069944506E-16));
#46367=CARTESIAN_POINT('Ctrl Pts',(4.63681759992347,-0.0766885915146454,
3.72153370275118E-16));
#46368=CARTESIAN_POINT('Ctrl Pts',(4.62166663169142,-0.215038242011895,
4.16333634234434E-16));
#46369=CARTESIAN_POINT('Ctrl Pts',(4.60648817669052,-0.353638885370275,
4.605940496854E-16));
#46370=CARTESIAN_POINT('Ctrl Pts',(4.58476541728463,-0.491744202092864,
1.3585326957315E-16));
#46371=CARTESIAN_POINT('Ctrl Pts',(4.55664910490708,-0.628889846984247,
2.22044604925031E-16));
#46372=CARTESIAN_POINT('Ctrl Pts',(4.54627797904168,-0.679478086507271,
2.53837578891091E-16));
#46373=CARTESIAN_POINT('Ctrl Pts',(4.53503649423606,-0.729935498537829,
-4.17628381648536E-17));
#46374=CARTESIAN_POINT('Ctrl Pts',(4.52293072203927,-0.780237766000663,
-5.55111512312578E-17));
#46375=CARTESIAN_POINT('Ctrl Pts',(4.51852089045776,-0.798561630358381,
-6.05193195799785E-17));
#46376=CARTESIAN_POINT('Ctrl Pts',(4.51399616118864,-0.816865466942453,
-2.76721061431502E-16));
#46377=CARTESIAN_POINT('Ctrl Pts',(4.50936083932464,-0.835132869996713,
-2.77555756156289E-16));
#46378=CARTESIAN_POINT('Ctrl Pts',(4.47555258032973,-0.968368298245966,
-2.83643699187054E-16));
#46379=CARTESIAN_POINT('Ctrl Pts',(4.43581935723855,-1.09986196998026,4.56182438062644E-17));
#46380=CARTESIAN_POINT('Ctrl Pts',(4.39038959840621,-1.229200829575,5.55111512312578E-17));
#46381=CARTESIAN_POINT('Ctrl Pts',(4.34480983538931,-1.35896675219327,6.54367239740816E-17));
#46382=CARTESIAN_POINT('Ctrl Pts',(4.29349546516567,-1.48656440482432,-4.64120495657098E-16));
#46383=CARTESIAN_POINT('Ctrl Pts',(4.23662839209755,-1.61155805192221,-3.05311331771918E-16));
#46384=CARTESIAN_POINT('Ctrl Pts',(4.17976131902944,-1.7365516990201,-1.46502167886738E-16));
#46385=CARTESIAN_POINT('Ctrl Pts',(4.11734114389621,-1.85894212089202,1.98375931461375E-16));
#46386=CARTESIAN_POINT('Ctrl Pts',(4.04950702451708,-1.97826322671605,2.22044604925031E-16));
#46387=CARTESIAN_POINT('Ctrl Pts',(4.0039219578893,-2.05844795689127,2.37950141352824E-16));
#46388=CARTESIAN_POINT('Ctrl Pts',(3.95589106826036,-2.13724588577774,1.34209299017938E-16));
#46389=CARTESIAN_POINT('Ctrl Pts',(3.90547300064698,-2.21455451296583,1.66533453693773E-16));
#46390=CARTESIAN_POINT('Ctrl Pts',(3.88226355505238,-2.25014275467462,1.81413550152313E-16));
#46391=CARTESIAN_POINT('Ctrl Pts',(3.85854814303777,-2.28541527809141,-1.96535868138964E-16));
#46392=CARTESIAN_POINT('Ctrl Pts',(3.8343320388377,-2.32036145673223,-2.22044604925031E-16));
#46393=CARTESIAN_POINT('Ctrl Pts',(3.81846869581275,-2.34325379377416,-2.38754718097135E-16));
#46394=CARTESIAN_POINT('Ctrl Pts',(3.80239048915502,-2.36600608076709,-1.28420314193019E-17));
#46395=CARTESIAN_POINT('Ctrl Pts',(3.78609884210449,-2.38861523157554,0.));
#46396=CARTESIAN_POINT('Ctrl Pts',(3.77490538198125,-2.40414924279059,8.82334156561408E-18));
#46397=CARTESIAN_POINT('Ctrl Pts',(3.76361599384939,-2.41960894071961,1.65364095173029E-16));
#46398=CARTESIAN_POINT('Ctrl Pts',(3.7522346949218,-2.43498912758705,1.66533453693773E-16));
#46399=CARTESIAN_POINT('Ctrl Pts',(3.66941253061457,-2.54691135824948,1.75042922090602E-16));
#46400=CARTESIAN_POINT('Ctrl Pts',(3.58167249725696,-2.65470179052059,3.28026165867355E-16));
#46401=CARTESIAN_POINT('Ctrl Pts',(3.48928766288614,-2.75807107487432,2.22044604925031E-16));
#46402=CARTESIAN_POINT('Ctrl Pts',(3.39991887248819,-2.85806571111424,1.19522973854221E-16));
#46403=CARTESIAN_POINT('Ctrl Pts',(3.30620285470906,-2.9539234934181,-1.0442180859248E-16));
#46404=CARTESIAN_POINT('Ctrl Pts',(3.20834980062004,-3.04534562649001,-1.66533453693773E-16));
#46405=CARTESIAN_POINT('Ctrl Pts',(3.11144260907094,-3.13588405928502,-2.28044718163707E-16));
#46406=CARTESIAN_POINT('Ctrl Pts',(3.01047744826623,-3.22207261031851,3.41219002678743E-16));
#46407=CARTESIAN_POINT('Ctrl Pts',(2.90563068007557,-3.30357847782834,3.33066907387547E-16));
#46408=CARTESIAN_POINT('Ctrl Pts',(2.80291415997029,-3.38342833131688,3.25080444148589E-16));
#46409=CARTESIAN_POINT('Ctrl Pts',(2.69647166403099,-3.45878415557578,1.92670969748543E-16));
#46410=CARTESIAN_POINT('Ctrl Pts',(2.58644978075874,-3.52928668450907,1.66533453693773E-16));
#46411=CARTESIAN_POINT('Ctrl Pts',(2.57049460076127,-3.53951083724989,1.62743037088118E-16));
#46412=CARTESIAN_POINT('Ctrl Pts',(2.5544641189252,-3.54963283815124,3.31276988434876E-16));
#46413=CARTESIAN_POINT('Ctrl Pts',(2.53835875722692,-3.55965150255041,3.33066907387547E-16));
#46414=CARTESIAN_POINT('Ctrl Pts',(0.446494146901359,4.91265885279923,19.058));
#46415=CARTESIAN_POINT('Ctrl Pts',(1.22846295052447,4.84360722676543,19.0327765671335));
#46416=CARTESIAN_POINT('Ctrl Pts',(1.9933030120195,4.59769822736177,19.0075531342671));
#46417=CARTESIAN_POINT('Ctrl Pts',(2.65082820116331,4.18037408759279,18.9823297014006));
#46418=CARTESIAN_POINT('Ctrl Pts',(4.02626712794074,3.307397848204,18.9295662605404));
#46419=CARTESIAN_POINT('Ctrl Pts',(4.93211723740144,1.68434260046616,18.8768028196802));
#46420=CARTESIAN_POINT('Ctrl Pts',(4.95046975302369,0.05301847033729,18.82403937882));
#46421=CARTESIAN_POINT('Ctrl Pts',(4.96882226864594,-1.57830565979157,18.7712759379598));
#46422=CARTESIAN_POINT('Ctrl Pts',(4.09967719042974,-3.21789867231146,18.7185124970995));
#46423=CARTESIAN_POINT('Ctrl Pts',(2.74135016758908,-4.12108640912056,18.6657490562393));
#46424=CARTESIAN_POINT('Ctrl Pts',(1.38302314474846,-5.02427414592964,18.6129856153791));
#46425=CARTESIAN_POINT('Ctrl Pts',(-0.464485822716606,-5.19105660702797,
18.5602221745189));
#46426=CARTESIAN_POINT('Ctrl Pts',(-1.9617212025883,-4.54471608580352,18.5074587336587));
#46427=CARTESIAN_POINT('Ctrl Pts',(-3.45895658246008,-3.89837556457903,
18.4546952927985));
#46428=CARTESIAN_POINT('Ctrl Pts',(-4.60591837473846,-2.43891206103166,
18.4019318519383));
#46429=CARTESIAN_POINT('Ctrl Pts',(-4.87985025660527,-0.831000068739,18.349168411078));
#46430=CARTESIAN_POINT('Ctrl Pts',(-4.92631242249651,-0.558278714746532,
18.340219092271));
#46431=CARTESIAN_POINT('Ctrl Pts',(-4.94765902855038,-0.28128675460715,
18.3312697734639));
#46432=CARTESIAN_POINT('Ctrl Pts',(-4.94522242777803,-0.0039236424385497,
18.3223204546569));
#46433=CARTESIAN_POINT('Origin',(0.,0.,-1.84858989190501));
#46434=CARTESIAN_POINT('',(-2.53835875722683,-3.55965150255047,0.));
#46435=CARTESIAN_POINT('Ctrl Pts',(-2.54467524200888,-3.56229978442276,
-3.12521276218947E-15));
#46436=CARTESIAN_POINT('Ctrl Pts',(-1.45608504857279,-4.32913804450291,
0.0486930492780809));
#46437=CARTESIAN_POINT('Ctrl Pts',(1.60942354292801,-4.84594693373762,0.150182632030869));
#46438=CARTESIAN_POINT('Ctrl Pts',(4.96501177239675,-1.41203703483287,0.304468748258361));
#46439=CARTESIAN_POINT('Ctrl Pts',(3.88934922870828,3.39617009289883,0.462858348682473));
#46440=CARTESIAN_POINT('Ctrl Pts',(-0.732920742143878,5.1113964007393,0.621247949106584));
#46441=CARTESIAN_POINT('Ctrl Pts',(-3.9420462167219,2.72159457156631,0.749825130180767));
#46442=CARTESIAN_POINT('Ctrl Pts',(-4.36729319104836,0.635050406119092,
0.825605777780246));
#46443=CARTESIAN_POINT('Ctrl Pts',(-4.36535621882271,0.0014563306878905,
0.848589891905021));
#46444=CARTESIAN_POINT('Origin',(0.,0.,0.));
#46445=CARTESIAN_POINT('Ctrl Pts',(-1.91898364244012,3.92834389788461,-0.329089653438086));
#46446=CARTESIAN_POINT('Ctrl Pts',(-2.57055919540632,3.61005128897394,-0.302691386700734));
#46447=CARTESIAN_POINT('Ctrl Pts',(-3.7023655534584,2.64307614504004,-0.24989485322603));
#46448=CARTESIAN_POINT('Ctrl Pts',(-4.81630944128875,-0.146849281373132,
-0.144301786276623));
#46449=CARTESIAN_POINT('Ctrl Pts',(-3.3181593418561,-3.95557434013013,-0.0123104525898624));
#46450=CARTESIAN_POINT('Ctrl Pts',(1.52017634683108,-4.93727721897207,0.146079147834249));
#46451=CARTESIAN_POINT('Ctrl Pts',(4.96501177239675,-1.41203703483287,0.304468748258361));
#46452=CARTESIAN_POINT('Ctrl Pts',(3.88934922870828,3.39617009289883,0.462858348682473));
#46453=CARTESIAN_POINT('Ctrl Pts',(-0.732920742143878,5.1113964007393,0.621247949106584));
#46454=CARTESIAN_POINT('Ctrl Pts',(-4.68612688169979,2.16748556327014,0.779637549530696));
#46455=CARTESIAN_POINT('Ctrl Pts',(-4.36939265644683,-2.75114092476471,
0.938027149954809));
#46456=CARTESIAN_POINT('Ctrl Pts',(-0.0704529116473286,-5.16289724783097,
1.09641675037892));
#46457=CARTESIAN_POINT('Ctrl Pts',(4.29252819085395,-2.86947836000301,1.25480635080303));
#46458=CARTESIAN_POINT('Ctrl Pts',(4.74374945851672,2.03886099295457,1.41319595122714));
#46459=CARTESIAN_POINT('Ctrl Pts',(0.87187597225223,5.08919664880298,1.57158555165126));
#46460=CARTESIAN_POINT('Ctrl Pts',(-3.79452777359949,3.50164966549009,1.72997515207536));
#46461=CARTESIAN_POINT('Ctrl Pts',(-5.00293367927747,-1.2769919878773,1.88836475249948));
#46462=CARTESIAN_POINT('Ctrl Pts',(-1.65208468153467,-4.89189754332655,
2.04675435292359));
#46463=CARTESIAN_POINT('Ctrl Pts',(3.20433051897175,-4.04874042926377,2.20514395334771));
#46464=CARTESIAN_POINT('Ctrl Pts',(5.14059300557593,0.484092964878372,2.36353355377181));
#46465=CARTESIAN_POINT('Ctrl Pts',(2.392155064142,4.57576601695794,2.52192315419593));
#46466=CARTESIAN_POINT('Ctrl Pts',(-2.53628918908134,4.49747442552335,2.68031275462004));
#46467=CARTESIAN_POINT('Ctrl Pts',(-5.15337531200808,0.320567159775624,
2.83870235504415));
#46468=CARTESIAN_POINT('Ctrl Pts',(-3.07411308423917,-4.14847788693502,
2.99709195546826));
#46469=CARTESIAN_POINT('Ctrl Pts',(1.80663443860224,-4.83695274769126,3.15548155589238));
#46470=CARTESIAN_POINT('Ctrl Pts',(5.04096893490742,-1.11744005069485,3.31387115631648));
#46471=CARTESIAN_POINT('Ctrl Pts',(3.68139281034196,3.62041254264275,3.4722607567406));
#46472=CARTESIAN_POINT('Ctrl Pts',(-1.03309179131411,5.05892887272037,3.63065035716471));
#46473=CARTESIAN_POINT('Ctrl Pts',(-4.80610435287845,1.88716744466989,3.78903995758882));
#46474=CARTESIAN_POINT('Ctrl Pts',(-4.19924192609147,-3.00439798462519,
3.94742955801293));
#46475=CARTESIAN_POINT('Ctrl Pts',(0.234452652827207,-5.15801046495039,
4.10581915843705));
#46476=CARTESIAN_POINT('Ctrl Pts',(4.4544870133001,-2.61105064195526,4.26420875886115));
#46477=CARTESIAN_POINT('Ctrl Pts',(4.61508054334482,2.31539879571022,4.42259835928526));
#46478=CARTESIAN_POINT('Ctrl Pts',(0.56988195080356,5.13179058096912,4.58098795970938));
#46479=CARTESIAN_POINT('Ctrl Pts',(-3.99465861152192,3.27150463588748,4.73937756013348));
#46480=CARTESIAN_POINT('Ctrl Pts',(-4.91880686345887,-1.5701525546756,4.89776716055761));
#46481=CARTESIAN_POINT('Ctrl Pts',(-1.36037264139205,-4.98090617072295,
5.05615676098171));
#46482=CARTESIAN_POINT('Ctrl Pts',(3.43778957362211,-3.85248528258675,5.21454636140584));
#46483=CARTESIAN_POINT('Ctrl Pts',(5.10304258525828,0.786763228710822,5.37293596182993));
#46484=CARTESIAN_POINT('Ctrl Pts',(2.11781634615703,4.70902260867037,5.53132556225406));
#46485=CARTESIAN_POINT('Ctrl Pts',(-2.79740769526454,4.33987905263503,5.68971516267816));
#46486=CARTESIAN_POINT('Ctrl Pts',(-5.16331214443354,0.0157386201644824,
5.84810476310228));
#46487=CARTESIAN_POINT('Ctrl Pts',(-2.82381278957536,-4.32274465293194,
6.00649436352639));
#46488=CARTESIAN_POINT('Ctrl Pts',(2.08906951604171,-4.72184588505036,6.16488396395049));
#46489=CARTESIAN_POINT('Ctrl Pts',(5.098151436811,-0.817858137064712,6.32327356437462));
#46490=CARTESIAN_POINT('Ctrl Pts',(3.46121148378334,3.83145599864432,6.48166316479871));
#46491=CARTESIAN_POINT('Ctrl Pts',(-1.32998241066,4.98910681308353,6.64005276522284));
#46492=CARTESIAN_POINT('Ctrl Pts',(-4.90914338527368,1.60010975493711,6.79844236564693));
#46493=CARTESIAN_POINT('Ctrl Pts',(-4.01452835847177,-3.24709132363831,
6.95683196607106));
#46494=CARTESIAN_POINT('Ctrl Pts',(0.538586577094185,-5.13516937442138,
7.11522156649516));
#46495=CARTESIAN_POINT('Ctrl Pts',(4.60087948645563,-2.34349054961462,7.27361116691928));
#46496=CARTESIAN_POINT('Ctrl Pts',(4.47032190918109,2.58384636410851,7.43200076734339));
#46497=CARTESIAN_POINT('Ctrl Pts',(0.26589292373178,5.15648532996368,7.59039036776751));
#46498=CARTESIAN_POINT('Ctrl Pts',(-4.18084827136001,3.02994187021587,7.74877996819161));
#46499=CARTESIAN_POINT('Ctrl Pts',(-4.81751972636668,-1.85783306329961,
7.90716956861574));
#46500=CARTESIAN_POINT('Ctrl Pts',(-1.06391319462353,-5.05253685976928,
8.06555916903983));
#46501=CARTESIAN_POINT('Ctrl Pts',(3.65925338948522,-3.64278803069328,8.22394876946396));
#46502=CARTESIAN_POINT('Ctrl Pts',(5.04768747299395,1.08668817054443,8.38233836988805));
#46503=CARTESIAN_POINT('Ctrl Pts',(1.83608824986349,4.82584914224785,8.54072797031219));
#46504=CARTESIAN_POINT('Ctrl Pts',(-3.04876573566835,4.1671414055724,8.69911757073628));
#46505=CARTESIAN_POINT('Ctrl Pts',(-5.15523377649819,-0.289144798800594,
8.8575071711604));
#46506=CARTESIAN_POINT('Ctrl Pts',(-2.56365995117077,-4.48192901101572,
9.01589677158451));
#46507=CARTESIAN_POINT('Ctrl Pts',(2.36421564112952,-4.59026408905411,9.17428637200862));
#46508=CARTESIAN_POINT('Ctrl Pts',(5.13754605775107,-0.515422651333577,
9.33267597243274));
#46509=CARTESIAN_POINT('Ctrl Pts',(3.22895369161553,4.02913117959985,9.49106557285684));
#46510=CARTESIAN_POINT('Ctrl Pts',(-1.62223260619563,4.90187733184103,9.64945517328097));
#46511=CARTESIAN_POINT('Ctrl Pts',(-4.99505399739544,1.30746914614654,9.80784477370506));
#46512=CARTESIAN_POINT('Ctrl Pts',(-3.81580775774175,-3.47845528374006,
9.96623437412919));
#46513=CARTESIAN_POINT('Ctrl Pts',(0.840841326532404,-5.09441123866306,
10.1246239745533));
#46514=CARTESIAN_POINT('Ctrl Pts',(4.73121909778617,-2.06775381846214,10.2830135749774));
#46515=CARTESIAN_POINT('Ctrl Pts',(4.30996593957687,2.84327867165857,10.4414031754015));
#46516=CARTESIAN_POINT('Ctrl Pts',(-0.0390238264566685,5.16318866070086,
10.5997927758256));
#46517=CARTESIAN_POINT('Ctrl Pts',(-4.35245059410458,2.77780737829316,10.7581823762498));
#46518=CARTESIAN_POINT('Ctrl Pts',(-4.69942385101101,-2.13903143351615,
10.9165719766738));
#46519=CARTESIAN_POINT('Ctrl Pts',(-0.763741663751577,-5.10653881568242,
11.074961577098));
#46520=CARTESIAN_POINT('Ctrl Pts',(3.86794975738412,-3.42038077988013,11.2333511775221));
#46521=CARTESIAN_POINT('Ctrl Pts',(4.97472054752429,1.38282156443299,11.3917407779462));
#46522=CARTESIAN_POINT('Ctrl Pts',(1.54795388466898,4.92583787552529,11.5501303783703));
#46523=CARTESIAN_POINT('Ctrl Pts',(-3.28948637173101,3.97986424582764,11.7085199787944));
#46524=CARTESIAN_POINT('Ctrl Pts',(-5.12916835710966,-0.593019366839089,
11.8669095792185));
#46525=CARTESIAN_POINT('Ctrl Pts',(-2.29456228398659,-4.62547553554524,
12.0252991796426));
#46526=CARTESIAN_POINT('Ctrl Pts',(2.63111281568934,-4.44266646915302,12.1836887800668));
#46527=CARTESIAN_POINT('Ctrl Pts',(5.15901534120123,-0.211188811899807,
12.3420783804909));
#46528=CARTESIAN_POINT('Ctrl Pts',(2.98542980392062,4.2127483773522,12.500467980915));
#46529=CARTESIAN_POINT('Ctrl Pts',(-1.90882269345658,4.79754478144462,12.6588575813391));
#46530=CARTESIAN_POINT('Ctrl Pts',(-5.0635364390099,1.01026666570772,12.8172471817632));
#46531=CARTESIAN_POINT('Ctrl Pts',(-3.60377347746801,-3.6976826159257,12.9756367821873));
#46532=CARTESIAN_POINT('Ctrl Pts',(1.14016230868481,-5.03587826648703,13.1340263826114));
#46533=CARTESIAN_POINT('Ctrl Pts',(4.84505108113381,-1.78480251743019,13.2924159830355));
#46534=CARTESIAN_POINT('Ctrl Pts',(4.13457213027864,3.09279053680373,13.4508055834596));
#46535=CARTESIAN_POINT('Ctrl Pts',(-0.343804419177731,5.15187718471428,
13.6091951838838));
#46536=CARTESIAN_POINT('Ctrl Pts',(-4.50886684456297,2.51598087890574,13.7675847843078));
#46537=CARTESIAN_POINT('Ctrl Pts',(-4.56493128400683,-2.41276654015816,
13.925974384732));
#46538=CARTESIAN_POINT('Ctrl Pts',(-0.460905372910369,-5.14272362102755,
14.0843639851561));
#46539=CARTESIAN_POINT('Ctrl Pts',(4.06315051784514,-3.18603952805496,14.2427535855802));
#46540=CARTESIAN_POINT('Ctrl Pts',(4.88439639669049,1.67413017563193,14.4011431860043));
#46541=CARTESIAN_POINT('Ctrl Pts',(1.25441857601452,5.00863993928383,14.5595327864284));
#46542=CARTESIAN_POINT('Ctrl Pts',(-3.51872970857736,3.7787009993846,14.7179223868525));
#46543=CARTESIAN_POINT('Ctrl Pts',(-5.08520683073047,-0.894824839523584,
14.8763119872766));
#46544=CARTESIAN_POINT('Ctrl Pts',(-2.01745869282129,-4.75288338056742,
15.0347015877008));
#46545=CARTESIAN_POINT('Ctrl Pts',(2.88882981271105,-4.27956800578602,15.1930911881249));
#46546=CARTESIAN_POINT('Ctrl Pts',(5.16248437889336,0.0937818828261288,
15.351480788549));
#46547=CARTESIAN_POINT('Ctrl Pts',(2.73148949656154,4.38166693681219,15.5098703889731));
#46548=CARTESIAN_POINT('Ctrl Pts',(-2.18875273549729,4.67647318514471,15.6682599893972));
#46549=CARTESIAN_POINT('Ctrl Pts',(-5.11435176830703,0.709539282194621,
15.8266495898213));
#46550=CARTESIAN_POINT('Ctrl Pts',(-3.37916532475269,-3.90400842437456,
15.9850391902454));
#46551=CARTESIAN_POINT('Ctrl Pts',(1.43550516966593,-4.9597746708902,16.1434287906695));
#46552=CARTESIAN_POINT('Ctrl Pts',(4.94197826197569,-1.49562391370258,16.3018183910937));
#46553=CARTESIAN_POINT('Ctrl Pts',(3.94475245484231,3.3315114408263,16.4602079915177));
#46554=CARTESIAN_POINT('Ctrl Pts',(-0.647385467154988,5.12259027405121,
16.6185975919419));
#46555=CARTESIAN_POINT('Ctrl Pts',(-4.64955123813058,2.24537608806315,16.776987192366));
#46556=CARTESIAN_POINT('Ctrl Pts',(-4.41451134820182,-2.67808364399215,
16.9353767927901));
#46557=CARTESIAN_POINT('Ctrl Pts',(-0.156460816144074,-5.16096436253732,
17.0937663932142));
#46558=CARTESIAN_POINT('Ctrl Pts',(4.24417435465306,-2.94058317628852,17.2521559936383));
#46559=CARTESIAN_POINT('Ctrl Pts',(4.7770306357801,1.95960002071087,17.4105455940624));
#46560=CARTESIAN_POINT('Ctrl Pts',(0.956505601666415,5.07396180892462,17.5689351944865));
#46561=CARTESIAN_POINT('Ctrl Pts',(-3.73569419127765,3.5643623764192,17.7273247949107));
#46562=CARTESIAN_POINT('Ctrl Pts',(-5.02350584303606,-1.19352508090609,
17.8857143953348));
#46563=CARTESIAN_POINT('Ctrl Pts',(-1.7333097832156,-4.86367572142824,18.0441039957589));
#46564=CARTESIAN_POINT('Ctrl Pts',(3.13645552043595,-4.10159948955856,18.202493596183));
#46565=CARTESIAN_POINT('Ctrl Pts',(5.14796384574126,0.398543369117654,18.3608831966071));
#46566=CARTESIAN_POINT('Ctrl Pts',(2.46797524199195,4.53507188733415,18.5192727970312));
#46567=CARTESIAN_POINT('Ctrl Pts',(-2.46096278237594,4.53951629179981,18.6776623974553));
#46568=CARTESIAN_POINT('Ctrl Pts',(-5.14748183280556,0.405511410062441,
18.8360519978794));
#46569=CARTESIAN_POINT('Ctrl Pts',(-3.14246278706502,-4.0951334678725,18.9944415983036));
#46570=CARTESIAN_POINT('Ctrl Pts',(1.72525842040716,-4.86940713488401,19.1528311987277));
#46571=CARTESIAN_POINT('Ctrl Pts',(5.02276837180745,-1.19521866677756,19.3112207991518));
#46572=CARTESIAN_POINT('Ctrl Pts',(3.95306672650205,2.75529758855723,19.4432121328385));
#46573=CARTESIAN_POINT('Ctrl Pts',(1.3947178009747,4.32991044428859,19.548805199788));
#46574=CARTESIAN_POINT('Ctrl Pts',(-0.0904913830656236,4.43080762341373,
19.6016017332627));
#46575=CARTESIAN_POINT('Ctrl Pts',(-0.803308159453631,4.29756675351939,
19.628));
#46576=CARTESIAN_POINT('Ctrl Pts',(-2.00237954638878,4.09906332620074,-0.219393102292058));
#46577=CARTESIAN_POINT('Ctrl Pts',(-2.6822715117666,3.76693823886074,-0.192994835554706));
#46578=CARTESIAN_POINT('Ctrl Pts',(-3.86326433094171,2.75793992993429,-0.140198302080001));
#46579=CARTESIAN_POINT('Ctrl Pts',(-5.02561840602911,-0.153231111990883,
-0.0346052351305939));
#46580=CARTESIAN_POINT('Ctrl Pts',(-3.46236114308042,-4.12747715912022,
0.0973860985561662));
#46581=CARTESIAN_POINT('Ctrl Pts',(1.58624073518831,-5.15184324632905,0.255775698980278));
#46582=CARTESIAN_POINT('Ctrl Pts',(5.18078309827857,-1.47340186480046,0.414165299404389));
#46583=CARTESIAN_POINT('Ctrl Pts',(4.0583740122066,3.54376211431939,0.572554899828502));
#46584=CARTESIAN_POINT('Ctrl Pts',(-0.764772284002811,5.33352936417491,
0.730944500252612));
#46585=CARTESIAN_POINT('Ctrl Pts',(-4.88977832440859,2.26168095600148,0.889334100676726));
#46586=CARTESIAN_POINT('Ctrl Pts',(-4.55927934554221,-2.87070102899737,
1.04772370110084));
#46587=CARTESIAN_POINT('Ctrl Pts',(-0.0735146804517841,-5.38726835420972,
1.20611330152495));
#46588=CARTESIAN_POINT('Ctrl Pts',(4.47907447545189,-2.9941812164533,1.36450290194906));
#46589=CARTESIAN_POINT('Ctrl Pts',(4.94990508457304,2.12746657133089,1.52289250237317));
#46590=CARTESIAN_POINT('Ctrl Pts',(0.909766282116828,5.31036484717274,1.68128210279728));
#46591=CARTESIAN_POINT('Ctrl Pts',(-3.95943177107978,3.65382565735724,1.8396717032214));
#46592=CARTESIAN_POINT('Ctrl Pts',(-5.2203530294748,-1.33248798003114,1.99806130364551));
#46593=CARTESIAN_POINT('Ctrl Pts',(-1.72388159129946,-5.10449144388282,
2.15645090406962));
#46594=CARTESIAN_POINT('Ctrl Pts',(3.34358550492888,-4.22469209476243,2.31484050449373));
#46595=CARTESIAN_POINT('Ctrl Pts',(5.36399480590974,0.505130856764646,2.47323010491784));
#46596=CARTESIAN_POINT('Ctrl Pts',(2.49611422749678,4.77462135621273,2.63161970534196));
#46597=CARTESIAN_POINT('Ctrl Pts',(-2.64651218677699,4.69292733971583,2.79000930576607));
#46598=CARTESIAN_POINT('Ctrl Pts',(-5.37733261056287,0.334498486481351,
2.94839890619018));
#46599=CARTESIAN_POINT('Ctrl Pts',(-3.20770903254784,-4.32876397991708,
3.10678850661429));
#46600=CARTESIAN_POINT('Ctrl Pts',(1.88514782911787,-5.04715883690933,3.2651781070384));
#46601=CARTESIAN_POINT('Ctrl Pts',(5.26004123537227,-1.16600217549634,3.42356770746252));
#46602=CARTESIAN_POINT('Ctrl Pts',(3.84138014656453,3.77774977574021,3.58195730788662));
#46603=CARTESIAN_POINT('Ctrl Pts',(-1.07798827812784,5.27878168283402,3.74034690831074));
#46604=CARTESIAN_POINT('Ctrl Pts',(-5.01496982109594,1.96918066847761,3.89873650873484));
#46605=CARTESIAN_POINT('Ctrl Pts',(-4.38173414154377,-3.1349642282388,4.05712610915897));
#46606=CARTESIAN_POINT('Ctrl Pts',(0.244641583302294,-5.38216919970349,
4.21551570958307));
#46607=CARTESIAN_POINT('Ctrl Pts',(4.64807176456428,-2.72452265064043,4.37390531000719));
#46608=CARTESIAN_POINT('Ctrl Pts',(4.81564442789093,2.41602225663996,4.53229491043129));
#46609=CARTESIAN_POINT('Ctrl Pts',(0.594648092306935,5.35480984226466,4.69068451085541));
#46610=CARTESIAN_POINT('Ctrl Pts',(-4.16825996929618,3.41367889956971,4.84907411127951));
#46611=CARTESIAN_POINT('Ctrl Pts',(-5.13257019924506,-1.63838882763724,
5.00746371170364));
#46612=CARTESIAN_POINT('Ctrl Pts',(-1.41949222095851,-5.19736824127129,
5.16585331212774));
#46613=CARTESIAN_POINT('Ctrl Pts',(3.58719030989569,-4.01990801902123,5.32424291255186));
#46614=CARTESIAN_POINT('Ctrl Pts',(5.32481250547765,0.820954677351021,5.48263251297596));
#46615=CARTESIAN_POINT('Ctrl Pts',(2.2098531956012,4.91366906238659,5.64102211340008));
#46616=CARTESIAN_POINT('Ctrl Pts',(-2.9189784779956,4.52848312857297,5.79941171382418));
#46617=CARTESIAN_POINT('Ctrl Pts',(-5.38770128154296,0.0164225949658002,
5.9578013142483));
#46618=CARTESIAN_POINT('Ctrl Pts',(-2.9465310947033,-4.51060409576292,6.11619091467242));
#46619=CARTESIAN_POINT('Ctrl Pts',(2.17985707506455,-4.92704961747478,6.27458051509652));
#46620=CARTESIAN_POINT('Ctrl Pts',(5.3197087956843,-0.853400919782555,6.43297011552065));
#46621=CARTESIAN_POINT('Ctrl Pts',(3.61163009812893,3.99796483664578,6.59135971594474));
#46622=CARTESIAN_POINT('Ctrl Pts',(-1.38778128029068,5.20592527019374,6.74974931636887));
#46623=CARTESIAN_POINT('Ctrl Pts',(-5.12248676203533,1.6696479190355,6.90813891679296));
#46624=CARTESIAN_POINT('Ctrl Pts',(-4.18899322308973,-3.38820462452834,
7.0665285172171));
#46625=CARTESIAN_POINT('Ctrl Pts',(0.561992672622043,-5.35833547257784,
7.22491811764118));
#46626=CARTESIAN_POINT('Ctrl Pts',(4.80082621619637,-2.44533483242041,7.38330771806533));
#46627=CARTESIAN_POINT('Ctrl Pts',(4.66459481923242,2.69613611918183,7.5416973184894));
#46628=CARTESIAN_POINT('Ctrl Pts',(0.27744819717852,5.38057778483401,7.70008691891355));
#46629=CARTESIAN_POINT('Ctrl Pts',(-4.36254112853255,3.16161820949792,7.85847651933763));
#46630=CARTESIAN_POINT('Ctrl Pts',(-5.02688128812553,-1.93857146266532,
8.01686611976177));
#46631=CARTESIAN_POINT('Ctrl Pts',(-1.11014912943107,-5.27211188340975,
8.17525572018585));
#46632=CARTESIAN_POINT('Ctrl Pts',(3.81827858253237,-3.80109766606194,8.33364532061));
#46633=CARTESIAN_POINT('Ctrl Pts',(5.26705175018262,1.13391386871537,8.49203492103408));
#46634=CARTESIAN_POINT('Ctrl Pts',(1.91588165504971,5.03557268685605,8.65042452145821));
#46635=CARTESIAN_POINT('Ctrl Pts',(-3.18126012948741,4.34823858468009,8.80881412188231));
#46636=CARTESIAN_POINT('Ctrl Pts',(-5.37927184089313,-0.301710560871043,
8.96720372230643));
#46637=CARTESIAN_POINT('Ctrl Pts',(-2.67507243761234,-4.67670634681008,
9.12559332273054));
#46638=CARTESIAN_POINT('Ctrl Pts',(2.46696060266074,-4.78974949091146,9.28398292315464));
#46639=CARTESIAN_POINT('Ctrl Pts',(5.36081544269451,-0.537822080371423,
9.44237252357877));
#46640=CARTESIAN_POINT('Ctrl Pts',(3.36927876055584,4.20423065904265,9.60076212400287));
#46641=CARTESIAN_POINT('Ctrl Pts',(-1.69273219338161,5.11490493775362,9.75915172442699));
#46642=CARTESIAN_POINT('Ctrl Pts',(-5.21213090945059,1.36428962596537,9.91754132485109));
#46643=CARTESIAN_POINT('Ctrl Pts',(-3.98163654867748,-3.62962328554942,
10.0759309252752));
#46644=CARTESIAN_POINT('Ctrl Pts',(0.877382921235304,-5.31580605461594,
10.2343205256993));
#46645=CARTESIAN_POINT('Ctrl Pts',(4.93683017477137,-2.15761503198178,10.3927101261234));
#46646=CARTESIAN_POINT('Ctrl Pts',(4.49727004033617,2.96684293232075,10.5510997265475));
#46647=CARTESIAN_POINT('Ctrl Pts',(-0.0407197384023858,5.38757243140836,
10.7094893269717));
#46648=CARTESIAN_POINT('Ctrl Pts',(-4.54160100876145,2.89852636316868,10.8678789273958));
#46649=CARTESIAN_POINT('Ctrl Pts',(-4.90365315835139,-2.23199025610718,
11.0262685278199));
#46650=CARTESIAN_POINT('Ctrl Pts',(-0.796932632670351,-5.32846067638225,
11.184658128244));
#46651=CARTESIAN_POINT('Ctrl Pts',(4.03604455470867,-3.56902495832874,11.3430477286681));
#46652=CARTESIAN_POINT('Ctrl Pts',(5.19091380096199,1.44291673763568,11.5014373290922));
#46653=CARTESIAN_POINT('Ctrl Pts',(1.6152254395837,5.13990676764554,11.6598269295163));
#46654=CARTESIAN_POINT('Ctrl Pts',(-3.43244209236889,4.15282266456216,11.8182165299404));
#46655=CARTESIAN_POINT('Ctrl Pts',(-5.3520736608267,-0.618791022762998,
11.9766061303646));
#46656=CARTESIAN_POINT('Ctrl Pts',(-2.39428022405006,-4.82649116952364,
12.1349957307887));
#46657=CARTESIAN_POINT('Ctrl Pts',(2.7454566937728,-4.63573751881888,12.2933853312128));
#46658=CARTESIAN_POINT('Ctrl Pts',(5.38321774623971,-0.22036673373445,12.4517749316369));
#46659=CARTESIAN_POINT('Ctrl Pts',(3.11517172129139,4.39582756118039,12.610164532061));
#46660=CARTESIAN_POINT('Ctrl Pts',(-1.99177701910997,5.00603826462726,12.7685541324851));
#46661=CARTESIAN_POINT('Ctrl Pts',(-5.28358948645086,1.05417120973438,12.9269437329092));
#46662=CARTESIAN_POINT('Ctrl Pts',(-3.76038760389046,-3.85837788057022,
13.0853333333334));
#46663=CARTESIAN_POINT('Ctrl Pts',(1.18971190581428,-5.25472933479274,13.2437229337574));
#46664=CARTESIAN_POINT('Ctrl Pts',(5.05560911073477,-1.862367128206,13.4021125341816));
#46665=CARTESIAN_POINT('Ctrl Pts',(4.3142539017226,3.22719817678374,13.5605021346057));
#46666=CARTESIAN_POINT('Ctrl Pts',(-0.358745599334103,5.37576937709664,
13.7188917350298));
#46667=CARTESIAN_POINT('Ctrl Pts',(-4.70481485473382,2.6253213105142,13.8772813354539));
#46668=CARTESIAN_POINT('Ctrl Pts',(-4.76331576341244,-2.51762144469383,
14.035670935878));
#46669=CARTESIAN_POINT('Ctrl Pts',(-0.480935569811807,-5.36621801443908,
14.1940605363021));
#46670=CARTESIAN_POINT('Ctrl Pts',(4.23972842232605,-3.32449961733459,14.3524501367262));
#46671=CARTESIAN_POINT('Ctrl Pts',(5.09666430962992,1.74688514666806,14.5108397371504));
#46672=CARTESIAN_POINT('Ctrl Pts',(1.30893356445067,5.22630727424813,14.6692293375744));
#46673=CARTESIAN_POINT('Ctrl Pts',(-3.67164797130143,3.94291719103216,14.8276189379986));
#46674=CARTESIAN_POINT('Ctrl Pts',(-5.30620163810439,-0.933712469786478,
14.9860085384227));
#46675=CARTESIAN_POINT('Ctrl Pts',(-2.10513416208848,-4.95943595200104,
15.1443981388468));
#46676=CARTESIAN_POINT('Ctrl Pts',(3.01437365178127,-4.46555106184718,15.3027877392709));
#46677=CARTESIAN_POINT('Ctrl Pts',(5.38683754266046,0.0978574907256861,
15.461177339695));
#46678=CARTESIAN_POINT('Ctrl Pts',(2.85019558172777,4.57208704614299,15.6195669401191));
#46679=CARTESIAN_POINT('Ctrl Pts',(-2.28387236489903,4.87970509392274,15.7779565405432));
#46680=CARTESIAN_POINT('Ctrl Pts',(-5.33661316720418,0.740374703881965,
15.9363461409674));
#46681=CARTESIAN_POINT('Ctrl Pts',(-3.5260183466427,-4.07367027264334,16.0947357413914));
#46682=CARTESIAN_POINT('Ctrl Pts',(1.49788988655441,-5.17531840086943,16.2531253418156));
#46683=CARTESIAN_POINT('Ctrl Pts',(5.15674858900573,-1.56062129330084,16.4115149422397));
#46684=CARTESIAN_POINT('Ctrl Pts',(4.11618497232175,3.47629350252734,16.5699045426638));
#46685=CARTESIAN_POINT('Ctrl Pts',(-0.675519785260975,5.34520970499122,
16.7282941430879));
#46686=CARTESIAN_POINT('Ctrl Pts',(-4.85161316293496,2.34295647615374,16.886683743512));
#46687=CARTESIAN_POINT('Ctrl Pts',(-4.60635882216303,-2.79446879777952,
17.0450733439361));
#46688=CARTESIAN_POINT('Ctrl Pts',(-0.16326034841019,-5.385251468869,17.2034629443603));
#46689=CARTESIAN_POINT('Ctrl Pts',(4.42861926027611,-3.06837613225715,17.3618525447843));
#46690=CARTESIAN_POINT('Ctrl Pts',(4.98463260760038,2.04476104631356,17.5202421452085));
#46691=CARTESIAN_POINT('Ctrl Pts',(0.998073777402168,5.29446792596388,17.6786317456326));
#46692=CARTESIAN_POINT('Ctrl Pts',(-3.89804137708339,3.71926376057284,17.8370213460567));
#46693=CARTESIAN_POINT('Ctrl Pts',(-5.24181922596764,-1.24539373721259,
17.9954109464808));
#46694=CARTESIAN_POINT('Ctrl Pts',(-1.8086366036207,-5.07504314756533,18.1538005469049));
#46695=CARTESIAN_POINT('Ctrl Pts',(3.27276076949422,-4.27984832373426,18.312190147329));
#46696=CARTESIAN_POINT('Ctrl Pts',(5.37168597078491,0.415863414893554,18.4705797477531));
#46697=CARTESIAN_POINT('Ctrl Pts',(2.57522942679949,4.73215872598774,18.6289693481773));
#46698=CARTESIAN_POINT('Ctrl Pts',(-2.56791221710864,4.73679627703356,18.7873589486013));
#46699=CARTESIAN_POINT('Ctrl Pts',(-5.371183010352,0.423134275550087,18.9457485490255));
#46700=CARTESIAN_POINT('Ctrl Pts',(-3.27902910214792,-4.27310129927592,
19.1041381494496));
#46701=CARTESIAN_POINT('Ctrl Pts',(1.80023534169657,-5.08102363891602,19.2625277498737));
#46702=CARTESIAN_POINT('Ctrl Pts',(5.24104970544042,-1.24716092356801,19.4209173502978));
#46703=CARTESIAN_POINT('Ctrl Pts',(4.12486056868766,2.87503833462901,19.5529086839846));
#46704=CARTESIAN_POINT('Ctrl Pts',(1.45532996524397,4.51808130074211,19.658501750934));
#46705=CARTESIAN_POINT('Ctrl Pts',(-0.0944239912043199,4.62336330695642,
19.7112982844087));
#46706=CARTESIAN_POINT('Ctrl Pts',(-0.838218623839749,4.48433200584526,
19.737696551146));
#46707=CARTESIAN_POINT('Ctrl Pts',(-2.08577545033744,4.26978275451687,-0.109696551146029));
#46708=CARTESIAN_POINT('Ctrl Pts',(-2.79398382812688,3.92382518874754,-0.0832982844086765));
#46709=CARTESIAN_POINT('Ctrl Pts',(-4.02416310842503,2.87280371482855,-0.0305017509339729));
#46710=CARTESIAN_POINT('Ctrl Pts',(-5.23492737076948,-0.159612942608633,
0.0750913160154349));
#46711=CARTESIAN_POINT('Ctrl Pts',(-3.60656294430474,-4.29937997811031,
0.207082649702195));
#46712=CARTESIAN_POINT('Ctrl Pts',(1.65230512354554,-5.36640927368603,0.365472250126306));
#46713=CARTESIAN_POINT('Ctrl Pts',(5.39655442416041,-1.53476669476806,0.523861850550419));
#46714=CARTESIAN_POINT('Ctrl Pts',(4.22739879570491,3.69135413573996,0.68225145097453));
#46715=CARTESIAN_POINT('Ctrl Pts',(-0.796623825861737,5.55566232761052,
0.840641051398642));
#46716=CARTESIAN_POINT('Ctrl Pts',(-5.09342976711741,2.35587634873282,0.999030651822753));
#46717=CARTESIAN_POINT('Ctrl Pts',(-4.74916603463757,-2.99026113323004,
1.15742025224687));
#46718=CARTESIAN_POINT('Ctrl Pts',(-0.0765764492562429,-5.61163946058846,
1.31580985267098));
#46719=CARTESIAN_POINT('Ctrl Pts',(4.66562076004983,-3.11888407290359,1.47419945309509));
#46720=CARTESIAN_POINT('Ctrl Pts',(5.15606071062936,2.21607214970721,1.6325890535192));
#46721=CARTESIAN_POINT('Ctrl Pts',(0.947656591981422,5.53153304554248,1.79097865394331));
#46722=CARTESIAN_POINT('Ctrl Pts',(-4.12433576856007,3.80600164922439,1.94936825436742));
#46723=CARTESIAN_POINT('Ctrl Pts',(-5.43777237967215,-1.38798397218498,
2.10775785479154));
#46724=CARTESIAN_POINT('Ctrl Pts',(-1.79567850106425,-5.31708534443909,
2.26614745521565));
#46725=CARTESIAN_POINT('Ctrl Pts',(3.482840490886,-4.4006437602611,2.42453705563976));
#46726=CARTESIAN_POINT('Ctrl Pts',(5.58739660624356,0.526168748650917,2.58292665606387));
#46727=CARTESIAN_POINT('Ctrl Pts',(2.60007339085155,4.97347669546753,2.74131625648798));
#46728=CARTESIAN_POINT('Ctrl Pts',(-2.75673518447264,4.88838025390829,2.8997058569121));
#46729=CARTESIAN_POINT('Ctrl Pts',(-5.60128990911765,0.348429813187091,
3.05809545733621));
#46730=CARTESIAN_POINT('Ctrl Pts',(-3.34130498085651,-4.50905007289915,
3.21648505776032));
#46731=CARTESIAN_POINT('Ctrl Pts',(1.9636612196335,-5.25736492612739,3.37487465818443));
#46732=CARTESIAN_POINT('Ctrl Pts',(5.47911353583714,-1.21456430029784,3.53326425860854));
#46733=CARTESIAN_POINT('Ctrl Pts',(4.00136748278709,3.93508700883766,3.69165385903265));
#46734=CARTESIAN_POINT('Ctrl Pts',(-1.12288476494156,5.49863449294768,3.85004345945677));
#46735=CARTESIAN_POINT('Ctrl Pts',(-5.22383528931343,2.05119389228533,4.00843305988088));
#46736=CARTESIAN_POINT('Ctrl Pts',(-4.56422635699607,-3.26553047185241,
4.16682266030499));
#46737=CARTESIAN_POINT('Ctrl Pts',(0.254830513777376,-5.6063279344566,4.3252122607291));
#46738=CARTESIAN_POINT('Ctrl Pts',(4.84165651582845,-2.8379946593256,4.48360186115322));
#46739=CARTESIAN_POINT('Ctrl Pts',(5.01620831243703,2.51664571756971,4.64199146157732));
#46740=CARTESIAN_POINT('Ctrl Pts',(0.619414233810315,5.57782910356021,4.80038106200144));
#46741=CARTESIAN_POINT('Ctrl Pts',(-4.34186132707045,3.55585316325194,4.95877066242554));
#46742=CARTESIAN_POINT('Ctrl Pts',(-5.34633353503125,-1.70662510059887,
5.11716026284966));
#46743=CARTESIAN_POINT('Ctrl Pts',(-1.47861180052498,-5.41383031181963,
5.27554986327377));
#46744=CARTESIAN_POINT('Ctrl Pts',(3.73659104616929,-4.18733075545571,5.43393946369789));
#46745=CARTESIAN_POINT('Ctrl Pts',(5.54658242569702,0.855146125991221,5.59232906412199));
#46746=CARTESIAN_POINT('Ctrl Pts',(2.30189004504538,5.11831551610282,5.75071866454611));
#46747=CARTESIAN_POINT('Ctrl Pts',(-3.04054926072666,4.71708720451092,5.90910826497022));
#46748=CARTESIAN_POINT('Ctrl Pts',(-5.61209041865238,0.0171065697671163,
6.06749786539433));
#46749=CARTESIAN_POINT('Ctrl Pts',(-3.06924939983126,-4.69846353859389,
6.22588746581845));
#46750=CARTESIAN_POINT('Ctrl Pts',(2.27064463408739,-5.13225334989921,6.38427706624255));
#46751=CARTESIAN_POINT('Ctrl Pts',(5.5412661545576,-0.888943702500394,6.54266666666667));
#46752=CARTESIAN_POINT('Ctrl Pts',(3.76204871247451,4.16447367464723,6.70105626709077));
#46753=CARTESIAN_POINT('Ctrl Pts',(-1.44558014992134,5.42274372730397,6.85944586751489));
#46754=CARTESIAN_POINT('Ctrl Pts',(-5.33583013879699,1.73918608313389,7.017835467939));
#46755=CARTESIAN_POINT('Ctrl Pts',(-4.36345808770768,-3.52931792541838,
7.17622506836312));
#46756=CARTESIAN_POINT('Ctrl Pts',(0.585398768149902,-5.58150157073431,
7.33461466878722));
#46757=CARTESIAN_POINT('Ctrl Pts',(5.00077294593711,-2.54717911522619,7.49300426921134));
#46758=CARTESIAN_POINT('Ctrl Pts',(4.85886772928377,2.80842587425515,7.65139386963545));
#46759=CARTESIAN_POINT('Ctrl Pts',(0.289003470625252,5.60467023970434,7.80978347005956));
#46760=CARTESIAN_POINT('Ctrl Pts',(-4.54423398570509,3.29329454877997,7.96817307048368));
#46761=CARTESIAN_POINT('Ctrl Pts',(-5.23624284988438,-2.01930986203101,
8.12656267090778));
#46762=CARTESIAN_POINT('Ctrl Pts',(-1.15638506423861,-5.49168690705022,
8.2849522713319));
#46763=CARTESIAN_POINT('Ctrl Pts',(3.97730377557951,-3.9594073014306,8.44334187175601));
#46764=CARTESIAN_POINT('Ctrl Pts',(5.48641602737129,1.1811395668863,8.60173147218012));
#46765=CARTESIAN_POINT('Ctrl Pts',(1.99567506023593,5.24529623146426,8.76012107260423));
#46766=CARTESIAN_POINT('Ctrl Pts',(-3.31375452330647,4.52933576378778,8.91851067302835));
#46767=CARTESIAN_POINT('Ctrl Pts',(-5.60330990528806,-0.314276322941499,
9.07690027345245));
#46768=CARTESIAN_POINT('Ctrl Pts',(-2.78648492405391,-4.87148368260443,
9.23528987387657));
#46769=CARTESIAN_POINT('Ctrl Pts',(2.56970556419197,-4.98923489276881,9.39367947430067));
#46770=CARTESIAN_POINT('Ctrl Pts',(5.58408482763794,-0.560221509409272,
9.5520690747248));
#46771=CARTESIAN_POINT('Ctrl Pts',(3.50960382949614,4.37933013848544,9.7104586751489));
#46772=CARTESIAN_POINT('Ctrl Pts',(-1.76323178056758,5.32793254366621,9.86884827557301));
#46773=CARTESIAN_POINT('Ctrl Pts',(-5.42920782150573,1.4211101057842,10.0272378759971));
#46774=CARTESIAN_POINT('Ctrl Pts',(-4.14746533961321,-3.78079128735878,
10.1856274764213));
#46775=CARTESIAN_POINT('Ctrl Pts',(0.913924515938199,-5.53720087056882,
10.3440170768453));
#46776=CARTESIAN_POINT('Ctrl Pts',(5.14244125175658,-2.24747624550143,10.5024066772695));
#46777=CARTESIAN_POINT('Ctrl Pts',(4.68457414109547,3.09040719298293,10.6607962776936));
#46778=CARTESIAN_POINT('Ctrl Pts',(-0.0424156503481004,5.61195620211585,
10.8191858781177));
#46779=CARTESIAN_POINT('Ctrl Pts',(-4.73075142341831,3.01924534804421,10.9775754785418));
#46780=CARTESIAN_POINT('Ctrl Pts',(-5.10788246569177,-2.32494907869821,
11.1359650789659));
#46781=CARTESIAN_POINT('Ctrl Pts',(-0.83012360158913,-5.55038253708208,
11.29435467939));
#46782=CARTESIAN_POINT('Ctrl Pts',(4.20413935203321,-3.71766913677734,11.4527442798141));
#46783=CARTESIAN_POINT('Ctrl Pts',(5.4071070543997,1.50301191083837,11.6111338802383));
#46784=CARTESIAN_POINT('Ctrl Pts',(1.68249699449844,5.35397565976581,11.7695234806624));
#46785=CARTESIAN_POINT('Ctrl Pts',(-3.57539781300678,4.32578108329668,11.9279130810865));
#46786=CARTESIAN_POINT('Ctrl Pts',(-5.57497896454372,-0.644562678686908,
12.0863026815106));
#46787=CARTESIAN_POINT('Ctrl Pts',(-2.49399816411355,-5.02750680350203,
12.2446922819347));
#46788=CARTESIAN_POINT('Ctrl Pts',(2.85980057185626,-4.82880856848474,12.4030818823588));
#46789=CARTESIAN_POINT('Ctrl Pts',(5.60742015127818,-0.229544655569092,
12.5614714827829));
#46790=CARTESIAN_POINT('Ctrl Pts',(3.24491363866216,4.57890674500859,12.719861083207));
#46791=CARTESIAN_POINT('Ctrl Pts',(-2.07473134476337,5.2145317478099,12.8782506836311));
#46792=CARTESIAN_POINT('Ctrl Pts',(-5.50364253389182,1.09807575376104,13.0366402840552));
#46793=CARTESIAN_POINT('Ctrl Pts',(-3.91700173031292,-4.01907314521474,
13.1950298844794));
#46794=CARTESIAN_POINT('Ctrl Pts',(1.23926150294374,-5.47358040309844,13.3534194849035));
#46795=CARTESIAN_POINT('Ctrl Pts',(5.26616714033573,-1.93993173898181,13.5118090853276));
#46796=CARTESIAN_POINT('Ctrl Pts',(4.49393567316656,3.36160581676376,13.6701986857517));
#46797=CARTESIAN_POINT('Ctrl Pts',(-0.37368677949048,5.59966156947901,13.8285882861758));
#46798=CARTESIAN_POINT('Ctrl Pts',(-4.90076286490465,2.73466174212266,13.9869778865999));
#46799=CARTESIAN_POINT('Ctrl Pts',(-4.96170024281806,-2.6224763492295,14.1453674870241));
#46800=CARTESIAN_POINT('Ctrl Pts',(-0.500965766713239,-5.58971240785062,
14.3037570874481));
#46801=CARTESIAN_POINT('Ctrl Pts',(4.41630632680696,-3.46295970661421,14.4621466878723));
#46802=CARTESIAN_POINT('Ctrl Pts',(5.30893222256936,1.81964011770419,14.6205362882964));
#46803=CARTESIAN_POINT('Ctrl Pts',(1.36344855288682,5.44397460921243,14.7789258887205));
#46804=CARTESIAN_POINT('Ctrl Pts',(-3.8245662340255,4.10713338267972,14.9373154891446));
#46805=CARTESIAN_POINT('Ctrl Pts',(-5.52719644547832,-0.972600100049373,
15.0957050895687));
#46806=CARTESIAN_POINT('Ctrl Pts',(-2.19280963135567,-5.16598852343466,
15.2540946899928));
#46807=CARTESIAN_POINT('Ctrl Pts',(3.1399174908515,-4.65153411790834,15.4124842904169));
#46808=CARTESIAN_POINT('Ctrl Pts',(5.61119070642755,0.101933098625243,15.570873890841));
#46809=CARTESIAN_POINT('Ctrl Pts',(2.96890166689401,4.76250715547379,15.7292634912652));
#46810=CARTESIAN_POINT('Ctrl Pts',(-2.37899199430077,5.08293700270077,15.8876530916893));
#46811=CARTESIAN_POINT('Ctrl Pts',(-5.55887456610132,0.77121012556931,16.0460426921134));
#46812=CARTESIAN_POINT('Ctrl Pts',(-3.6728713685327,-4.24333212091212,16.2044322925375));
#46813=CARTESIAN_POINT('Ctrl Pts',(1.56027460344289,-5.39086213084865,16.3628218929616));
#46814=CARTESIAN_POINT('Ctrl Pts',(5.37151891603578,-1.6256186728991,16.5212114933857));
#46815=CARTESIAN_POINT('Ctrl Pts',(4.28761748980119,3.62107556422837,16.6796010938098));
#46816=CARTESIAN_POINT('Ctrl Pts',(-0.703654103366955,5.56782913593124,
16.837990694234));
#46817=CARTESIAN_POINT('Ctrl Pts',(-5.05367508773934,2.44053686424434,16.996380294658));
#46818=CARTESIAN_POINT('Ctrl Pts',(-4.79820629612424,-2.91085395156691,
17.1547698950822));
#46819=CARTESIAN_POINT('Ctrl Pts',(-0.170059880676311,-5.60953857520067,
17.3131594955063));
#46820=CARTESIAN_POINT('Ctrl Pts',(4.61306416589918,-3.1961690882258,17.4715490959304));
#46821=CARTESIAN_POINT('Ctrl Pts',(5.19223457942065,2.12992207191625,17.6299386963545));
#46822=CARTESIAN_POINT('Ctrl Pts',(1.03964195313792,5.51497404300314,17.7883282967786));
#46823=CARTESIAN_POINT('Ctrl Pts',(-4.06038856288912,3.87416514472648,17.9467178972027));
#46824=CARTESIAN_POINT('Ctrl Pts',(-5.46013260889923,-1.2972623935191,18.1051074976268));
#46825=CARTESIAN_POINT('Ctrl Pts',(-1.88396342402579,-5.28641057370242,
18.263497098051));
#46826=CARTESIAN_POINT('Ctrl Pts',(3.40906601855249,-4.45809715790996,18.421886698475));
#46827=CARTESIAN_POINT('Ctrl Pts',(5.59540809582856,0.433183460669457,18.5802762988992));
#46828=CARTESIAN_POINT('Ctrl Pts',(2.68248361160703,4.92924556464132,18.7386658993233));
#46829=CARTESIAN_POINT('Ctrl Pts',(-2.67486165184133,4.93407626226733,18.8970554997474));
#46830=CARTESIAN_POINT('Ctrl Pts',(-5.59488418789844,0.440757141037727,
19.0554451001715));
#46831=CARTESIAN_POINT('Ctrl Pts',(-3.41559541723082,-4.45106913067933,
19.2138347005956));
#46832=CARTESIAN_POINT('Ctrl Pts',(1.87521226298597,-5.29264014294805,19.3722243010197));
#46833=CARTESIAN_POINT('Ctrl Pts',(5.4593310390734,-1.29910318035845,19.5306139014438));
#46834=CARTESIAN_POINT('Ctrl Pts',(4.29665441087326,2.99477908070078,19.6626052351306));
#46835=CARTESIAN_POINT('Ctrl Pts',(1.51594212951325,4.70625215719564,19.76819830208));
#46836=CARTESIAN_POINT('Ctrl Pts',(-0.098356599343019,4.8159189904991,19.8209948355547));
#46837=CARTESIAN_POINT('Ctrl Pts',(-0.873129088225867,4.67109725817113,
19.8473931022921));
#46838=CARTESIAN_POINT('Ctrl Pts',(-2.1691713542861,4.440502182833,2.77555756156289E-16));
#46839=CARTESIAN_POINT('Ctrl Pts',(-2.90569614448715,4.08071213863434,0.0263982667373523));
#46840=CARTESIAN_POINT('Ctrl Pts',(-4.18506188590834,2.9876674997228,0.079194800212056));
#46841=CARTESIAN_POINT('Ctrl Pts',(-5.44423633550983,-0.165994773226382,
0.184787867161464));
#46842=CARTESIAN_POINT('Ctrl Pts',(-3.75076474552906,-4.4712827971004,0.316779200848224));
#46843=CARTESIAN_POINT('Ctrl Pts',(1.71836951190277,-5.58097530104301,0.475168801272335));
#46844=CARTESIAN_POINT('Ctrl Pts',(5.61232575004223,-1.59613152473566,0.633558401696447));
#46845=CARTESIAN_POINT('Ctrl Pts',(4.39642357920323,3.83894615716052,0.79194800212056));
#46846=CARTESIAN_POINT('Ctrl Pts',(-0.828475367720669,5.77779529104613,
0.95033760254467));
#46847=CARTESIAN_POINT('Ctrl Pts',(-5.29708120982622,2.45007174146416,1.10872720296878));
#46848=CARTESIAN_POINT('Ctrl Pts',(-4.93905272373294,-3.10982123746271,
1.26711680339289));
#46849=CARTESIAN_POINT('Ctrl Pts',(-0.0796382180607007,-5.83601056696721,
1.42550640381701));
#46850=CARTESIAN_POINT('Ctrl Pts',(4.85216704464777,-3.24358692935388,1.58389600424112));
#46851=CARTESIAN_POINT('Ctrl Pts',(5.36221633668567,2.30467772808354,1.74228560466523));
#46852=CARTESIAN_POINT('Ctrl Pts',(0.985546901846022,5.75270124391223,1.90067520508934));
#46853=CARTESIAN_POINT('Ctrl Pts',(-4.28923976604036,3.95817764109155,2.05906480551345));
#46854=CARTESIAN_POINT('Ctrl Pts',(-5.65519172986948,-1.44347996433883,
2.21745440593756));
#46855=CARTESIAN_POINT('Ctrl Pts',(-1.86747541082905,-5.52967924499536,
2.37584400636168));
#46856=CARTESIAN_POINT('Ctrl Pts',(3.62209547684312,-4.57659542575977,2.53423360678579));
#46857=CARTESIAN_POINT('Ctrl Pts',(5.81079840657738,0.547206640537195,2.6926232072099));
#46858=CARTESIAN_POINT('Ctrl Pts',(2.70403255420632,5.17233203472232,2.85101280763401));
#46859=CARTESIAN_POINT('Ctrl Pts',(-2.86695818216828,5.08383316810077,3.00940240805812));
#46860=CARTESIAN_POINT('Ctrl Pts',(-5.82524720767244,0.362361139892822,
3.16779200848224));
#46861=CARTESIAN_POINT('Ctrl Pts',(-3.47490092916519,-4.68933616588121,
3.32618160890635));
#46862=CARTESIAN_POINT('Ctrl Pts',(2.04217461014913,-5.46757101534546,3.48457120933046));
#46863=CARTESIAN_POINT('Ctrl Pts',(5.698185836302,-1.26312642509933,3.64296080975457));
#46864=CARTESIAN_POINT('Ctrl Pts',(4.16135481900965,4.09242424193511,3.80135041017868));
#46865=CARTESIAN_POINT('Ctrl Pts',(-1.16778125175528,5.71848730306133,3.95974001060279));
#46866=CARTESIAN_POINT('Ctrl Pts',(-5.43270075753092,2.13320711609306,4.11812961102691));
#46867=CARTESIAN_POINT('Ctrl Pts',(-4.74671857244836,-3.39609671546603,
4.27651921145102));
#46868=CARTESIAN_POINT('Ctrl Pts',(0.265019444252462,-5.8304866692097,4.43490881187513));
#46869=CARTESIAN_POINT('Ctrl Pts',(5.03524126709262,-2.95146666801078,4.59329841229924));
#46870=CARTESIAN_POINT('Ctrl Pts',(5.21677219698313,2.61726917849946,4.75168801272335));
#46871=CARTESIAN_POINT('Ctrl Pts',(0.644180375313696,5.80084836485576,4.91007761314747));
#46872=CARTESIAN_POINT('Ctrl Pts',(-4.51546268484472,3.69802742693416,5.06846721357158));
#46873=CARTESIAN_POINT('Ctrl Pts',(-5.56009687081743,-1.77486137356051,
5.22685681399569));
#46874=CARTESIAN_POINT('Ctrl Pts',(-1.53773138009144,-5.63029238236797,
5.3852464144198));
#46875=CARTESIAN_POINT('Ctrl Pts',(3.88599178244287,-4.35475349189019,5.54363601484391));
#46876=CARTESIAN_POINT('Ctrl Pts',(5.7683523459164,0.889337574631424,5.70202561526803));
#46877=CARTESIAN_POINT('Ctrl Pts',(2.39392689448955,5.32296196981904,5.86041521569214));
#46878=CARTESIAN_POINT('Ctrl Pts',(-3.16212004345771,4.90569128044887,6.01880481611624));
#46879=CARTESIAN_POINT('Ctrl Pts',(-5.8364795557618,0.0177905445684291,
6.17719441654037));
#46880=CARTESIAN_POINT('Ctrl Pts',(-3.19196770495921,-4.88632298142486,
6.33558401696446));
#46881=CARTESIAN_POINT('Ctrl Pts',(2.36143219311022,-5.33745708232365,6.49397361738859));
#46882=CARTESIAN_POINT('Ctrl Pts',(5.7628235134309,-0.924486485218232,6.65236321781269));
#46883=CARTESIAN_POINT('Ctrl Pts',(3.9124673268201,4.33098251264868,6.81075281823681));
#46884=CARTESIAN_POINT('Ctrl Pts',(-1.50337901955202,5.63956218441419,6.96914241866092));
#46885=CARTESIAN_POINT('Ctrl Pts',(-5.54917351555865,1.80872424723227,7.12753201908502));
#46886=CARTESIAN_POINT('Ctrl Pts',(-4.53792295232564,-3.6704312263084,7.28592161950915));
#46887=CARTESIAN_POINT('Ctrl Pts',(0.60880486367776,-5.80466766889078,7.44431121993324));
#46888=CARTESIAN_POINT('Ctrl Pts',(5.20071967567786,-2.64902339803196,7.60270082035738));
#46889=CARTESIAN_POINT('Ctrl Pts',(5.0531406393351,2.92071562932846,7.76109042078146));
#46890=CARTESIAN_POINT('Ctrl Pts',(0.300558744071995,5.82876269457468,7.9194800212056));
#46891=CARTESIAN_POINT('Ctrl Pts',(-4.72592684287763,3.42497088806201,8.07786962162969));
#46892=CARTESIAN_POINT('Ctrl Pts',(-5.44560441164323,-2.10004826139671,
8.23625922205382));
#46893=CARTESIAN_POINT('Ctrl Pts',(-1.20262099904615,-5.7112619306907,8.39464882247792));
#46894=CARTESIAN_POINT('Ctrl Pts',(4.13632896862666,-4.11771693679927,8.55303842290205));
#46895=CARTESIAN_POINT('Ctrl Pts',(5.70578030455996,1.22836526505724,8.71142802332614));
#46896=CARTESIAN_POINT('Ctrl Pts',(2.07546846542215,5.45501977607246,8.86981762375027));
#46897=CARTESIAN_POINT('Ctrl Pts',(-3.44624891712552,4.71043294289546,9.02820722417436));
#46898=CARTESIAN_POINT('Ctrl Pts',(-5.827347969683,-0.32684208501195,9.18659682459849));
#46899=CARTESIAN_POINT('Ctrl Pts',(-2.89789741049547,-5.06626101839879,
9.3449864250226));
#46900=CARTESIAN_POINT('Ctrl Pts',(2.6724505257232,-5.18872029462616,9.50337602544671));
#46901=CARTESIAN_POINT('Ctrl Pts',(5.80735421258137,-0.582620938447121,
9.66176562587082));
#46902=CARTESIAN_POINT('Ctrl Pts',(3.64992889843646,4.55442961792825,9.82015522629493));
#46903=CARTESIAN_POINT('Ctrl Pts',(-1.83373136775356,5.54096014957879,9.97854482671904));
#46904=CARTESIAN_POINT('Ctrl Pts',(-5.64628473356088,1.47793058560304,10.1369344271431));
#46905=CARTESIAN_POINT('Ctrl Pts',(-4.31329413054894,-3.93195928916814,
10.2953240275673));
#46906=CARTESIAN_POINT('Ctrl Pts',(0.950466110641093,-5.7585956865217,10.4537136279914));
#46907=CARTESIAN_POINT('Ctrl Pts',(5.34805232874179,-2.33733745902108,10.6121032284155));
#46908=CARTESIAN_POINT('Ctrl Pts',(4.87187824185477,3.2139714536451,10.7704928288396));
#46909=CARTESIAN_POINT('Ctrl Pts',(-0.0441115622938141,5.83633997282335,
10.9288824292637));
#46910=CARTESIAN_POINT('Ctrl Pts',(-4.91990183807518,3.13996433291973,11.0872720296878));
#46911=CARTESIAN_POINT('Ctrl Pts',(-5.31211177303214,-2.41790790128923,
11.2456616301119));
#46912=CARTESIAN_POINT('Ctrl Pts',(-0.863314570507911,-5.77230439778191,
11.404051230536));
#46913=CARTESIAN_POINT('Ctrl Pts',(4.37223414935776,-3.86631331522594,11.5624408309602));
#46914=CARTESIAN_POINT('Ctrl Pts',(5.6233003078374,1.56310708404107,11.7208304313843));
#46915=CARTESIAN_POINT('Ctrl Pts',(1.74976854941316,5.56804455188607,11.8792200318084));
#46916=CARTESIAN_POINT('Ctrl Pts',(-3.71835353364465,4.4987395020312,12.0376096322325));
#46917=CARTESIAN_POINT('Ctrl Pts',(-5.79788426826075,-0.670334334610817,
12.1959992326566));
#46918=CARTESIAN_POINT('Ctrl Pts',(-2.59371610417703,-5.22852243748043,
12.3543888330807));
#46919=CARTESIAN_POINT('Ctrl Pts',(2.97414444993972,-5.0218796181506,12.5127784335049));
#46920=CARTESIAN_POINT('Ctrl Pts',(5.83162255631666,-0.238722577403733,
12.6711680339289));
#46921=CARTESIAN_POINT('Ctrl Pts',(3.37465555603293,4.76198592883678,12.8295576343531));
#46922=CARTESIAN_POINT('Ctrl Pts',(-2.15768567041678,5.42302523099255,12.9879472347772));
#46923=CARTESIAN_POINT('Ctrl Pts',(-5.72369558133277,1.1419802977877,13.1463368352013));
#46924=CARTESIAN_POINT('Ctrl Pts',(-4.07361585673539,-4.17976840985925,
13.3047264356254));
#46925=CARTESIAN_POINT('Ctrl Pts',(1.28881110007321,-5.69243147140415,13.4631160360495));
#46926=CARTESIAN_POINT('Ctrl Pts',(5.47672516993668,-2.01749634975762,13.6215056364736));
#46927=CARTESIAN_POINT('Ctrl Pts',(4.67361744461052,3.49601345674377,13.7798952368977));
#46928=CARTESIAN_POINT('Ctrl Pts',(-0.388627959646856,5.82355376186139,
13.9382848373218));
#46929=CARTESIAN_POINT('Ctrl Pts',(-5.09671087507549,2.84400217373111,14.096674437746));
#46930=CARTESIAN_POINT('Ctrl Pts',(-5.16008472222368,-2.72733125376517,
14.2550640381701));
#46931=CARTESIAN_POINT('Ctrl Pts',(-0.520995963614669,-5.81320680126216,
14.4134536385942));
#46932=CARTESIAN_POINT('Ctrl Pts',(4.59288423128786,-3.60141979589384,14.5718432390183));
#46933=CARTESIAN_POINT('Ctrl Pts',(5.5212001355088,1.89239508874033,14.7302328394424));
#46934=CARTESIAN_POINT('Ctrl Pts',(1.41796354132297,5.66164194417672,14.8886224398665));
#46935=CARTESIAN_POINT('Ctrl Pts',(-3.97748449674956,4.27134957432729,15.0470120402906));
#46936=CARTESIAN_POINT('Ctrl Pts',(-5.74819125285225,-1.01148773031227,
15.2054016407147));
#46937=CARTESIAN_POINT('Ctrl Pts',(-2.28048510062285,-5.37254109486827,
15.3637912411389));
#46938=CARTESIAN_POINT('Ctrl Pts',(3.26546132992172,-4.8375171739695,15.5221808415629));
#46939=CARTESIAN_POINT('Ctrl Pts',(5.83554387019465,0.106008706524804,15.6805704419871));
#46940=CARTESIAN_POINT('Ctrl Pts',(3.08760775206024,4.95292726480458,15.8389600424112));
#46941=CARTESIAN_POINT('Ctrl Pts',(-2.4741116237025,5.2861689114788,15.9973496428353));
#46942=CARTESIAN_POINT('Ctrl Pts',(-5.78113596499847,0.802045547256652,
16.1557392432594));
#46943=CARTESIAN_POINT('Ctrl Pts',(-3.81972439042269,-4.4129939691809,16.3141288436835));
#46944=CARTESIAN_POINT('Ctrl Pts',(1.62265932033137,-5.60640586082788,16.4725184441076));
#46945=CARTESIAN_POINT('Ctrl Pts',(5.58628924306583,-1.69061605249735,16.6309080445317));
#46946=CARTESIAN_POINT('Ctrl Pts',(4.45905000728063,3.76585762592941,16.7892976449558));
#46947=CARTESIAN_POINT('Ctrl Pts',(-0.731788421472935,5.79044856687125,
16.94768724538));
#46948=CARTESIAN_POINT('Ctrl Pts',(-5.25573701254373,2.53811725233494,17.106076845804));
#46949=CARTESIAN_POINT('Ctrl Pts',(-4.99005377008544,-3.02723910535429,
17.2644664462282));
#46950=CARTESIAN_POINT('Ctrl Pts',(-0.176859412942431,-5.83382568153235,
17.4228560466523));
#46951=CARTESIAN_POINT('Ctrl Pts',(4.79750907152224,-3.32396204419444,17.5812456470764));
#46952=CARTESIAN_POINT('Ctrl Pts',(5.39983655124094,2.21508309751895,17.7396352475005));
#46953=CARTESIAN_POINT('Ctrl Pts',(1.08121012887367,5.73548016004241,17.8980248479246));
#46954=CARTESIAN_POINT('Ctrl Pts',(-4.22273574869486,4.02906652888012,18.0564144483487));
#46955=CARTESIAN_POINT('Ctrl Pts',(-5.67844599183081,-1.34913104982561,
18.2148040487729));
#46956=CARTESIAN_POINT('Ctrl Pts',(-1.95929024443088,-5.4977779998395,18.373193649197));
#46957=CARTESIAN_POINT('Ctrl Pts',(3.54537126761076,-4.63634599208567,18.5315832496211));
#46958=CARTESIAN_POINT('Ctrl Pts',(5.81913022087222,0.450503506445362,18.6899728500452));
#46959=CARTESIAN_POINT('Ctrl Pts',(2.78973779641457,5.12633240329489,18.8483624504693));
#46960=CARTESIAN_POINT('Ctrl Pts',(-2.78181108657403,5.13135624750109,19.0067520508934));
#46961=CARTESIAN_POINT('Ctrl Pts',(-5.81858536544488,0.458380006525366,
19.1651416513175));
#46962=CARTESIAN_POINT('Ctrl Pts',(-3.55216173231372,-4.62903696208274,
19.3235312517416));
#46963=CARTESIAN_POINT('Ctrl Pts',(1.95018918427537,-5.50425664698007,19.4819208521657));
#46964=CARTESIAN_POINT('Ctrl Pts',(5.67761237270639,-1.3510454371489,19.6403104525899));
#46965=CARTESIAN_POINT('Ctrl Pts',(4.46844825305886,3.11451982677256,19.7723017862766));
#46966=CARTESIAN_POINT('Ctrl Pts',(1.57655429378253,4.89442301364916,19.877894853226));
#46967=CARTESIAN_POINT('Ctrl Pts',(-0.102289207481715,5.00847467404178,
19.9306913867007));
#46968=CARTESIAN_POINT('Ctrl Pts',(-0.908039552611985,4.857862510497,19.9570896534381));
#46969=CARTESIAN_POINT('Ctrl Pts',(-4.94192999916445,-0.00446510791632448,
18.1776795453431));
#46970=CARTESIAN_POINT('Ctrl Pts',(-4.94542698461402,-0.388624254474772,
18.1900543798197));
#46971=CARTESIAN_POINT('Ctrl Pts',(-4.90438878928145,-0.772044124408378,
18.2024292142963));
#46972=CARTESIAN_POINT('Ctrl Pts',(-4.81596832674149,-1.14420594504366,
18.2148040487729));
#46973=CARTESIAN_POINT('Ctrl Pts',(-4.43872740936416,-2.73201336649694,
18.2676005822476));
#46974=CARTESIAN_POINT('Ctrl Pts',(-3.19900882689749,-4.11489568316824,
18.3203971157223));
#46975=CARTESIAN_POINT('Ctrl Pts',(-1.66170595032388,-4.66276484021157,
18.373193649197));
#46976=CARTESIAN_POINT('Ctrl Pts',(-0.124403073750308,-5.21063399725488,
18.4259901826717));
#46977=CARTESIAN_POINT('Ctrl Pts',(1.71048409693019,-4.92348999467027,18.4787867161464));
#46978=CARTESIAN_POINT('Ctrl Pts',(3.00688750781402,-3.93210974362283,18.5315832496211));
#46979=CARTESIAN_POINT('Ctrl Pts',(4.3032909186979,-2.94072949257537,18.5843797830958));
#46980=CARTESIAN_POINT('Ctrl Pts',(5.06121056978506,-1.24511299306501,18.6371763165705));
#46981=CARTESIAN_POINT('Ctrl Pts',(4.93527165791903,0.38200007283176,18.6899728500452));
#46982=CARTESIAN_POINT('Ctrl Pts',(4.80933274605301,2.00911313872853,18.7427693835199));
#46983=CARTESIAN_POINT('Ctrl Pts',(3.79953527123378,3.56772277101172,18.7955659169946));
#46984=CARTESIAN_POINT('Ctrl Pts',(2.36604505332606,4.34786489452101,18.8483624504693));
#46985=CARTESIAN_POINT('Ctrl Pts',(0.932554835418334,5.1280070180303,18.901158983944));
#46986=CARTESIAN_POINT('Ctrl Pts',(-0.92462812557789,5.12968163276569,18.9539555174187));
#46987=CARTESIAN_POINT('Ctrl Pts',(-2.35934865255447,4.3516895666374,19.0067520508934));
#46988=CARTESIAN_POINT('Ctrl Pts',(-2.82356148188028,4.09996535176783,19.0238347005956));
#46989=CARTESIAN_POINT('Ctrl Pts',(-3.24354728379133,3.7666188744385,19.0409173502978));
#46990=CARTESIAN_POINT('Ctrl Pts',(-3.60367707498796,3.37571982724537,19.058));
#46991=CARTESIAN_POINT('Ctrl Pts',(-2.54467524200881,-3.56229978442281,
-6.93889390390723E-18));
#46992=CARTESIAN_POINT('Ctrl Pts',(-2.64087676169121,-3.50326719695733,
3.78010404015323E-18));
#46993=CARTESIAN_POINT('Ctrl Pts',(-2.73444512499906,-3.44042480726573,
1.70774935809012E-16));
#46994=CARTESIAN_POINT('Ctrl Pts',(-2.82511133337028,-3.37382080685403,
1.33573707650214E-16));
#46995=CARTESIAN_POINT('Ctrl Pts',(-2.93010592262241,-3.29669108243516,
6.34680042936623E-17));
#46996=CARTESIAN_POINT('Ctrl Pts',(-3.0312098993845,-3.21451805045997,-1.1579302301566E-16));
#46997=CARTESIAN_POINT('Ctrl Pts',(-3.12833116102487,-3.1277186925041,-1.87350135405495E-16));
#46998=CARTESIAN_POINT('Ctrl Pts',(-3.19203631412683,-3.07078402861756,
-2.34286889761188E-16));
#46999=CARTESIAN_POINT('Ctrl Pts',(-3.25402740755314,-3.01185787186213,
2.54730009275007E-16));
#47000=CARTESIAN_POINT('Ctrl Pts',(-3.3142718238098,-2.95104792020956,3.67761376907083E-16));
#47001=CARTESIAN_POINT('Ctrl Pts',(-3.34056115234898,-2.92451180455305,
4.17085761531429E-16));
#47002=CARTESIAN_POINT('Ctrl Pts',(-3.36651779652415,-2.8976168731598,-1.29958168485043E-16));
#47003=CARTESIAN_POINT('Ctrl Pts',(-3.39213869657566,-2.87037166754254,
-1.66533453693773E-16));
#47004=CARTESIAN_POINT('Ctrl Pts',(-3.4107075535189,-2.85062558819017,-1.9304154815313E-16));
#47005=CARTESIAN_POINT('Ctrl Pts',(-3.42910165503002,-2.83069359301782,
5.20445990861309E-16));
#47006=CARTESIAN_POINT('Ctrl Pts',(-3.44730402197008,-2.81059669044114,
5.13478148889135E-16));
#47007=CARTESIAN_POINT('Ctrl Pts',(-3.53659117665104,-2.71201636542733,
4.79299144256909E-16));
#47008=CARTESIAN_POINT('Ctrl Pts',(-3.62135066124632,-2.60938482813861,
1.69265913904123E-16));
#47009=CARTESIAN_POINT('Ctrl Pts',(-3.70148784592851,-2.50313357384095,
1.80411241501588E-16));
#47010=CARTESIAN_POINT('Ctrl Pts',(-3.78346559823418,-2.39444197154017,
1.91812551751929E-16));
#47011=CARTESIAN_POINT('Ctrl Pts',(-3.86060678067413,-2.28196193869908,
-1.60403205534396E-16));
#47012=CARTESIAN_POINT('Ctrl Pts',(-3.93277586934314,-2.16611326123794,
-5.55111512312578E-17));
#47013=CARTESIAN_POINT('Ctrl Pts',(-3.96434984563583,-2.1154294648487,-9.62087747363501E-18));
#47014=CARTESIAN_POINT('Ctrl Pts',(-3.99497165206884,-2.06410040223293,
2.30246512287273E-16));
#47015=CARTESIAN_POINT('Ctrl Pts',(-4.02462756948077,-2.01215919201488,
2.91433543964104E-16));
#47016=CARTESIAN_POINT('Ctrl Pts',(-4.03961656660672,-1.98590653424469,
3.22359319390632E-16));
#47017=CARTESIAN_POINT('Ctrl Pts',(-4.05435879396083,-1.95949747991113,
2.06007824657555E-17));
#47018=CARTESIAN_POINT('Ctrl Pts',(-4.06885232846184,-1.93293620549746,
1.38777878078145E-17));
#47019=CARTESIAN_POINT('Ctrl Pts',(-4.08041475408644,-1.91174656677398,
8.51442211522865E-18));
#47020=CARTESIAN_POINT('Ctrl Pts',(-4.09181979945551,-1.89045816584063,
2.1634594979841E-16));
#47021=CARTESIAN_POINT('Ctrl Pts',(-4.10305617212226,-1.86909315496197,
2.08166817117217E-16));
#47022=CARTESIAN_POINT('Ctrl Pts',(-4.16736596175704,-1.74681353716178,
1.61354708109947E-16));
#47023=CARTESIAN_POINT('Ctrl Pts',(-4.22623125974132,-1.62188769970873,
-1.58091925840003E-16));
#47024=CARTESIAN_POINT('Ctrl Pts',(-4.27954887166761,-1.49476314498018,
-1.66533453693773E-16));
#47025=CARTESIAN_POINT('Ctrl Pts',(-4.33347479304113,-1.36618820519452,
-1.75071292334113E-16));
#47026=CARTESIAN_POINT('Ctrl Pts',(-4.38172617240059,-1.23536340764327,
-1.43714543602008E-16));
#47027=CARTESIAN_POINT('Ctrl Pts',(-4.42415678995003,-1.10271583109255,
-9.71445146547012E-17));
#47028=CARTESIAN_POINT('Ctrl Pts',(-4.46710218965978,-0.968458930662989,
-5.00094828511621E-17));
#47029=CARTESIAN_POINT('Ctrl Pts',(-4.50408524649974,-0.832334009558243,
-1.01069852635313E-16));
#47030=CARTESIAN_POINT('Ctrl Pts',(-4.53490679318661,-0.694758137572736,
-1.38777878078145E-16));
#47031=CARTESIAN_POINT('Ctrl Pts',(-4.55802295320176,-0.591576233583606,
-1.67058897160268E-16));
#47032=CARTESIAN_POINT('Ctrl Pts',(-4.5776723273625,-0.487577560717138,
-2.48733805589575E-17));
#47033=CARTESIAN_POINT('Ctrl Pts',(-4.59375100179198,-0.38293266212137,
-5.55111512312578E-17));
#47034=CARTESIAN_POINT('Ctrl Pts',(-4.60074932415958,-0.337385453754768,
-6.88463920640666E-17));
#47035=CARTESIAN_POINT('Ctrl Pts',(-4.60707095895173,-0.291715781756126,
-3.50051711561292E-16));
#47036=CARTESIAN_POINT('Ctrl Pts',(-4.61270623945594,-0.245937595982269,
-3.60822483003176E-16));
#47037=CARTESIAN_POINT('Ctrl Pts',(-4.61510536794149,-0.226448282287078,
-3.65407962742523E-16));
#47038=CARTESIAN_POINT('Ctrl Pts',(-4.61738026973089,-0.206937176747096,
-2.11235974110856E-16));
#47039=CARTESIAN_POINT('Ctrl Pts',(-4.61952832377542,-0.187423425576886,
-2.22044604925031E-16));
#47040=CARTESIAN_POINT('Ctrl Pts',(-4.63503826526744,-0.0465251368621273,
-3.00087907403534E-16));
#47041=CARTESIAN_POINT('Ctrl Pts',(-4.64396392467283,0.0947008669712182,
-1.99183435512137E-16));
#47042=CARTESIAN_POINT('Ctrl Pts',(-4.64615947496329,0.235825173850752,
-2.22044604925031E-16));
#47043=CARTESIAN_POINT('Ctrl Pts',(-4.64786848339456,0.345675825581053,
-2.39839656782873E-16));
#47044=CARTESIAN_POINT('Ctrl Pts',(-4.64549890174975,0.455465549450203,
-1.5964104232527E-16));
#47045=CARTESIAN_POINT('Ctrl Pts',(-4.63896138884064,0.56499930567962,-1.38777878078145E-16));
#47046=CARTESIAN_POINT('Ctrl Pts',(-4.63077575597687,0.702146738831947,
-1.08813479195783E-16));
#47047=CARTESIAN_POINT('Ctrl Pts',(-4.61605776615402,0.838893185885087,
-2.45094142526848E-16));
#47048=CARTESIAN_POINT('Ctrl Pts',(-4.59507497843275,0.974861012835041,
-2.22044604925031E-16));
#47049=CARTESIAN_POINT('Ctrl Pts',(-4.57379787866946,1.11273597287572,-1.98671766312435E-16));
#47050=CARTESIAN_POINT('Ctrl Pts',(-4.54607882402517,1.24981106593623,-1.79874459778951E-16));
#47051=CARTESIAN_POINT('Ctrl Pts',(-4.51214338117474,1.38568894112939,-8.32667268468867E-17));
#47052=CARTESIAN_POINT('Ctrl Pts',(-4.50044605637916,1.43252515439685,-4.99666743073618E-17));
#47053=CARTESIAN_POINT('Ctrl Pts',(-4.48800969217396,1.47921903836149,8.24656052999656E-18));
#47054=CARTESIAN_POINT('Ctrl Pts',(-4.47484214689978,1.52575396812219,5.55111512312578E-17));
#47055=CARTESIAN_POINT('Ctrl Pts',(-4.46954654891505,1.54446894309507,7.45195742938095E-17));
#47056=CARTESIAN_POINT('Ctrl Pts',(-4.4641321445575,1.56316001192783,2.98076212871544E-17));
#47057=CARTESIAN_POINT('Ctrl Pts',(-4.45860111065483,1.58182037106622,2.77555756156289E-17));
#47058=CARTESIAN_POINT('Ctrl Pts',(-4.41871853179728,1.7163744631118,1.29589074421813E-17));
#47059=CARTESIAN_POINT('Ctrl Pts',(-4.37289155988743,1.84894716867807,-3.65495115057949E-16));
#47060=CARTESIAN_POINT('Ctrl Pts',(-4.32143318995775,1.97915634222774,-3.60822483003176E-16));
#47061=CARTESIAN_POINT('Ctrl Pts',(-4.26919198995651,2.11134637247354,-3.56078766751783E-16));
#47062=CARTESIAN_POINT('Ctrl Pts',(-4.21114654432903,2.24110115829447,1.76811505571791E-16));
#47063=CARTESIAN_POINT('Ctrl Pts',(-4.147570486657,2.36801906886784,1.66533453693773E-16));
#47064=CARTESIAN_POINT('Ctrl Pts',(-4.08343929176894,2.49604520883007,1.56165655308743E-16));
#47065=CARTESIAN_POINT('Ctrl Pts',(-4.01368020422711,2.62118552486071,-5.6466401912637E-17));
#47066=CARTESIAN_POINT('Ctrl Pts',(-3.93852341174026,2.7430141593252,-2.77555756156289E-17));
#47067=CARTESIAN_POINT('Ctrl Pts',(-3.9294168218154,2.75777587784009,-2.4276745388323E-17));
#47068=CARTESIAN_POINT('Ctrl Pts',(-3.9202309270139,2.77248895031151,-1.25624424874937E-18));
#47069=CARTESIAN_POINT('Ctrl Pts',(-3.91096608990011,2.78715259668566,0.));
#47070=CARTESIAN_POINT('Ctrl Pts',(-3.85692740501027,2.87268072373382,-4.76202655277902E-17));
#47071=CARTESIAN_POINT('Ctrl Pts',(-3.80020397437343,2.95652797095731,1.2876992925575E-16));
#47072=CARTESIAN_POINT('Ctrl Pts',(-3.74088150109056,3.03859647479229,1.66533453693773E-16));
#47073=CARTESIAN_POINT('Ctrl Pts',(-3.7149279190293,3.0745014452201,1.83054995635409E-16));
#47074=CARTESIAN_POINT('Ctrl Pts',(-3.68847672600951,3.11006585723381,-1.71465257258441E-16));
#47075=CARTESIAN_POINT('Ctrl Pts',(-3.66153447975748,3.14528103385681,-1.66533453693773E-16));
#47076=CARTESIAN_POINT('Ctrl Pts',(-3.64469680263863,3.16728891575776,-1.6345130103068E-16));
#47077=CARTESIAN_POINT('Ctrl Pts',(-3.62766732852701,3.18916039136048,2.64610714971295E-16));
#47078=CARTESIAN_POINT('Ctrl Pts',(-3.6104475878738,3.21089327815198,2.77555756156289E-16));
#47079=CARTESIAN_POINT('Ctrl Pts',(-3.59895112257703,3.22540286826887,2.86198291473495E-16));
#47080=CARTESIAN_POINT('Ctrl Pts',(-3.58737284218715,3.23984685581822,3.27202329850872E-16));
#47081=CARTESIAN_POINT('Ctrl Pts',(-3.57571845845413,3.25421848714644,3.33066907387547E-16));
#47082=CARTESIAN_POINT('Ctrl Pts',(-3.4847651283665,3.36637780487935,3.78835338283328E-16));
#47083=CARTESIAN_POINT('Ctrl Pts',(-3.38908875605728,3.4742480319481,-5.71170610872501E-17));
#47084=CARTESIAN_POINT('Ctrl Pts',(-3.28901395033307,3.5775964314093,-5.55111512312578E-17));
#47085=CARTESIAN_POINT('Ctrl Pts',(-3.1878935796381,3.68202459780562,-5.38884630954632E-17));
#47086=CARTESIAN_POINT('Ctrl Pts',(-3.08228201196636,3.78183656326097,2.20761671403476E-16));
#47087=CARTESIAN_POINT('Ctrl Pts',(-2.97246730240431,3.87676781486652,2.77555756156289E-16));
#47088=CARTESIAN_POINT('Ctrl Pts',(-2.86296602007246,3.97142811880605,3.34187742290929E-16));
#47089=CARTESIAN_POINT('Ctrl Pts',(-2.74928508452755,4.0612360937228,2.13145292818159E-16));
#47090=CARTESIAN_POINT('Ctrl Pts',(-2.63167026985783,4.14589663192155,2.22044604925031E-16));
#47091=CARTESIAN_POINT('Ctrl Pts',(-2.51583556938655,4.22927582281283,2.3080922488549E-16));
#47092=CARTESIAN_POINT('Ctrl Pts',(-2.39618466430397,4.30766267709754,-5.76377990669945E-17));
#47093=CARTESIAN_POINT('Ctrl Pts',(-2.27292097783335,4.38073587186789,-1.11022302462516E-16));
#47094=CARTESIAN_POINT('Ctrl Pts',(-2.23861641107446,4.40107230963037,-1.25879332241991E-16));
#47095=CARTESIAN_POINT('Ctrl Pts',(-2.2040318620339,4.42099693210222,2.77555756156289E-16));
#47096=CARTESIAN_POINT('Ctrl Pts',(-2.1691713542861,4.440502182833,2.77555756156289E-16));
#47097=CARTESIAN_POINT('Origin',(0.,0.,0.));
#47098=CARTESIAN_POINT('Origin',(-2.30940107675851,-4.,-10.));
#47099=CARTESIAN_POINT('',(-2.30940107675851,-4.,-10.));
#47100=CARTESIAN_POINT('',(2.3094010767585,-4.,-10.));
#47101=CARTESIAN_POINT('',(-1.15470053837925,-4.,-10.));
#47102=CARTESIAN_POINT('',(-2.30940107675851,-4.,-4.));
#47103=CARTESIAN_POINT('',(-2.30940107675851,-4.,-10.));
#47104=CARTESIAN_POINT('',(2.3094010767585,-4.,-4.));
#47105=CARTESIAN_POINT('',(-2.30940107675851,-4.,-4.));
#47106=CARTESIAN_POINT('',(2.3094010767585,-4.,-10.));
#47107=CARTESIAN_POINT('Origin',(-4.61880215351701,5.6564012731995E-16,
-10.));
#47108=CARTESIAN_POINT('',(-4.61880215351701,5.6564012731995E-16,-10.));
#47109=CARTESIAN_POINT('',(-4.04145188432738,-0.999999999999999,-10.));
#47110=CARTESIAN_POINT('',(-4.61880215351701,5.55111512312578E-16,-4.));
#47111=CARTESIAN_POINT('',(-4.61880215351701,5.6564012731995E-16,-10.));
#47112=CARTESIAN_POINT('',(-4.61880215351701,5.6564012731995E-16,-4.));
#47113=CARTESIAN_POINT('Origin',(-2.3094010767585,4.,-10.));
#47114=CARTESIAN_POINT('',(-2.3094010767585,4.,-10.));
#47115=CARTESIAN_POINT('',(-2.88675134594813,3.,-10.));
#47116=CARTESIAN_POINT('',(-2.3094010767585,4.,-4.));
#47117=CARTESIAN_POINT('',(-2.3094010767585,4.,-10.));
#47118=CARTESIAN_POINT('',(-2.3094010767585,4.,-4.));
#47119=CARTESIAN_POINT('Origin',(2.3094010767585,4.,-10.));
#47120=CARTESIAN_POINT('',(2.3094010767585,4.,-10.));
#47121=CARTESIAN_POINT('',(1.15470053837925,4.,-10.));
#47122=CARTESIAN_POINT('',(2.3094010767585,4.,-4.));
#47123=CARTESIAN_POINT('',(2.3094010767585,4.,-10.));
#47124=CARTESIAN_POINT('',(2.3094010767585,4.,-4.));
#47125=CARTESIAN_POINT('Origin',(4.61880215351701,0.,-10.));
#47126=CARTESIAN_POINT('',(4.61880215351701,0.,-10.));
#47127=CARTESIAN_POINT('',(4.04145188432738,1.,-10.));
#47128=CARTESIAN_POINT('',(4.61880215351701,0.,-4.));
#47129=CARTESIAN_POINT('',(4.61880215351701,0.,-10.));
#47130=CARTESIAN_POINT('',(4.61880215351701,0.,-4.));
#47131=CARTESIAN_POINT('Origin',(2.3094010767585,-4.,-10.));
#47132=CARTESIAN_POINT('',(2.88675134594813,-3.,-10.));
#47133=CARTESIAN_POINT('',(2.3094010767585,-4.,-4.));
#47134=CARTESIAN_POINT('Origin',(0.,0.,-4.));
#47135=CARTESIAN_POINT('Origin',(0.,0.,0.));
#47136=CARTESIAN_POINT('',(-8.,-9.79717439317883E-16,0.));
#47137=CARTESIAN_POINT('Origin',(0.,0.,0.));
#47138=CARTESIAN_POINT('Origin',(0.,0.,-10.));
#47139=CARTESIAN_POINT('',(-8.,-9.79717439317883E-16,-10.));
#47140=CARTESIAN_POINT('',(-8.,-9.79717439317883E-16,-10.));
#47141=CARTESIAN_POINT('Origin',(0.,0.,-10.));
#47142=CARTESIAN_POINT('Origin',(0.,0.,-10.));
#47143=CARTESIAN_POINT('Origin',(0.,0.,20.));
#47144=CARTESIAN_POINT('',(0.,0.,0.));
#47145=CARTESIAN_POINT('Origin',(0.,0.,0.));
#47146=CARTESIAN_POINT('',(-30.,-3.67394039744206E-15,4.));
#47147=CARTESIAN_POINT('Origin',(0.,0.,4.));
#47148=CARTESIAN_POINT('',(-30.,-3.67394039744206E-15,0.));
#47149=CARTESIAN_POINT('',(-30.,-3.67394039744206E-15,0.));
#47150=CARTESIAN_POINT('Origin',(0.,0.,0.));
#47151=CARTESIAN_POINT('Origin',(0.,0.,4.));
#47152=CARTESIAN_POINT('Origin',(0.,0.,0.));
#47153=CARTESIAN_POINT('',(0.,0.,0.));
#47154=CARTESIAN_POINT('Origin',(-7.50000000000001,-12.9903810567666,7.5));
#47155=CARTESIAN_POINT('',(-10.0135514395051,-12.9904666377399,4.38741669750803));
#47156=CARTESIAN_POINT('',(-10.0159862278212,-12.9935669321582,4.11258330249198));
#47157=CARTESIAN_POINT('',(-10.0175,-12.9903810567666,7.5));
#47158=CARTESIAN_POINT('',(-9.41346599666503,-11.3543938533916,4.));
#47159=CARTESIAN_POINT('Ctrl Pts',(-10.0159862278212,-12.9935669321582,
4.11258330249198));
#47160=CARTESIAN_POINT('Ctrl Pts',(-10.0108023762528,-12.4010697429433,
4.07505553499466));
#47161=CARTESIAN_POINT('Ctrl Pts',(-9.79922182808404,-11.8055774964621,
4.03752776749733));
#47162=CARTESIAN_POINT('Ctrl Pts',(-9.41346599666503,-11.3543938533916,
4.));
#47163=CARTESIAN_POINT('',(-10.0175,-12.9903810567666,4.));
#47164=CARTESIAN_POINT('Origin',(-7.50000000000001,-12.9903810567666,4.));
#47165=CARTESIAN_POINT('',(-10.0175,-12.9903810567666,3.));
#47166=CARTESIAN_POINT('',(-10.0175,-12.9903810567666,7.5));
#47167=CARTESIAN_POINT('Origin',(-7.50000000000001,-12.9903810567666,3.));
#47168=CARTESIAN_POINT('',(-5.58300636833058,-11.3520706988407,4.));
#47169=CARTESIAN_POINT('Origin',(-7.50000000000001,-12.9903810567666,4.));
#47170=CARTESIAN_POINT('Ctrl Pts',(-5.58299257280548,-11.3520616136783,
4.));
#47171=CARTESIAN_POINT('Ctrl Pts',(-6.09671565847252,-10.7549231085896,
4.04999787746244));
#47172=CARTESIAN_POINT('Ctrl Pts',(-6.91408826359173,-10.4146529403296,
4.09999575492489));
#47173=CARTESIAN_POINT('Ctrl Pts',(-7.6991792943871,-10.4769907523554,4.14999363238733));
#47174=CARTESIAN_POINT('Ctrl Pts',(-8.52094345767964,-10.5422404851016,
4.20232700817142));
#47175=CARTESIAN_POINT('Ctrl Pts',(-9.30733973752043,-11.0485898984475,
4.2546603839555));
#47176=CARTESIAN_POINT('Ctrl Pts',(-9.70625816906456,-11.7696982113955,
4.30699375973958));
#47177=CARTESIAN_POINT('Ctrl Pts',(-9.91060317652291,-12.1390842109776,
4.3338014056624));
#47178=CARTESIAN_POINT('Ctrl Pts',(-10.0132749267868,-12.5648224302545,
4.36060905158521));
#47179=CARTESIAN_POINT('Ctrl Pts',(-10.0135514395051,-12.9904666377399,
4.38741669750803));
#47180=CARTESIAN_POINT('Origin',(-7.50000000000001,-12.9903810567666,7.5));
#47181=CARTESIAN_POINT('',(-10.0201378128903,-12.991921413328,5.38741669750803));
#47182=CARTESIAN_POINT('',(-10.020701946345,-12.9891728119784,5.11258330249198));
#47183=CARTESIAN_POINT('',(-10.0175,-12.9903810567666,7.5));
#47184=CARTESIAN_POINT('Ctrl Pts',(-10.020701946345,-12.9891728119784,5.11258330249198));
#47185=CARTESIAN_POINT('Ctrl Pts',(-10.0211241641948,-12.9178130461518,
5.10805583214991));
#47186=CARTESIAN_POINT('Ctrl Pts',(-10.0183502770585,-12.846486861832,5.10352836180784));
#47187=CARTESIAN_POINT('Ctrl Pts',(-10.0122725294143,-12.775443667658,5.09900089146577));
#47188=CARTESIAN_POINT('Ctrl Pts',(-9.94201937978509,-11.9542499553417,
5.04666751568169));
#47189=CARTESIAN_POINT('Ctrl Pts',(-9.43032999980707,-11.170867192649,4.99433413989761));
#47190=CARTESIAN_POINT('Ctrl Pts',(-8.70662199025935,-10.7764184817432,
4.94200076411352));
#47191=CARTESIAN_POINT('Ctrl Pts',(-7.98291398071162,-10.3819697708373,
4.88966738832944));
#47192=CARTESIAN_POINT('Ctrl Pts',(-7.04718734159418,-10.3764551117184,
4.83733401254535));
#47193=CARTESIAN_POINT('Ctrl Pts',(-6.31898112841336,-10.7625629528365,
4.78500063676127));
#47194=CARTESIAN_POINT('Ctrl Pts',(-5.59077491523255,-11.1486707939545,
4.73266726097718));
#47195=CARTESIAN_POINT('Ctrl Pts',(-5.07008912798835,-11.9264011353096,
4.6803338851931));
#47196=CARTESIAN_POINT('Ctrl Pts',(-4.99037287718051,-12.7466319075856,
4.62800050940901));
#47197=CARTESIAN_POINT('Ctrl Pts',(-4.91065662637267,-13.5668626798615,
4.57566713362493));
#47198=CARTESIAN_POINT('Ctrl Pts',(-5.27190991200121,-14.4295938830583,
4.52333375784085));
#47199=CARTESIAN_POINT('Ctrl Pts',(-5.9121672709983,-14.948847615037,4.47100038205676));
#47200=CARTESIAN_POINT('Ctrl Pts',(-6.55242462999539,-15.4681013470158,
4.41866700627267));
#47201=CARTESIAN_POINT('Ctrl Pts',(-7.47168606236103,-15.6438776077765,
4.36633363048859));
#47202=CARTESIAN_POINT('Ctrl Pts',(-8.25780335304795,-15.3956944886946,
4.31400025470451));
#47203=CARTESIAN_POINT('Ctrl Pts',(-9.04392064373486,-15.1475113696128,
4.26166687892042));
#47204=CARTESIAN_POINT('Ctrl Pts',(-9.69689379274305,-14.4753688706883,
4.20933350313634));
#47205=CARTESIAN_POINT('Ctrl Pts',(-9.92376658082896,-13.6843861063472,
4.15700012735226));
#47206=CARTESIAN_POINT('Ctrl Pts',(-9.98795104401328,-13.460609581425,4.1421945190655));
#47207=CARTESIAN_POINT('Ctrl Pts',(-10.0180313821391,-13.2273213460105,
4.12738891077874));
#47208=CARTESIAN_POINT('Ctrl Pts',(-10.0159862278212,-12.9935669321582,
4.11258330249198));
#47209=CARTESIAN_POINT('Ctrl Pts',(-10.0135514395051,-12.9904666377399,
4.38741669750803));
#47210=CARTESIAN_POINT('Ctrl Pts',(-10.013814729649,-13.3957569451608,4.41294242736929));
#47211=CARTESIAN_POINT('Ctrl Pts',(-9.92124152424158,-13.8009620169255,
4.43846815723057));
#47212=CARTESIAN_POINT('Ctrl Pts',(-9.73520854233975,-14.1573521883653,
4.46399388709184));
#47213=CARTESIAN_POINT('Ctrl Pts',(-9.35379990082332,-14.8880306398367,
4.51632726287592));
#47214=CARTESIAN_POINT('Ctrl Pts',(-8.57954203454297,-15.4135203302294,
4.56866063866001));
#47215=CARTESIAN_POINT('Ctrl Pts',(-7.75970075309617,-15.4983926191754,
4.62099401444409));
#47216=CARTESIAN_POINT('Ctrl Pts',(-6.93985947164937,-15.5832649081213,
4.67332739022818));
#47217=CARTESIAN_POINT('Ctrl Pts',(-6.07443477503611,-15.2275197956205,
4.72566076601226));
#47218=CARTESIAN_POINT('Ctrl Pts',(-5.5513808289996,-14.5905667824841,4.77799414179634));
#47219=CARTESIAN_POINT('Ctrl Pts',(-5.02832688296309,-13.9536137693476,
4.83032751758043));
#47220=CARTESIAN_POINT('Ctrl Pts',(-4.84764368750334,-13.0354528555755,
4.88266089336451));
#47221=CARTESIAN_POINT('Ctrl Pts',(-5.09037368993613,-12.2477921509444,
4.93499426914859));
#47222=CARTESIAN_POINT('Ctrl Pts',(-5.33310369236891,-11.4601314463133,
4.98732764493268));
#47223=CARTESIAN_POINT('Ctrl Pts',(-5.99924689269421,-10.8029709508232,
5.03966102071677));
#47224=CARTESIAN_POINT('Ctrl Pts',(-6.79011830096555,-10.5709280850384,
5.09199439650085));
#47225=CARTESIAN_POINT('Ctrl Pts',(-7.58098970923688,-10.3388852192536,
5.14432777228494));
#47226=CARTESIAN_POINT('Ctrl Pts',(-8.49658932545427,-10.5319599831741,
5.19666114806902));
#47227=CARTESIAN_POINT('Ctrl Pts',(-9.1264120969476,-11.0635984608226,5.2489945238531));
#47228=CARTESIAN_POINT('Ctrl Pts',(-9.68170742388623,-11.532327721848,5.29513524840475));
#47229=CARTESIAN_POINT('Ctrl Pts',(-10.0148568228205,-12.2642362843572,
5.34127597295639));
#47230=CARTESIAN_POINT('Ctrl Pts',(-10.0201378128903,-12.991921413328,5.38741669750803));
#47231=CARTESIAN_POINT('Origin',(-7.50000000000001,-12.9903810567666,7.5));
#47232=CARTESIAN_POINT('',(-10.0170829580245,-12.9882144302548,6.38741669750803));
#47233=CARTESIAN_POINT('',(-10.0137189064297,-12.9898141627747,6.11258330249198));
#47234=CARTESIAN_POINT('',(-10.0175,-12.9903810567666,7.5));
#47235=CARTESIAN_POINT('Ctrl Pts',(-10.0137189064297,-12.9898141627747,
6.11258330249198));
#47236=CARTESIAN_POINT('Ctrl Pts',(-10.0144984482212,-12.6110466544282,
6.08872275352109));
#47237=CARTESIAN_POINT('Ctrl Pts',(-9.93406605373638,-12.2325935036327,
6.06486220455019));
#47238=CARTESIAN_POINT('Ctrl Pts',(-9.77069376862533,-11.8941805898436,
6.04100165557929));
#47239=CARTESIAN_POINT('Ctrl Pts',(-9.41236910476912,-11.151939067693,5.98866827979521));
#47240=CARTESIAN_POINT('Ctrl Pts',(-8.65505620083081,-10.6023139521363,
5.93633490401113));
#47241=CARTESIAN_POINT('Ctrl Pts',(-7.83829991591844,-10.4917303363644,
5.88400152822705));
#47242=CARTESIAN_POINT('Ctrl Pts',(-7.02154363100607,-10.3811467205925,
5.83166815244296));
#47243=CARTESIAN_POINT('Ctrl Pts',(-6.14534396511963,-10.7096046046056,
5.77933477665887));
#47244=CARTESIAN_POINT('Ctrl Pts',(-5.60254926887142,-11.3298421637022,
5.72700140087479));
#47245=CARTESIAN_POINT('Ctrl Pts',(-5.05975457262321,-11.9500797227988,
5.6746680250907));
#47246=CARTESIAN_POINT('Ctrl Pts',(-4.8503648460132,-12.862096956979,5.62233464930662));
#47247=CARTESIAN_POINT('Ctrl Pts',(-5.06826092360056,-13.6569790435728,
5.57000127352254));
#47248=CARTESIAN_POINT('Ctrl Pts',(-5.28615700118792,-14.4518611301666,
5.51766789773845));
#47249=CARTESIAN_POINT('Ctrl Pts',(-5.93133888297262,-15.129608069174,5.46533452195437));
#47250=CARTESIAN_POINT('Ctrl Pts',(-6.71453628267279,-15.3863634879565,
5.41300114617028));
#47251=CARTESIAN_POINT('Ctrl Pts',(-7.49773368237297,-15.6431189067389,
5.3606677703862));
#47252=CARTESIAN_POINT('Ctrl Pts',(-8.41894659998862,-15.4788828052965,
5.30833439460211));
#47253=CARTESIAN_POINT('Ctrl Pts',(-9.06514459915626,-14.9672624236053,
5.25600101881803));
#47254=CARTESIAN_POINT('Ctrl Pts',(-9.65543865112952,-14.4999033965431,
5.20819511337601));
#47255=CARTESIAN_POINT('Ctrl Pts',(-10.0162437157927,-13.7426660344013,
5.160389207934));
#47256=CARTESIAN_POINT('Ctrl Pts',(-10.020701946345,-12.9891728119784,5.11258330249198));
#47257=CARTESIAN_POINT('Ctrl Pts',(-10.0201378128903,-12.991921413328,5.38741669750803));
#47258=CARTESIAN_POINT('Ctrl Pts',(-10.0208465865384,-13.0895856839813,
5.39360934874047));
#47259=CARTESIAN_POINT('Ctrl Pts',(-10.0156494886519,-13.1871738782112,
5.39980199997292));
#47260=CARTESIAN_POINT('Ctrl Pts',(-10.004290929159,-13.2840395347951,5.40599465120536));
#47261=CARTESIAN_POINT('Ctrl Pts',(-9.90830106310784,-14.1026399397423,
5.45832802698944));
#47262=CARTESIAN_POINT('Ctrl Pts',(-9.37227540423617,-14.8696385582602,
5.51066140277353));
#47263=CARTESIAN_POINT('Ctrl Pts',(-8.63654582863995,-15.2411510354214,
5.56299477855761));
#47264=CARTESIAN_POINT('Ctrl Pts',(-7.90081625304375,-15.6126635125827,
5.61532815434169));
#47265=CARTESIAN_POINT('Ctrl Pts',(-6.96538276072302,-15.5886898483873,
5.66766153012578));
#47266=CARTESIAN_POINT('Ctrl Pts',(-6.24965032039424,-15.1799771379828,
5.71999490590986));
#47267=CARTESIAN_POINT('Ctrl Pts',(-5.53391788006544,-14.7712644275784,
5.77232828169395));
#47268=CARTESIAN_POINT('Ctrl Pts',(-5.03788649172861,-13.9778126709648,
5.82466165747803));
#47269=CARTESIAN_POINT('Ctrl Pts',(-4.9839547824182,-13.1553705931073,5.87699503326212));
#47270=CARTESIAN_POINT('Ctrl Pts',(-4.9300230731078,-12.3329285152499,5.9293284090462));
#47271=CARTESIAN_POINT('Ctrl Pts',(-5.31819104282381,-11.4814961161485,
5.98166178483029));
#47272=CARTESIAN_POINT('Ctrl Pts',(-5.97442142669028,-10.9828167750565,
6.03399516061437));
#47273=CARTESIAN_POINT('Ctrl Pts',(-6.63065181055676,-10.4841374339645,
6.08632853639846));
#47274=CARTESIAN_POINT('Ctrl Pts',(-7.5549446085737,-10.338211150882,6.13866191218254));
#47275=CARTESIAN_POINT('Ctrl Pts',(-8.33288886120492,-10.6104648899579,
6.19099528796662));
#47276=CARTESIAN_POINT('Ctrl Pts',(-9.11083311383614,-10.8827186290339,
6.24332866375071));
#47277=CARTESIAN_POINT('Ctrl Pts',(-9.74242882108165,-11.5731523902683,
6.29566203953479));
#47278=CARTESIAN_POINT('Ctrl Pts',(-9.94449694127237,-12.3722067750024,
6.34799541531888));
#47279=CARTESIAN_POINT('Ctrl Pts',(-9.9952343802911,-12.5728419522874,6.36113584271526));
#47280=CARTESIAN_POINT('Ctrl Pts',(-10.0188915771041,-12.7803252875989,
6.37427627011165));
#47281=CARTESIAN_POINT('Ctrl Pts',(-10.0170829580245,-12.9882144302548,
6.38741669750803));
#47282=CARTESIAN_POINT('Origin',(-7.50000000000001,-12.9903810567666,7.5));
#47283=CARTESIAN_POINT('',(-10.0145082114167,-12.9918189296441,7.38741669750803));
#47284=CARTESIAN_POINT('',(-10.018916148665,-12.992363782792,7.11258330249199));
#47285=CARTESIAN_POINT('',(-10.0175,-12.9903810567666,7.5));
#47286=CARTESIAN_POINT('Ctrl Pts',(-10.018916148665,-12.992363782792,7.11258330249199));
#47287=CARTESIAN_POINT('Ctrl Pts',(-10.0130304015467,-12.3102957636159,
7.06938967489226));
#47288=CARTESIAN_POINT('Ctrl Pts',(-9.72554857159998,-11.6238530781169,
7.02619604729253));
#47289=CARTESIAN_POINT('Ctrl Pts',(-9.23088494583046,-11.1568755721922,
6.98300241969281));
#47290=CARTESIAN_POINT('Ctrl Pts',(-8.63155076501069,-10.5910858791674,
6.93066904390873));
#47291=CARTESIAN_POINT('Ctrl Pts',(-7.72807925079087,-10.3474651982644,
6.87833566812465));
#47292=CARTESIAN_POINT('Ctrl Pts',(-6.92554619007859,-10.5352419954014,
6.82600229234057));
#47293=CARTESIAN_POINT('Ctrl Pts',(-6.12301312936631,-10.7230187925383,
6.77366891655648));
#47294=CARTESIAN_POINT('Ctrl Pts',(-5.42141852216156,-11.342193067715,6.72133554077239));
#47295=CARTESIAN_POINT('Ctrl Pts',(-5.13532567649039,-12.1151551330277,
6.6690021649883));
#47296=CARTESIAN_POINT('Ctrl Pts',(-4.84923283081922,-12.8881171983403,
6.61666878920422));
#47297=CARTESIAN_POINT('Ctrl Pts',(-4.97864174668163,-13.8148670537889,
6.56433541342015));
#47298=CARTESIAN_POINT('Ctrl Pts',(-5.46553131494727,-14.4798918223762,
6.51200203763606));
#47299=CARTESIAN_POINT('Ctrl Pts',(-5.95242088321289,-15.1449165909636,
6.45966866185198));
#47300=CARTESIAN_POINT('Ctrl Pts',(-6.79679110388174,-15.5482162726898,
6.40733528606788));
#47301=CARTESIAN_POINT('Ctrl Pts',(-7.62006454012935,-15.5089697827308,
6.3550019102838));
#47302=CARTESIAN_POINT('Ctrl Pts',(-8.44333797637697,-15.4697232927718,
6.30266853449971));
#47303=CARTESIAN_POINT('Ctrl Pts',(-9.24551462820336,-14.9879306311276,
6.25033515871564));
#47304=CARTESIAN_POINT('Ctrl Pts',(-9.6669347422295,-14.2796053359332,6.19800178293155));
#47305=CARTESIAN_POINT('Ctrl Pts',(-9.89621522991991,-13.8942294041248,
6.16952895611836));
#47306=CARTESIAN_POINT('Ctrl Pts',(-10.012788678108,-13.4417979658618,6.14105612930517));
#47307=CARTESIAN_POINT('Ctrl Pts',(-10.0137189064297,-12.9898141627747,
6.11258330249198));
#47308=CARTESIAN_POINT('Ctrl Pts',(-10.0170829580245,-12.9882144302548,
6.38741669750803));
#47309=CARTESIAN_POINT('Ctrl Pts',(-10.0116885281401,-13.6082694857485,
6.42660964589573));
#47310=CARTESIAN_POINT('Ctrl Pts',(-9.77974909684708,-14.2319346209584,
6.46580259428343));
#47311=CARTESIAN_POINT('Ctrl Pts',(-9.36410112291705,-14.688271412029,6.50499554267113));
#47312=CARTESIAN_POINT('Ctrl Pts',(-8.80909665123509,-15.2976066560878,
6.55732891845521));
#47313=CARTESIAN_POINT('Ctrl Pts',(-7.92654717473526,-15.6086021359717,
6.6096622942393));
#47314=CARTESIAN_POINT('Ctrl Pts',(-7.11214796457486,-15.4818215077834,
6.66199567002339));
#47315=CARTESIAN_POINT('Ctrl Pts',(-6.29774875441446,-15.3550408795951,
6.71432904580747));
#47316=CARTESIAN_POINT('Ctrl Pts',(-5.55149981059349,-14.7904841433347,
6.76666242159156));
#47317=CARTESIAN_POINT('Ctrl Pts',(-5.20798543690379,-14.041273034435,6.81899579737564));
#47318=CARTESIAN_POINT('Ctrl Pts',(-4.8644710632141,-13.2920619255352,6.87132917315972));
#47319=CARTESIAN_POINT('Ctrl Pts',(-4.92369125965567,-12.3581964439962,
6.92366254894381));
#47320=CARTESIAN_POINT('Ctrl Pts',(-5.35909436185687,-11.6583796505146,
6.97599592472789));
#47321=CARTESIAN_POINT('Ctrl Pts',(-5.79449746405807,-10.958562857033,7.02832930051198));
#47322=CARTESIAN_POINT('Ctrl Pts',(-6.60608347201889,-10.4927947516089,
7.08066267629606));
#47323=CARTESIAN_POINT('Ctrl Pts',(-7.42997390874126,-10.469904702335,7.13299605208014));
#47324=CARTESIAN_POINT('Ctrl Pts',(-8.25386434546363,-10.4470146530611,
7.18532942786423));
#47325=CARTESIAN_POINT('Ctrl Pts',(-9.09005921094755,-10.8670026599375,
7.23766280364831));
#47326=CARTESIAN_POINT('Ctrl Pts',(-9.56364652484227,-11.5415650835207,
7.2899961794324));
#47327=CARTESIAN_POINT('Ctrl Pts',(-9.8575133022249,-11.9601393986381,7.32246968545761));
#47328=CARTESIAN_POINT('Ctrl Pts',(-10.0117632716449,-12.4767339212603,
7.35494319148282));
#47329=CARTESIAN_POINT('Ctrl Pts',(-10.0145082114167,-12.9918189296441,
7.38741669750803));
#47330=CARTESIAN_POINT('Origin',(-7.50000000000001,-12.9903810567666,7.5));
#47331=CARTESIAN_POINT('',(-10.0214372954169,-12.9905287409231,8.38741669750803));
#47332=CARTESIAN_POINT('',(-10.0184392382435,-12.988301844852,8.11258330249199));
#47333=CARTESIAN_POINT('',(-10.0175,-12.9903810567666,7.5));
#47334=CARTESIAN_POINT('Ctrl Pts',(-10.0184392382435,-12.988301844852,8.11258330249199));
#47335=CARTESIAN_POINT('Ctrl Pts',(-10.0198619759554,-12.8272606230119,
8.10238997204752));
#47336=CARTESIAN_POINT('Ctrl Pts',(-10.0057050234181,-12.6664683956915,
8.09219664160306));
#47337=CARTESIAN_POINT('Ctrl Pts',(-9.97504897913497,-12.5088858958898,
8.08200331115859));
#47338=CARTESIAN_POINT('Ctrl Pts',(-9.81765838984107,-11.699844707237,8.02966993537451));
#47339=CARTESIAN_POINT('Ctrl Pts',(-9.22537188297354,-10.9754080177822,
7.97733655959042));
#47340=CARTESIAN_POINT('Ctrl Pts',(-8.46374395491092,-10.660380492594,7.92500318380633));
#47341=CARTESIAN_POINT('Ctrl Pts',(-7.70211602684831,-10.3453529674058,
7.87266980802225));
#47342=CARTESIAN_POINT('Ctrl Pts',(-6.77114667759061,-10.4397346064841,
7.82033643223817));
#47343=CARTESIAN_POINT('Ctrl Pts',(-6.0882404805551,-10.9012089485628,7.76800305645409));
#47344=CARTESIAN_POINT('Ctrl Pts',(-5.4053342835196,-11.3626832906415,7.71566968067));
#47345=CARTESIAN_POINT('Ctrl Pts',(-4.97049123870628,-12.1912503357206,
7.66333630488591));
#47346=CARTESIAN_POINT('Ctrl Pts',(-4.97867531110115,-13.0154180759185,
7.61100292910183));
#47347=CARTESIAN_POINT('Ctrl Pts',(-4.98685938349602,-13.8395858161164,
7.55866955331774));
#47348=CARTESIAN_POINT('Ctrl Pts',(-5.43807057309907,-14.6593542514331,
7.50633617753366));
#47349=CARTESIAN_POINT('Ctrl Pts',(-6.130006178679,-15.1071762692505,7.45400280174958));
#47350=CARTESIAN_POINT('Ctrl Pts',(-6.82194178425893,-15.554998287068,7.40166942596549));
#47351=CARTESIAN_POINT('Ctrl Pts',(-7.75460180581574,-15.6308738873863,
7.3493360501814));
#47352=CARTESIAN_POINT('Ctrl Pts',(-8.509823648947,-15.3007838855131,7.29700267439732));
#47353=CARTESIAN_POINT('Ctrl Pts',(-9.26504549207826,-14.9706938836398,
7.24466929861323));
#47354=CARTESIAN_POINT('Ctrl Pts',(-9.84282915678396,-14.2346382795751,
7.19233592282916));
#47355=CARTESIAN_POINT('Ctrl Pts',(-9.98412256542695,-13.4226311249693,
7.14000254704507));
#47356=CARTESIAN_POINT('Ctrl Pts',(-10.0087987143617,-13.2808183562381,
7.13086279886071));
#47357=CARTESIAN_POINT('Ctrl Pts',(-10.0201615695645,-13.1366890058931,
7.12172305067635));
#47358=CARTESIAN_POINT('Ctrl Pts',(-10.018916148665,-12.992363782792,7.11258330249199));
#47359=CARTESIAN_POINT('Ctrl Pts',(-10.0145082114167,-12.9918189296441,
7.38741669750803));
#47360=CARTESIAN_POINT('Ctrl Pts',(-10.0161869382632,-13.306830224492,7.4072765672669));
#47361=CARTESIAN_POINT('Ctrl Pts',(-9.96119980531574,-13.6212769313365,
7.42713643702578));
#47362=CARTESIAN_POINT('Ctrl Pts',(-9.84682750368121,-13.9123926462011,
7.44699630678465));
#47363=CARTESIAN_POINT('Ctrl Pts',(-9.54544140631991,-14.6795209450086,
7.49932968256874));
#47364=CARTESIAN_POINT('Ctrl Pts',(-8.83168944929182,-15.2846407023335,
7.55166305835282));
#47365=CARTESIAN_POINT('Ctrl Pts',(-8.02558574588715,-15.4564435717975,
7.60399643413691));
#47366=CARTESIAN_POINT('Ctrl Pts',(-7.21948204248248,-15.6282464412614,
7.65632980992099));
#47367=CARTESIAN_POINT('Ctrl Pts',(-6.32102659270125,-15.3667324228643,
7.70866318570508));
#47368=CARTESIAN_POINT('Ctrl Pts',(-5.73304620733022,-14.789152581525,7.76099656148916));
#47369=CARTESIAN_POINT('Ctrl Pts',(-5.1450658219592,-14.2115727401857,7.81332993727324));
#47370=CARTESIAN_POINT('Ctrl Pts',(-4.86756050099838,-13.3179270759042,
7.86566331305732));
#47371=CARTESIAN_POINT('Ctrl Pts',(-5.02495108614128,-12.5088859085888,
7.91799668884141));
#47372=CARTESIAN_POINT('Ctrl Pts',(-5.18234167128417,-11.6998447412735,
7.9703300646255));
#47373=CARTESIAN_POINT('Ctrl Pts',(-5.77462816253079,-10.9754080709243,
8.02266344040959));
#47374=CARTESIAN_POINT('Ctrl Pts',(-6.53625607050644,-10.6603805540446,
8.07499681619367));
#47375=CARTESIAN_POINT('Ctrl Pts',(-7.29788397848209,-10.3453530371649,
8.12733019197775));
#47376=CARTESIAN_POINT('Ctrl Pts',(-8.22885330318678,-10.4397346737546,
8.17966356776183));
#47377=CARTESIAN_POINT('Ctrl Pts',(-8.91175948221152,-10.9012090036623,
8.23199694354592));
#47378=CARTESIAN_POINT('Ctrl Pts',(-9.5877914836703,-11.3580381032537,8.28380352819995));
#47379=CARTESIAN_POINT('Ctrl Pts',(-10.0207292434803,-12.1746067346983,
8.33561011285399));
#47380=CARTESIAN_POINT('Ctrl Pts',(-10.0214372954169,-12.9905287409231,
8.38741669750803));
#47381=CARTESIAN_POINT('Origin',(-7.50000000000001,-12.9903810567666,7.5));
#47382=CARTESIAN_POINT('',(-10.014824715197,-12.9887562509003,9.38741669750802));
#47383=CARTESIAN_POINT('',(-10.0138589040853,-12.9911961164478,9.11258330249198));
#47384=CARTESIAN_POINT('',(-10.0175,-12.9903810567666,7.5));
#47385=CARTESIAN_POINT('Ctrl Pts',(-10.0138589040853,-12.9911961164478,
9.11258330249198));
#47386=CARTESIAN_POINT('Ctrl Pts',(-10.0124667099841,-12.5225530777913,
9.08305689341869));
#47387=CARTESIAN_POINT('Ctrl Pts',(-9.88655945291767,-12.0532151702485,
9.05353048434541));
#47388=CARTESIAN_POINT('Ctrl Pts',(-9.64090569460772,-11.6583796153827,
9.02400407527212));
#47389=CARTESIAN_POINT('Ctrl Pts',(-9.20550258092411,-10.9585628034427,
8.97167069948803));
#47390=CARTESIAN_POINT('Ctrl Pts',(-8.39391655155678,-10.4927946857384,
8.91933732370393));
#47391=CARTESIAN_POINT('Ctrl Pts',(-7.57002609310491,-10.4699046358618,
8.86700394791985));
#47392=CARTESIAN_POINT('Ctrl Pts',(-6.74613563465304,-10.4470145859851,
8.81467057213576));
#47393=CARTESIAN_POINT('Ctrl Pts',(-5.90994074711664,-10.8670026039362,
8.7623371963517));
#47394=CARTESIAN_POINT('Ctrl Pts',(-5.43635342073195,-11.5415650453096,
8.71000382056761));
#47395=CARTESIAN_POINT('Ctrl Pts',(-4.96276609434725,-12.216127486683,8.65767044478353));
#47396=CARTESIAN_POINT('Ctrl Pts',(-4.85178632911427,-13.1452643514787,
8.60533706899943));
#47397=CARTESIAN_POINT('Ctrl Pts',(-5.15317243442415,-13.9123926705184,
8.55300369321534));
#47398=CARTESIAN_POINT('Ctrl Pts',(-5.45455853973402,-14.6795209895581,
8.50067031743125));
#47399=CARTESIAN_POINT('Ctrl Pts',(-6.16831051558674,-15.2846407628417,
8.44833694164718));
#47400=CARTESIAN_POINT('Ctrl Pts',(-6.97441424025143,-15.4564436368365,
8.3960035658631));
#47401=CARTESIAN_POINT('Ctrl Pts',(-7.78051796491612,-15.6282465108314,
8.34367019007902));
#47402=CARTESIAN_POINT('Ctrl Pts',(-8.67897343839277,-15.3667324855376,
8.29133681429492));
#47403=CARTESIAN_POINT('Ctrl Pts',(-9.26695383927095,-14.7891526289653,
8.23900343851084));
#47404=CARTESIAN_POINT('Ctrl Pts',(-9.74040926576667,-14.324071961446,8.19686339317122));
#47405=CARTESIAN_POINT('Ctrl Pts',(-10.0125575264699,-13.6540591679237,
8.15472334783161));
#47406=CARTESIAN_POINT('Ctrl Pts',(-10.0184392382435,-12.988301844852,8.11258330249199));
#47407=CARTESIAN_POINT('Ctrl Pts',(-10.0214372954169,-12.9905287409231,
8.38741669750803));
#47408=CARTESIAN_POINT('Ctrl Pts',(-10.0214444951867,-12.9988253788613,
8.38794348863808));
#47409=CARTESIAN_POINT('Ctrl Pts',(-10.0214070037996,-13.0071219499406,
8.38847027976813));
#47410=CARTESIAN_POINT('Ctrl Pts',(-10.0213246224021,-13.0154180752574,
8.38899707089817));
#47411=CARTESIAN_POINT('Ctrl Pts',(-10.0131405502232,-13.8395857937195,
8.44133044668226));
#47412=CARTESIAN_POINT('Ctrl Pts',(-9.56192937252059,-14.6593542074181,
8.49366382246634));
#47413=CARTESIAN_POINT('Ctrl Pts',(-8.86999378518945,-15.1071762134239,
8.54599719825042));
#47414=CARTESIAN_POINT('Ctrl Pts',(-8.17805819785831,-15.5549982194297,
8.59833057403451));
#47415=CARTESIAN_POINT('Ctrl Pts',(-7.24539820089864,-15.6308738177427,
8.6506639498186));
#47416=CARTESIAN_POINT('Ctrl Pts',(-6.49017637768564,-15.300783824577,8.70299732560268));
#47417=CARTESIAN_POINT('Ctrl Pts',(-5.73495455447264,-14.9706938314114,
8.75533070138677));
#47418=CARTESIAN_POINT('Ctrl Pts',(-5.15717090500631,-14.2346382467671,
8.80766407717085));
#47419=CARTESIAN_POINT('Ctrl Pts',(-5.01587750008917,-13.4226311135736,
8.85999745295493));
#47420=CARTESIAN_POINT('Ctrl Pts',(-4.87458409517204,-12.6106239803801,
8.91233082873901));
#47421=CARTESIAN_POINT('Ctrl Pts',(-5.16978093480409,-11.7226652986374,
8.96466420452309));
#47422=CARTESIAN_POINT('Ctrl Pts',(-5.76911509981821,-11.1568756205409,
9.01699758030718));
#47423=CARTESIAN_POINT('Ctrl Pts',(-6.36844926483233,-10.5910859424444,
9.06933095609127));
#47424=CARTESIAN_POINT('Ctrl Pts',(-7.27192075522852,-10.3474652679941,
9.12166433187536));
#47425=CARTESIAN_POINT('Ctrl Pts',(-8.07445379477299,-10.5352420601668,
9.17399770765945));
#47426=CARTESIAN_POINT('Ctrl Pts',(-8.87698683431745,-10.7230188523395,
9.22633108344353));
#47427=CARTESIAN_POINT('Ctrl Pts',(-9.5785814230102,-11.3421931111353,9.27866445922761));
#47428=CARTESIAN_POINT('Ctrl Pts',(-9.86467426114011,-12.1151551560838,
9.33099783501169));
#47429=CARTESIAN_POINT('Ctrl Pts',(-9.96748330192147,-12.3929233341375,
9.34980412251047));
#47430=CARTESIAN_POINT('Ctrl Pts',(-10.0166359465243,-12.6905511117478,
9.36861041000925));
#47431=CARTESIAN_POINT('Ctrl Pts',(-10.014824715197,-12.9887562509003,9.38741669750802));
#47432=CARTESIAN_POINT('Origin',(-7.50000000000001,-12.9903810567666,7.5));
#47433=CARTESIAN_POINT('',(-10.0166114900998,-12.9925168768863,10.387416697508));
#47434=CARTESIAN_POINT('',(-10.0209920718673,-12.9913179799917,10.112583302492));
#47435=CARTESIAN_POINT('',(-10.0175,-12.9903810567666,7.5));
#47436=CARTESIAN_POINT('Ctrl Pts',(-10.0209920718673,-12.9913179799917,
10.112583302492));
#47437=CARTESIAN_POINT('Ctrl Pts',(-10.0172626706847,-12.2214467116455,
10.0637238147899));
#47438=CARTESIAN_POINT('Ctrl Pts',(-9.63824845828795,-11.4483937541634,
10.0148643270877));
#47439=CARTESIAN_POINT('Ctrl Pts',(-9.02557861358329,-10.9828167220247,
9.96600483938563));
#47440=CARTESIAN_POINT('Ctrl Pts',(-8.36934821243818,-10.4841373677117,
9.91367146360155));
#47441=CARTESIAN_POINT('Ctrl Pts',(-7.44505538997194,-10.3382110809426,
9.86133808781746));
#47442=CARTESIAN_POINT('Ctrl Pts',(-6.66711111680735,-10.6104648272364,
9.80900471203337));
#47443=CARTESIAN_POINT('Ctrl Pts',(-5.88916684364275,-10.8827185735301,
9.75667133624929));
#47444=CARTESIAN_POINT('Ctrl Pts',(-5.2575711197798,-11.5731523528866,9.70433796046521));
#47445=CARTESIAN_POINT('Ctrl Pts',(-5.05550299426883,-12.3722067586746,
9.65200458468113));
#47446=CARTESIAN_POINT('Ctrl Pts',(-4.85343486875787,-13.1712611644625,
9.59967120889704));
#47447=CARTESIAN_POINT('Ctrl Pts',(-5.08089434159889,-14.0789361966818,
9.54733783311295));
#47448=CARTESIAN_POINT('Ctrl Pts',(-5.63589882791342,-14.6882714568219,
9.49500445732887));
#47449=CARTESIAN_POINT('Ctrl Pts',(-6.19090331422795,-15.297606716962,9.44267108154478));
#47450=CARTESIAN_POINT('Ctrl Pts',(-7.07345281401599,-15.6086022050228,
9.3903377057607));
#47451=CARTESIAN_POINT('Ctrl Pts',(-7.88785204565785,-15.4818215734849,
9.33800432997662));
#47452=CARTESIAN_POINT('Ctrl Pts',(-8.70225127729972,-15.3550409419471,
9.28567095419253));
#47453=CARTESIAN_POINT('Ctrl Pts',(-9.44850024079541,-14.7904841908106,
9.23333757840844));
#47454=CARTESIAN_POINT('Ctrl Pts',(-9.79201462354332,-14.0412730621545,
9.18100420262436));
#47455=CARTESIAN_POINT('Ctrl Pts',(-9.94171872679729,-13.7147656848908,
9.15819723591356));
#47456=CARTESIAN_POINT('Ctrl Pts',(-10.0149342710371,-13.3531881946364,
9.13539026920277));
#47457=CARTESIAN_POINT('Ctrl Pts',(-10.0138589040853,-12.9911961164478,
9.11258330249198));
#47458=CARTESIAN_POINT('Ctrl Pts',(-10.014824715197,-12.9887562509003,9.38741669750802));
#47459=CARTESIAN_POINT('Ctrl Pts',(-10.0115957252851,-13.5203843049831,
9.42094378579333));
#47460=CARTESIAN_POINT('Ctrl Pts',(-9.84639173717802,-14.053847347733,9.45447087407864));
#47461=CARTESIAN_POINT('Ctrl Pts',(-9.53446863140466,-14.4798917831418,
9.48799796236395));
#47462=CARTESIAN_POINT('Ctrl Pts',(-9.04757907597225,-15.1449165341501,
9.54033133814803));
#47463=CARTESIAN_POINT('Ctrl Pts',(-8.20320887754036,-15.5482162050654,
9.59266471393211));
#47464=CARTESIAN_POINT('Ctrl Pts',(-7.37993546302102,-15.5089697162145,
9.6449980897162));
#47465=CARTESIAN_POINT('Ctrl Pts',(-6.55666204850167,-15.4697232273637,
9.69733146550028));
#47466=CARTESIAN_POINT('Ctrl Pts',(-5.75448541789485,-14.9879305787468,
9.74966484128437));
#47467=CARTESIAN_POINT('Ctrl Pts',(-5.3330653149527,-14.2796053021006,9.80199821706846));
#47468=CARTESIAN_POINT('Ctrl Pts',(-4.91164521201054,-13.5712800254544,
9.85433159285254));
#47469=CARTESIAN_POINT('Ctrl Pts',(-4.87098163673303,-12.636422120779,9.90666496863662));
#47470=CARTESIAN_POINT('Ctrl Pts',(-5.22930629119846,-11.8941806184447,
9.95899834442071));
#47471=CARTESIAN_POINT('Ctrl Pts',(-5.58763094566388,-11.1519391161105,
10.0113317202048));
#47472=CARTESIAN_POINT('Ctrl Pts',(-6.34494382987224,-10.6023140161175,
10.0636650959889));
#47473=CARTESIAN_POINT('Ctrl Pts',(-7.1617000931268,-10.4917304028291,10.115998471773));
#47474=CARTESIAN_POINT('Ctrl Pts',(-7.97845635638136,-10.3811467895407,
10.168331847557));
#47475=CARTESIAN_POINT('Ctrl Pts',(-8.85465599868212,-10.7096046629569,
10.2206652233411));
#47476=CARTESIAN_POINT('Ctrl Pts',(-9.39745068084417,-11.3298422064682,
10.2729985991252));
#47477=CARTESIAN_POINT('Ctrl Pts',(-9.79302701821837,-11.781857128182,10.3111379652528));
#47478=CARTESIAN_POINT('Ctrl Pts',(-10.0115266235871,-12.3888409214585,
10.3492773313804));
#47479=CARTESIAN_POINT('Ctrl Pts',(-10.0166114900998,-12.9925168768863,
10.387416697508));
#47480=CARTESIAN_POINT('Origin',(-7.50000000000001,-12.9903810567666,7.5));
#47481=CARTESIAN_POINT('',(-10.0205077525331,-12.989132710429,11.387416697508));
#47482=CARTESIAN_POINT('',(-10.0159021674261,-12.9883695445715,11.112583302492));
#47483=CARTESIAN_POINT('',(-10.0175,-12.9903810567666,7.5));
#47484=CARTESIAN_POINT('',(-5.5865340033349,-11.3543938533917,12.));
#47485=CARTESIAN_POINT('Ctrl Pts',(-10.0205077525331,-12.989132710429,11.387416697508));
#47486=CARTESIAN_POINT('Ctrl Pts',(-10.0157036585105,-13.732988657673,11.4346110043198));
#47487=CARTESIAN_POINT('Ctrl Pts',(-9.66521749773701,-14.4805837586295,
11.4818053111315));
#47488=CARTESIAN_POINT('Ctrl Pts',(-9.08783263489828,-14.9488474815931,
11.5289996179432));
#47489=CARTESIAN_POINT('Ctrl Pts',(-8.44757534455355,-15.468101244079,11.5813329937273));
#47490=CARTESIAN_POINT('Ctrl Pts',(-7.52831414497493,-15.6438777379762,
11.6336663695114));
#47491=CARTESIAN_POINT('Ctrl Pts',(-6.74219676859447,-15.395694540416,11.6859997452955));
#47492=CARTESIAN_POINT('Ctrl Pts',(-5.956079392214,-15.1475113428559,11.7383331210796));
#47493=CARTESIAN_POINT('Ctrl Pts',(-5.3031058390317,-14.4753684538384,11.7906664968637));
#47494=CARTESIAN_POINT('Ctrl Pts',(-5.07623304195856,-13.6843856961865,
11.8429998726477));
#47495=CARTESIAN_POINT('Ctrl Pts',(-4.84936024488542,-12.8934029385347,
11.8953332484318));
#47496=CARTESIAN_POINT('Ctrl Pts',(-5.04858820392145,-11.9835803122485,
11.9476666242159));
#47497=CARTESIAN_POINT('Ctrl Pts',(-5.5865340033349,-11.3543938533917,12.));
#47498=CARTESIAN_POINT('',(-9.41699369782473,-11.3520708274328,12.));
#47499=CARTESIAN_POINT('Origin',(-7.50000000000001,-12.9903810567666,12.));
#47500=CARTESIAN_POINT('Ctrl Pts',(-9.41700750114216,-11.3520617378123,
12.));
#47501=CARTESIAN_POINT('Ctrl Pts',(-8.90328443334769,-10.7549233049312,
11.9500021225376));
#47502=CARTESIAN_POINT('Ctrl Pts',(-8.08591177198773,-10.4146528382252,
11.9000042450751));
#47503=CARTESIAN_POINT('Ctrl Pts',(-7.30082070365003,-10.4769905890799,
11.8500063676127));
#47504=CARTESIAN_POINT('Ctrl Pts',(-6.47905650106146,-10.5422402577977,
11.7976729918286));
#47505=CARTESIAN_POINT('Ctrl Pts',(-5.69266020241076,-11.048589867075,11.7453396160445));
#47506=CARTESIAN_POINT('Ctrl Pts',(-5.29374176559417,-11.769698237016,11.6930062402604));
#47507=CARTESIAN_POINT('Ctrl Pts',(-4.89482332877758,-12.4908066069571,
11.6406728644763));
#47508=CARTESIAN_POINT('Ctrl Pts',(-4.88338275379511,-13.4266737375619,
11.5883394886922));
#47509=CARTESIAN_POINT('Ctrl Pts',(-5.2647914049726,-14.1573521857831,11.5360061129082));
#47510=CARTESIAN_POINT('Ctrl Pts',(-5.64620005615009,-14.8880306340043,
11.4836727371241));
#47511=CARTESIAN_POINT('Ctrl Pts',(-6.42045793348755,-15.413520399842,11.43133936134));
#47512=CARTESIAN_POINT('Ctrl Pts',(-7.24029923554721,-15.4983927042523,
11.3790059855559));
#47513=CARTESIAN_POINT('Ctrl Pts',(-8.06014053760687,-15.5832650086627,
11.3266726097718));
#47514=CARTESIAN_POINT('Ctrl Pts',(-8.92556526438873,-15.2275198516459,
11.2743392339877));
#47515=CARTESIAN_POINT('Ctrl Pts',(-9.44861922536103,-14.5905668140585,
11.2220058582037));
#47516=CARTESIAN_POINT('Ctrl Pts',(-9.81316607095874,-14.146637051602,11.1855316729664));
#47517=CARTESIAN_POINT('Ctrl Pts',(-10.0114059764305,-13.566110281377,11.1490574877292));
#47518=CARTESIAN_POINT('Ctrl Pts',(-10.0159021674261,-12.9883695445715,
11.112583302492));
#47519=CARTESIAN_POINT('Origin',(-7.50000000000001,-12.9903810567666,14.2084234471775));
#47520=CARTESIAN_POINT('',(-10.5774091090731,-12.9889059662574,4.79157655282255));
#47521=CARTESIAN_POINT('',(-10.5686793840393,-12.990485538642,4.70842344717746));
#47522=CARTESIAN_POINT('',(-10.5735,-12.9903810567665,14.2084234471775));
#47523=CARTESIAN_POINT('',(-6.7062007174672,-15.9596040105123,4.));
#47524=CARTESIAN_POINT('Ctrl Pts',(-10.5686793840393,-12.990485538642,4.70842344717746));
#47525=CARTESIAN_POINT('Ctrl Pts',(-10.568341802375,-12.4708360960575,4.68161580125464));
#47526=CARTESIAN_POINT('Ctrl Pts',(-10.1982941291361,-10.9363980734526,
4.60247477954775));
#47527=CARTESIAN_POINT('Ctrl Pts',(-7.78634786537746,-9.38338007605921,
4.47100038205676));
#47528=CARTESIAN_POINT('Ctrl Pts',(-4.64704854581202,-10.7599538374027,
4.31400025470451));
#47529=CARTESIAN_POINT('Ctrl Pts',(-4.0706083548489,-14.143375884847,4.15700012735225));
#47530=CARTESIAN_POINT('Ctrl Pts',(-5.72985994157699,-15.6985866940351,
4.05233337578409));
#47531=CARTESIAN_POINT('Ctrl Pts',(-6.7062007174672,-15.9596040105123,4.));
#47532=CARTESIAN_POINT('',(-8.29574206058843,-15.9643807808206,4.));
#47533=CARTESIAN_POINT('Origin',(-7.50000000000001,-12.9903810567666,4.));
#47534=CARTESIAN_POINT('Ctrl Pts',(-10.5774091090731,-12.9889059662574,
4.79157655282255));
#47535=CARTESIAN_POINT('Ctrl Pts',(-10.5779245754331,-12.90178610915,4.78704908248048));
#47536=CARTESIAN_POINT('Ctrl Pts',(-10.5353931215559,-11.8081560623987,
4.73018823635433));
#47537=CARTESIAN_POINT('Ctrl Pts',(-9.23195310627391,-9.81262424147309,
4.62099401444409));
#47538=CARTESIAN_POINT('Ctrl Pts',(-5.80479621412607,-9.79242646017958,
4.46399388709183));
#47539=CARTESIAN_POINT('Ctrl Pts',(-3.89775220169895,-12.6409121056472,
4.30699375973959));
#47540=CARTESIAN_POINT('Ctrl Pts',(-5.20118245874298,-15.7537141165304,
4.15232913070897));
#47541=CARTESIAN_POINT('Ctrl Pts',(-7.3659421433414,-16.2099240527811,4.04999787746244));
#47542=CARTESIAN_POINT('Ctrl Pts',(-8.2957496623611,-15.9643994715412,4.));
#47543=CARTESIAN_POINT('Origin',(-7.50000000000001,-12.9903810567666,14.2084234471775));
#47544=CARTESIAN_POINT('',(-10.5688838367077,-12.9896889619566,5.79157655282255));
#47545=CARTESIAN_POINT('',(-10.576720384476,-12.9922616072697,5.70842344717746));
#47546=CARTESIAN_POINT('',(-10.5735,-12.9903810567665,14.2084234471775));
#47547=CARTESIAN_POINT('Ctrl Pts',(-10.576720384476,-12.9922616072697,5.70842344717746));
#47548=CARTESIAN_POINT('Ctrl Pts',(-10.5702730665099,-12.1038642909273,
5.66228272262582));
#47549=CARTESIAN_POINT('Ctrl Pts',(-9.70223177580237,-10.196831424253,5.56380862229009));
#47550=CARTESIAN_POINT('Ctrl Pts',(-6.48106313838945,-9.51757559757857,
5.41300114617028));
#47551=CARTESIAN_POINT('Ctrl Pts',(-4.04127232265978,-11.9244666993329,
5.25600101881803));
#47552=CARTESIAN_POINT('Ctrl Pts',(-4.70303574023142,-15.2872880321773,
5.09900089146577));
#47553=CARTESIAN_POINT('Ctrl Pts',(-7.87270740462966,-16.5902265862243,
4.94200076411352));
#47554=CARTESIAN_POINT('Ctrl Pts',(-10.2242698683325,-14.9942184798723,
4.81180828268408));
#47555=CARTESIAN_POINT('Ctrl Pts',(-10.5690008228703,-13.4852858404724,
4.73394917703873));
#47556=CARTESIAN_POINT('Ctrl Pts',(-10.5686793840393,-12.990485538642,4.70842344717746));
#47557=CARTESIAN_POINT('Ctrl Pts',(-10.5688838367077,-12.9896889619566,
5.79157655282255));
#47558=CARTESIAN_POINT('Ctrl Pts',(-10.5698355434391,-12.5272691260468,
5.76771600385165));
#47559=CARTESIAN_POINT('Ctrl Pts',(-10.2562654399242,-11.0518487505808,
5.69152207909667));
#47560=CARTESIAN_POINT('Ctrl Pts',(-7.98558650367391,-9.40388769480238,
5.56299477855761));
#47561=CARTESIAN_POINT('Ctrl Pts',(-4.77645084555843,-10.6068850809164,
5.40599465120535));
#47562=CARTESIAN_POINT('Ctrl Pts',(-4.00954797596254,-13.9472048059447,
5.24899452385311));
#47563=CARTESIAN_POINT('Ctrl Pts',(-6.37256666156175,-16.4294950347898,
5.09199439650084));
#47564=CARTESIAN_POINT('Ctrl Pts',(-9.64926888537511,-15.8453165147797,
4.93952173949067));
#47565=CARTESIAN_POINT('Ctrl Pts',(-10.5719662603729,-13.908811197287,4.83938245826456));
#47566=CARTESIAN_POINT('Ctrl Pts',(-10.5774091090731,-12.9889059662574,
4.79157655282255));
#47567=CARTESIAN_POINT('Origin',(-7.50000000000001,-12.9903810567666,14.2084234471775));
#47568=CARTESIAN_POINT('',(-10.5752289107932,-12.9928016758089,6.79157655282255));
#47569=CARTESIAN_POINT('',(-10.5729908526269,-12.9877359220758,6.70842344717746));
#47570=CARTESIAN_POINT('',(-10.5735,-12.9903810567665,14.2084234471775));
#47571=CARTESIAN_POINT('Ctrl Pts',(-10.5729908526269,-12.9877359220758,
6.70842344717746));
#47572=CARTESIAN_POINT('Ctrl Pts',(-10.5751989125043,-12.733933626166,6.69528301978108));
#47573=CARTESIAN_POINT('Ctrl Pts',(-10.4312908590873,-11.4718008748884,
6.62980921660061));
#47574=CARTESIAN_POINT('Ctrl Pts',(-8.69550592617927,-9.57431407095109,
6.51200203763606));
#47575=CARTESIAN_POINT('Ctrl Pts',(-5.31022618670948,-10.1087781397346,
6.3550019102838));
#47576=CARTESIAN_POINT('Ctrl Pts',(-3.88853690576949,-13.2272021460562,
6.19800178293155));
#47577=CARTESIAN_POINT('Ctrl Pts',(-5.70528265200966,-16.133268450666,6.0410016555793));
#47578=CARTESIAN_POINT('Ctrl Pts',(-9.13136587582039,-16.22107348372,5.88400152822704));
#47579=CARTESIAN_POINT('Ctrl Pts',(-10.5176208014685,-14.2374825953214,
5.77314212542643));
#47580=CARTESIAN_POINT('Ctrl Pts',(-10.5775856936348,-13.1114954248875,
5.7146160984099));
#47581=CARTESIAN_POINT('Ctrl Pts',(-10.576720384476,-12.9922616072697,5.70842344717746));
#47582=CARTESIAN_POINT('Ctrl Pts',(-10.5752289107932,-12.9928016758089,
6.79157655282255));
#47583=CARTESIAN_POINT('Ctrl Pts',(-10.5680432727522,-12.1600961914245,
6.74838292522283));
#47584=CARTESIAN_POINT('Ctrl Pts',(-9.79183080592196,-10.3066734191141,
6.65285592183901));
#47585=CARTESIAN_POINT('Ctrl Pts',(-6.67544463886838,-9.46634131342536,
6.50499554267114));
#47586=CARTESIAN_POINT('Ctrl Pts',(-4.10581084513197,-11.7341055256468,
6.34799541531887));
#47587=CARTESIAN_POINT('Ctrl Pts',(-4.57977903131249,-15.1283843904584,
6.19099528796663));
#47588=CARTESIAN_POINT('Ctrl Pts',(-7.67233737080682,-16.6054945057935,
6.03399516061437));
#47589=CARTESIAN_POINT('Ctrl Pts',(-10.1638447789511,-15.1090784945035,
5.90085558223301));
#47590=CARTESIAN_POINT('Ctrl Pts',(-10.56774816372,-13.5414952057652,5.82004937963574));
#47591=CARTESIAN_POINT('Ctrl Pts',(-10.5688838367077,-12.9896889619566,
5.79157655282255));
#47592=CARTESIAN_POINT('Origin',(-7.50000000000001,-12.9903810567666,14.2084234471775));
#47593=CARTESIAN_POINT('',(-10.574646672787,-12.9878426425384,7.79157655282256));
#47594=CARTESIAN_POINT('',(-10.5698474628756,-12.992136489652,7.70842344717746));
#47595=CARTESIAN_POINT('',(-10.5735,-12.9903810567665,14.2084234471775));
#47596=CARTESIAN_POINT('Ctrl Pts',(-10.5698474628756,-12.9921364896521,
7.70842344717746));
#47597=CARTESIAN_POINT('Ctrl Pts',(-10.5664962921154,-12.3632928855735,
7.67594994115225));
#47598=CARTESIAN_POINT('Ctrl Pts',(-10.0746937830591,-10.7162100151804,
7.59114305934296));
#47599=CARTESIAN_POINT('Ctrl Pts',(-7.39948645351245,-9.37255790644949,
7.45400280174957));
#47600=CARTESIAN_POINT('Ctrl Pts',(-4.42700232783115,-11.078462500715,7.29700267439732));
#47601=CARTESIAN_POINT('Ctrl Pts',(-4.21010468283033,-14.4988027877182,
7.14000254704507));
#47602=CARTESIAN_POINT('Ctrl Pts',(-6.94328775591919,-16.5665268737914,
6.98300241969282));
#47603=CARTESIAN_POINT('Ctrl Pts',(-9.90513870920436,-15.5228207892163,
6.83914271973694));
#47604=CARTESIAN_POINT('Ctrl Pts',(-10.566405041207,-13.7447326303419,6.74761639556516));
#47605=CARTESIAN_POINT('Ctrl Pts',(-10.5729908526269,-12.9877359220758,
6.70842344717746));
#47606=CARTESIAN_POINT('Ctrl Pts',(-10.574646672787,-12.9878426425384,7.79157655282256));
#47607=CARTESIAN_POINT('Ctrl Pts',(-10.5763836278447,-12.7912348191717,
7.78138322237809));
#47608=CARTESIAN_POINT('Ctrl Pts',(-10.4703648087191,-11.5870913412493,
7.71885651614955));
#47609=CARTESIAN_POINT('Ctrl Pts',(-8.88333183851511,-9.64596167231467,
7.60399643413689));
#47610=CARTESIAN_POINT('Ctrl Pts',(-5.47359881574229,-9.99164028328652,
7.44699630678467));
#47611=CARTESIAN_POINT('Ctrl Pts',(-3.88095917534459,-13.0263185113509,
7.28999617943238));
#47612=CARTESIAN_POINT('Ctrl Pts',(-5.53354816193247,-16.0287712850697,
7.13299605208016));
#47613=CARTESIAN_POINT('Ctrl Pts',(-8.94947337693327,-16.3066703804957,
6.97599592472788));
#47614=CARTESIAN_POINT('Ctrl Pts',(-10.4834449578808,-14.3524988668243,
6.86218942497536));
#47615=CARTESIAN_POINT('Ctrl Pts',(-10.5767493879072,-13.1690017048858,
6.80071630100692));
#47616=CARTESIAN_POINT('Ctrl Pts',(-10.5752289107932,-12.9928016758089,
6.79157655282255));
#47617=CARTESIAN_POINT('Origin',(-7.50000000000001,-12.9903810567666,14.2084234471775));
#47618=CARTESIAN_POINT('',(-10.5690547534087,-12.9913761256565,8.79157655282255));
#47619=CARTESIAN_POINT('',(-10.5783068629449,-12.9905613575631,8.70842344717746));
#47620=CARTESIAN_POINT('',(-10.5735,-12.9903810567665,14.2084234471775));
#47621=CARTESIAN_POINT('Ctrl Pts',(-10.5783068629449,-12.9905613575631,
8.70842344717747));
#47622=CARTESIAN_POINT('Ctrl Pts',(-10.5774424348904,-11.99443969475,8.65661686252343));
#47623=CARTESIAN_POINT('Ctrl Pts',(-9.51496026706992,-9.99048048802178,
8.55247690208529));
#47624=CARTESIAN_POINT('Ctrl Pts',(-6.11666819796815,-9.64596176051859,
8.3960035658631));
#47625=CARTESIAN_POINT('Ctrl Pts',(-3.94738216319582,-12.2992560282264,
8.23900343851084));
#47626=CARTESIAN_POINT('Ctrl Pts',(-4.96376262473273,-15.5722887382593,
8.0820033111586));
#47627=CARTESIAN_POINT('Ctrl Pts',(-8.25441147268027,-16.5301000616477,
7.92500318380633));
#47628=CARTESIAN_POINT('Ctrl Pts',(-10.3278659516785,-14.7722228904523,
7.80047656247929));
#47629=CARTESIAN_POINT('Ctrl Pts',(-10.5718969432977,-13.3767192958943,
7.72828331693634));
#47630=CARTESIAN_POINT('Ctrl Pts',(-10.5698474628756,-12.9921364896521,
7.70842344717746));
#47631=CARTESIAN_POINT('Ctrl Pts',(-10.5690547534086,-12.9913761256565,
8.79157655282255));
#47632=CARTESIAN_POINT('Ctrl Pts',(-10.5673550876409,-12.4192313871019,
8.76205014374926));
#47633=CARTESIAN_POINT('Ctrl Pts',(-10.1411933372985,-10.8306504836598,
8.6801903588919));
#47634=CARTESIAN_POINT('Ctrl Pts',(-7.60051354913579,-9.37255781103892,
8.54599719825042));
#47635=CARTESIAN_POINT('Ctrl Pts',(-4.53789787464541,-10.9107899935683,
8.38899707089818));
#47636=CARTESIAN_POINT('Ctrl Pts',(-4.13142759646044,-14.3138114282651,
8.23199694354591));
#47637=CARTESIAN_POINT('Ctrl Pts',(-6.74558850742372,-16.5301001550025,
8.07499681619368));
#47638=CARTESIAN_POINT('Ctrl Pts',(-9.82259002330375,-15.634475301008,7.92819001928586));
#47639=CARTESIAN_POINT('Ctrl Pts',(-10.5674659613129,-13.8006351479846,
7.83371659816217));
#47640=CARTESIAN_POINT('Ctrl Pts',(-10.574646672787,-12.9878426425384,7.79157655282256));
#47641=CARTESIAN_POINT('Origin',(-7.50000000000001,-12.9903810567666,14.2084234471775));
#47642=CARTESIAN_POINT('',(-10.5777633099838,-12.991524903254,9.79157655282255));
#47643=CARTESIAN_POINT('',(-10.5702338677887,-12.98839740599,9.70842344717746));
#47644=CARTESIAN_POINT('',(-10.5735,-12.9903810567665,14.2084234471775));
#47645=CARTESIAN_POINT('Ctrl Pts',(-10.5702338677887,-12.98839740599,9.70842344717746));
#47646=CARTESIAN_POINT('Ctrl Pts',(-10.5724451168391,-12.6243324625202,
9.68961715967868));
#47647=CARTESIAN_POINT('Ctrl Pts',(-10.3454485117827,-11.2498286970771,
9.61847749639582));
#47648=CARTESIAN_POINT('Ctrl Pts',(-8.32455533939524,-9.46634140643289,
9.49500445732887));
#47649=CARTESIAN_POINT('Ctrl Pts',(-5.01553493137219,-10.3586172470561,
9.33800432997662));
#47650=CARTESIAN_POINT('Ctrl Pts',(-3.93435818466818,-13.6108210305748,
9.18100420262436));
#47651=CARTESIAN_POINT('Ctrl Pts',(-6.05052666129351,-16.3066702930228,
9.02400407527212));
#47652=CARTESIAN_POINT('Ctrl Pts',(-9.46645178620579,-16.0287712049414,
8.86700394791984));
#47653=CARTESIAN_POINT('Ctrl Pts',(-10.5737227704402,-14.0170617812033,
8.76181040522164));
#47654=CARTESIAN_POINT('Ctrl Pts',(-10.5783156528128,-13.0006903413578,
8.70895023830751));
#47655=CARTESIAN_POINT('Ctrl Pts',(-10.5783068629449,-12.9905613575631,
8.70842344717747));
#47656=CARTESIAN_POINT('Ctrl Pts',(-10.5777633099838,-12.991524903254,9.79157655282255));
#47657=CARTESIAN_POINT('Ctrl Pts',(-10.5732102555509,-12.0516244689892,
9.74271706512043));
#47658=CARTESIAN_POINT('Ctrl Pts',(-9.61486894310576,-10.0969521595311,
9.64152420163424));
#47659=CARTESIAN_POINT('Ctrl Pts',(-6.30449404219616,-9.57431398106461,
9.48799796236394));
#47660=CARTESIAN_POINT('Ctrl Pts',(-3.99123550321764,-12.1030705501041,
9.33099783501171));
#47661=CARTESIAN_POINT('Ctrl Pts',(-4.82431993989319,-15.4274866909495,
9.17399770765942));
#47662=CARTESIAN_POINT('Ctrl Pts',(-8.05671225877921,-16.5665269680756,
9.0169975803072));
#47663=CARTESIAN_POINT('Ctrl Pts',(-10.2758761800147,-14.8876717402662,
8.88952386202821));
#47664=CARTESIAN_POINT('Ctrl Pts',(-10.5703676194767,-13.4333156101897,
8.81438351953334));
#47665=CARTESIAN_POINT('Ctrl Pts',(-10.5690547534086,-12.9913761256565,
8.79157655282255));
#47666=CARTESIAN_POINT('Origin',(-7.50000000000001,-12.9903810567666,14.2084234471775));
#47667=CARTESIAN_POINT('',(-10.5715492796759,-12.9879252940133,10.7915765528226));
#47668=CARTESIAN_POINT('',(-10.5724152591149,-12.9929885813497,10.7084234471775));
#47669=CARTESIAN_POINT('',(-10.5735,-12.9903810567665,14.2084234471775));
#47670=CARTESIAN_POINT('Ctrl Pts',(-10.5724152591149,-12.9929885813497,
10.7084234471775));
#47671=CARTESIAN_POINT('Ctrl Pts',(-10.5662073793823,-12.2559883632733,
10.6702840810499));
#47672=CARTESIAN_POINT('Ctrl Pts',(-9.93341873530542,-10.4981249983676,
10.5798113391382));
#47673=CARTESIAN_POINT('Ctrl Pts',(-7.01441350972263,-9.40388779191504,
10.4370052214424));
#47674=CARTESIAN_POINT('Ctrl Pts',(-4.2407080682755,-11.4169238334189,10.2800050940901));
#47675=CARTESIAN_POINT('Ctrl Pts',(-4.38964093653616,-14.8408989317544,
10.1230049667379));
#47676=CARTESIAN_POINT('Ctrl Pts',(-7.32766263366035,-16.6054944100355,
9.96600483938563));
#47677=CARTESIAN_POINT('Ctrl Pts',(-10.049778264125,-15.305320221038,9.82781099953216));
#47678=CARTESIAN_POINT('Ctrl Pts',(-10.5662917424682,-13.6374376539438,
9.74195053546276));
#47679=CARTESIAN_POINT('Ctrl Pts',(-10.5702338677887,-12.98839740599,9.70842344717746));
#47680=CARTESIAN_POINT('Ctrl Pts',(-10.5715492796759,-12.9879252940133,
10.7915765528226));
#47681=CARTESIAN_POINT('Ctrl Pts',(-10.5739360130587,-12.6812405681054,
10.7757173622757));
#47682=CARTESIAN_POINT('Ctrl Pts',(-10.3919168575192,-11.3652990254922,
10.7075247959448));
#47683=CARTESIAN_POINT('Ctrl Pts',(-8.51893689306524,-9.51757549146244,
10.5869988538297));
#47684=CARTESIAN_POINT('Ctrl Pts',(-5.16549637569413,-10.2247238388162,
10.4299987264775));
#47685=CARTESIAN_POINT('Ctrl Pts',(-3.90540678666615,-13.4118934459175,
10.2729985991252));
#47686=CARTESIAN_POINT('Ctrl Pts',(-5.86863408021139,-16.2210735713392,
10.115998471773));
#47687=CARTESIAN_POINT('Ctrl Pts',(-9.29471739586239,-16.133268532241,9.9589983444207));
#47688=CARTESIAN_POINT('Ctrl Pts',(-10.5460797704268,-14.1315894099677,
9.85085770477056));
#47689=CARTESIAN_POINT('Ctrl Pts',(-10.5780870301511,-13.0583514106611,
9.79505044090451));
#47690=CARTESIAN_POINT('Ctrl Pts',(-10.5777633099838,-12.991524903254,9.79157655282255));
#47691=CARTESIAN_POINT('Origin',(-7.50000000000001,-12.9903810567666,14.2084234471775));
#47692=CARTESIAN_POINT('',(-10.5702205181091,-12.9936861301783,11.7915765528225));
#47693=CARTESIAN_POINT('',(-10.5771720267767,-12.9888570081198,11.7084234471775));
#47694=CARTESIAN_POINT('',(-10.5735,-12.9903810567665,14.2084234471775));
#47695=CARTESIAN_POINT('',(-8.29379928253297,-15.9596040105122,12.));
#47696=CARTESIAN_POINT('Ctrl Pts',(-8.29379928253297,-15.9596040105122,
12.));
#47697=CARTESIAN_POINT('Ctrl Pts',(-9.27014005842316,-15.698586694035,11.9476666242159));
#47698=CARTESIAN_POINT('Ctrl Pts',(-10.3714986866323,-14.6662860075735,
11.8781921418234));
#47699=CARTESIAN_POINT('Ctrl Pts',(-10.5724951032558,-13.3253966136884,
11.8087176594309));
#47700=CARTESIAN_POINT('Ctrl Pts',(-10.5702205181091,-12.9936861301783,
11.7915765528225));
#47701=CARTESIAN_POINT('',(-6.70425809489808,-15.964380864449,12.));
#47702=CARTESIAN_POINT('Origin',(-7.50000000000001,-12.9903810567666,12.));
#47703=CARTESIAN_POINT('Ctrl Pts',(-6.70425049788239,-15.9643995452956,
12.));
#47704=CARTESIAN_POINT('Ctrl Pts',(-7.63405808481853,-16.2099241868245,
11.9500021225376));
#47705=CARTESIAN_POINT('Ctrl Pts',(-9.69010316575102,-15.7766245762052,
11.8528099382634));
#47706=CARTESIAN_POINT('Ctrl Pts',(-10.571306929268,-13.8969965329875,11.7556177539892));
#47707=CARTESIAN_POINT('Ctrl Pts',(-10.5771720267767,-12.9888570081198,
11.7084234471775));
#47708=CARTESIAN_POINT('Origin',(-7.5,12.9903810567666,7.5));
#47709=CARTESIAN_POINT('',(-10.0135512354019,12.9902955808623,4.38741669750803));
#47710=CARTESIAN_POINT('',(-10.0159871075715,12.98719611739,4.11258330249198));
#47711=CARTESIAN_POINT('',(-10.0175,12.9903810567666,7.5));
#47712=CARTESIAN_POINT('',(-9.41346599666504,14.6263682601415,4.));
#47713=CARTESIAN_POINT('Ctrl Pts',(-10.0159871075715,12.98719611739,4.11258330249198));
#47714=CARTESIAN_POINT('Ctrl Pts',(-10.0108029441705,13.5796929638899,4.07505553499465));
#47715=CARTESIAN_POINT('Ctrl Pts',(-9.79922182808404,14.175184617071,4.03752776749733));
#47716=CARTESIAN_POINT('Ctrl Pts',(-9.41346599666504,14.6263682601416,4.));
#47717=CARTESIAN_POINT('',(-10.0175,12.9903810567666,4.));
#47718=CARTESIAN_POINT('Origin',(-7.5,12.9903810567666,4.));
#47719=CARTESIAN_POINT('',(-10.0175,12.9903810567666,3.));
#47720=CARTESIAN_POINT('',(-10.0175,12.9903810567666,7.5));
#47721=CARTESIAN_POINT('Origin',(-7.5,12.9903810567666,3.));
#47722=CARTESIAN_POINT('',(-5.58300657818904,14.6286918237334,4.));
#47723=CARTESIAN_POINT('Origin',(-7.5,12.9903810567666,4.));
#47724=CARTESIAN_POINT('Ctrl Pts',(-5.58299280741585,14.6287008947316,4.));
#47725=CARTESIAN_POINT('Ctrl Pts',(-6.09671594976083,15.225839628633,4.04999787746244));
#47726=CARTESIAN_POINT('Ctrl Pts',(-6.91408837638834,15.566108849254,4.09999575492489));
#47727=CARTESIAN_POINT('Ctrl Pts',(-7.69917928811933,15.5037708430362,4.14999363238733));
#47728=CARTESIAN_POINT('Ctrl Pts',(-8.52094332678579,15.4385209070269,4.20232700817142));
#47729=CARTESIAN_POINT('Ctrl Pts',(-9.30733954710939,14.9321721158988,4.2546603839555));
#47730=CARTESIAN_POINT('Ctrl Pts',(-9.7062579619942,14.2110639837978,4.30699375973958));
#47731=CARTESIAN_POINT('Ctrl Pts',(-9.91060296091885,13.8416780768541,4.3338014056624));
#47732=CARTESIAN_POINT('Ctrl Pts',(-10.0132747138948,13.4159398344011,4.36060905158521));
#47733=CARTESIAN_POINT('Ctrl Pts',(-10.0135512354019,12.9902955808623,4.38741669750803));
#47734=CARTESIAN_POINT('Origin',(-7.5,12.9903810567666,7.5));
#47735=CARTESIAN_POINT('',(-10.0201376030965,12.9888406983805,5.38741669750803));
#47736=CARTESIAN_POINT('',(-10.0207017684327,12.9915893349038,5.11258330249198));
#47737=CARTESIAN_POINT('',(-10.0175,12.9903810567666,7.5));
#47738=CARTESIAN_POINT('Ctrl Pts',(-10.0207017684327,12.9915893349038,5.11258330249198));
#47739=CARTESIAN_POINT('Ctrl Pts',(-10.021123985829,13.062949094674,5.10805583214991));
#47740=CARTESIAN_POINT('Ctrl Pts',(-10.0183500982852,13.1342752724561,5.10352836180784));
#47741=CARTESIAN_POINT('Ctrl Pts',(-10.0122723502588,13.2053184595532,5.09900089146578));
#47742=CARTESIAN_POINT('Ctrl Pts',(-9.94201919621031,14.0265120900682,5.04666751568169));
#47743=CARTESIAN_POINT('Ctrl Pts',(-9.43032981516091,14.8098946989374,4.99433413989761));
#47744=CARTESIAN_POINT('Ctrl Pts',(-8.7066218792309,15.204343412931,4.94200076411352));
#47745=CARTESIAN_POINT('Ctrl Pts',(-7.98291394330089,15.5987921269246,4.88966738832944));
#47746=CARTESIAN_POINT('Ctrl Pts',(-7.04718745249026,15.6043069460425,4.83733401254535));
#47747=CARTESIAN_POINT('Ctrl Pts',(-6.31898125676283,15.2181990815764,4.78500063676127));
#47748=CARTESIAN_POINT('Ctrl Pts',(-5.59077506103539,14.8320912171102,4.73266726097718));
#47749=CARTESIAN_POINT('Ctrl Pts',(-5.07008916039116,14.0543606690598,4.6803338851931));
#47750=CARTESIAN_POINT('Ctrl Pts',(-4.99037298951262,13.2341300396427,4.62800050940902));
#47751=CARTESIAN_POINT('Ctrl Pts',(-4.91065681863409,12.4138994102257,4.57566713362493));
#47752=CARTESIAN_POINT('Ctrl Pts',(-5.27191037752124,11.5511686994419,4.52333375784085));
#47753=CARTESIAN_POINT('Ctrl Pts',(-5.91216754016691,11.0319148801645,4.47100038205676));
#47754=CARTESIAN_POINT('Ctrl Pts',(-6.55242470281257,10.5126610608871,4.41866700627268));
#47755=CARTESIAN_POINT('Ctrl Pts',(-7.47168546921673,10.336884133116,4.36633363048859));
#47756=CARTESIAN_POINT('Ctrl Pts',(-8.25780300491658,10.5850674765643,4.31400025470451));
#47757=CARTESIAN_POINT('Ctrl Pts',(-9.04392054061644,10.8332508200125,4.26166687892042));
#47758=CARTESIAN_POINT('Ctrl Pts',(-9.696894845612,11.50539443468,4.20933350313634));
#47759=CARTESIAN_POINT('Ctrl Pts',(-9.92376765947752,12.2963771799981,4.15700012735225));
#47760=CARTESIAN_POINT('Ctrl Pts',(-9.98795212995513,12.5201536995385,4.1421945190655));
#47761=CARTESIAN_POINT('Ctrl Pts',(-10.0180323849149,12.7534418387471,4.12738891077874));
#47762=CARTESIAN_POINT('Ctrl Pts',(-10.0159871075715,12.98719611739,4.11258330249198));
#47763=CARTESIAN_POINT('Ctrl Pts',(-10.0135512354019,12.9902955808623,4.38741669750803));
#47764=CARTESIAN_POINT('Ctrl Pts',(-10.0138145339143,12.5850052295903,4.4129424273693));
#47765=CARTESIAN_POINT('Ctrl Pts',(-9.92124134238478,12.1798000932329,4.43846815723057));
#47766=CARTESIAN_POINT('Ctrl Pts',(-9.73520837540778,11.8234099166911,4.46399388709184));
#47767=CARTESIAN_POINT('Ctrl Pts',(-9.35379976449056,11.0927314547595,4.51632726287592));
#47768=CARTESIAN_POINT('Ctrl Pts',(-8.57954193321014,10.5672420039701,4.56866063866001));
#47769=CARTESIAN_POINT('Ctrl Pts',(-7.75970071708304,10.482369764132,4.62099401444409));
#47770=CARTESIAN_POINT('Ctrl Pts',(-6.93985950095593,10.3974975242939,4.67332739022817));
#47771=CARTESIAN_POINT('Ctrl Pts',(-6.07443489998217,10.7532424954071,4.72566076601226));
#47772=CARTESIAN_POINT('Ctrl Pts',(-5.55138100127894,11.3901954309976,4.77799414179634));
#47773=CARTESIAN_POINT('Ctrl Pts',(-5.02832710257572,12.0271483665881,4.83032751758043));
#47774=CARTESIAN_POINT('Ctrl Pts',(-4.84764390614303,12.945309266656,4.88266089336452));
#47775=CARTESIAN_POINT('Ctrl Pts',(-5.09037388542358,13.7329699193423,4.9349942691486));
#47776=CARTESIAN_POINT('Ctrl Pts',(-5.33310386470412,14.5206305720287,4.98732764493268));
#47777=CARTESIAN_POINT('Ctrl Pts',(-5.9992470196979,15.1777909773334,5.03966102071676));
#47778=CARTESIAN_POINT('Ctrl Pts',(-6.79011836385736,15.4098338158843,5.09199439650085));
#47779=CARTESIAN_POINT('Ctrl Pts',(-7.58098970801682,15.6418766544352,5.14432777228493));
#47780=CARTESIAN_POINT('Ctrl Pts',(-8.49658924134195,15.4488019262325,5.19666114806902));
#47781=CARTESIAN_POINT('Ctrl Pts',(-9.12641195891838,14.9171634974037,5.24899452385311));
#47782=CARTESIAN_POINT('Ctrl Pts',(-9.68170723832013,14.4484342794212,5.29513524840475));
#47783=CARTESIAN_POINT('Ctrl Pts',(-10.0148566122412,13.7165257701398,5.34127597295639));
#47784=CARTESIAN_POINT('Ctrl Pts',(-10.0201376030965,12.9888406983805,5.38741669750803));
#47785=CARTESIAN_POINT('Origin',(-7.5,12.9903810567666,7.5));
#47786=CARTESIAN_POINT('',(-10.0170827477036,12.9925476830062,6.38741669750803));
#47787=CARTESIAN_POINT('',(-10.0137187170915,12.9909479514162,6.11258330249198));
#47788=CARTESIAN_POINT('',(-10.0175,12.9903810567666,7.5));
#47789=CARTESIAN_POINT('Ctrl Pts',(-10.0137187170915,12.9909479514162,6.11258330249198));
#47790=CARTESIAN_POINT('Ctrl Pts',(-10.0144982588899,13.3697154315319,6.08872275352109));
#47791=CARTESIAN_POINT('Ctrl Pts',(-9.93406587049998,13.7481685539756,6.06486220455019));
#47792=CARTESIAN_POINT('Ctrl Pts',(-9.77069359762705,14.0865814419388,6.0410016555793));
#47793=CARTESIAN_POINT('Ctrl Pts',(-9.41236896061271,14.8288229074456,5.98866827979521));
#47794=CARTESIAN_POINT('Ctrl Pts',(-8.65505611306826,15.3784479785104,5.93633490401113));
#47795=CARTESIAN_POINT('Ctrl Pts',(-7.83829989006264,15.4890315871854,5.88400152822704));
#47796=CARTESIAN_POINT('Ctrl Pts',(-7.02154366705702,15.5996151958603,5.83166815244296));
#47797=CARTESIAN_POINT('Ctrl Pts',(-6.14534406859022,15.2711573421455,5.77933477665887));
#47798=CARTESIAN_POINT('Ctrl Pts',(-5.60254941260429,14.6509198275943,5.72700140087479));
#47799=CARTESIAN_POINT('Ctrl Pts',(-5.05975475661836,14.0306823130431,5.6746680250907));
#47800=CARTESIAN_POINT('Ctrl Pts',(-4.8503650431133,13.1186651376555,5.62233464930662));
#47801=CARTESIAN_POINT('Ctrl Pts',(-5.06826110556232,12.3237831148942,5.57000127352254));
#47802=CARTESIAN_POINT('Ctrl Pts',(-5.28615716801134,11.5289010921329,5.51766789773845));
#47803=CARTESIAN_POINT('Ctrl Pts',(-5.93133900641445,10.8511542219977,5.46533452195436));
#47804=CARTESIAN_POINT('Ctrl Pts',(-6.71453634454677,10.5943988157391,5.41300114617028));
#47805=CARTESIAN_POINT('Ctrl Pts',(-7.49773368267909,10.3376434094805,5.3606677703862));
#47806=CARTESIAN_POINT('Ctrl Pts',(-8.41894652054063,10.5018794670985,5.30833439460211));
#47807=CARTESIAN_POINT('Ctrl Pts',(-9.06514447594766,11.0134998219879,5.25600101881803));
#47808=CARTESIAN_POINT('Ctrl Pts',(-9.65543848794614,11.4808588245671,5.20819511337601));
#47809=CARTESIAN_POINT('Ctrl Pts',(-10.0162435426697,12.2380961764306,5.160389207934));
#47810=CARTESIAN_POINT('Ctrl Pts',(-10.0207017684327,12.9915893349038,5.11258330249198));
#47811=CARTESIAN_POINT('Ctrl Pts',(-10.0201376030965,12.9888406983805,5.38741669750803));
#47812=CARTESIAN_POINT('Ctrl Pts',(-10.02084637685,12.8911764354056,5.39360934874047));
#47813=CARTESIAN_POINT('Ctrl Pts',(-10.0156492795336,12.793588248926,5.39980199997291));
#47814=CARTESIAN_POINT('Ctrl Pts',(-10.0042907210835,12.6967226001492,5.40599465120536));
#47815=CARTESIAN_POINT('Ctrl Pts',(-9.90830086384453,11.8781222611782,5.45832802698944));
#47816=CARTESIAN_POINT('Ctrl Pts',(-9.37227524753879,11.1111237126909,5.51066140277353));
#47817=CARTESIAN_POINT('Ctrl Pts',(-8.63654573295752,10.739611267924,5.56299477855761));
#47818=CARTESIAN_POINT('Ctrl Pts',(-7.90081621837627,10.368098823157,5.6153281543417));
#47819=CARTESIAN_POINT('Ctrl Pts',(-6.96538280551948,10.3920724821103,5.66766153012578));
#47820=CARTESIAN_POINT('Ctrl Pts',(-6.24965042528476,10.8007851576184,5.71999490590986));
#47821=CARTESIAN_POINT('Ctrl Pts',(-5.53391804505003,11.2094978331266,5.77232828169395));
#47822=CARTESIAN_POINT('Ctrl Pts',(-5.03788669743737,12.0029495251895,5.82466165747803));
#47823=CARTESIAN_POINT('Ctrl Pts',(-4.98395499247446,12.8253915347154,5.87699503326212));
#47824=CARTESIAN_POINT('Ctrl Pts',(-4.93002328751154,13.6478335442413,5.9293284090462));
#47825=CARTESIAN_POINT('Ctrl Pts',(-5.31819122519835,14.4992658712303,5.98166178483029));
#47826=CARTESIAN_POINT('Ctrl Pts',(-5.97442155431181,14.997945170426,6.03399516061437));
#47827=CARTESIAN_POINT('Ctrl Pts',(-6.63065188342527,15.4966244696218,6.08632853639846));
#47828=CARTESIAN_POINT('Ctrl Pts',(-7.55494460396538,15.6425507410243,6.13866191218253));
#47829=CARTESIAN_POINT('Ctrl Pts',(-8.33288879152928,15.3702970248207,6.19099528796662));
#47830=CARTESIAN_POINT('Ctrl Pts',(-9.11083297909318,15.0980433086171,6.2433286637507));
#47831=CARTESIAN_POINT('Ctrl Pts',(-9.74242863368087,14.4076096048073,6.2956620395348));
#47832=CARTESIAN_POINT('Ctrl Pts',(-9.94449673701248,13.6085552867894,6.34799541531888));
#47833=CARTESIAN_POINT('Ctrl Pts',(-9.99523417179805,13.4079201262562,6.36113584271526));
#47834=CARTESIAN_POINT('Ctrl Pts',(-10.0188913666349,13.2004368082823,6.37427627011165));
#47835=CARTESIAN_POINT('Ctrl Pts',(-10.0170827477036,12.9925476830062,6.38741669750803));
#47836=CARTESIAN_POINT('Origin',(-7.5,12.9903810567666,7.5));
#47837=CARTESIAN_POINT('',(-10.0145080012689,12.9889431840086,7.38741669750803));
#47838=CARTESIAN_POINT('',(-10.0189159587739,12.9883983308864,7.11258330249199));
#47839=CARTESIAN_POINT('',(-10.0175,12.9903810567666,7.5));
#47840=CARTESIAN_POINT('Ctrl Pts',(-10.0189159587739,12.9883983308864,7.11258330249199));
#47841=CARTESIAN_POINT('Ctrl Pts',(-10.0130302121016,13.6704662986594,7.06938967489226));
#47842=CARTESIAN_POINT('Ctrl Pts',(-9.72554840383075,14.3569089324365,7.02619604729254));
#47843=CARTESIAN_POINT('Ctrl Pts',(-9.2308848153494,14.8238864031427,6.98300241969281));
#47844=CARTESIAN_POINT('Ctrl Pts',(-8.63155067970796,15.3896760534967,6.93066904390873));
#47845=CARTESIAN_POINT('Ctrl Pts',(-7.72807923358486,15.6332967159553,6.87833566812465));
#47846=CARTESIAN_POINT('Ctrl Pts',(-6.9255462333781,15.4455199330078,6.82600229234057));
#47847=CARTESIAN_POINT('Ctrl Pts',(-6.12301323317133,15.2577431500604,6.77366891655648));
#47848=CARTESIAN_POINT('Ctrl Pts',(-5.4214186788809,14.638568921707,6.72133554077239));
#47849=CARTESIAN_POINT('Ctrl Pts',(-5.13532585476554,13.8656069146025,6.66900216498831));
#47850=CARTESIAN_POINT('Ctrl Pts',(-4.84923303065017,13.092644907498,6.61666878920422));
#47851=CARTESIAN_POINT('Ctrl Pts',(-4.97864193670987,12.1658951216425,6.56433541342014));
#47852=CARTESIAN_POINT('Ctrl Pts',(-5.46553146829354,11.5008704033029,6.51200203763605));
#47853=CARTESIAN_POINT('Ctrl Pts',(-5.95242099987721,10.8358456849633,6.45966866185197));
#47854=CARTESIAN_POINT('Ctrl Pts',(-6.79679115698486,10.4325460341398,6.40733528606789));
#47855=CARTESIAN_POINT('Ctrl Pts',(-7.62006453112491,10.471792520931,6.35500191028381));
#47856=CARTESIAN_POINT('Ctrl Pts',(-8.44333790526497,10.5110390077222,6.30266853449972));
#47857=CARTESIAN_POINT('Ctrl Pts',(-9.24551449643742,10.9928316321281,6.25033515871563));
#47858=CARTESIAN_POINT('Ctrl Pts',(-9.66693457878153,11.7011568743055,6.19800178293155));
#47859=CARTESIAN_POINT('Ctrl Pts',(-9.89621504923482,12.0865327772692,6.16952895611836));
#47860=CARTESIAN_POINT('Ctrl Pts',(-10.0127884887617,12.5389641820168,6.14105612930517));
#47861=CARTESIAN_POINT('Ctrl Pts',(-10.0137187170915,12.9909479514162,6.11258330249198));
#47862=CARTESIAN_POINT('Ctrl Pts',(-10.0170827477036,12.9925476830062,6.38741669750803));
#47863=CARTESIAN_POINT('Ctrl Pts',(-10.0116883182615,12.3724926793498,6.42660964589573));
#47864=CARTESIAN_POINT('Ctrl Pts',(-9.77974890631033,11.7488275963524,6.46580259428343));
#47865=CARTESIAN_POINT('Ctrl Pts',(-9.36410096710587,11.2924908434457,6.50499554267113));
#47866=CARTESIAN_POINT('Ctrl Pts',(-8.80909654179214,10.6831556503463,6.55732891845521));
#47867=CARTESIAN_POINT('Ctrl Pts',(-7.92654713908917,10.3721601963736,6.6096622942393));
#47868=CARTESIAN_POINT('Ctrl Pts',(-7.11214799700031,10.4989408139477,6.66199567002338));
#47869=CARTESIAN_POINT('Ctrl Pts',(-6.29774885491145,10.6257214315218,6.71432904580747));
#47870=CARTESIAN_POINT('Ctrl Pts',(-5.55149997343671,11.1902781206427,6.76666242159156));
#47871=CARTESIAN_POINT('Ctrl Pts',(-5.20798562845119,11.9394891669376,6.81899579737564));
#47872=CARTESIAN_POINT('Ctrl Pts',(-4.86447128346568,12.6887002132326,6.87132917315972));
#47873=CARTESIAN_POINT('Ctrl Pts',(-4.92369147496937,13.6225656167016,6.92366254894381));
#47874=CARTESIAN_POINT('Ctrl Pts',(-5.35909454078469,14.3223823516912,6.97599592472789));
#47875=CARTESIAN_POINT('Ctrl Pts',(-5.79449760660002,15.0221990866808,7.02832930051197));
#47876=CARTESIAN_POINT('Ctrl Pts',(-6.60608354672698,15.4879671531909,7.08066267629606));
#47877=CARTESIAN_POINT('Ctrl Pts',(-7.42997391459192,15.5108572005546,7.13299605208014));
#47878=CARTESIAN_POINT('Ctrl Pts',(-8.25386428245684,15.5337472479183,7.18532942786423));
#47879=CARTESIAN_POINT('Ctrl Pts',(-9.09005907805975,15.1137592761355,7.23766280364831));
#47880=CARTESIAN_POINT('Ctrl Pts',(-9.56364635237551,14.4391969089269,7.2899961794324));
#47881=CARTESIAN_POINT('Ctrl Pts',(-9.85751310519891,14.0206226287906,7.32246968545761));
#47882=CARTESIAN_POINT('Ctrl Pts',(-10.0117630617271,13.5040281493434,7.35494319148282));
#47883=CARTESIAN_POINT('Ctrl Pts',(-10.0145080012689,12.9889431840086,7.38741669750803));
#47884=CARTESIAN_POINT('Origin',(-7.5,12.9903810567666,7.5));
#47885=CARTESIAN_POINT('',(-10.0214370846894,12.9902333726245,8.38741669750803));
#47886=CARTESIAN_POINT('',(-10.0184390483887,12.992460268524,8.11258330249199));
#47887=CARTESIAN_POINT('',(-10.0175,12.9903810567666,7.5));
#47888=CARTESIAN_POINT('Ctrl Pts',(-10.0184390483887,12.992460268524,8.11258330249199));
#47889=CARTESIAN_POINT('Ctrl Pts',(-10.0198617859934,13.1535014782239,8.10238997204752));
#47890=CARTESIAN_POINT('Ctrl Pts',(-10.0057048345233,13.3142936934228,8.09219664160306));
#47891=CARTESIAN_POINT('Ctrl Pts',(-9.9750487925512,13.4718761813451,8.08200331115859));
#47892=CARTESIAN_POINT('Ctrl Pts',(-9.8176582151223,14.2809173090076,8.02966993537451));
#47893=CARTESIAN_POINT('Ctrl Pts',(-9.22537175290504,15.0053539438514,7.97733655959042));
#47894=CARTESIAN_POINT('Ctrl Pts',(-8.46374388225838,15.3203814452906,7.92500318380634));
#47895=CARTESIAN_POINT('Ctrl Pts',(-7.70211601161172,15.6354089467299,7.87266980802225));
#47896=CARTESIAN_POINT('Ctrl Pts',(-6.77114673253565,15.5410273147647,7.82033643223817));
#47897=CARTESIAN_POINT('Ctrl Pts',(-6.08824058698168,15.0795530074754,7.76800305645409));
#47898=CARTESIAN_POINT('Ctrl Pts',(-5.40533444142772,14.6180787001861,7.71566968067));
#47899=CARTESIAN_POINT('Ctrl Pts',(-4.97049142939586,13.7895117175727,7.66333630488591));
#47900=CARTESIAN_POINT('Ctrl Pts',(-4.97867550117357,12.9653440395039,7.61100292910182));
#47901=CARTESIAN_POINT('Ctrl Pts',(-4.98685957295128,12.1411763614351,7.55866955331774));
#47902=CARTESIAN_POINT('Ctrl Pts',(-5.43807072853852,11.3214079879109,7.50633617753367));
#47903=CARTESIAN_POINT('Ctrl Pts',(-6.13000628195668,10.8735860038557,7.45400280174958));
#47904=CARTESIAN_POINT('Ctrl Pts',(-6.82194183537485,10.4257640198005,7.4016694259655));
#47905=CARTESIAN_POINT('Ctrl Pts',(-7.75460178662392,10.3498884252143,7.3493360501814));
#47906=CARTESIAN_POINT('Ctrl Pts',(-8.50982357282137,10.6799784021981,7.29700267439732));
#47907=CARTESIAN_POINT('Ctrl Pts',(-9.2650453590188,11.0100683791819,7.24466929861323));
#47908=CARTESIAN_POINT('Ctrl Pts',(-9.84282898016461,11.7461239277358,7.19233592282916));
#47909=CARTESIAN_POINT('Ctrl Pts',(-9.98412237815762,12.5581310211375,7.14000254704507));
#47910=CARTESIAN_POINT('Ctrl Pts',(-10.0087985252324,12.6999437791798,7.13086279886071));
#47911=CARTESIAN_POINT('Ctrl Pts',(-10.020161379579,12.8440731186622,7.12172305067635));
#47912=CARTESIAN_POINT('Ctrl Pts',(-10.0189159587739,12.9883983308864,7.11258330249199));
#47913=CARTESIAN_POINT('Ctrl Pts',(-10.0145080012689,12.9889431840086,7.38741669750803));
#47914=CARTESIAN_POINT('Ctrl Pts',(-10.0161867279748,12.6739319154882,7.4072765672669));
#47915=CARTESIAN_POINT('Ctrl Pts',(-9.96119959962244,12.359485234924,7.42713643702578));
#47916=CARTESIAN_POINT('Ctrl Pts',(-9.84682730754632,12.0683695443894,7.44699630678465));
#47917=CARTESIAN_POINT('Ctrl Pts',(-9.54544123537271,11.3012413096949,7.49932968256874));
#47918=CARTESIAN_POINT('Ctrl Pts',(-8.83168933799688,10.6961216029404,7.55166305835282));
#47919=CARTESIAN_POINT('Ctrl Pts',(-8.02558570196195,10.5243187478344,7.60399643413691));
#47920=CARTESIAN_POINT('Ctrl Pts',(-7.21948206592701,10.3525158927284,7.65632980992099));
#47921=CARTESIAN_POINT('Ctrl Pts',(-6.32102669123297,10.6140298892709,7.70866318570508));
#47922=CARTESIAN_POINT('Ctrl Pts',(-5.73304635500187,11.1916096823396,7.76099656148916));
#47923=CARTESIAN_POINT('Ctrl Pts',(-5.14506601877077,11.7691894754082,7.81332993727325));
#47924=CARTESIAN_POINT('Ctrl Pts',(-4.8675607210026,12.6628350650029,7.86566331305733));
#47925=CARTESIAN_POINT('Ctrl Pts',(-5.02495129299175,13.4718761647033,7.91799668884141));
#47926=CARTESIAN_POINT('Ctrl Pts',(-5.18234186498089,14.2809172644038,7.9703300646255));
#47927=CARTESIAN_POINT('Ctrl Pts',(-5.77462830672734,15.0053538742101,8.02266344040958));
#47928=CARTESIAN_POINT('Ctrl Pts',(-6.53625615105054,15.3203813647611,8.07499681619367));
#47929=CARTESIAN_POINT('Ctrl Pts',(-7.29788399537374,15.6354088553122,8.12733019197775));
#47930=CARTESIAN_POINT('Ctrl Pts',(-8.22885324227368,15.5410272266082,8.17966356776184));
#47931=CARTESIAN_POINT('Ctrl Pts',(-8.91175936422494,15.0795529352688,8.23199694354592));
#47932=CARTESIAN_POINT('Ctrl Pts',(-9.58779130918474,14.6227238738573,8.28380352819996));
#47933=CARTESIAN_POINT('Ctrl Pts',(-10.0207290328118,13.8061553106607,8.33561011285399));
#47934=CARTESIAN_POINT('Ctrl Pts',(-10.0214370846894,12.9902333726245,8.38741669750803));
#47935=CARTESIAN_POINT('Origin',(-7.5,12.9903810567666,7.5));
#47936=CARTESIAN_POINT('',(-10.0148245050326,12.9920058624485,9.38741669750802));
#47937=CARTESIAN_POINT('',(-10.0138587145805,12.9895659971561,9.11258330249198));
#47938=CARTESIAN_POINT('',(-10.0175,12.9903810567666,7.5));
#47939=CARTESIAN_POINT('Ctrl Pts',(-10.0138587145805,12.9895659971561,9.11258330249198));
#47940=CARTESIAN_POINT('Ctrl Pts',(-10.0124665205819,13.458209000479,9.08305689341869));
#47941=CARTESIAN_POINT('Ctrl Pts',(-9.88655927300326,13.9275468726326,9.0535304843454));
#47942=CARTESIAN_POINT('Ctrl Pts',(-9.64090553321082,14.3223823977307,9.02400407527211));
#47943=CARTESIAN_POINT('Ctrl Pts',(-9.20550245234811,15.0221991569096,8.97167069948803));
#47944=CARTESIAN_POINT('Ctrl Pts',(-8.39391648416845,15.4879672395126,8.91933732370394));
#47945=CARTESIAN_POINT('Ctrl Pts',(-7.57002608782754,15.5108572876662,8.86700394791986));
#47946=CARTESIAN_POINT('Ctrl Pts',(-6.74613569148664,15.5337473358198,8.81467057213577));
#47947=CARTESIAN_POINT('Ctrl Pts',(-5.90994086698447,15.113759349524,8.76233719635169));
#47948=CARTESIAN_POINT('Ctrl Pts',(-5.43635357630086,14.4391969590017,8.71000382056761));
#47949=CARTESIAN_POINT('Ctrl Pts',(-4.96276628561725,13.7646345684795,8.65767044478352));
#47950=CARTESIAN_POINT('Ctrl Pts',(-4.85178652875219,12.8354977737306,8.60533706899943));
#47951=CARTESIAN_POINT('Ctrl Pts',(-5.15317261134217,12.0683695125223,8.55300369321535));
#47952=CARTESIAN_POINT('Ctrl Pts',(-5.45455869393216,11.3012412513139,8.50067031743126));
#47953=CARTESIAN_POINT('Ctrl Pts',(-6.16831061597719,10.696121523646,8.44833694164718));
#47954=CARTESIAN_POINT('Ctrl Pts',(-6.97441427987286,10.5243186626023,8.3960035658631));
#47955=CARTESIAN_POINT('Ctrl Pts',(-7.78051794376854,10.3525158015586,8.34367019007901));
#47956=CARTESIAN_POINT('Ctrl Pts',(-8.67897334951486,10.6140298071391,8.29133681429493));
#47957=CARTESIAN_POINT('Ctrl Pts',(-9.26695370606775,11.1916096201701,8.23900343851084));
#47958=CARTESIAN_POINT('Ctrl Pts',(-9.74040909687172,11.656690252629,8.19686339317122));
#47959=CARTESIAN_POINT('Ctrl Pts',(-10.0125573370586,12.3267029956413,8.15472334783161));
#47960=CARTESIAN_POINT('Ctrl Pts',(-10.0184390483887,12.992460268524,8.11258330249199));
#47961=CARTESIAN_POINT('Ctrl Pts',(-10.0214370846894,12.9902333726245,8.38741669750803));
#47962=CARTESIAN_POINT('Ctrl Pts',(-10.0214442844586,12.9819367353796,8.38794348863807));
#47963=CARTESIAN_POINT('Ctrl Pts',(-10.0214067930746,12.9736401649937,8.38847027976812));
#47964=CARTESIAN_POINT('Ctrl Pts',(-10.021324411684,12.9653440403702,8.38899707089817));
#47965=CARTESIAN_POINT('Ctrl Pts',(-10.0131403401893,12.1411763907856,8.44133044668226));
#47966=CARTESIAN_POINT('Ctrl Pts',(-9.56192920019726,11.3214080455913,8.49366382246634));
#47967=CARTESIAN_POINT('Ctrl Pts',(-8.86999367069368,10.873586077015,8.54599719825042));
#47968=CARTESIAN_POINT('Ctrl Pts',(-8.1780581411901,10.4257641084388,8.59833057403451));
#47969=CARTESIAN_POINT('Ctrl Pts',(-7.24539822217496,10.3498885164806,8.65066394981859));
#47970=CARTESIAN_POINT('Ctrl Pts',(-6.49017646207993,10.6799784820534,8.70299732560268));
#47971=CARTESIAN_POINT('Ctrl Pts',(-5.7349547019849,11.0100684476262,8.75533070138676));
#47972=CARTESIAN_POINT('Ctrl Pts',(-5.15717110080998,11.7461239707299,8.80766407717085));
#47973=CARTESIAN_POINT('Ctrl Pts',(-5.01587770769964,12.5581310360714,8.85999745295494));
#47974=CARTESIAN_POINT('Ctrl Pts',(-4.8745843145893,13.3701381014129,8.91233082873902));
#47975=CARTESIAN_POINT('Ctrl Pts',(-5.16978112954355,14.2580967089923,8.96466420452309));
#47976=CARTESIAN_POINT('Ctrl Pts',(-5.76911524447212,14.823886339783,9.01699758030718));
#47977=CARTESIAN_POINT('Ctrl Pts',(-6.36844935940068,15.3896759705738,9.06933095609126));
#47978=CARTESIAN_POINT('Ctrl Pts',(-7.27192077430355,15.633296624576,9.12166433187536));
#47979=CARTESIAN_POINT('Ctrl Pts',(-8.07445374677037,15.4455198481341,9.17399770765944));
#47980=CARTESIAN_POINT('Ctrl Pts',(-8.87698671923719,15.2577430716922,9.22633108344353));
#47981=CARTESIAN_POINT('Ctrl Pts',(-9.57858124926796,14.6385688648061,9.2786644592276));
#47982=CARTESIAN_POINT('Ctrl Pts',(-9.8646740635007,13.8656068843882,9.33099783501169));
#47983=CARTESIAN_POINT('Ctrl Pts',(-9.96748309569448,13.5878387295239,9.34980412251046));
#47984=CARTESIAN_POINT('Ctrl Pts',(-10.0166357361991,13.2902109767329,9.36861041000924));
#47985=CARTESIAN_POINT('Ctrl Pts',(-10.0148245050326,12.9920058624485,9.38741669750802));
#47986=CARTESIAN_POINT('Origin',(-7.5,12.9903810567666,7.5));
#47987=CARTESIAN_POINT('',(-10.0166112816083,12.988245230306,10.387416697508));
#47988=CARTESIAN_POINT('',(-10.0209918820407,12.9894441341194,10.112583302492));
#47989=CARTESIAN_POINT('',(-10.0175,12.9903810567666,7.5));
#47990=CARTESIAN_POINT('Ctrl Pts',(-10.0209918820407,12.9894441341194,10.112583302492));
#47991=CARTESIAN_POINT('Ctrl Pts',(-10.0172624812131,13.7593153446234,10.0637238147899));
#47992=CARTESIAN_POINT('Ctrl Pts',(-9.63824829706051,14.5323682430672,10.0148643270877));
#47993=CARTESIAN_POINT('Ctrl Pts',(-9.02557849846605,14.9979452399236,9.96600483938563));
#47994=CARTESIAN_POINT('Ctrl Pts',(-8.36934814670953,15.4966245564456,9.91367146360154));
#47995=CARTESIAN_POINT('Ctrl Pts',(-7.44505539412875,15.642550832678,9.86133808781746));
#47996=CARTESIAN_POINT('Ctrl Pts',(-6.66711117965626,15.3702971070154,9.80900471203338));
#47997=CARTESIAN_POINT('Ctrl Pts',(-5.88916696518377,15.0980433813528,9.75667133624929));
#47998=CARTESIAN_POINT('Ctrl Pts',(-5.25757128881956,14.4076096537953,9.70433796046521));
#47999=CARTESIAN_POINT('Ctrl Pts',(-5.05550317851592,13.608555308187,9.65200458468112));
#48000=CARTESIAN_POINT('Ctrl Pts',(-4.85343506821227,12.8095009625786,9.59967120889704));
#48001=CARTESIAN_POINT('Ctrl Pts',(-5.08089452396919,11.9018259989194,9.54733783311296));
#48002=CARTESIAN_POINT('Ctrl Pts',(-5.6358989684585,11.2924907847457,9.49500445732887));
#48003=CARTESIAN_POINT('Ctrl Pts',(-6.19090341294781,10.683155570572,9.44267108154479));
#48004=CARTESIAN_POINT('Ctrl Pts',(-7.0734528461695,10.3721601058839,9.3903377057607));
#48005=CARTESIAN_POINT('Ctrl Pts',(-7.88785201640932,10.4989407278476,9.33800432997662));
#48006=CARTESIAN_POINT('Ctrl Pts',(-8.70225118664915,10.6257213498112,9.28567095419253));
#48007=CARTESIAN_POINT('Ctrl Pts',(-9.44850009390711,11.1902780584266,9.23333757840845));
#48008=CARTESIAN_POINT('Ctrl Pts',(-9.79201445076321,11.9394891306117,9.18100420262436));
#48009=CARTESIAN_POINT('Ctrl Pts',(-9.9417185427335,12.2659964832652,9.15819723591357));
#48010=CARTESIAN_POINT('Ctrl Pts',(-10.014934081453,12.6275739462602,9.13539026920278));
#48011=CARTESIAN_POINT('Ctrl Pts',(-10.0138587145805,12.9895659971561,9.11258330249198));
#48012=CARTESIAN_POINT('Ctrl Pts',(-10.0148245050326,12.9920058624485,9.38741669750802));
#48013=CARTESIAN_POINT('Ctrl Pts',(-10.0115955154073,12.4603778526996,9.42094378579333));
#48014=CARTESIAN_POINT('Ctrl Pts',(-9.84639154112273,11.9269148544392,9.45447087407864));
#48015=CARTESIAN_POINT('Ctrl Pts',(-9.53446846140197,11.5008704547181,9.48799796236395));
#48016=CARTESIAN_POINT('Ctrl Pts',(-9.0475789466358,10.8358457594159,9.54033133814803));
#48017=CARTESIAN_POINT('Ctrl Pts',(-8.20320881866876,10.4325461227612,9.59266471393211));
#48018=CARTESIAN_POINT('Ctrl Pts',(-7.37993547300324,10.4717926080996,9.64499808971619));
#48019=CARTESIAN_POINT('Ctrl Pts',(-6.55666212733773,10.5110390934381,9.69733146550028));
#48020=CARTESIAN_POINT('Ctrl Pts',(-5.75448556397372,10.9928317007697,9.74966484128437));
#48021=CARTESIAN_POINT('Ctrl Pts',(-5.33306549615464,11.7011569186411,9.80199821706845));
#48022=CARTESIAN_POINT('Ctrl Pts',(-4.91164542833556,12.4094821365125,9.85433159285254));
#48023=CARTESIAN_POINT('Ctrl Pts',(-4.87098185606138,13.3443399649238,9.90666496863662));
#48024=CARTESIAN_POINT('Ctrl Pts',(-5.22930648076992,14.0865814044601,9.9589983444207));
#48025=CARTESIAN_POINT('Ctrl Pts',(-5.58763110547847,14.8288228439964,10.0113317202048));
#48026=CARTESIAN_POINT('Ctrl Pts',(-6.34494392716974,15.3784478946578,10.0636650959889));
#48027=CARTESIAN_POINT('Ctrl Pts',(-7.1617001217923,15.489031500081,10.115998471773));
#48028=CARTESIAN_POINT('Ctrl Pts',(-7.97845631641486,15.5996151055041,10.168331847557));
#48029=CARTESIAN_POINT('Ctrl Pts',(-8.8546558839687,15.2711572656891,10.2206652233411));
#48030=CARTESIAN_POINT('Ctrl Pts',(-9.39745052149691,14.6509197715574,10.2729985991252));
#48031=CARTESIAN_POINT('Ctrl Pts',(-9.79302682634298,14.1989048858303,10.3111379652528));
#48032=CARTESIAN_POINT('Ctrl Pts',(-10.0115264151771,13.5919211369207,10.3492773313804));
#48033=CARTESIAN_POINT('Ctrl Pts',(-10.0166112816083,12.988245230306,10.387416697508));
#48034=CARTESIAN_POINT('Origin',(-7.5,12.9903810567666,7.5));
#48035=CARTESIAN_POINT('',(-10.020507596494,12.9916292754481,11.387416697508));
#48036=CARTESIAN_POINT('',(-10.0159019782719,12.9923925656114,11.112583302492));
#48037=CARTESIAN_POINT('',(-10.0175,12.9903810567666,7.5));
#48038=CARTESIAN_POINT('',(-5.58653400333491,14.6263682601415,12.));
#48039=CARTESIAN_POINT('Ctrl Pts',(-10.020507596494,12.9916292754481,11.387416697508));
#48040=CARTESIAN_POINT('Ctrl Pts',(-10.0157033908479,12.2477735308672,11.4346110043198));
#48041=CARTESIAN_POINT('Ctrl Pts',(-9.66521700262529,11.5001788657538,11.4818053111315));
#48042=CARTESIAN_POINT('Ctrl Pts',(-9.08783233623607,11.0319150553912,11.5289996179432));
#48043=CARTESIAN_POINT('Ctrl Pts',(-8.44757526373259,10.5126611959891,11.5813329937273));
#48044=CARTESIAN_POINT('Ctrl Pts',(-7.52831480323821,10.3368839617759,11.6336663695114));
#48045=CARTESIAN_POINT('Ctrl Pts',(-6.74219715513642,10.5850674081367,11.6859997452955));
#48046=CARTESIAN_POINT('Ctrl Pts',(-5.95607950703463,10.8332508544976,11.7383331210796));
#48047=CARTESIAN_POINT('Ctrl Pts',(-5.30310467132541,11.5053949814325,11.7906664968637));
#48048=CARTESIAN_POINT('Ctrl Pts',(-5.07623184554712,12.2963777181293,11.8429998726477));
#48049=CARTESIAN_POINT('Ctrl Pts',(-4.84935901976883,13.0873604548261,11.8953332484318));
#48050=CARTESIAN_POINT('Ctrl Pts',(-5.04858820392146,13.9971818012847,11.9476666242159));
#48051=CARTESIAN_POINT('Ctrl Pts',(-5.58653400333491,14.6263682601415,12.));
#48052=CARTESIAN_POINT('',(-9.41699350863879,14.6286916542883,12.));
#48053=CARTESIAN_POINT('Origin',(-7.5,12.9903810567666,12.));
#48054=CARTESIAN_POINT('Ctrl Pts',(-9.41700728965905,14.6287007311509,12.));
#48055=CARTESIAN_POINT('Ctrl Pts',(-8.90328417076102,15.2258393704274,11.9500021225376));
#48056=CARTESIAN_POINT('Ctrl Pts',(-8.08591167026785,15.5661089832965,11.9000042450751));
#48057=CARTESIAN_POINT('Ctrl Pts',(-7.30082070927967,15.5037710574514,11.8500063676127));
#48058=CARTESIAN_POINT('Ctrl Pts',(-6.47905661905513,15.438521205569,11.7976729918286));
#48059=CARTESIAN_POINT('Ctrl Pts',(-5.6926603741346,14.9321721568753,11.7453396160445));
#48060=CARTESIAN_POINT('Ctrl Pts',(-5.29374195236929,14.2110639499398,11.6930062402604));
#48061=CARTESIAN_POINT('Ctrl Pts',(-4.89482353060398,13.4899557430043,11.6406728644763));
#48062=CARTESIAN_POINT('Ctrl Pts',(-4.88338293199389,12.554088377827,11.5883394886922));
#48063=CARTESIAN_POINT('Ctrl Pts',(-5.26479155556264,11.8234099202509,11.5360061129082));
#48064=CARTESIAN_POINT('Ctrl Pts',(-5.64620017913138,11.0927314626748,11.4836727371241));
#48065=CARTESIAN_POINT('Ctrl Pts',(-6.42045802487898,10.5672419126997,11.43133936134));
#48066=CARTESIAN_POINT('Ctrl Pts',(-7.24029926801916,10.482369652534,11.3790059855559));
#48067=CARTESIAN_POINT('Ctrl Pts',(-8.06014051115934,10.3974973923684,11.3266726097718));
#48068=CARTESIAN_POINT('Ctrl Pts',(-8.92556515169212,10.753242422012,11.2743392339877));
#48069=CARTESIAN_POINT('Ctrl Pts',(-9.44861906997071,11.3901953896836,11.2220058582037));
#48070=CARTESIAN_POINT('Ctrl Pts',(-9.81316588581269,11.8341251034117,11.1855316729664));
#48071=CARTESIAN_POINT('Ctrl Pts',(-10.0114057826858,12.4146518528183,11.1490574877292));
#48072=CARTESIAN_POINT('Ctrl Pts',(-10.0159019782719,12.9923925656114,11.112583302492));
#48073=CARTESIAN_POINT('Origin',(-7.5,12.9903810567666,14.2084234471775));
#48074=CARTESIAN_POINT('',(-10.5774088918681,12.99185618799,4.79157655282255));
#48075=CARTESIAN_POINT('',(-10.5686791348591,12.9902767031652,4.70842344717746));
#48076=CARTESIAN_POINT('',(-10.5735,12.9903810567666,14.2084234471775));
#48077=CARTESIAN_POINT('',(-6.70620071746715,10.0211581030209,4.));
#48078=CARTESIAN_POINT('Ctrl Pts',(-10.5686791348591,12.9902767031652,4.70842344717746));
#48079=CARTESIAN_POINT('Ctrl Pts',(-10.568341542465,13.509926201974,4.68161580125464));
#48080=CARTESIAN_POINT('Ctrl Pts',(-10.1982938594512,15.0443643081101,4.60247477954774));
#48081=CARTESIAN_POINT('Ctrl Pts',(-7.78634777823694,16.5973803971072,4.47100038205676));
#48082=CARTESIAN_POINT('Ctrl Pts',(-4.64704915358778,15.2208104036021,4.31400025470451));
#48083=CARTESIAN_POINT('Ctrl Pts',(-4.07060765975928,11.8373819589561,4.15700012735225));
#48084=CARTESIAN_POINT('Ctrl Pts',(-5.72985994157694,10.2821754194981,4.05233337578409));
#48085=CARTESIAN_POINT('Ctrl Pts',(-6.70620071746715,10.0211581030209,4.));
#48086=CARTESIAN_POINT('',(-8.29574161562937,10.0163810931058,4.00000000000001));
#48087=CARTESIAN_POINT('Origin',(-7.5,12.9903810567666,4.));
#48088=CARTESIAN_POINT('Ctrl Pts',(-10.5774088918681,12.99185618799,4.79157655282254));
#48089=CARTESIAN_POINT('Ctrl Pts',(-10.5779243576744,13.0789760377035,4.78704908248048));
#48090=CARTESIAN_POINT('Ctrl Pts',(-10.535392897551,14.1726059842126,4.73018823635432));
#48091=CARTESIAN_POINT('Ctrl Pts',(-9.2319528795399,16.1681374132995,4.62099401444409));
#48092=CARTESIAN_POINT('Ctrl Pts',(-5.80479653057489,16.1883357805992,4.46399388709183));
#48093=CARTESIAN_POINT('Ctrl Pts',(-3.89775210281319,13.3398493780975,4.30699375973959));
#48094=CARTESIAN_POINT('Ctrl Pts',(-5.2011833457958,10.227049143879,4.15232913070897));
#48095=CARTESIAN_POINT('Ctrl Pts',(-7.36594149062469,9.77083767708475,4.04999787746245));
#48096=CARTESIAN_POINT('Ctrl Pts',(-8.29574920379123,10.0163624306404,4.00000000000001));
#48097=CARTESIAN_POINT('Origin',(-7.5,12.9903810567666,14.2084234471775));
#48098=CARTESIAN_POINT('',(-10.5688836055535,12.9910731523796,5.79157655282255));
#48099=CARTESIAN_POINT('',(-10.5767201283484,12.9885005040359,5.70842344717746));
#48100=CARTESIAN_POINT('',(-10.5735,12.9903810567666,14.2084234471775));
#48101=CARTESIAN_POINT('Ctrl Pts',(-10.5767201283484,12.9885005040358,5.70842344717746));
#48102=CARTESIAN_POINT('Ctrl Pts',(-10.5702728094234,13.8768977505312,5.66228272262582));
#48103=CARTESIAN_POINT('Ctrl Pts',(-9.70223158388916,15.7839304785174,5.56380862229009));
#48104=CARTESIAN_POINT('Ctrl Pts',(-6.48106323809927,16.4631861795336,5.41300114617029));
#48105=CARTESIAN_POINT('Ctrl Pts',(-4.04127258839909,14.0562954080889,5.25600101881802));
#48106=CARTESIAN_POINT('Ctrl Pts',(-4.70303600953422,10.693474125437,5.09900089146578));
#48107=CARTESIAN_POINT('Ctrl Pts',(-7.87270732364685,9.390536089231,4.94200076411351));
#48108=CARTESIAN_POINT('Ctrl Pts',(-10.2242696810485,10.9865434678639,4.81180828268408));
#48109=CARTESIAN_POINT('Ctrl Pts',(-10.5690005839068,12.4954763477989,4.73394917703873));
#48110=CARTESIAN_POINT('Ctrl Pts',(-10.5686791348591,12.9902767031652,4.70842344717746));
#48111=CARTESIAN_POINT('Ctrl Pts',(-10.5688836055535,12.9910731523796,5.79157655282255));
#48112=CARTESIAN_POINT('Ctrl Pts',(-10.5698353122932,13.4534929538237,5.76771600385165));
#48113=CARTESIAN_POINT('Ctrl Pts',(-10.2562652325398,14.9289132187583,5.69152207909668));
#48114=CARTESIAN_POINT('Ctrl Pts',(-7.98558646537732,16.576874141135,5.56299477855761));
#48115=CARTESIAN_POINT('Ctrl Pts',(-4.77645105419042,15.3738768659897,5.40599465120536));
#48116=CARTESIAN_POINT('Ctrl Pts',(-4.00954823259222,12.0335573562934,5.24899452385311));
#48117=CARTESIAN_POINT('Ctrl Pts',(-6.37256675930357,9.55126737969704,5.09199439650085));
#48118=CARTESIAN_POINT('Ctrl Pts',(-9.64926869943611,10.135445743826,4.93952173949067));
#48119=CARTESIAN_POINT('Ctrl Pts',(-10.571966049015,12.0719510350338,4.83938245826456));
#48120=CARTESIAN_POINT('Ctrl Pts',(-10.5774088918681,12.99185618799,4.79157655282254));
#48121=CARTESIAN_POINT('Origin',(-7.5,12.9903810567666,14.2084234471775));
#48122=CARTESIAN_POINT('',(-10.5752286789639,12.9879604379016,6.79157655282255));
#48123=CARTESIAN_POINT('',(-10.5729905958558,12.9930261911251,6.70842344717746));
#48124=CARTESIAN_POINT('',(-10.5735,12.9903810567666,14.2084234471775));
#48125=CARTESIAN_POINT('Ctrl Pts',(-10.5729905958558,12.9930261911251,6.70842344717746));
#48126=CARTESIAN_POINT('Ctrl Pts',(-10.5751986555521,13.2468284658167,6.69528301978108));
#48127=CARTESIAN_POINT('Ctrl Pts',(-10.4312906141563,14.5089611116288,6.62980921660061));
#48128=CARTESIAN_POINT('Ctrl Pts',(-8.69550582596531,16.4064477577484,6.51200203763606));
#48129=CARTESIAN_POINT('Ctrl Pts',(-5.31022637025923,15.8719837317436,6.3550019102838));
#48130=CARTESIAN_POINT('Ctrl Pts',(-3.88853720662811,12.7535599895385,6.19800178293155));
#48131=CARTESIAN_POINT('Ctrl Pts',(-5.70528280371351,9.84749392134933,6.04100165557929));
#48132=CARTESIAN_POINT('Ctrl Pts',(-9.13136573648253,9.75968890749465,5.88400152822705));
#48133=CARTESIAN_POINT('Ctrl Pts',(-10.5176205520478,11.7432796147819,5.77314212542643));
#48134=CARTESIAN_POINT('Ctrl Pts',(-10.5775854376359,12.8692666957923,5.7146160984099));
#48135=CARTESIAN_POINT('Ctrl Pts',(-10.5767201283484,12.9885005040358,5.70842344717746));
#48136=CARTESIAN_POINT('Ctrl Pts',(-10.5752286789639,12.9879604379016,6.79157655282255));
#48137=CARTESIAN_POINT('Ctrl Pts',(-10.5680430414674,13.8206658595303,6.74838292522283));
#48138=CARTESIAN_POINT('Ctrl Pts',(-9.79183063316292,15.6740884921896,6.65285592183902));
#48139=CARTESIAN_POINT('Ctrl Pts',(-6.67544470099851,16.5144205342573,6.50499554267113));
#48140=CARTESIAN_POINT('Ctrl Pts',(-4.10581110106408,14.2466564935293,6.34799541531888));
#48141=CARTESIAN_POINT('Ctrl Pts',(-4.57977925134152,10.8523778836063,6.19099528796662));
#48142=CARTESIAN_POINT('Ctrl Pts',(-7.67233735803906,9.3752678814539,6.03399516061438));
#48143=CARTESIAN_POINT('Ctrl Pts',(-10.1638445777963,10.8716837770844,5.90085558223301));
#48144=CARTESIAN_POINT('Ctrl Pts',(-10.5677479325558,12.4392669496988,5.82004937963574));
#48145=CARTESIAN_POINT('Ctrl Pts',(-10.5688836055535,12.9910731523796,5.79157655282255));
#48146=CARTESIAN_POINT('Origin',(-7.5,12.9903810567666,14.2084234471775));
#48147=CARTESIAN_POINT('',(-10.5746464410021,12.992919470803,7.79157655282256));
#48148=CARTESIAN_POINT('',(-10.5698472063158,12.988625624027,7.70842344717746));
#48149=CARTESIAN_POINT('',(-10.5735,12.9903810567666,14.2084234471775));
#48150=CARTESIAN_POINT('Ctrl Pts',(-10.5698472063158,12.988625624027,7.70842344717746));
#48151=CARTESIAN_POINT('Ctrl Pts',(-10.5664960358364,13.6174691755491,7.67594994115225));
#48152=CARTESIAN_POINT('Ctrl Pts',(-10.0746935678837,15.2645519082853,7.59114305934296));
#48153=CARTESIAN_POINT('Ctrl Pts',(-7.39948646190492,16.6082039047423,7.45400280174958));
#48154=CARTESIAN_POINT('Ctrl Pts',(-4.42700258466931,14.902299453002,7.29700267439732));
#48155=CARTESIAN_POINT('Ctrl Pts',(-4.21010495775379,11.4819594519348,7.14000254704507));
#48156=CARTESIAN_POINT('Ctrl Pts',(-6.94328780249567,9.41423553851335,6.98300241969282));
#48157=CARTESIAN_POINT('Ctrl Pts',(-9.90513850811741,10.4579415361298,6.83914271973694));
#48158=CARTESIAN_POINT('Ctrl Pts',(-10.5664047849758,12.2360295461447,6.74761639556516));
#48159=CARTESIAN_POINT('Ctrl Pts',(-10.5729905958558,12.9930261911251,6.70842344717746));
#48160=CARTESIAN_POINT('Ctrl Pts',(-10.5746464410021,12.992919470803,7.79157655282255));
#48161=CARTESIAN_POINT('Ctrl Pts',(-10.5763833959288,13.1895272793482,7.78138322237809));
#48162=CARTESIAN_POINT('Ctrl Pts',(-10.4703645847954,14.393670666495,7.71885651614954));
#48163=CARTESIAN_POINT('Ctrl Pts',(-8.88333173423194,16.3348001890992,7.6039964341369));
#48164=CARTESIAN_POINT('Ctrl Pts',(-5.47359896850368,15.9891216041795,7.44699630678466));
#48165=CARTESIAN_POINT('Ctrl Pts',(-3.88095944817013,12.9544436048999,7.28999617943239));
#48166=CARTESIAN_POINT('Ctrl Pts',(-5.53354831017302,9.95199105749957,7.13299605208015));
#48167=CARTESIAN_POINT('Ctrl Pts',(-8.9494732676674,9.67409198306777,6.97599592472789));
#48168=CARTESIAN_POINT('Ctrl Pts',(-10.4834447329667,11.6282633493619,6.86218942497536));
#48169=CARTESIAN_POINT('Ctrl Pts',(-10.5767491559627,12.8117604221037,6.80071630100691));
#48170=CARTESIAN_POINT('Ctrl Pts',(-10.5752286789639,12.9879604379016,6.79157655282255));
#48171=CARTESIAN_POINT('Origin',(-7.5,12.9903810567666,14.2084234471775));
#48172=CARTESIAN_POINT('',(-10.5690545220509,12.9893859879631,8.79157655282255));
#48173=CARTESIAN_POINT('',(-10.5783066056774,12.9902007559877,8.70842344717746));
#48174=CARTESIAN_POINT('',(-10.5735,12.9903810567666,14.2084234471775));
#48175=CARTESIAN_POINT('Ctrl Pts',(-10.5783066056774,12.9902007559877,8.70842344717746));
#48176=CARTESIAN_POINT('Ctrl Pts',(-10.5774421776949,13.9863223355525,8.65661686252342));
#48177=CARTESIAN_POINT('Ctrl Pts',(-9.51496009867182,15.9902813747918,8.5524769020853));
#48178=CARTESIAN_POINT('Ctrl Pts',(-6.11666831357863,16.3348000735102,8.3960035658631));
#48179=CARTESIAN_POINT('Ctrl Pts',(-3.9473824601037,13.6815060275445,8.23900343851085));
#48180=CARTESIAN_POINT('Ctrl Pts',(-4.9637628366961,10.4084735910568,8.08200331115859));
#48181=CARTESIAN_POINT('Ctrl Pts',(-8.25441140963209,9.45066234771208,7.92500318380633));
#48182=CARTESIAN_POINT('Ctrl Pts',(-10.3278657153401,11.208539372,7.80047656247929));
#48183=CARTESIAN_POINT('Ctrl Pts',(-10.5718966865663,12.6040428499268,7.72828331693633));
#48184=CARTESIAN_POINT('Ctrl Pts',(-10.5698472063158,12.988625624027,7.70842344717746));
#48185=CARTESIAN_POINT('Ctrl Pts',(-10.5690545220509,12.9893859879631,8.79157655282255));
#48186=CARTESIAN_POINT('Ctrl Pts',(-10.5673548564085,13.5615306833804,8.76205014374926));
#48187=CARTESIAN_POINT('Ctrl Pts',(-10.1411931381796,15.1501114670399,8.6801903588919));
#48188=CARTESIAN_POINT('Ctrl Pts',(-7.60051354156566,16.6082040297755,8.54599719825042));
#48189=CARTESIAN_POINT('Ctrl Pts',(-4.53789809794217,15.0699719631857,8.38899707089818));
#48190=CARTESIAN_POINT('Ctrl Pts',(-4.1314278504052,11.6669507850401,8.23199694354592));
#48191=CARTESIAN_POINT('Ctrl Pts',(-6.74558856429446,9.45066222537301,8.07499681619367));
#48192=CARTESIAN_POINT('Ctrl Pts',(-9.82258984821385,10.3462870118539,7.92819001928587));
#48193=CARTESIAN_POINT('Ctrl Pts',(-10.5674657300694,12.1801270266301,7.83371659816217));
#48194=CARTESIAN_POINT('Ctrl Pts',(-10.5746464410021,12.992919470803,7.79157655282255));
#48195=CARTESIAN_POINT('Origin',(-7.5,12.9903810567666,14.2084234471775));
#48196=CARTESIAN_POINT('',(-10.5777630782332,12.9892372109846,9.79157655282255));
#48197=CARTESIAN_POINT('',(-10.5702336112086,12.9923647073181,9.70842344717745));
#48198=CARTESIAN_POINT('',(-10.5735,12.9903810567666,14.2084234471775));
#48199=CARTESIAN_POINT('Ctrl Pts',(-10.5702336112086,12.9923647073181,9.70842344717746));
#48200=CARTESIAN_POINT('Ctrl Pts',(-10.5724448600627,13.3564296204275,9.68961715967868));
#48201=CARTESIAN_POINT('Ctrl Pts',(-10.3454482739325,14.7309332712505,9.61847749639582));
#48202=CARTESIAN_POINT('Ctrl Pts',(-8.32455527051676,16.5144204123725,9.49500445732887));
#48203=CARTESIAN_POINT('Ctrl Pts',(-5.01553513899265,15.6221446466417,9.33800432997661));
#48204=CARTESIAN_POINT('Ctrl Pts',(-3.93435848267263,12.3699411347509,9.18100420262437));
#48205=CARTESIAN_POINT('Ctrl Pts',(-6.0505267824277,9.67409209769908,9.02400407527211));
#48206=CARTESIAN_POINT('Ctrl Pts',(-9.46645162186327,9.95199116250562,8.86700394791985));
#48207=CARTESIAN_POINT('Ctrl Pts',(-10.573722513556,11.9637004181345,8.76181040522164));
#48208=CARTESIAN_POINT('Ctrl Pts',(-10.5783153955445,12.9800717730395,8.70895023830751));
#48209=CARTESIAN_POINT('Ctrl Pts',(-10.5783066056774,12.9902007559877,8.70842344717746));
#48210=CARTESIAN_POINT('Ctrl Pts',(-10.5777630782332,12.9892372109846,9.79157655282255));
#48211=CARTESIAN_POINT('Ctrl Pts',(-10.5732100242337,13.9291375746327,9.74271706512043));
#48212=CARTESIAN_POINT('Ctrl Pts',(-9.61486878320428,15.8838097348119,9.64152420163422));
#48213=CARTESIAN_POINT('Ctrl Pts',(-6.30449413259093,16.4064478755407,9.48799796236394));
#48214=CARTESIAN_POINT('Ctrl Pts',(-3.99123576757957,13.8776914962184,9.3309978350117));
#48215=CARTESIAN_POINT('Ctrl Pts',(-4.82432014168349,10.5532756064786,9.17399770765943));
#48216=CARTESIAN_POINT('Ctrl Pts',(-8.05671221676616,9.41423541495656,9.0169975803072));
#48217=CARTESIAN_POINT('Ctrl Pts',(-10.2758759707643,11.0930905163184,8.88952386202821));
#48218=CARTESIAN_POINT('Ctrl Pts',(-10.5703673880222,12.5474465367502,8.81438351953334));
#48219=CARTESIAN_POINT('Ctrl Pts',(-10.5690545220509,12.9893859879631,8.79157655282255));
#48220=CARTESIAN_POINT('Origin',(-7.5,12.9903810567666,14.2084234471775));
#48221=CARTESIAN_POINT('',(-10.5715490487462,12.9928368154298,10.7915765528225));
#48222=CARTESIAN_POINT('',(-10.5724150045772,12.9877735244422,10.7084234471775));
#48223=CARTESIAN_POINT('',(-10.5735,12.9903810567666,14.2084234471775));
#48224=CARTESIAN_POINT('Ctrl Pts',(-10.5724150045772,12.9877735244422,10.7084234471775));
#48225=CARTESIAN_POINT('Ctrl Pts',(-10.5662071249442,13.7247736829249,10.6702840810499));
#48226=CARTESIAN_POINT('Ctrl Pts',(-9.93341852875246,15.4826369193415,10.5798113391382));
#48227=CARTESIAN_POINT('Ctrl Pts',(-7.01441355218445,16.5768740138536,10.4370052214424));
#48228=CARTESIAN_POINT('Ctrl Pts',(-4.24070833971001,14.56383815303,10.2800050940901));
#48229=CARTESIAN_POINT('Ctrl Pts',(-4.38964119697082,11.1398633340167,10.1230049667379));
#48230=CARTESIAN_POINT('Ctrl Pts',(-7.32766264781398,9.3752680069458,9.96600483938563));
#48231=CARTESIAN_POINT('Ctrl Pts',(-10.0497780511113,10.6754420854925,9.82781099953215));
#48232=CARTESIAN_POINT('Ctrl Pts',(-10.5662914862381,12.3433245134896,9.74195053546276));
#48233=CARTESIAN_POINT('Ctrl Pts',(-10.5702336112086,12.9923647073181,9.70842344717746));
#48234=CARTESIAN_POINT('Ctrl Pts',(-10.5715490487462,12.9928368154298,10.7915765528225));
#48235=CARTESIAN_POINT('Ctrl Pts',(-10.5739357845658,13.2995215285911,10.7757173622757));
#48236=CARTESIAN_POINT('Ctrl Pts',(-10.391916652594,14.6154630132259,10.7075247959447));
#48237=CARTESIAN_POINT('Ctrl Pts',(-8.5189368031419,16.4631863186891,10.5869988538297));
#48238=CARTESIAN_POINT('Ctrl Pts',(-5.16549655959477,15.7560380892136,10.4299987264775));
#48239=CARTESIAN_POINT('Ctrl Pts',(-3.90540705298465,12.5688686867556,10.2729985991252));
#48240=CARTESIAN_POINT('Ctrl Pts',(-5.86863420589283,9.75968879265402,10.115998471773));
#48241=CARTESIAN_POINT('Ctrl Pts',(-9.29471725902464,9.84749381445728,9.9589983444207));
#48242=CARTESIAN_POINT('Ctrl Pts',(-10.5460795409153,11.8491727898316,9.85085770477057));
#48243=CARTESIAN_POINT('Ctrl Pts',(-10.5780867983696,12.9224107085984,9.79505044090452));
#48244=CARTESIAN_POINT('Ctrl Pts',(-10.5777630782332,12.9892372109846,9.79157655282255));
#48245=CARTESIAN_POINT('Origin',(-7.5,12.9903810567666,14.2084234471775));
#48246=CARTESIAN_POINT('',(-10.5702206634037,12.9870745539208,11.7915765528226));
#48247=CARTESIAN_POINT('',(-10.5771718362758,12.9919049495641,11.7084234471775));
#48248=CARTESIAN_POINT('',(-10.5735,12.9903810567666,14.2084234471775));
#48249=CARTESIAN_POINT('',(-8.29379928253292,10.0211581030209,12.));
#48250=CARTESIAN_POINT('Ctrl Pts',(-8.29379928253292,10.0211581030209,12.));
#48251=CARTESIAN_POINT('Ctrl Pts',(-9.27014005842312,10.2821754194981,11.9476666242159));
#48252=CARTESIAN_POINT('Ctrl Pts',(-10.3714991025232,11.3144735509882,11.8781921418234));
#48253=CARTESIAN_POINT('Ctrl Pts',(-10.5724953140326,12.655363779409,11.808717659431));
#48254=CARTESIAN_POINT('Ctrl Pts',(-10.5702206634037,12.9870745539208,11.7915765528226));
#48255=CARTESIAN_POINT('',(-6.70425858890745,10.0163809826708,12.));
#48256=CARTESIAN_POINT('Origin',(-7.5,12.9903810567666,12.));
#48257=CARTESIAN_POINT('Ctrl Pts',(-6.70425100699972,10.0163623331919,12.));
#48258=CARTESIAN_POINT('Ctrl Pts',(-7.63405880919358,9.77083750064795,11.9500021225376));
#48259=CARTESIAN_POINT('Ctrl Pts',(-9.69010226711413,10.2041387247117,11.8528099382634));
#48260=CARTESIAN_POINT('Ctrl Pts',(-10.5713066024909,12.0837656721183,11.7556177539892));
#48261=CARTESIAN_POINT('Ctrl Pts',(-10.5771718362758,12.9919049495641,11.7084234471775));
#48262=CARTESIAN_POINT('Origin',(15.,0.,7.5));
#48263=CARTESIAN_POINT('',(12.4864520394788,-8.37379766882585E-5,4.38741669750802));
#48264=CARTESIAN_POINT('',(12.4839933051997,-0.00316412607611227,4.11258330249198));
#48265=CARTESIAN_POINT('',(12.4825,3.08304831685346E-16,7.5));
#48266=CARTESIAN_POINT('',(13.086534003335,1.63598720337497,4.));
#48267=CARTESIAN_POINT('Ctrl Pts',(12.4839933051997,-0.00316412607611227,
4.11258330249198));
#48268=CARTESIAN_POINT('Ctrl Pts',(12.4891843965477,0.589325119423629,4.07505553499466));
#48269=CARTESIAN_POINT('Ctrl Pts',(12.700778171916,1.18480356030443,4.03752776749733));
#48270=CARTESIAN_POINT('Ctrl Pts',(13.086534003335,1.63598720337497,4.));
#48271=CARTESIAN_POINT('',(12.4825,3.08304831685346E-16,4.));
#48272=CARTESIAN_POINT('Origin',(15.,0.,4.));
#48273=CARTESIAN_POINT('',(12.4825,-3.08304831685346E-16,3.));
#48274=CARTESIAN_POINT('',(12.4825,3.08304831685346E-16,7.5));
#48275=CARTESIAN_POINT('Origin',(15.,0.,3.));
#48276=CARTESIAN_POINT('',(16.9169900003259,1.63831767401966,4.));
#48277=CARTESIAN_POINT('Origin',(15.,0.,4.));
#48278=CARTESIAN_POINT('Ctrl Pts',(16.9170033607455,1.63832650944338,4.));
#48279=CARTESIAN_POINT('Ctrl Pts',(16.4032792982694,2.23546892087832,4.04999787746244));
#48280=CARTESIAN_POINT('Ctrl Pts',(15.5859097998096,2.57572249729409,4.09999575492489));
#48281=CARTESIAN_POINT('Ctrl Pts',(14.8008208232653,2.51338129467797,4.14999363238733));
#48282=CARTESIAN_POINT('Ctrl Pts',(13.9790588101819,2.44812801296032,4.20232700817141));
#48283=CARTESIAN_POINT('Ctrl Pts',(13.1926635275253,1.94178951401471,4.2546603839555));
#48284=CARTESIAN_POINT('Ctrl Pts',(12.7937453701095,1.22068434196769,4.30699375973958));
#48285=CARTESIAN_POINT('Ctrl Pts',(12.5894005030727,0.851299951304611,4.3338014056624));
#48286=CARTESIAN_POINT('Ctrl Pts',(12.4867287035022,0.425561301199251,4.36060905158521));
#48287=CARTESIAN_POINT('Ctrl Pts',(12.4864520394788,-8.37379766882585E-5,
4.38741669750802));
#48288=CARTESIAN_POINT('Origin',(15.,0.,7.5));
#48289=CARTESIAN_POINT('',(12.4798657694311,-0.00154038945686864,5.38741669750803));
#48290=CARTESIAN_POINT('',(12.4793021139561,0.00120904389216911,5.11258330249198));
#48291=CARTESIAN_POINT('',(12.4825,3.08304831685346E-16,7.5));
#48292=CARTESIAN_POINT('Ctrl Pts',(12.4793021139561,0.00120904389216911,
5.11258330249198));
#48293=CARTESIAN_POINT('Ctrl Pts',(12.478879906904,0.0725686704440801,5.10805583214991));
#48294=CARTESIAN_POINT('Ctrl Pts',(12.4816538040259,0.14389470397244,5.10352836180784));
#48295=CARTESIAN_POINT('Ctrl Pts',(12.4877315613661,0.214937734438189,5.09900089146578));
#48296=CARTESIAN_POINT('Ctrl Pts',(12.5579848230722,1.0361295544392,5.04666751568169));
#48297=CARTESIAN_POINT('Ctrl Pts',(13.0696742764471,1.81950869898314,4.99433413989761));
#48298=CARTESIAN_POINT('Ctrl Pts',(13.7933805800141,2.21395750784665,4.94200076411352));
#48299=CARTESIAN_POINT('Ctrl Pts',(14.5170868835811,2.60840631671017,4.88966738832944));
#48300=CARTESIAN_POINT('Ctrl Pts',(15.4528100373402,2.61392478989326,4.83733401254535));
#48301=CARTESIAN_POINT('Ctrl Pts',(16.1810158838377,2.22781637405164,4.78500063676127));
#48302=CARTESIAN_POINT('Ctrl Pts',(16.9092217303351,1.84170795821001,4.73266726097718));
#48303=CARTESIAN_POINT('Ctrl Pts',(17.4299102695709,1.06397265334366,4.6803338851931));
#48304=CARTESIAN_POINT('Ctrl Pts',(17.5096246317311,0.243745210316159,4.62800050940901));
#48305=CARTESIAN_POINT('Ctrl Pts',(17.5893389938914,-0.576482232711353,
4.57566713362493));
#48306=CARTESIAN_POINT('Ctrl Pts',(17.2280791789763,-1.43920181390003,4.52333375784085));
#48307=CARTESIAN_POINT('Ctrl Pts',(16.5878264117224,-1.95845762325597,4.47100038205676));
#48308=CARTESIAN_POINT('Ctrl Pts',(15.9475736444685,-2.47771343261192,4.41866700627268));
#48309=CARTESIAN_POINT('Ctrl Pts',(15.0283279248759,-2.65350547013512,4.36633363048859));
#48310=CARTESIAN_POINT('Ctrl Pts',(14.2422049662735,-2.40531717421469,4.3140002547045));
#48311=CARTESIAN_POINT('Ctrl Pts',(13.4560820076711,-2.15712887829427,4.26166687892042));
#48312=CARTESIAN_POINT('Ctrl Pts',(12.8030818100589,-1.48496024893023,4.20933350313634));
#48313=CARTESIAN_POINT('Ctrl Pts',(12.5762083591215,-0.69397784322712,4.15700012735226));
#48314=CARTESIAN_POINT('Ctrl Pts',(12.5120237084102,-0.470201419766977,
4.1421945190655));
#48315=CARTESIAN_POINT('Ctrl Pts',(12.4819452946144,-0.236915405941376,
4.12738891077874));
#48316=CARTESIAN_POINT('Ctrl Pts',(12.4839933051997,-0.00316412607611227,
4.11258330249198));
#48317=CARTESIAN_POINT('Ctrl Pts',(12.4864520394788,-8.37379766882585E-5,
4.38741669750802));
#48318=CARTESIAN_POINT('Ctrl Pts',(12.4861886052651,-0.405374837317443,
4.41294242736929));
#48319=CARTESIAN_POINT('Ctrl Pts',(12.5787615741259,-0.810581064443052,
4.43846815723057));
#48320=CARTESIAN_POINT('Ctrl Pts',(12.7647943027407,-1.16697133984538,4.46399388709184));
#48321=CARTESIAN_POINT('Ctrl Pts',(13.146202424963,-1.897650004463,4.51632726287592));
#48322=CARTESIAN_POINT('Ctrl Pts',(13.9204597015827,-2.42313548854983,4.56866063866001));
#48323=CARTESIAN_POINT('Ctrl Pts',(14.7402998673034,-2.50800691661078,4.62099401444409));
#48324=CARTESIAN_POINT('Ctrl Pts',(15.560140033024,-2.59287834467174,4.67332739022818));
#48325=CARTESIAN_POINT('Ctrl Pts',(16.4255630878457,-2.23713571670682,4.72566076601226));
#48326=CARTESIAN_POINT('Ctrl Pts',(16.9486162247073,-1.60018404184685,4.77799414179635));
#48327=CARTESIAN_POINT('Ctrl Pts',(17.471669361569,-0.963232366986897,4.83032751758043));
#48328=CARTESIAN_POINT('Ctrl Pts',(17.6523525804706,-0.0450716452319087,
4.88266089336451));
#48329=CARTESIAN_POINT('Ctrl Pts',(17.4096229743894,0.742588180844264,4.9349942691486));
#48330=CARTESIAN_POINT('Ctrl Pts',(17.1668933683082,1.53024800692044,4.98732764493268));
#48331=CARTESIAN_POINT('Ctrl Pts',(16.5007509372442,2.1874069373178,5.03966102071677));
#48332=CARTESIAN_POINT('Ctrl Pts',(15.7098806230762,2.41944933284425,5.09199439650085));
#48333=CARTESIAN_POINT('Ctrl Pts',(14.9190103089082,2.6514917283707,5.14432777228493));
#48334=CARTESIAN_POINT('Ctrl Pts',(14.0034121116361,2.45841758902623,5.19666114806902));
#48335=CARTESIAN_POINT('Ctrl Pts',(13.3735902615222,1.92677994818613,5.2489945238531));
#48336=CARTESIAN_POINT('Ctrl Pts',(12.8182957469354,1.45805142494902,5.29513524840474));
#48337=CARTESIAN_POINT('Ctrl Pts',(12.4851467735748,0.72614376520494,5.34127597295639));
#48338=CARTESIAN_POINT('Ctrl Pts',(12.4798657694311,-0.00154038945686864,
5.38741669750803));
#48339=CARTESIAN_POINT('Origin',(15.,0.,7.5));
#48340=CARTESIAN_POINT('',(12.482920633805,0.00216662177004473,6.38741669750803));
#48341=CARTESIAN_POINT('',(12.4862854318642,0.000566909999415368,6.11258330249198));
#48342=CARTESIAN_POINT('',(12.4825,3.08304831685346E-16,7.5));
#48343=CARTESIAN_POINT('Ctrl Pts',(12.4862854318642,0.000566909999415368,
6.11258330249198));
#48344=CARTESIAN_POINT('Ctrl Pts',(12.4855058897774,0.379333771915191,6.08872275352109));
#48345=CARTESIAN_POINT('Ctrl Pts',(12.5659381445238,0.757786273313489,6.06486220455019));
#48346=CARTESIAN_POINT('Ctrl Pts',(12.7293101493446,1.09619859491376,6.04100165557929));
#48347=CARTESIAN_POINT('Ctrl Pts',(13.08763419844,1.83843881821599,5.98866827979521));
#48348=CARTESIAN_POINT('Ctrl Pts',(13.8449458114837,2.38806291012985,5.93633490401113));
#48349=CARTESIAN_POINT('Ctrl Pts',(14.6617006772638,2.49864636478707,5.88400152822704));
#48350=CARTESIAN_POINT('Ctrl Pts',(15.4784555430439,2.60922981944428,5.83166815244296));
#48351=CARTESIAN_POINT('Ctrl Pts',(16.3546536615603,2.28077263684485,5.77933477665887));
#48352=CARTESIAN_POINT('Ctrl Pts',(16.8974474362482,1.66053609593171,5.72700140087479));
#48353=CARTESIAN_POINT('Ctrl Pts',(17.4402412109362,1.04029955501857,5.6746680250907));
#48354=CARTESIAN_POINT('Ctrl Pts',(17.6496306417956,0.128283655791723,5.62233464930662));
#48355=CARTESIAN_POINT('Ctrl Pts',(17.4317349092204,-0.66659696383412,5.57000127352254));
#48356=CARTESIAN_POINT('Ctrl Pts',(17.2138391766452,-1.46147758345996,5.51766789773845));
#48357=CARTESIAN_POINT('Ctrl Pts',(16.5686582806354,-2.13922292348481,5.46533452195437));
#48358=CARTESIAN_POINT('Ctrl Pts',(15.7854622951236,-2.39597806232545,5.41300114617028));
#48359=CARTESIAN_POINT('Ctrl Pts',(15.0022663096119,-2.65273320116609,5.3606677703862));
#48360=CARTESIAN_POINT('Ctrl Pts',(14.0810552345983,-2.48849813882253,5.30833439460211));
#48361=CARTESIAN_POINT('Ctrl Pts',(13.4348582321103,-1.9768783599217,5.25600101881803));
#48362=CARTESIAN_POINT('Ctrl Pts',(12.8445650905918,-1.50951988350108,5.20819511337601));
#48363=CARTESIAN_POINT('Ctrl Pts',(12.4837602304949,-0.752282707918894,
5.160389207934));
#48364=CARTESIAN_POINT('Ctrl Pts',(12.4793021139561,0.00120904389216911,
5.11258330249198));
#48365=CARTESIAN_POINT('Ctrl Pts',(12.4798657694311,-0.00154038945686864,
5.38741669750803));
#48366=CARTESIAN_POINT('Ctrl Pts',(12.4791569938941,-0.0992045293459824,
5.39360934874047));
#48367=CARTESIAN_POINT('Ctrl Pts',(12.4843540819724,-0.196792591522919,
5.39980199997291));
#48368=CARTESIAN_POINT('Ctrl Pts',(12.4957126236098,-0.293658114991017,
5.40599465120536));
#48369=CARTESIAN_POINT('Ctrl Pts',(12.5917023387672,-1.11225739499233,5.45832802698944));
#48370=CARTESIAN_POINT('Ctrl Pts',(13.1277272720379,-1.87925481265923,5.51066140277353));
#48371=CARTESIAN_POINT('Ctrl Pts',(13.8634558058795,-2.25076673554666,5.56299477855761));
#48372=CARTESIAN_POINT('Ctrl Pts',(14.5991843397211,-2.62227865843409,5.61532815434169));
#48373=CARTESIAN_POINT('Ctrl Pts',(15.5346164741336,-2.59830508654206,5.66766153012578));
#48374=CARTESIAN_POINT('Ctrl Pts',(16.2503478880118,-2.18959297269902,5.71999490590987));
#48375=CARTESIAN_POINT('Ctrl Pts',(16.96607930189,-1.78088085885597,5.77232828169395));
#48376=CARTESIAN_POINT('Ctrl Pts',(17.4621099952338,-0.98743020306191,5.82466165747803));
#48377=CARTESIAN_POINT('Ctrl Pts',(17.5160416303984,-0.16498929182795,5.87699503326212));
#48378=CARTESIAN_POINT('Ctrl Pts',(17.5699732655631,0.657451619406004,5.9293284090462));
#48379=CARTESIAN_POINT('Ctrl Pts',(17.1818058425485,1.50888278607985,5.98166178483029));
#48380=CARTESIAN_POINT('Ctrl Pts',(16.5255763936941,2.00756141147231,6.03399516061437));
#48381=CARTESIAN_POINT('Ctrl Pts',(15.8693469448397,2.50624003686478,6.08632853639846));
#48382=CARTESIAN_POINT('Ctrl Pts',(14.9450554701454,2.65216612097585,6.13866191218254));
#48383=CARTESIAN_POINT('Ctrl Pts',(14.1671123287709,2.37991277262463,6.19099528796662));
#48384=CARTESIAN_POINT('Ctrl Pts',(13.3891691873965,2.10765942427341,6.24332866375071));
#48385=CARTESIAN_POINT('Ctrl Pts',(12.7575743793418,1.41722664345988,6.2956620395348));
#48386=CARTESIAN_POINT('Ctrl Pts',(12.5555065470498,0.618173398042358,6.34799541531888));
#48387=CARTESIAN_POINT('Ctrl Pts',(12.5047691803197,0.417538506829285,6.36113584271526));
#48388=CARTESIAN_POINT('Ctrl Pts',(12.4811120172555,0.210055467607507,6.37427627011165));
#48389=CARTESIAN_POINT('Ctrl Pts',(12.482920633805,0.00216662177004473,
6.38741669750803));
#48390=CARTESIAN_POINT('Origin',(15.,0.,7.5));
#48391=CARTESIAN_POINT('',(12.4854953774899,-0.00143787083715985,7.38741669750803));
#48392=CARTESIAN_POINT('',(12.4810882026093,-0.00198272270578489,7.11258330249199));
#48393=CARTESIAN_POINT('',(12.4825,3.08304831685346E-16,7.5));
#48394=CARTESIAN_POINT('Ctrl Pts',(12.4810882026093,-0.00198272270578489,
7.11258330249199));
#48395=CARTESIAN_POINT('Ctrl Pts',(12.4869739395021,0.680084118616307,7.06938967489226));
#48396=CARTESIAN_POINT('Ctrl Pts',(12.7744552727444,1.36652561897882,7.02619604729254));
#48397=CARTESIAN_POINT('Ctrl Pts',(13.269118044078,1.83350231786092,6.98300241969281));
#48398=CARTESIAN_POINT('Ctrl Pts',(13.8684511896637,2.39929103307328,6.93066904390873));
#48399=CARTESIAN_POINT('Ctrl Pts',(14.7719211435091,2.64291129119537,6.87833566812465));
#48400=CARTESIAN_POINT('Ctrl Pts',(15.5744528177492,2.45513481925728,6.82600229234056));
#48401=CARTESIAN_POINT('Ctrl Pts',(16.3769844919893,2.26735834731918,6.77366891655648));
#48402=CARTESIAN_POINT('Ctrl Pts',(17.0785778866242,1.64818514532091,6.72133554077239));
#48403=CARTESIAN_POINT('Ctrl Pts',(17.3646702383797,0.875224413728682,6.66900216498831));
#48404=CARTESIAN_POINT('Ctrl Pts',(17.6507625901351,0.102263682136454,6.61666878920422));
#48405=CARTESIAN_POINT('Ctrl Pts',(17.5213538990113,-0.82448457904973,6.56433541342014));
#48406=CARTESIAN_POINT('Ctrl Pts',(17.0344651712476,-1.48950819606356,6.51200203763606));
#48407=CARTESIAN_POINT('Ctrl Pts',(16.547576443484,-2.15453181307739,6.45966866185197));
#48408=CARTESIAN_POINT('Ctrl Pts',(15.7032076790805,-2.55783078591888,6.40733528606789));
#48409=CARTESIAN_POINT('Ctrl Pts',(14.8799356660918,-2.51858436884117,6.3550019102838));
#48410=CARTESIAN_POINT('Ctrl Pts',(14.0566636531032,-2.47933795176346,6.30266853449972));
#48411=CARTESIAN_POINT('Ctrl Pts',(13.2544883915292,-1.99754614476656,6.25033515871564));
#48412=CARTESIAN_POINT('Ctrl Pts',(12.8330690033158,-1.28922206392281,6.19800178293155));
#48413=CARTESIAN_POINT('Ctrl Pts',(12.6037889105156,-0.903846792801687,
6.16952895611836));
#48414=CARTESIAN_POINT('Ctrl Pts',(12.4872156605381,-0.451416121701059,
6.14105612930517));
#48415=CARTESIAN_POINT('Ctrl Pts',(12.4862854318642,0.000566909999415368,
6.11258330249198));
#48416=CARTESIAN_POINT('Ctrl Pts',(12.482920633805,0.00216662177004473,
6.38741669750803));
#48417=CARTESIAN_POINT('Ctrl Pts',(12.488315056143,-0.617887548426095,6.42660964589573));
#48418=CARTESIAN_POINT('Ctrl Pts',(12.7202541571503,-1.24155179185567,6.46580259428343));
#48419=CARTESIAN_POINT('Ctrl Pts',(13.1359015380453,-1.69788793113621,6.50499554267113));
#48420=CARTESIAN_POINT('Ctrl Pts',(13.6909052178623,-2.30722230487577,6.55732891845522));
#48421=CARTESIAN_POINT('Ctrl Pts',(14.5734534340258,-2.61821734233337,6.6096622942393));
#48422=CARTESIAN_POINT('Ctrl Pts',(15.3878514816524,-2.49143689543374,6.66199567002338));
#48423=CARTESIAN_POINT('Ctrl Pts',(16.2022495292791,-2.36465644853411,6.71432904580747));
#48424=CARTESIAN_POINT('Ctrl Pts',(16.9484974083689,-1.80010051727723,6.76666242159155));
#48425=CARTESIAN_POINT('Ctrl Pts',(17.2920112918525,-1.05089047753226,6.81899579737564));
#48426=CARTESIAN_POINT('Ctrl Pts',(17.635525175336,-0.301680437787271,6.87132917315973));
#48427=CARTESIAN_POINT('Ctrl Pts',(17.5763050632133,0.632183710445827,6.92366254894381));
#48428=CARTESIAN_POINT('Ctrl Pts',(17.1409025824082,1.33199950499447,6.97599592472789));
#48429=CARTESIAN_POINT('Ctrl Pts',(16.7055001016032,2.03181529954311,7.02832930051198));
#48430=CARTESIAN_POINT('Ctrl Pts',(15.8939152521159,2.49758274040729,7.08066267629606));
#48431=CARTESIAN_POINT('Ctrl Pts',(15.0700259913432,2.52047275706227,7.13299605208015));
#48432=CARTESIAN_POINT('Ctrl Pts',(14.2461367305706,2.54336277371724,7.18532942786423));
#48433=CARTESIAN_POINT('Ctrl Pts',(13.4099430585124,2.12337536616301,7.23766280364831));
#48434=CARTESIAN_POINT('Ctrl Pts',(12.9363564205467,1.44881390534349,7.2899961794324));
#48435=CARTESIAN_POINT('Ctrl Pts',(12.6424900625863,1.03024018763275,7.32246968545761));
#48436=CARTESIAN_POINT('Ctrl Pts',(12.4882403133338,0.513646402355209,7.35494319148282));
#48437=CARTESIAN_POINT('Ctrl Pts',(12.4854953774899,-0.00143787083715985,
7.38741669750803));
#48438=CARTESIAN_POINT('Origin',(15.,0.,7.5));
#48439=CARTESIAN_POINT('',(12.4785663033905,-0.000147683907944251,8.38741669750803));
#48440=CARTESIAN_POINT('',(12.4815651121962,0.00207920831391662,8.11258330249198));
#48441=CARTESIAN_POINT('',(12.4825,3.08304831685346E-16,7.5));
#48442=CARTESIAN_POINT('Ctrl Pts',(12.4815651121962,0.00207920831391661,
8.11258330249198));
#48443=CARTESIAN_POINT('Ctrl Pts',(12.4801423769425,0.163120151964822,8.10238997204752));
#48444=CARTESIAN_POINT('Ctrl Pts',(12.4942993050251,0.323912101526709,8.09219664160305));
#48445=CARTESIAN_POINT('Ctrl Pts',(12.524955296352,0.48149432911561,8.08200331115859));
#48446=CARTESIAN_POINT('Ctrl Pts',(12.6823456137647,1.29053412020584,8.0296699353745));
#48447=CARTESIAN_POINT('Ctrl Pts',(13.27463109749,2.01496955827445,7.97733655959042));
#48448=CARTESIAN_POINT('Ctrl Pts',(14.036257709891,2.32999653926404,7.92500318380634));
#48449=CARTESIAN_POINT('Ctrl Pts',(14.797884322292,2.64502352025364,7.87266980802225));
#48450=CARTESIAN_POINT('Ctrl Pts',(15.7288520633688,2.55064204416424,7.82033643223817));
#48451=CARTESIAN_POINT('Ctrl Pts',(16.4117570807264,2.08916849927148,7.76800305645408));
#48452=CARTESIAN_POINT('Ctrl Pts',(17.0946620980841,1.62769495437873,7.71566968067));
#48453=CARTESIAN_POINT('Ctrl Pts',(17.5295043917226,0.799129340682624,7.66333630488591));
#48454=CARTESIAN_POINT('Ctrl Pts',(17.5213203334702,-0.0250369758568184,
7.61100292910183));
#48455=CARTESIAN_POINT('Ctrl Pts',(17.5131362752179,-0.849203292396252,
7.55866955331774));
#48456=CARTESIAN_POINT('Ctrl Pts',(17.0619258650746,-1.66897031177902,7.50633617753366));
#48457=CARTESIAN_POINT('Ctrl Pts',(16.3699914547578,-2.11679155594354,7.45400280174958));
#48458=CARTESIAN_POINT('Ctrl Pts',(15.678057044441,-2.56461280010805,7.4016694259655));
#48459=CARTESIAN_POINT('Ctrl Pts',(14.7453986339507,-2.6404882690543,7.34933605018141));
#48460=CARTESIAN_POINT('Ctrl Pts',(13.9901780954356,-2.31039883752012,7.29700267439732));
#48461=CARTESIAN_POINT('Ctrl Pts',(13.2349575569204,-1.98030940598595,7.24466929861324));
#48462=CARTESIAN_POINT('Ctrl Pts',(12.6571748903804,-1.24425507397135,7.19233592282916));
#48463=CARTESIAN_POINT('Ctrl Pts',(12.5158817257734,-0.43224932181273,7.14000254704507));
#48464=CARTESIAN_POINT('Ctrl Pts',(12.4912056194582,-0.29043679801142,7.13086279886071));
#48465=CARTESIAN_POINT('Ctrl Pts',(12.4798427838735,-0.146307696573625,
7.12172305067635));
#48466=CARTESIAN_POINT('Ctrl Pts',(12.4810882026093,-0.00198272270578489,
7.11258330249199));
#48467=CARTESIAN_POINT('Ctrl Pts',(12.4854953774899,-0.00143787083715985,
7.38741669750803));
#48468=CARTESIAN_POINT('Ctrl Pts',(12.4838166530455,-0.316448716062932,
7.4072765672669));
#48469=CARTESIAN_POINT('Ctrl Pts',(12.5388037075173,-0.630894974090679,
7.42713643702578));
#48470=CARTESIAN_POINT('Ctrl Pts',(12.6531758459131,-0.922010273445696,
7.44699630678465));
#48471=CARTESIAN_POINT('Ctrl Pts',(12.9545615131189,-1.68913747733048,7.49932968256874));
#48472=CARTESIAN_POINT('Ctrl Pts',(13.6683124514037,-2.29425637101525,7.55166305835282));
#48473=CARTESIAN_POINT('Ctrl Pts',(14.474415004267,-2.46605899527454,7.6039964341369));
#48474=CARTESIAN_POINT('Ctrl Pts',(15.2805175571303,-2.63786161953383,7.65632980992099));
#48475=CARTESIAN_POINT('Ctrl Pts',(16.1789717245721,-2.37634797436764,7.70866318570507));
#48476=CARTESIAN_POINT('Ctrl Pts',(16.766951270731,-1.79876895739606,7.76099656148916));
#48477=CARTESIAN_POINT('Ctrl Pts',(17.35493081689,-1.22118994042448,7.81332993727324));
#48478=CARTESIAN_POINT('Ctrl Pts',(17.6324357417662,-0.327545551647488,
7.86566331305733));
#48479=CARTESIAN_POINT('Ctrl Pts',(17.4750453812635,0.48149446094025,7.91799668884141));
#48480=CARTESIAN_POINT('Ctrl Pts',(17.3176550207607,1.290534473528,7.97033006462549));
#48481=CARTESIAN_POINT('Ctrl Pts',(16.7253693748791,2.01497010992651,8.02266344040958));
#48482=CARTESIAN_POINT('Ctrl Pts',(15.9637425539609,2.32999717716545,8.07499681619367));
#48483=CARTESIAN_POINT('Ctrl Pts',(15.2021157330427,2.64502424440439,8.12733019197775));
#48484=CARTESIAN_POINT('Ctrl Pts',(14.271147737088,2.55064274248376,8.17966356776183));
#48485=CARTESIAN_POINT('Ctrl Pts',(13.5882425327649,2.08916907124602,8.23199694354592));
#48486=CARTESIAN_POINT('Ctrl Pts',(12.9122114961964,1.63234062369425,8.28380352819995));
#48487=CARTESIAN_POINT('Ctrl Pts',(12.4792743543203,0.815773157793952,8.33561011285399));
#48488=CARTESIAN_POINT('Ctrl Pts',(12.4785663033905,-0.000147683907944251,
8.38741669750803));
#48489=CARTESIAN_POINT('Origin',(15.,0.,7.5));
#48490=CARTESIAN_POINT('',(12.4851788739807,0.00162480267774629,9.38741669750802));
#48491=CARTESIAN_POINT('',(12.486145438329,-0.000815058042068406,9.11258330249198));
#48492=CARTESIAN_POINT('',(12.4825,3.08304831685346E-16,7.5));
#48493=CARTESIAN_POINT('Ctrl Pts',(12.486145438329,-0.000815058042068406,
9.11258330249198));
#48494=CARTESIAN_POINT('Ctrl Pts',(12.4875376300823,0.467827170949961,9.08305689341869));
#48495=CARTESIAN_POINT('Ctrl Pts',(12.6134446697461,0.937164267550756,9.0535304843454));
#48496=CARTESIAN_POINT('Ctrl Pts',(12.8590980037376,1.33199914029708,9.02400407527211));
#48497=CARTESIAN_POINT('Ctrl Pts',(13.2945003653482,2.03181474323085,8.97167069948803));
#48498=CARTESIAN_POINT('Ctrl Pts',(14.1060849926179,2.49758205662421,8.91933732370394));
#48499=CARTESIAN_POINT('Ctrl Pts',(14.9299740278219,2.52047206702312,8.86700394791986));
#48500=CARTESIAN_POINT('Ctrl Pts',(15.753863063026,2.54336207742203,8.81467057213577));
#48501=CARTESIAN_POINT('Ctrl Pts',(16.5900565061644,2.12337478482649,8.76233719635169));
#48502=CARTESIAN_POINT('Ctrl Pts',(17.063643014475,1.44881350868189,8.7100038205676));
#48503=CARTESIAN_POINT('Ctrl Pts',(17.5372295227856,0.774252232537298,8.65767044478352));
#48504=CARTESIAN_POINT('Ctrl Pts',(17.6482090962684,-0.154883027156347,
8.60533706899943));
#48505=CARTESIAN_POINT('Ctrl Pts',(17.3468235115742,-0.922010021015011,
8.55300369321535));
#48506=CARTESIAN_POINT('Ctrl Pts',(17.0454379268799,-1.68913701487367,8.50067031743127));
#48507=CARTESIAN_POINT('Ctrl Pts',(16.3316871840086,-2.29425574289735,8.44833694164718));
#48508=CARTESIAN_POINT('Ctrl Pts',(15.5255848518399,-2.46605832012208,8.3960035658631));
#48509=CARTESIAN_POINT('Ctrl Pts',(14.7194825196712,-2.6378608973468,8.34367019007902));
#48510=CARTESIAN_POINT('Ctrl Pts',(13.8210285982051,-2.37634732377256,8.29133681429493));
#48511=CARTESIAN_POINT('Ctrl Pts',(13.2330492130222,-1.79876846492951,8.23900343851085));
#48512=CARTESIAN_POINT('Ctrl Pts',(12.7595946043877,-1.33368860080475,8.19686339317123));
#48513=CARTESIAN_POINT('Ctrl Pts',(12.4874468138073,-0.663676964701131,
8.1547233478316));
#48514=CARTESIAN_POINT('Ctrl Pts',(12.4815651121962,0.00207920831391661,
8.11258330249198));
#48515=CARTESIAN_POINT('Ctrl Pts',(12.4785663033905,-0.000147683907944251,
8.38741669750803));
#48516=CARTESIAN_POINT('Ctrl Pts',(12.478559103631,-0.0084443100048087,
8.38794348863808));
#48517=CARTESIAN_POINT('Ctrl Pts',(12.4785965949646,-0.016740869242818,
8.38847027976812));
#48518=CARTESIAN_POINT('Ctrl Pts',(12.4786789762444,-0.0250369827190495,
8.38899707089817));
#48519=CARTESIAN_POINT('Ctrl Pts',(12.4868630367383,-0.84920352489154,8.44133044668226));
#48520=CARTESIAN_POINT('Ctrl Pts',(12.9380735704173,-1.66897076868167,8.49366382246634));
#48521=CARTESIAN_POINT('Ctrl Pts',(13.6300081701693,-2.11679213546203,8.54599719825043));
#48522=CARTESIAN_POINT('Ctrl Pts',(14.3219427699214,-2.5646135022424,8.59833057403451));
#48523=CARTESIAN_POINT('Ctrl Pts',(15.2546014357464,-2.64048899201301,8.65066394981859));
#48524=CARTESIAN_POINT('Ctrl Pts',(16.0098221810285,-2.31039947008532,8.70299732560268));
#48525=CARTESIAN_POINT('Ctrl Pts',(16.7650429263106,-1.98030994815763,8.75533070138676));
#48526=CARTESIAN_POINT('Ctrl Pts',(17.3428257510498,-1.24425541453165,8.80766407717086));
#48527=CARTESIAN_POINT('Ctrl Pts',(17.4841189543331,-0.432249440103775,
8.85999745295494));
#48528=CARTESIAN_POINT('Ctrl Pts',(17.6254121576165,0.379756534324098,8.91233082873902));
#48529=CARTESIAN_POINT('Ctrl Pts',(17.3302157394439,1.26771394955386,8.9646642045231));
#48530=CARTESIAN_POINT('Ctrl Pts',(16.7308824297867,1.83350281974262,9.01699758030718));
#48531=CARTESIAN_POINT('Ctrl Pts',(16.1315491201295,2.39929168993138,9.06933095609127));
#48532=CARTESIAN_POINT('Ctrl Pts',(15.2280789189876,2.64291201507916,9.12166433187536));
#48533=CARTESIAN_POINT('Ctrl Pts',(14.4255470250055,2.45513549159302,9.17399770765945));
#48534=CARTESIAN_POINT('Ctrl Pts',(13.6230151310234,2.26735896810689,9.22633108344353));
#48535=CARTESIAN_POINT('Ctrl Pts',(12.9214215442012,1.64818559598687,9.2786644592276));
#48536=CARTESIAN_POINT('Ctrl Pts',(12.6353291141696,0.875224653029136,9.33099783501169));
#48537=CARTESIAN_POINT('Ctrl Pts',(12.5325202200407,0.597456870981902,9.34980412251047));
#48538=CARTESIAN_POINT('Ctrl Pts',(12.4833676454127,0.29982951718309,9.36861041000924));
#48539=CARTESIAN_POINT('Ctrl Pts',(12.4851788739807,0.00162480267774629,
9.38741669750802));
#48540=CARTESIAN_POINT('Origin',(15.,0.,7.5));
#48541=CARTESIAN_POINT('',(12.4833920687165,-0.00213593309729046,10.387416697508));
#48542=CARTESIAN_POINT('',(12.4790122776664,-0.000936909191352325,10.112583302492));
#48543=CARTESIAN_POINT('',(12.4825,3.08304831685346E-16,7.5));
#48544=CARTESIAN_POINT('Ctrl Pts',(12.4790122776664,-0.000936909191352325,
10.112583302492));
#48545=CARTESIAN_POINT('Ctrl Pts',(12.4827416706421,0.768933033990792,10.0637238147899));
#48546=CARTESIAN_POINT('Ctrl Pts',(12.8617552362247,1.54198463745441,10.0148643270877));
#48547=CARTESIAN_POINT('Ctrl Pts',(13.4744240244193,2.00756086084053,9.96600483938563));
#48548=CARTESIAN_POINT('Ctrl Pts',(14.1306532939369,2.50623934889895,9.91367146360154));
#48549=CARTESIAN_POINT('Ctrl Pts',(15.0549445147503,2.65216539497217,9.86133808781746));
#48550=CARTESIAN_POINT('Ctrl Pts',(15.8328874429565,2.37991212159725,9.80900471203338));
#48551=CARTESIAN_POINT('Ctrl Pts',(16.6108303711627,2.10765884822232,9.75667133624929));
#48552=CARTESIAN_POINT('Ctrl Pts',(17.2424250067619,1.41722625539925,9.70433796046521));
#48553=CARTESIAN_POINT('Ctrl Pts',(17.4444927838351,0.618173228507267,9.65200458468112));
#48554=CARTESIAN_POINT('Ctrl Pts',(17.6465605609084,-0.18087979838472,9.59967120889704));
#48555=CARTESIAN_POINT('Ctrl Pts',(17.4191014794558,-1.08855325934562,9.54733783311295));
#48556=CARTESIAN_POINT('Ctrl Pts',(16.8640979515296,-1.69788746613335,9.49500445732887));
#48557=CARTESIAN_POINT('Ctrl Pts',(16.3090944236034,-2.30722167292107,9.44267108154478));
#48558=CARTESIAN_POINT('Ctrl Pts',(15.4265464492036,-2.61821662553562,9.3903377057607));
#48559=CARTESIAN_POINT('Ctrl Pts',(14.6121486245737,-2.49143621341537,9.33800432997662));
#48560=CARTESIAN_POINT('Ctrl Pts',(13.7977507999438,-2.36465580129513,9.28567095419253));
#48561=CARTESIAN_POINT('Ctrl Pts',(13.0515031250838,-1.80010002444009,9.23333757840845));
#48562=CARTESIAN_POINT('Ctrl Pts',(12.7079893356296,-1.05089018977548,9.18100420262436));
#48563=CARTESIAN_POINT('Ctrl Pts',(12.5582854909339,-0.724383376435316,
9.15819723591357));
#48564=CARTESIAN_POINT('Ctrl Pts',(12.4850700731909,-0.362806510824638,
9.13539026920278));
#48565=CARTESIAN_POINT('Ctrl Pts',(12.486145438329,-0.000815058042068406,
9.11258330249198));
#48566=CARTESIAN_POINT('Ctrl Pts',(12.4851788739807,0.00162480267774629,
9.38741669750802));
#48567=CARTESIAN_POINT('Ctrl Pts',(12.4884078589736,-0.530002494361348,
9.42094378579333));
#48568=CARTESIAN_POINT('Ctrl Pts',(12.6536116109961,-1.06346477741145,9.45447087407864));
#48569=CARTESIAN_POINT('Ctrl Pts',(12.9655342718635,-1.48950860327335,9.48799796236395));
#48570=CARTESIAN_POINT('Ctrl Pts',(13.4524231328298,-2.15453240282264,9.54033133814804));
#48571=CARTESIAN_POINT('Ctrl Pts',(14.2967921280032,-2.55783148812579,9.59266471393212));
#48572=CARTESIAN_POINT('Ctrl Pts',(15.1200643665754,-2.51858505945467,9.6449980897162));
#48573=CARTESIAN_POINT('Ctrl Pts',(15.9433366051476,-2.47933863078355,9.69733146550028));
#48574=CARTESIAN_POINT('Ctrl Pts',(16.7455120871185,-1.99754668813814,9.74966484128436));
#48575=CARTESIAN_POINT('Ctrl Pts',(17.1669315903404,-1.28922241490791,9.80199821706845));
#48576=CARTESIAN_POINT('Ctrl Pts',(17.5883510935622,-0.580898141677671,
9.85433159285254));
#48577=CARTESIAN_POINT('Ctrl Pts',(17.6290146180349,0.353958462137397,9.90666496863663));
#48578=CARTESIAN_POINT('Ctrl Pts',(17.2706904715522,1.09619889141998,9.95899834442071));
#48579=CARTESIAN_POINT('Ctrl Pts',(16.9123663250695,1.83843932070257,10.0113317202048));
#48580=CARTESIAN_POINT('Ctrl Pts',(16.1550545076315,2.38806357545267,10.0636650959889));
#48581=CARTESIAN_POINT('Ctrl Pts',(15.3382994168527,2.49864705542611,10.115998471773));
#48582=CARTESIAN_POINT('Ctrl Pts',(14.5215443260739,2.60923053539955,10.168331847557));
#48583=CARTESIAN_POINT('Ctrl Pts',(13.6453459619542,2.28077324059635,10.2206652233411));
#48584=CARTESIAN_POINT('Ctrl Pts',(13.1025520413601,1.66053653868267,10.2729985991252));
#48585=CARTESIAN_POINT('Ctrl Pts',(12.7069762589991,1.20852223030592,10.3111379652528));
#48586=CARTESIAN_POINT('Ctrl Pts',(12.4884769342622,0.601539190041919,10.3492773313804));
#48587=CARTESIAN_POINT('Ctrl Pts',(12.4833920687165,-0.00213593309729046,
10.387416697508));
#48588=CARTESIAN_POINT('Origin',(15.,0.,7.5));
#48589=CARTESIAN_POINT('',(12.4794948718273,0.00124609658704006,11.387416697508));
#48590=CARTESIAN_POINT('',(12.4841021658346,0.00201143405015815,11.112583302492));
#48591=CARTESIAN_POINT('',(12.4825,3.08304831685346E-16,7.5));
#48592=CARTESIAN_POINT('',(16.9134659966651,1.63598720337492,12.));
#48593=CARTESIAN_POINT('Ctrl Pts',(12.4794948718273,0.00124609658704006,
11.387416697508));
#48594=CARTESIAN_POINT('Ctrl Pts',(12.4843009282632,-0.742606326482963,
11.4346110043198));
#48595=CARTESIAN_POINT('Ctrl Pts',(12.8347911135691,-1.49019380442116,11.4818053111315));
#48596=CARTESIAN_POINT('Ctrl Pts',(13.4121725655462,-1.95845906653105,11.5289996179432));
#48597=CARTESIAN_POINT('Ctrl Pts',(14.0524260736147,-2.47771453576351,11.5813329937273));
#48598=CARTESIAN_POINT('Ctrl Pts',(14.971674348053,-2.65350400257885,11.6336663695114));
#48599=CARTESIAN_POINT('Ctrl Pts',(15.7577964008607,-2.4053165320775,11.6859997452955));
#48600=CARTESIAN_POINT('Ctrl Pts',(16.5439184536685,-2.15712906157615,11.7383331210796));
#48601=CARTESIAN_POINT('Ctrl Pts',(17.1969142848456,-1.4849646537581,11.7906664968637));
#48602=CARTESIAN_POINT('Ctrl Pts',(17.4237876204482,-0.693982202234524,
11.8429998726477));
#48603=CARTESIAN_POINT('Ctrl Pts',(17.6506609560507,0.0970002492890512,
11.8953332484318));
#48604=CARTESIAN_POINT('Ctrl Pts',(17.4514117960785,1.00680074451815,11.9476666242159));
#48605=CARTESIAN_POINT('Ctrl Pts',(16.9134659966651,1.63598720337493,12.));
#48606=CARTESIAN_POINT('',(13.0830107080184,1.63831915944298,12.));
#48607=CARTESIAN_POINT('Origin',(15.,0.,12.));
#48608=CARTESIAN_POINT('Ctrl Pts',(13.0829974340784,1.63832794503776,12.));
#48609=CARTESIAN_POINT('Ctrl Pts',(13.5967216860793,2.23547110522819,11.9500021225376));
#48610=CARTESIAN_POINT('Ctrl Pts',(14.4140905740858,2.57572139725963,11.9000042450751));
#48611=CARTESIAN_POINT('Ctrl Pts',(15.1991791514308,2.51337952595466,11.8500063676127));
#48612=CARTESIAN_POINT('Ctrl Pts',(16.0209407466675,2.44812554431239,11.7976729918286));
#48613=CARTESIAN_POINT('Ctrl Pts',(16.8073358429282,1.94178921121356,11.7453396160445));
#48614=CARTESIAN_POINT('Ctrl Pts',(17.2062539503585,1.22068465472099,11.6930062402604));
#48615=CARTESIAN_POINT('Ctrl Pts',(17.6051720577887,0.499580098228415,11.6406728644763));
#48616=CARTESIAN_POINT('Ctrl Pts',(17.6166131763885,-0.436292681657898,
11.5883394886922));
#48617=CARTESIAN_POINT('Ctrl Pts',(17.2352051529428,-1.16697139580525,11.5360061129082));
#48618=CARTESIAN_POINT('Ctrl Pts',(16.853797129497,-1.8976501099526,11.4836727371241));
#48619=CARTESIAN_POINT('Ctrl Pts',(16.0795399640059,-2.42313475836099,11.43133936134));
#48620=CARTESIAN_POINT('Ctrl Pts',(15.259700012361,-2.508006015706,11.3790059855559));
#48621=CARTESIAN_POINT('Ctrl Pts',(14.439860060716,-2.59287727305101,11.3266726097718));
#48622=CARTESIAN_POINT('Ctrl Pts',(13.5744373229174,-2.23713513933264,11.2743392339877));
#48623=CARTESIAN_POINT('Ctrl Pts',(13.0513843414681,-1.60018372469102,11.2220058582037));
#48624=CARTESIAN_POINT('Ctrl Pts',(12.6868381785572,-1.15625509336019,11.1855316729664));
#48625=CARTESIAN_POINT('Ctrl Pts',(12.488598465426,-0.575728774038117,11.1490574877292));
#48626=CARTESIAN_POINT('Ctrl Pts',(12.4841021658346,0.00201143405015815,
11.112583302492));
#48627=CARTESIAN_POINT('Origin',(15.,0.,14.2084234471775));
#48628=CARTESIAN_POINT('',(11.9225958479619,0.00147606609843115,4.79157655282255));
#48629=CARTESIAN_POINT('',(11.9313248632922,-0.000102231845577353,4.70842344717745));
#48630=CARTESIAN_POINT('',(11.9265,6.70613782525944E-14,14.2084234471775));
#48631=CARTESIAN_POINT('',(15.7937992825329,-2.9692229537457,4.));
#48632=CARTESIAN_POINT('Ctrl Pts',(11.9313248632922,-0.000102231845577234,
4.70842344717745));
#48633=CARTESIAN_POINT('Ctrl Pts',(11.9316626296779,0.519548226111607,4.68161580125464));
#48634=CARTESIAN_POINT('Ctrl Pts',(12.3017104806267,2.0539878015009,4.60247477954774));
#48635=CARTESIAN_POINT('Ctrl Pts',(14.713653685934,3.60697232347283,4.47100038205677));
#48636=CARTESIAN_POINT('Ctrl Pts',(17.8529409071999,2.23046453345384,4.3140002547045));
#48637=CARTESIAN_POINT('Ctrl Pts',(18.4294036968932,-1.15306868324745,4.15700012735226));
#48638=CARTESIAN_POINT('Ctrl Pts',(16.7701400584231,-2.7082056372685,4.05233337578409));
#48639=CARTESIAN_POINT('Ctrl Pts',(15.7937992825329,-2.9692229537457,4.));
#48640=CARTESIAN_POINT('',(14.2042685477155,-2.9740056618826,4.));
#48641=CARTESIAN_POINT('Origin',(15.,0.,4.));
#48642=CARTESIAN_POINT('Ctrl Pts',(11.9225958479619,0.00147606609843164,
4.79157655282255));
#48643=CARTESIAN_POINT('Ctrl Pts',(11.9220803947843,0.0885957531718082,
4.78704908248048));
#48644=CARTESIAN_POINT('Ctrl Pts',(11.9646120017673,1.18222348786824,4.73018823635433));
#48645=CARTESIAN_POINT('Ctrl Pts',(13.2680522040149,3.17774609218688,4.62099401444409));
#48646=CARTESIAN_POINT('Ctrl Pts',(16.6951963308219,3.19795784272698,4.46399388709183));
#48647=CARTESIAN_POINT('Ctrl Pts',(18.6022504225887,0.349454018091392,4.30699375973959));
#48648=CARTESIAN_POINT('Ctrl Pts',(17.2987966073653,-2.76330605967289,4.15232913070897));
#48649=CARTESIAN_POINT('Ctrl Pts',(15.1340732479013,-3.21955219912907,4.04999787746244));
#48650=CARTESIAN_POINT('Ctrl Pts',(14.2042612683071,-2.97402368063355,4.));
#48651=CARTESIAN_POINT('Origin',(15.,0.,14.2084234471775));
#48652=CARTESIAN_POINT('',(11.9311214597158,0.000692114352876805,5.79157655282255));
#48653=CARTESIAN_POINT('',(11.9232839890155,-0.001880590663607,5.70842344717745));
#48654=CARTESIAN_POINT('',(11.9265,6.70613782525944E-14,14.2084234471775));
#48655=CARTESIAN_POINT('Ctrl Pts',(11.9232839890155,-0.00188059066360697,
5.70842344717745));
#48656=CARTESIAN_POINT('Ctrl Pts',(11.9297313241637,0.88651553618964,5.66228272262581));
#48657=CARTESIAN_POINT('Ctrl Pts',(12.7977715060129,2.79354605065376,5.56380862229009));
#48658=CARTESIAN_POINT('Ctrl Pts',(16.0189351514379,3.47279968000896,5.41300114617029));
#48659=CARTESIAN_POINT('Ctrl Pts',(18.4587231497003,1.06591431050395,5.25600101881802));
#48660=CARTESIAN_POINT('Ctrl Pts',(17.7969596462713,-2.29690631906584,5.09900089146578));
#48661=CARTESIAN_POINT('Ctrl Pts',(14.6272939950368,-3.59983577334609,4.94200076411352));
#48662=CARTESIAN_POINT('Ctrl Pts',(12.2757333222409,-2.00384044231271,4.81180828268409));
#48663=CARTESIAN_POINT('Ctrl Pts',(11.9310032485729,-0.494903500494573,
4.73394917703873));
#48664=CARTESIAN_POINT('Ctrl Pts',(11.9313248632922,-0.000102231845577234,
4.70842344717745));
#48665=CARTESIAN_POINT('Ctrl Pts',(11.9311214597158,0.000692114352877186,
5.79157655282255));
#48666=CARTESIAN_POINT('Ctrl Pts',(11.930169752624,0.463111161065124,5.76771600385165));
#48667=CARTESIAN_POINT('Ctrl Pts',(12.2437393113606,1.9385290048203,5.69152207909668));
#48668=CARTESIAN_POINT('Ctrl Pts',(14.5144143770745,3.58648699137295,5.56299477855761));
#48669=CARTESIAN_POINT('Ctrl Pts',(17.7235443678513,2.3834921742297,5.40599465120536));
#48670=CARTESIAN_POINT('Ctrl Pts',(18.4904461542425,-0.956822661448993,
5.2489945238531));
#48671=CARTESIAN_POINT('Ctrl Pts',(16.1274310791049,-3.43910703392132,5.09199439650085));
#48672=CARTESIAN_POINT('Ctrl Pts',(12.8507354093227,-2.85493220992714,4.93952173949066));
#48673=CARTESIAN_POINT('Ctrl Pts',(11.9280385574681,-0.918427369528735,
4.83938245826456));
#48674=CARTESIAN_POINT('Ctrl Pts',(11.9225958479619,0.00147606609843164,
4.79157655282255));
#48675=CARTESIAN_POINT('Origin',(15.,0.,14.2084234471775));
#48676=CARTESIAN_POINT('',(11.9247764014775,-0.00242061498952145,6.79157655282255));
#48677=CARTESIAN_POINT('',(11.9270135324726,0.00264512890178066,6.70842344717746));
#48678=CARTESIAN_POINT('',(11.9265,6.70613782525944E-14,14.2084234471775));
#48679=CARTESIAN_POINT('Ctrl Pts',(11.9270135324726,0.00264512890178106,
6.70842344717746));
#48680=CARTESIAN_POINT('Ctrl Pts',(11.9248054756842,0.256447062439599,6.69528301978107));
#48681=CARTESIAN_POINT('Ctrl Pts',(12.0687133238052,1.518578012587,6.62980921660061));
#48682=CARTESIAN_POINT('Ctrl Pts',(13.8044957855091,3.41606212207931,6.51200203763605));
#48683=CARTESIAN_POINT('Ctrl Pts',(17.1897706782275,2.88159878204111,6.35500191028381));
#48684=CARTESIAN_POINT('Ctrl Pts',(18.6114579568395,-0.236820710438023,
6.19800178293155));
#48685=CARTESIAN_POINT('Ctrl Pts',(16.7947147560542,-3.14288298322814,6.04100165557929));
#48686=CARTESIAN_POINT('Ctrl Pts',(13.3686365056666,-3.23068767821543,5.88400152822705));
#48687=CARTESIAN_POINT('Ctrl Pts',(11.9823834565481,-1.24709989542488,5.77314212542643));
#48688=CARTESIAN_POINT('Ctrl Pts',(11.9224186775506,-0.121114248637474,
5.7146160984099));
#48689=CARTESIAN_POINT('Ctrl Pts',(11.9232839890155,-0.00188059066360697,
5.70842344717745));
#48690=CARTESIAN_POINT('Ctrl Pts',(11.9247764014775,-0.00242061498952133,
6.79157655282255));
#48691=CARTESIAN_POINT('Ctrl Pts',(11.9319620270346,0.830283431407061,6.74838292522283));
#48692=CARTESIAN_POINT('Ctrl Pts',(12.7081731527432,2.68370300380156,6.65285592183902));
#48693=CARTESIAN_POINT('Ctrl Pts',(15.824553937525,3.52403365117268,6.50499554267113));
#48694=CARTESIAN_POINT('Ctrl Pts',(18.3941832901488,1.25627336953411,6.34799541531888));
#48695=CARTESIAN_POINT('Ctrl Pts',(17.9202159270872,-2.13799965619268,6.19099528796662));
#48696=CARTESIAN_POINT('Ctrl Pts',(14.8276629212552,-3.61510717519363,6.03399516061437));
#48697=CARTESIAN_POINT('Ctrl Pts',(12.3361598311427,-2.11869381838128,5.90085558223301));
#48698=CARTESIAN_POINT('Ctrl Pts',(11.9322571331336,-0.551113187705301,
5.82004937963574));
#48699=CARTESIAN_POINT('Ctrl Pts',(11.9311214597158,0.000692114352877186,
5.79157655282255));
#48700=CARTESIAN_POINT('Origin',(15.,0.,14.2084234471775));
#48701=CARTESIAN_POINT('',(11.9253586384648,0.00253840983232584,7.79157655282255));
#48702=CARTESIAN_POINT('',(11.9301569186554,-0.00175543039446494,7.70842344717746));
#48703=CARTESIAN_POINT('',(11.9265,6.70613782525944E-14,14.2084234471775));
#48704=CARTESIAN_POINT('Ctrl Pts',(11.9301569186554,-0.00175543039446478,
7.70842344717746));
#48705=CARTESIAN_POINT('Ctrl Pts',(11.9335080846202,0.627087276122613,7.67594994115225));
#48706=CARTESIAN_POINT('Ctrl Pts',(12.425309891706,2.27416779560488,7.59114305934296));
#48707=CARTESIAN_POINT('Ctrl Pts',(15.1005134031695,3.61781798694653,7.45400280174957));
#48708=CARTESIAN_POINT('Ctrl Pts',(18.0729932858696,1.91191582667314,7.29700267439733));
#48709=CARTESIAN_POINT('Ctrl Pts',(18.2898906220475,-1.50841957701434,7.14000254704506));
#48710=CARTESIAN_POINT('Ctrl Pts',(15.5567114486024,-3.57614071471203,6.98300241969282));
#48711=CARTESIAN_POINT('Ctrl Pts',(12.5948647250275,-2.532436114927,6.83914271973694));
#48712=CARTESIAN_POINT('Ctrl Pts',(11.9335993346794,-0.754350498545223,
6.74761639556516));
#48713=CARTESIAN_POINT('Ctrl Pts',(11.9270135324726,0.00264512890178106,
6.70842344717746));
#48714=CARTESIAN_POINT('Ctrl Pts',(11.9253586384648,0.00253840983232619,
7.79157655282255));
#48715=CARTESIAN_POINT('Ctrl Pts',(11.9236216864083,0.199145893570575,7.78138322237808));
#48716=CARTESIAN_POINT('Ctrl Pts',(12.0296403223963,1.40328729141077,7.71885651614953));
#48717=CARTESIAN_POINT('Ctrl Pts',(13.6166705510885,3.34441360725337,7.60399643413689));
#48718=CARTESIAN_POINT('Ctrl Pts',(17.0263976837988,2.99873559323853,7.44699630678466));
#48719=CARTESIAN_POINT('Ctrl Pts',(18.6190345729722,-0.0359373922966709,
7.2899961794324));
#48720=CARTESIAN_POINT('Ctrl Pts',(16.9664484412042,-3.03838498006983,7.13299605208014));
#48721=CARTESIAN_POINT('Ctrl Pts',(13.5505291268344,-3.3162835943375,6.97599592472789));
#48722=CARTESIAN_POINT('Ctrl Pts',(12.0165601959407,-1.36211545786235,6.86218942497536));
#48723=CARTESIAN_POINT('Ctrl Pts',(11.923255927005,-0.178620339789062,6.80071630100691));
#48724=CARTESIAN_POINT('Ctrl Pts',(11.9247764014775,-0.00242061498952133,
6.79157655282255));
#48725=CARTESIAN_POINT('Origin',(15.,0.,14.2084234471775));
#48726=CARTESIAN_POINT('',(11.9309505480454,-0.000995066888654084,8.79157655282255));
#48727=CARTESIAN_POINT('',(11.9216975306736,-0.000180300492997754,8.70842344717746));
#48728=CARTESIAN_POINT('',(11.9265,6.70613782525944E-14,14.2084234471775));
#48729=CARTESIAN_POINT('Ctrl Pts',(11.9216975306736,-0.000180300492997622,
8.70842344717746));
#48730=CARTESIAN_POINT('Ctrl Pts',(11.9225619574989,0.995939940607609,8.65661686252342));
#48731=CARTESIAN_POINT('Ctrl Pts',(12.9850426088341,2.99989628694768,8.5524769020853));
#48732=CARTESIAN_POINT('Ctrl Pts',(16.383329827636,3.34441452287188,8.39600356586309));
#48733=CARTESIAN_POINT('Ctrl Pts',(18.5526127662067,0.691124042072478,8.23900343851084));
#48734=CARTESIAN_POINT('Ctrl Pts',(17.5362337553543,-2.58190399634584,8.08200331115859));
#48735=CARTESIAN_POINT('Ctrl Pts',(14.2455896040548,-3.53971395275292,7.92500318380633));
#48736=CARTESIAN_POINT('Ctrl Pts',(12.1721380845128,-1.78183929043833,7.8004765624793));
#48737=CARTESIAN_POINT('Ctrl Pts',(11.928107441166,-0.386337687713779,7.72828331693634));
#48738=CARTESIAN_POINT('Ctrl Pts',(11.9301569186554,-0.00175543039446478,
7.70842344717746));
#48739=CARTESIAN_POINT('Ctrl Pts',(11.9309505480454,-0.000995066888653875,
8.79157655282255));
#48740=CARTESIAN_POINT('Ctrl Pts',(11.9326502109465,0.571148683183627,8.76205014374926));
#48741=CARTESIAN_POINT('Ctrl Pts',(12.3588112254404,2.15972684180816,8.68019035889189));
#48742=CARTESIAN_POINT('Ctrl Pts',(14.8994866243195,3.61781699652394,8.54599719825042));
#48743=CARTESIAN_POINT('Ctrl Pts',(17.9620970086125,2.07958747065415,8.38899707089818));
#48744=CARTESIAN_POINT('Ctrl Pts',(18.3685665845007,-1.32342808525659,8.23199694354591));
#48745=CARTESIAN_POINT('Ctrl Pts',(15.7544101894084,-3.53971298366467,8.07499681619367));
#48746=CARTESIAN_POINT('Ctrl Pts',(12.6774139888043,-2.64408967670503,7.92819001928588));
#48747=CARTESIAN_POINT('Ctrl Pts',(11.932539337532,-0.810252691562618,7.83371659816217));
#48748=CARTESIAN_POINT('Ctrl Pts',(11.9253586384648,0.00253840983232619,
7.79157655282255));
#48749=CARTESIAN_POINT('Origin',(15.,0.,14.2084234471775));
#48750=CARTESIAN_POINT('',(11.9222420001619,-0.00114382935434674,9.79157655282255));
#48751=CARTESIAN_POINT('',(11.9297705140734,0.00198364688382296,9.70842344717746));
#48752=CARTESIAN_POINT('',(11.9265,6.70613782525944E-14,14.2084234471775));
#48753=CARTESIAN_POINT('Ctrl Pts',(11.9297705140734,0.00198364688382347,
9.70842344717746));
#48754=CARTESIAN_POINT('Ctrl Pts',(11.9275592683916,0.36604807192143,9.68961715967868));
#48755=CARTESIAN_POINT('Ctrl Pts',(12.1545555502906,1.7405498801195,9.61847749639582));
#48756=CARTESIAN_POINT('Ctrl Pts',(14.1754458368614,3.52403461675767,9.49500445732887));
#48757=CARTESIAN_POINT('Ctrl Pts',(17.4844615229107,2.63176005547664,9.33800432997661));
#48758=CARTESIAN_POINT('Ctrl Pts',(18.565636725993,-0.620439089359897,9.18100420262437));
#48759=CARTESIAN_POINT('Ctrl Pts',(16.4494712699821,-3.31628450238807,9.0240040752721));
#48760=CARTESIAN_POINT('Ctrl Pts',(13.033551020433,-3.03838581184986,8.86700394791986));
#48761=CARTESIAN_POINT('Ctrl Pts',(11.9262816166307,-1.02667925906391,8.76181040522164));
#48762=CARTESIAN_POINT('Ctrl Pts',(11.9216887408183,-0.0103092698311159,
8.70895023830751));
#48763=CARTESIAN_POINT('Ctrl Pts',(11.9216975306736,-0.000180300492997622,
8.70842344717746));
#48764=CARTESIAN_POINT('Ctrl Pts',(11.9222420001619,-0.00114382935434687,
9.79157655282255));
#48765=CARTESIAN_POINT('Ctrl Pts',(11.9267950445754,0.938754987078744,9.74271706512043));
#48766=CARTESIAN_POINT('Ctrl Pts',(12.8851347215443,2.89342387288723,9.64152420163423));
#48767=CARTESIAN_POINT('Ctrl Pts',(16.1955038860992,3.41606118929613,9.48799796236394));
#48768=CARTESIAN_POINT('Ctrl Pts',(18.5087584392439,0.887308966009096,9.3309978350117));
#48769=CARTESIAN_POINT('Ctrl Pts',(17.6756754360527,-2.43710142000481,9.17399770765943));
#48770=CARTESIAN_POINT('Ctrl Pts',(14.4432887039958,-3.57613973602564,9.0169975803072));
#48771=CARTESIAN_POINT('Ctrl Pts',(12.2241286148511,-1.89728740549368,8.88952386202822));
#48772=CARTESIAN_POINT('Ctrl Pts',(11.9296376841916,-0.442933787892533,
8.81438351953334));
#48773=CARTESIAN_POINT('Ctrl Pts',(11.9309505480454,-0.000995066888653875,
8.79157655282255));
#48774=CARTESIAN_POINT('Origin',(15.,0.,14.2084234471775));
#48775=CARTESIAN_POINT('',(11.9284560106028,0.00245566734982605,10.7915765528225));
#48776=CARTESIAN_POINT('',(11.9275890856804,-0.00260766251225693,10.7084234471775));
#48777=CARTESIAN_POINT('',(11.9265,6.70613782525944E-14,14.2084234471775));
#48778=CARTESIAN_POINT('Ctrl Pts',(11.9275890856804,-0.00260766251225678,
10.7084234471775));
#48779=CARTESIAN_POINT('Ctrl Pts',(11.9337969642323,0.734391539461283,10.6702840810499));
#48780=CARTESIAN_POINT('Ctrl Pts',(12.5665847955819,2.49225272359552,10.5798113391382));
#48781=CARTESIAN_POINT('Ctrl Pts',(15.4855857629831,3.58648800243424,10.4370052214424));
#48782=CARTESIAN_POINT('Ctrl Pts',(18.2592872973176,1.57345505668517,10.2800050940901));
#48783=CARTESIAN_POINT('Ctrl Pts',(18.1103546151327,-1.85051527716861,10.1230049667379));
#48784=CARTESIAN_POINT('Ctrl Pts',(15.1723371249586,-3.61510816978504,9.96600483938563));
#48785=CARTESIAN_POINT('Ctrl Pts',(12.4502253736084,-2.31493586870828,9.82781099953215));
#48786=CARTESIAN_POINT('Ctrl Pts',(11.9337126333884,-0.647055676830039,
9.74195053546276));
#48787=CARTESIAN_POINT('Ctrl Pts',(11.9297705140734,0.00198364688382347,
9.70842344717746));
#48788=CARTESIAN_POINT('Ctrl Pts',(11.9284560106028,0.0024556673498264,
10.7915765528226));
#48789=CARTESIAN_POINT('Ctrl Pts',(11.9260692195737,0.309140112596412,10.7757173622757));
#48790=CARTESIAN_POINT('Ctrl Pts',(12.1080878285752,1.62508037117336,10.7075247959448));
#48791=CARTESIAN_POINT('Ctrl Pts',(13.9810651784412,3.47279856287599,10.5869988538297));
#48792=CARTESIAN_POINT('Ctrl Pts',(17.3344994031312,2.76565299665532,10.4299987264775));
#48793=CARTESIAN_POINT('Ctrl Pts',(18.5945871152999,-0.421511967551375,
10.2729985991252));
#48794=CARTESIAN_POINT('Ctrl Pts',(16.6313630370479,-3.23068676566348,10.115998471773));
#48795=CARTESIAN_POINT('Ctrl Pts',(13.205285741413,-3.14288213812672,9.9589983444207));
#48796=CARTESIAN_POINT('Ctrl Pts',(11.9539254885605,-1.14120637601563,9.85085770477057));
#48797=CARTESIAN_POINT('Ctrl Pts',(11.921918280707,-0.0679702217342443,
9.79505044090452));
#48798=CARTESIAN_POINT('Ctrl Pts',(11.9222420001619,-0.00114382935434687,
9.79157655282255));
#48799=CARTESIAN_POINT('Origin',(15.,0.,14.2084234471775));
#48800=CARTESIAN_POINT('',(11.9297760945785,-0.00333806817183438,11.7915765528226));
#48801=CARTESIAN_POINT('',(11.9228311771842,0.00152130202986591,11.7084234471775));
#48802=CARTESIAN_POINT('',(11.9265,6.70613782525944E-14,14.2084234471775));
#48803=CARTESIAN_POINT('',(14.2062007174671,-2.96922295374568,12.));
#48804=CARTESIAN_POINT('Ctrl Pts',(14.2062007174671,-2.96922295374568,12.));
#48805=CARTESIAN_POINT('Ctrl Pts',(13.2298599415769,-2.70820563726846,11.9476666242159));
#48806=CARTESIAN_POINT('Ctrl Pts',(12.1284916041782,-1.6759644246982,11.8781921418234));
#48807=CARTESIAN_POINT('Ctrl Pts',(11.9274999800733,-0.33505537898738,11.8087176594309));
#48808=CARTESIAN_POINT('Ctrl Pts',(11.9297760945785,-0.00333806817183434,
11.7915765528225));
#48809=CARTESIAN_POINT('',(15.7957331921886,-2.97400465723624,12.));
#48810=CARTESIAN_POINT('Origin',(15.,0.,12.));
#48811=CARTESIAN_POINT('Ctrl Pts',(15.7957405241459,-2.97402278592475,12.));
#48812=CARTESIAN_POINT('Ctrl Pts',(14.8659292530302,-3.21955068215558,11.9500021225376));
#48813=CARTESIAN_POINT('Ctrl Pts',(12.809912552641,-2.78622279751186,11.8528099382634));
#48814=CARTESIAN_POINT('Ctrl Pts',(11.9286986705132,-0.906613920335824,
11.7556177539892));
#48815=CARTESIAN_POINT('Ctrl Pts',(11.9228311771842,0.00152130202986659,
11.7084234471775));
#48816=CARTESIAN_POINT('Origin',(15.,1.36827403442078E-16,4.));
#48817=CARTESIAN_POINT('Ctrl Pts',(13.086534003335,1.63598720337497,4.));
#48818=CARTESIAN_POINT('Ctrl Pts',(13.0243671614557,1.57756563722365,4.));
#48819=CARTESIAN_POINT('Ctrl Pts',(12.9655713261624,1.51589246301216,4.));
#48820=CARTESIAN_POINT('Ctrl Pts',(12.9101605215997,1.45134356594541,4.));
#48821=CARTESIAN_POINT('Ctrl Pts',(12.8533994594265,1.38522173305508,4.));
#48822=CARTESIAN_POINT('Ctrl Pts',(12.8001899401135,1.31608182626898,4.));
#48823=CARTESIAN_POINT('Ctrl Pts',(12.7505758639603,1.24428161564212,4.));
#48824=CARTESIAN_POINT('Ctrl Pts',(12.737567030614,1.22545556774005,4.));
#48825=CARTESIAN_POINT('Ctrl Pts',(12.7248055528518,1.20644640781821,4.));
#48826=CARTESIAN_POINT('Ctrl Pts',(12.7122926030956,1.18726014528907,4.));
#48827=CARTESIAN_POINT('Ctrl Pts',(12.7022174307361,1.17181175736453,4.));
#48828=CARTESIAN_POINT('Ctrl Pts',(12.6923030248513,1.15624777849328,4.));
#48829=CARTESIAN_POINT('Ctrl Pts',(12.6825586157748,1.14058556199816,4.));
#48830=CARTESIAN_POINT('Ctrl Pts',(12.6350797654636,1.06427267050556,4.));
#48831=CARTESIAN_POINT('Ctrl Pts',(12.5915831545383,0.985554475328281,4.00000000000001));
#48832=CARTESIAN_POINT('Ctrl Pts',(12.5521056896097,0.904822546167765,4.00000000000001));
#48833=CARTESIAN_POINT('Ctrl Pts',(12.5205631790518,0.840317701884819,4.));
#48834=CARTESIAN_POINT('Ctrl Pts',(12.4915870127793,0.774526199173173,4.));
#48835=CARTESIAN_POINT('Ctrl Pts',(12.4652125787776,0.707630559635218,4.));
#48836=CARTESIAN_POINT('Ctrl Pts',(12.4565302425272,0.685608838292681,4.));
#48837=CARTESIAN_POINT('Ctrl Pts',(12.4481299823828,0.663467358107674,4.));
#48838=CARTESIAN_POINT('Ctrl Pts',(12.4400134491405,0.641212348322469,4.));
#48839=CARTESIAN_POINT('Ctrl Pts',(12.4326491678695,0.6210199648435,4.));
#48840=CARTESIAN_POINT('Ctrl Pts',(12.4255170259942,0.600729502784082,4.));
#48841=CARTESIAN_POINT('Ctrl Pts',(12.41862769741,0.580374130450127,4.));
#48842=CARTESIAN_POINT('Ctrl Pts',(12.3890480800735,0.492977497088245,4.));
#48843=CARTESIAN_POINT('Ctrl Pts',(12.363907391977,0.404299179172776,4.00000000000001));
#48844=CARTESIAN_POINT('Ctrl Pts',(12.3432403919349,0.314735964380019,4.00000000000001));
#48845=CARTESIAN_POINT('Ctrl Pts',(12.322257026321,0.223801736977766,4.00000000000001));
#48846=CARTESIAN_POINT('Ctrl Pts',(12.3058848583804,0.131954509394712,4.));
#48847=CARTESIAN_POINT('Ctrl Pts',(12.2942020415478,0.039576420273935,4.));
#48848=CARTESIAN_POINT('Ctrl Pts',(12.2826102453471,-0.0520819526881022,
4.));
#48849=CARTESIAN_POINT('Ctrl Pts',(12.2756346673422,-0.14426387445687,4.));
#48850=CARTESIAN_POINT('Ctrl Pts',(12.2733985971608,-0.236615283315844,
4.));
#48851=CARTESIAN_POINT('Ctrl Pts',(12.2723186623648,-0.28121741642928,4.));
#48852=CARTESIAN_POINT('Ctrl Pts',(12.2723449592516,-0.325859284098739,
4.));
#48853=CARTESIAN_POINT('Ctrl Pts',(12.2734957210626,-0.370501641907857,
4.));
#48854=CARTESIAN_POINT('Ctrl Pts',(12.2738658684163,-0.384861043177254,
4.));
#48855=CARTESIAN_POINT('Ctrl Pts',(12.2743523774935,-0.399220495972395,
4.));
#48856=CARTESIAN_POINT('Ctrl Pts',(12.2749559214615,-0.413578694513598,
4.));
#48857=CARTESIAN_POINT('Ctrl Pts',(12.2755868612803,-0.428588635239398,
4.));
#48858=CARTESIAN_POINT('Ctrl Pts',(12.2763453773817,-0.443588732674977,
4.));
#48859=CARTESIAN_POINT('Ctrl Pts',(12.2772314223084,-0.458571999977678,
4.));
#48860=CARTESIAN_POINT('Ctrl Pts',(12.2828802428556,-0.554095133908471,
4.));
#48861=CARTESIAN_POINT('Ctrl Pts',(12.2937114584574,-0.649002595692518,
4.));
#48862=CARTESIAN_POINT('Ctrl Pts',(12.3097976800713,-0.742900147453328,
4.));
#48863=CARTESIAN_POINT('Ctrl Pts',(12.3112861449746,-0.75158852771142,4.));
#48864=CARTESIAN_POINT('Ctrl Pts',(12.3128196370525,-0.760268274419424,
4.));
#48865=CARTESIAN_POINT('Ctrl Pts',(12.3143982352413,-0.768939082485976,
4.));
#48866=CARTESIAN_POINT('Ctrl Pts',(12.3307867311623,-0.858956607935255,
4.));
#48867=CARTESIAN_POINT('Ctrl Pts',(12.3520323002905,-0.948010485772638,
4.));
#48868=CARTESIAN_POINT('Ctrl Pts',(12.3778326203319,-1.03586583972401,4.));
#48869=CARTESIAN_POINT('Ctrl Pts',(12.4042241967268,-1.12573454219727,4.));
#48870=CARTESIAN_POINT('Ctrl Pts',(12.435381875245,-1.21434985801567,4.));
#48871=CARTESIAN_POINT('Ctrl Pts',(12.4710363747919,-1.30145748669412,4.));
#48872=CARTESIAN_POINT('Ctrl Pts',(12.4909273060557,-1.35005308827618,4.));
#48873=CARTESIAN_POINT('Ctrl Pts',(12.5122187298043,-1.39817934130794,4.));
#48874=CARTESIAN_POINT('Ctrl Pts',(12.534870586159,-1.44579043537726,4.));
#48875=CARTESIAN_POINT('Ctrl Pts',(12.5412077066689,-1.45911019319316,4.));
#48876=CARTESIAN_POINT('Ctrl Pts',(12.5476516035311,-1.47239000998161,4.));
#48877=CARTESIAN_POINT('Ctrl Pts',(12.5541943737652,-1.48561501829369,4.));
#48878=CARTESIAN_POINT('Ctrl Pts',(12.5969523561364,-1.57204242626194,4.));
#48879=CARTESIAN_POINT('Ctrl Pts',(12.6439961654632,-1.65627338500264,4.));
#48880=CARTESIAN_POINT('Ctrl Pts',(12.6949857265575,-1.73805452373085,4.));
#48881=CARTESIAN_POINT('Ctrl Pts',(12.7469808269627,-1.82144842687817,4.));
#48882=CARTESIAN_POINT('Ctrl Pts',(12.8030791489228,-1.90229571208266,4.));
#48883=CARTESIAN_POINT('Ctrl Pts',(12.8629750013787,-1.98032077373009,4.));
#48884=CARTESIAN_POINT('Ctrl Pts',(12.9233424571313,-2.05896018302908,4.));
#48885=CARTESIAN_POINT('Ctrl Pts',(12.9875679362272,-2.13473359370643,4.));
#48886=CARTESIAN_POINT('Ctrl Pts',(13.0553877098439,-2.20733955177719,4.));
#48887=CARTESIAN_POINT('Ctrl Pts',(13.0913230991629,-2.24581097730712,4.));
#48888=CARTESIAN_POINT('Ctrl Pts',(13.1282683996108,-2.28339271539353,4.));
#48889=CARTESIAN_POINT('Ctrl Pts',(13.1661892287502,-2.32003649064048,4.));
#48890=CARTESIAN_POINT('Ctrl Pts',(13.1814900570711,-2.33482203533466,4.));
#48891=CARTESIAN_POINT('Ctrl Pts',(13.196949744001,-2.34945484110134,4.));
#48892=CARTESIAN_POINT('Ctrl Pts',(13.2125661689314,-2.36393160001069,4.));
#48893=CARTESIAN_POINT('Ctrl Pts',(13.2232570858249,-2.37384230794012,4.));
#48894=CARTESIAN_POINT('Ctrl Pts',(13.2340146157559,-2.3836735202466,4.));
#48895=CARTESIAN_POINT('Ctrl Pts',(13.2448364129784,-2.39342320679516,4.));
#48896=CARTESIAN_POINT('Ctrl Pts',(13.320625051765,-2.46170349859172,4.));
#48897=CARTESIAN_POINT('Ctrl Pts',(13.3995829817648,-2.52600647852482,4.));
#48898=CARTESIAN_POINT('Ctrl Pts',(13.4813873531473,-2.58604589859231,4.));
#48899=CARTESIAN_POINT('Ctrl Pts',(13.5632614554873,-2.64613649693043,4.));
#48900=CARTESIAN_POINT('Ctrl Pts',(13.6479874247046,-2.70195710712452,4.));
#48901=CARTESIAN_POINT('Ctrl Pts',(13.7352864859208,-2.75319451696124,4.));
#48902=CARTESIAN_POINT('Ctrl Pts',(13.8208945029142,-2.80343942212848,4.));
#48903=CARTESIAN_POINT('Ctrl Pts',(13.9089775477651,-2.84927765377448,4.));
#48904=CARTESIAN_POINT('Ctrl Pts',(13.9993066119595,-2.89037749094858,4.));
#48905=CARTESIAN_POINT('Ctrl Pts',(14.025515470362,-2.90230255429857,4.));
#48906=CARTESIAN_POINT('Ctrl Pts',(14.0519135997525,-2.91382843622988,4.));
#48907=CARTESIAN_POINT('Ctrl Pts',(14.0784958352494,-2.92494631785187,4.));
#48908=CARTESIAN_POINT('Ctrl Pts',(14.1199798960696,-2.94229681034347,4.));
#48909=CARTESIAN_POINT('Ctrl Pts',(14.1619123028466,-2.95865373590191,4.));
#48910=CARTESIAN_POINT('Ctrl Pts',(14.204261268307,-2.97402368063354,4.));
#48911=CARTESIAN_POINT('Ctrl Pts',(15.7937992825329,-2.9692229537457,4.));
#48912=CARTESIAN_POINT('Ctrl Pts',(15.8886556608518,-2.93452406683594,4.));
#48913=CARTESIAN_POINT('Ctrl Pts',(15.9814715788842,-2.89484190048077,4.));
#48914=CARTESIAN_POINT('Ctrl Pts',(16.0720047548823,-2.85049467748599,4.));
#48915=CARTESIAN_POINT('Ctrl Pts',(16.1637866430073,-2.80553577910774,4.));
#48916=CARTESIAN_POINT('Ctrl Pts',(16.2532230529932,-2.75578154813471,4.));
#48917=CARTESIAN_POINT('Ctrl Pts',(16.3400275203182,-2.70152291880737,4.));
#48918=CARTESIAN_POINT('Ctrl Pts',(16.3646888442304,-2.686107932988,4.));
#48919=CARTESIAN_POINT('Ctrl Pts',(16.389137491053,-2.67032916740001,4.));
#48920=CARTESIAN_POINT('Ctrl Pts',(16.4133662837328,-2.65419282892726,4.));
#48921=CARTESIAN_POINT('Ctrl Pts',(16.4325631402962,-2.64140775212984,4.));
#48922=CARTESIAN_POINT('Ctrl Pts',(16.4516239542716,-2.62839666993241,4.));
#48923=CARTESIAN_POINT('Ctrl Pts',(16.4705261961219,-2.61517619923621,4.));
#48924=CARTESIAN_POINT('Ctrl Pts',(16.5532306656362,-2.55733163115156,4.));
#48925=CARTESIAN_POINT('Ctrl Pts',(16.6329816584356,-2.49543011909309,4.));
#48926=CARTESIAN_POINT('Ctrl Pts',(16.7095117106738,-2.42976651841151,4.));
#48927=CARTESIAN_POINT('Ctrl Pts',(16.7679773228431,-2.37960239988795,4.));
#48928=CARTESIAN_POINT('Ctrl Pts',(16.8245624524955,-2.32724171199687,4.));
#48929=CARTESIAN_POINT('Ctrl Pts',(16.8791308185435,-2.27280449707864,4.));
#48930=CARTESIAN_POINT('Ctrl Pts',(16.9076285190194,-2.2443752887693,4.));
#48931=CARTESIAN_POINT('Ctrl Pts',(16.9355759205114,-2.21537960309138,4.));
#48932=CARTESIAN_POINT('Ctrl Pts',(16.9629517841853,-2.18583377975445,4.));
#48933=CARTESIAN_POINT('Ctrl Pts',(16.9740993314633,-2.17380261732463,4.));
#48934=CARTESIAN_POINT('Ctrl Pts',(16.9851523150081,-2.16167987026619,4.));
#48935=CARTESIAN_POINT('Ctrl Pts',(16.9960991984116,-2.14947815004889,4.));
#48936=CARTESIAN_POINT('Ctrl Pts',(17.061864093391,-2.07617465177648,4.));
#48937=CARTESIAN_POINT('Ctrl Pts',(17.1238952962526,-1.9999250033291,4.));
#48938=CARTESIAN_POINT('Ctrl Pts',(17.1819478816723,-1.92100525783345,4.));
#48939=CARTESIAN_POINT('Ctrl Pts',(17.2389325987962,-1.84353722880334,4.));
#48940=CARTESIAN_POINT('Ctrl Pts',(17.2920840747574,-1.76349564200828,4.));
#48941=CARTESIAN_POINT('Ctrl Pts',(17.3411263889919,-1.681119910375,4.));
#48942=CARTESIAN_POINT('Ctrl Pts',(17.3892346863819,-1.6003130345782,4.));
#48943=CARTESIAN_POINT('Ctrl Pts',(17.4333891346359,-1.51725940586905,4.));
#48944=CARTESIAN_POINT('Ctrl Pts',(17.473281665729,-1.43217460910322,4.));
#48945=CARTESIAN_POINT('Ctrl Pts',(17.4935758753293,-1.38889009814213,4.));
#48946=CARTESIAN_POINT('Ctrl Pts',(17.5127663147042,-1.34507981852401,4.));
#48947=CARTESIAN_POINT('Ctrl Pts',(17.5308071984732,-1.30077191375233,4.));
#48948=CARTESIAN_POINT('Ctrl Pts',(17.5396600651807,-1.27902952130341,4.));
#48949=CARTESIAN_POINT('Ctrl Pts',(17.548236065603,-1.25716730274661,4.));
#48950=CARTESIAN_POINT('Ctrl Pts',(17.5565294575664,-1.23518860043795,4.));
#48951=CARTESIAN_POINT('Ctrl Pts',(17.5612619499656,-1.22264680305532,4.));
#48952=CARTESIAN_POINT('Ctrl Pts',(17.5659011120686,-1.21007041067208,4.));
#48953=CARTESIAN_POINT('Ctrl Pts',(17.5704433141742,-1.19746790314509,4.));
#48954=CARTESIAN_POINT('Ctrl Pts',(17.601949668132,-1.11005236027246,4.));
#48955=CARTESIAN_POINT('Ctrl Pts',(17.6288373085193,-1.02126995392761,4.));
#48956=CARTESIAN_POINT('Ctrl Pts',(17.6508530784154,-0.931342019285625,
4.));
#48957=CARTESIAN_POINT('Ctrl Pts',(17.6541059208438,-0.918055116184408,
4.));
#48958=CARTESIAN_POINT('Ctrl Pts',(17.6572523179739,-0.90474318860678,4.));
#48959=CARTESIAN_POINT('Ctrl Pts',(17.6602913566075,-0.891406935242469,
4.));
#48960=CARTESIAN_POINT('Ctrl Pts',(17.6812030503878,-0.79963987330047,4.));
#48961=CARTESIAN_POINT('Ctrl Pts',(17.6970357825963,-0.706720788882977,
4.));
#48962=CARTESIAN_POINT('Ctrl Pts',(17.7078979433461,-0.613041608366267,
4.));
#48963=CARTESIAN_POINT('Ctrl Pts',(17.71918010274,-0.515740208504458,4.));
#48964=CARTESIAN_POINT('Ctrl Pts',(17.7250998267343,-0.417617597139405,
4.));
#48965=CARTESIAN_POINT('Ctrl Pts',(17.7257219253175,-0.319126306900475,
4.));
#48966=CARTESIAN_POINT('Ctrl Pts',(17.7259028938113,-0.290475188042702,
4.));
#48967=CARTESIAN_POINT('Ctrl Pts',(17.7256352115795,-0.261793020088843,
4.));
#48968=CARTESIAN_POINT('Ctrl Pts',(17.7249196338,-0.233091376404626,4.));
#48969=CARTESIAN_POINT('Ctrl Pts',(17.7245239501318,-0.217220604586536,
4.));
#48970=CARTESIAN_POINT('Ctrl Pts',(17.7239913108662,-0.201343881980789,
4.));
#48971=CARTESIAN_POINT('Ctrl Pts',(17.7233217966467,-0.185463198608965,
4.));
#48972=CARTESIAN_POINT('Ctrl Pts',(17.7227411089474,-0.171689454568016,
4.));
#48973=CARTESIAN_POINT('Ctrl Pts',(17.7220574547657,-0.157914135821034,
4.));
#48974=CARTESIAN_POINT('Ctrl Pts',(17.7212718008001,-0.144150654953,4.));
#48975=CARTESIAN_POINT('Ctrl Pts',(17.7159690064325,-0.0512536391956395,
4.));
#48976=CARTESIAN_POINT('Ctrl Pts',(17.7060179260155,0.0412556969053557,
4.));
#48977=CARTESIAN_POINT('Ctrl Pts',(17.691537290537,0.133004324856137,4.));
#48978=CARTESIAN_POINT('Ctrl Pts',(17.6770974224585,0.224494652470098,4.));
#48979=CARTESIAN_POINT('Ctrl Pts',(17.6581530629752,0.315229493843254,4.));
#48980=CARTESIAN_POINT('Ctrl Pts',(17.6347733990709,0.404821867293602,4.));
#48981=CARTESIAN_POINT('Ctrl Pts',(17.6117974920603,0.492867018399034,4.));
#48982=CARTESIAN_POINT('Ctrl Pts',(17.5845376887683,0.579809603493695,4.));
#48983=CARTESIAN_POINT('Ctrl Pts',(17.5530192634714,0.665253146715262,4.));
#48984=CARTESIAN_POINT('Ctrl Pts',(17.5376266260196,0.706981166786664,4.));
#48985=CARTESIAN_POINT('Ctrl Pts',(17.521217712657,0.748351139728866,4.));
#48986=CARTESIAN_POINT('Ctrl Pts',(17.5037923624592,0.789313445373718,4.));
#48987=CARTESIAN_POINT('Ctrl Pts',(17.4980299458858,0.802859334911291,4.));
#48988=CARTESIAN_POINT('Ctrl Pts',(17.4921563593103,0.816360622497498,4.));
#48989=CARTESIAN_POINT('Ctrl Pts',(17.4861715515314,0.829815450098292,4.));
#48990=CARTESIAN_POINT('Ctrl Pts',(17.4804842577731,0.842601417477522,4.));
#48991=CARTESIAN_POINT('Ctrl Pts',(17.4746999465266,0.855337690933622,4.));
#48992=CARTESIAN_POINT('Ctrl Pts',(17.4688205030047,0.868019526422757,4.));
#48993=CARTESIAN_POINT('Ctrl Pts',(17.4313685751689,0.948802543693164,4.));
#48994=CARTESIAN_POINT('Ctrl Pts',(17.3900398049897,1.02742425086957,4.));
#48995=CARTESIAN_POINT('Ctrl Pts',(17.3448999527151,1.10353609749938,4.));
#48996=CARTESIAN_POINT('Ctrl Pts',(17.3005164856713,1.17837257715787,4.));
#48997=CARTESIAN_POINT('Ctrl Pts',(17.2524481398624,1.25078327494736,4.));
#48998=CARTESIAN_POINT('Ctrl Pts',(17.2007210868077,1.32040265351989,4.));
#48999=CARTESIAN_POINT('Ctrl Pts',(17.1505256542607,1.38796062589101,4.));
#49000=CARTESIAN_POINT('Ctrl Pts',(17.0968845380256,1.45289058144554,4.));
#49001=CARTESIAN_POINT('Ctrl Pts',(17.0397936511852,1.5148180351349,4.));
#49002=CARTESIAN_POINT('Ctrl Pts',(17.0255930287153,1.53022169128796,4.));
#49003=CARTESIAN_POINT('Ctrl Pts',(17.0111788466503,1.54543936332989,4.));
#49004=CARTESIAN_POINT('Ctrl Pts',(16.9965508084827,1.56046483491105,4.));
#49005=CARTESIAN_POINT('Ctrl Pts',(16.9706944922369,1.58702364891564,4.));
#49006=CARTESIAN_POINT('Ctrl Pts',(16.9441700096348,1.61298203696882,4.));
#49007=CARTESIAN_POINT('Ctrl Pts',(16.9170033607454,1.6383265094434,4.));
#49008=CARTESIAN_POINT('Origin',(15.,0.,14.2084234471775));
#49009=CARTESIAN_POINT('Ctrl Pts',(11.9228311771842,0.0015213020298664,
11.7084234471775));
#49010=CARTESIAN_POINT('Ctrl Pts',(11.9221922557771,0.100409703179003,11.7032843782051));
#49011=CARTESIAN_POINT('Ctrl Pts',(11.9710108327432,1.20571704782255,11.6458119334487));
#49012=CARTESIAN_POINT('Ctrl Pts',(13.3048024582519,3.19795728077006,11.5360061129082));
#49013=CARTESIAN_POINT('Ctrl Pts',(16.7319486542021,3.17774782202826,11.3790059855559));
#49014=CARTESIAN_POINT('Ctrl Pts',(18.606042966971,0.308570934784431,11.2220058582037));
#49015=CARTESIAN_POINT('Ctrl Pts',(17.246562375271,-2.83758641060089,11.0650057308514));
#49016=CARTESIAN_POINT('Ctrl Pts',(13.8725685599584,-3.4391081414099,10.9080056034992));
#49017=CARTESIAN_POINT('Ctrl Pts',(12.0835901505745,-1.55983373126709,10.7891448422745));
#49018=CARTESIAN_POINT('Ctrl Pts',(11.9252787513183,-0.276890505982443,
10.7226174568339));
#49019=CARTESIAN_POINT('Ctrl Pts',(11.9275890856804,-0.00260766251225678,
10.7084234471775));
#49020=CARTESIAN_POINT('Ctrl Pts',(11.9297760945785,-0.00333806817183434,
11.7915765528225));
#49021=CARTESIAN_POINT('Ctrl Pts',(11.9344491671038,0.677708095250012,11.7563842836469));
#49022=CARTESIAN_POINT('Ctrl Pts',(12.4898049314569,2.38075616290146,11.6688586386871));
#49023=CARTESIAN_POINT('Ctrl Pts',(15.2863460006058,3.60696666543133,11.5289996179432));
#49024=CARTESIAN_POINT('Ctrl Pts',(18.1665668486981,1.75247841941832,11.371999490591));
#49025=CARTESIAN_POINT('Ctrl Pts',(18.2084706556688,-1.6752137223659,11.2149993632387));
#49026=CARTESIAN_POINT('Ctrl Pts',(15.3727057323674,-3.59983386165072,11.0579992358865));
#49027=CARTESIAN_POINT('Ctrl Pts',(12.5232213208654,-2.42851998200457,10.9168582990811));
#49028=CARTESIAN_POINT('Ctrl Pts',(11.9339453360424,-0.702880789277512,
10.8280507380598));
#49029=CARTESIAN_POINT('Ctrl Pts',(11.9284560106028,0.0024556673498264,
10.7915765528226));
#49030=CARTESIAN_POINT('Ctrl Pts',(16.9134659966651,1.63598720337493,12.));
#49031=CARTESIAN_POINT('Ctrl Pts',(17.4514117960785,1.00680074451815,11.9476666242159));
#49032=CARTESIAN_POINT('Ctrl Pts',(17.8499101160228,-0.812800245940048,
11.8429998726477));
#49033=CARTESIAN_POINT('Ctrl Pts',(15.8909226224913,-2.8292934693942,11.6859997452955));
#49034=CARTESIAN_POINT('Ctrl Pts',(13.1331777991764,-2.30192506894816,11.5289996179432));
#49035=CARTESIAN_POINT('Ctrl Pts',(12.0494015740803,0.286239346000545,11.371999490591));
#49036=CARTESIAN_POINT('Ctrl Pts',(13.6114658170324,2.61944280277814,11.2149993632387));
#49037=CARTESIAN_POINT('Ctrl Pts',(16.4186369731426,2.60288926043798,11.0579992358865));
#49038=CARTESIAN_POINT('Ctrl Pts',(17.9537052771594,0.252750066152531,10.9009991085342));
#49039=CARTESIAN_POINT('Ctrl Pts',(16.8401564274426,-2.32426347443882,10.743998981182));
#49040=CARTESIAN_POINT('Ctrl Pts',(14.0765223197317,-2.81696917065216,10.5869988538297));
#49041=CARTESIAN_POINT('Ctrl Pts',(12.1409791666289,-0.783732381279285,
10.4299987264775));
#49042=CARTESIAN_POINT('Ctrl Pts',(12.7691475978345,1.95231594579313,10.2729985991252));
#49043=CARTESIAN_POINT('Ctrl Pts',(15.3977426901935,2.93768783020276,10.1159984717729));
#49044=CARTESIAN_POINT('Ctrl Pts',(17.6696781425075,1.28881506595247,9.95899834442072));
#49045=CARTESIAN_POINT('Ctrl Pts',(17.5476875690895,-1.51575474549275,9.80199821706844));
#49046=CARTESIAN_POINT('Ctrl Pts',(15.1411611231766,-2.96113057342894,9.6449980897162));
#49047=CARTESIAN_POINT('Ctrl Pts',(12.6080541376564,-1.75123331751949,9.48799796236395));
#49048=CARTESIAN_POINT('Ctrl Pts',(12.2198279573789,1.02901222386683,9.33099783501168));
#49049=CARTESIAN_POINT('Ctrl Pts',(14.3246087178457,2.88653234022692,9.17399770765945));
#49050=CARTESIAN_POINT('Ctrl Pts',(17.0350193212714,2.15567136478361,9.01699758030717));
#49051=CARTESIAN_POINT('Ctrl Pts',(17.920608575789,-0.508200880905659,8.85999745295495));
#49052=CARTESIAN_POINT('Ctrl Pts',(16.1872601015714,-2.71636448178362,8.70299732560267));
#49053=CARTESIAN_POINT('Ctrl Pts',(13.3892841040964,-2.48873801247178,8.54599719825043));
#49054=CARTESIAN_POINT('Ctrl Pts',(12.0356525030592,-0.0294362811014349,
8.38899707089817));
#49055=CARTESIAN_POINT('Ctrl Pts',(13.3401797411332,2.45626124056312,8.23199694354592));
#49056=CARTESIAN_POINT('Ctrl Pts',(16.1330837289975,2.73940574632503,8.07499681619367));
#49057=CARTESIAN_POINT('Ctrl Pts',(17.9099406666424,0.566098837129481,7.91799668884141));
#49058=CARTESIAN_POINT('Ctrl Pts',(17.0774258920138,-2.11483432920145,7.76099656148916));
#49059=CARTESIAN_POINT('Ctrl Pts',(14.3820633896886,-2.89937526470001,7.6039964341369));
#49060=CARTESIAN_POINT('Ctrl Pts',(12.240810574834,-1.08401858364571,7.44699630678465));
#49061=CARTESIAN_POINT('Ctrl Pts',(12.5737493864543,1.70338795860876,7.28999617943239));
#49062=CARTESIAN_POINT('Ctrl Pts',(15.0823304026287,2.96335018127148,7.13299605208015));
#49063=CARTESIAN_POINT('Ctrl Pts',(17.5170849510905,1.56604785867891,6.97599592472789));
#49064=CARTESIAN_POINT('Ctrl Pts',(17.6947452874587,-1.23554458602037,6.81899579737564));
#49065=CARTESIAN_POINT('Ctrl Pts',(15.4560016501892,-2.92921237979097,6.66199567002338));
#49066=CARTESIAN_POINT('Ctrl Pts',(12.8083570016989,-1.99622726741817,6.50499554267113));
#49067=CARTESIAN_POINT('Ctrl Pts',(12.1259795712872,0.726793862646375,6.34799541531888));
#49068=CARTESIAN_POINT('Ctrl Pts',(14.0207639954511,2.79809220508692,6.19099528796662));
#49069=CARTESIAN_POINT('Ctrl Pts',(16.793638419534,2.3603139527537,6.03399516061437));
#49070=CARTESIAN_POINT('Ctrl Pts',(17.9581406885776,-0.193979547267846,
5.87699503326211));
#49071=CARTESIAN_POINT('Ctrl Pts',(16.4700486085461,-2.57433151465002,5.71999490590987));
#49072=CARTESIAN_POINT('Ctrl Pts',(13.6637522053085,-2.64625223032612,5.56299477855761));
#49073=CARTESIAN_POINT('Ctrl Pts',(12.0556774054966,-0.345259977325435,
5.40599465120536));
#49074=CARTESIAN_POINT('Ctrl Pts',(13.0878139143641,2.26534344968177,5.2489945238531));
#49075=CARTESIAN_POINT('Ctrl Pts',(15.8346085061802,2.84456586771516,5.09199439650085));
#49076=CARTESIAN_POINT('Ctrl Pts',(17.8330357993722,0.87308907652308,4.9349942691486));
#49077=CARTESIAN_POINT('Ctrl Pts',(17.2909861426673,-1.8813930887419,4.77799414179634));
#49078=CARTESIAN_POINT('Ctrl Pts',(14.6947169782024,-2.94862097263666,4.62099401444409));
#49079=CARTESIAN_POINT('Ctrl Pts',(12.3719451483433,-1.37216452037615,4.46399388709184));
#49080=CARTESIAN_POINT('Ctrl Pts',(12.4062682448688,1.4354510150691,4.30699375973958));
#49081=CARTESIAN_POINT('Ctrl Pts',(14.7654540928384,2.95446651190592,4.14999363238733));
#49082=CARTESIAN_POINT('Ctrl Pts',(17.3368403233694,1.82697070537499,3.99299350503508));
#49083=CARTESIAN_POINT('Ctrl Pts',(17.8090202723047,-0.94447711406392,3.83599337768282));
#49084=CARTESIAN_POINT('Ctrl Pts',(16.4499195044998,-2.21828784507026,3.73132662611465));
#49085=CARTESIAN_POINT('Ctrl Pts',(15.6501999979751,-2.43208680203507,3.67899325033057));
#49086=CARTESIAN_POINT('Ctrl Pts',(17.0543315503421,1.75642532122682,12.1070022498898));
#49087=CARTESIAN_POINT('Ctrl Pts',(17.6318798475343,1.08091940905997,12.0546688741057));
#49088=CARTESIAN_POINT('Ctrl Pts',(18.0597148196982,-0.872636980364766,
11.9500021225376));
#49089=CARTESIAN_POINT('Ctrl Pts',(15.9565105706019,-3.03758041662798,11.7930019951853));
#49090=CARTESIAN_POINT('Ctrl Pts',(12.9957460688013,-2.47138820543743,11.6360018678331));
#49091=CARTESIAN_POINT('Ctrl Pts',(11.8321843976736,0.307311716258913,11.4790017404808));
#49092=CARTESIAN_POINT('Ctrl Pts',(13.5092446974389,2.81228096210878,11.3220016131285));
#49093=CARTESIAN_POINT('Ctrl Pts',(16.5230742001624,2.79450878096808,11.1650014857763));
#49094=CARTESIAN_POINT('Ctrl Pts',(18.1711511737633,0.271357022363162,11.008001358424));
#49095=CARTESIAN_POINT('Ctrl Pts',(16.9756250767187,-2.49537111982618,10.8510012310718));
#49096=CARTESIAN_POINT('Ctrl Pts',(14.0085377331406,-3.02434882757141,10.6940011037195));
#49097=CARTESIAN_POINT('Ctrl Pts',(11.9305037500974,-0.841429197431721,
10.5370009763673));
#49098=CARTESIAN_POINT('Ctrl Pts',(12.604916689446,2.09604155530799,10.380000849015));
#49099=CARTESIAN_POINT('Ctrl Pts',(15.4270237144567,3.15395455427992,10.2230007216628));
#49100=CARTESIAN_POINT('Ctrl Pts',(17.8662145274442,1.38369506286337,10.0660005943105));
#49101=CARTESIAN_POINT('Ctrl Pts',(17.7352432511039,-1.62734158938471,9.90900046695827));
#49102=CARTESIAN_POINT('Ctrl Pts',(15.1515531237706,-3.17912310554764,9.752000339606));
#49103=CARTESIAN_POINT('Ctrl Pts',(12.4319638497434,-1.88015562464175,9.59500021225376));
#49104=CARTESIAN_POINT('Ctrl Pts',(12.0151572316991,1.10476605325709,9.4380000849015));
#49105=CARTESIAN_POINT('Ctrl Pts',(14.2748877575176,3.09903309907051,9.28099995754925));
#49106=CARTESIAN_POINT('Ctrl Pts',(17.1848333884845,2.31436759501462,9.123999830197));
#49107=CARTESIAN_POINT('Ctrl Pts',(18.1356179591903,-0.54561361705707,8.96699970284474));
#49108=CARTESIAN_POINT('Ctrl Pts',(16.274663824375,-2.9163378219851,8.80999957549249));
#49109=CARTESIAN_POINT('Ctrl Pts',(13.2707064095419,-2.67195394559781,8.65299944814023));
#49110=CARTESIAN_POINT('Ctrl Pts',(11.817423147442,-0.0316033214579261,
8.49599932078798));
#49111=CARTESIAN_POINT('Ctrl Pts',(13.2179870812285,2.63708629845826,8.33899919343572));
#49112=CARTESIAN_POINT('Ctrl Pts',(16.2164990952103,2.94107533850731,8.18199906608348));
#49113=CARTESIAN_POINT('Ctrl Pts',(18.1241646998305,0.607773905443812,8.02499893873121));
#49114=CARTESIAN_POINT('Ctrl Pts',(17.2303618464606,-2.27052421824958,7.86799881137898));
#49115=CARTESIAN_POINT('Ctrl Pts',(14.3365721278107,-3.11282149405098,7.71099868402671));
#49116=CARTESIAN_POINT('Ctrl Pts',(12.0376845476387,-1.16382187163074,7.55399855667447));
#49117=CARTESIAN_POINT('Ctrl Pts',(12.3951336511175,1.8287879857503,7.39699842932221));
#49118=CARTESIAN_POINT('Ctrl Pts',(15.088391402809,3.1815061164965,7.23999830196995));
#49119=CARTESIAN_POINT('Ctrl Pts',(17.7023877293502,1.68133718134365,7.0829981746177));
#49120=CARTESIAN_POINT('Ctrl Pts',(17.893127065655,-1.3265029163517,6.92599804726544));
#49121=CARTESIAN_POINT('Ctrl Pts',(15.4895715829936,-3.14485515809799,6.7689979199132));
#49122=CARTESIAN_POINT('Ctrl Pts',(12.6470126114897,-2.1431855409282,6.61199779256094));
#49123=CARTESIAN_POINT('Ctrl Pts',(11.9143999144365,0.780298978519449,6.45499766520869));
#49124=CARTESIAN_POINT('Ctrl Pts',(13.9486745921371,3.00408217741771,6.29799753785644));
#49125=CARTESIAN_POINT('Ctrl Pts',(16.9256825057651,2.53407556251617,6.14099741050418));
#49126=CARTESIAN_POINT('Ctrl Pts',(18.1759131113316,-0.208259934991238,
5.98399728315193));
#49127=CARTESIAN_POINT('Ctrl Pts',(16.5782706577155,-2.76384867084273,5.82699715579967));
#49128=CARTESIAN_POINT('Ctrl Pts',(13.5653803054279,-2.84106404628923,5.66999702844742));
#49129=CARTESIAN_POINT('Ctrl Pts',(11.8389222432929,-0.370677328850485,
5.51299690109516));
#49130=CARTESIAN_POINT('Ctrl Pts',(12.9470425851866,2.43211352025748,5.35599677374291));
#49131=CARTESIAN_POINT('Ctrl Pts',(15.8960507212661,3.05397713847976,5.19899664639066));
#49132=CARTESIAN_POINT('Ctrl Pts',(18.0415982494816,0.937364154516702,5.04199651903841));
#49133=CARTESIAN_POINT('Ctrl Pts',(17.459643977202,-2.01989749884988,4.88499639168616));
#49134=CARTESIAN_POINT('Ctrl Pts',(14.6722426504805,-3.16569257287314,4.7279962643339));
#49135=CARTESIAN_POINT('Ctrl Pts',(12.1784729871356,-1.4731805380298,4.57099613698165));
#49136=CARTESIAN_POINT('Ctrl Pts',(12.215322881631,1.54112605834992,4.41399600962939));
#49137=CARTESIAN_POINT('Ctrl Pts',(14.7481872905369,3.17196844909489,4.25699588227714));
#49138=CARTESIAN_POINT('Ctrl Pts',(17.5088738513129,1.96146864806794,4.09999575492489));
#49139=CARTESIAN_POINT('Ctrl Pts',(18.0158147471675,-1.0140076371251,3.94299562757263));
#49140=CARTESIAN_POINT('Ctrl Pts',(16.5566596891409,-2.38159377580301,3.83832887600446));
#49141=CARTESIAN_POINT('Ctrl Pts',(15.698066426161,-2.61113218593862,3.78599550022038));
#49142=CARTESIAN_POINT('Ctrl Pts',(17.1951971040191,1.87686343907872,12.2140044997796));
#49143=CARTESIAN_POINT('Ctrl Pts',(17.8123478989901,1.15503807360179,12.1616711239955));
#49144=CARTESIAN_POINT('Ctrl Pts',(18.2695195233736,-0.932473714789483,
12.0570043724274));
#49145=CARTESIAN_POINT('Ctrl Pts',(16.0220985187125,-3.24586736386177,11.9000042450751));
#49146=CARTESIAN_POINT('Ctrl Pts',(12.8583143384262,-2.6408513419267,11.7430041177229));
#49147=CARTESIAN_POINT('Ctrl Pts',(11.6149672212669,0.328384086517278,11.5860039903706));
#49148=CARTESIAN_POINT('Ctrl Pts',(13.4070235778454,3.00511912143942,11.4290038630183));
#49149=CARTESIAN_POINT('Ctrl Pts',(16.6275114271823,2.98612830149817,11.2720037356661));
#49150=CARTESIAN_POINT('Ctrl Pts',(18.3885970703671,0.289963978573797,11.1150036083139));
#49151=CARTESIAN_POINT('Ctrl Pts',(17.1110937259949,-2.66647876521353,10.9580034809616));
#49152=CARTESIAN_POINT('Ctrl Pts',(13.9405531465495,-3.23172848449065,10.8010033536093));
#49153=CARTESIAN_POINT('Ctrl Pts',(11.7200283335659,-0.899126013584159,
10.6440032262571));
#49154=CARTESIAN_POINT('Ctrl Pts',(12.4406857810575,2.23976716482285,10.4870030989048));
#49155=CARTESIAN_POINT('Ctrl Pts',(15.4563047387199,3.37022127835708,10.3300029715526));
#49156=CARTESIAN_POINT('Ctrl Pts',(18.0627509123809,1.47857505977427,10.1730028442003));
#49157=CARTESIAN_POINT('Ctrl Pts',(17.9227989331183,-1.73892843327666,10.0160027168481));
#49158=CARTESIAN_POINT('Ctrl Pts',(15.1619451243646,-3.39711563766634,9.85900258949583));
#49159=CARTESIAN_POINT('Ctrl Pts',(12.2558735618304,-2.00907793176401,9.70200246214356));
#49160=CARTESIAN_POINT('Ctrl Pts',(11.8104865060192,1.18051988264736,9.54500233479131));
#49161=CARTESIAN_POINT('Ctrl Pts',(14.2251667971895,3.31153385791409,9.38800220743906));
#49162=CARTESIAN_POINT('Ctrl Pts',(17.3346474556976,2.47306382524563,9.2310020800868));
#49163=CARTESIAN_POINT('Ctrl Pts',(18.3506273425917,-0.583026353208485,
9.07400195273456));
#49164=CARTESIAN_POINT('Ctrl Pts',(16.3620675471785,-3.11631116218659,8.91700182538229));
#49165=CARTESIAN_POINT('Ctrl Pts',(13.1521287149875,-2.85516987872383,8.76000169803006));
#49166=CARTESIAN_POINT('Ctrl Pts',(11.5991937918248,-0.0337703618144171,
8.60300157067778));
#49167=CARTESIAN_POINT('Ctrl Pts',(13.0957944213239,2.81791135635341,8.44600144332555));
#49168=CARTESIAN_POINT('Ctrl Pts',(16.2999144614232,3.1427449306896,8.28900131597327));
#49169=CARTESIAN_POINT('Ctrl Pts',(18.3383887330186,0.649448973758145,8.13200118862104));
#49170=CARTESIAN_POINT('Ctrl Pts',(17.3832978009075,-2.42621410729771,7.97500106126878));
#49171=CARTESIAN_POINT('Ctrl Pts',(14.2910808659327,-3.32626772340195,7.81800093391653));
#49172=CARTESIAN_POINT('Ctrl Pts',(11.8345585204434,-1.24362515961579,7.66100080656427));
#49173=CARTESIAN_POINT('Ctrl Pts',(12.2165179157807,1.95418801289184,7.50400067921202));
#49174=CARTESIAN_POINT('Ctrl Pts',(15.0944524029892,3.39966205172151,7.34700055185976));
#49175=CARTESIAN_POINT('Ctrl Pts',(17.8876905076099,1.7966265040084,7.19000042450751));
#49176=CARTESIAN_POINT('Ctrl Pts',(18.0915088438512,-1.41746124668302,7.03300029715526));
#49177=CARTESIAN_POINT('Ctrl Pts',(15.523141515798,-3.36049793640501,6.87600016980301));
#49178=CARTESIAN_POINT('Ctrl Pts',(12.4856682212804,-2.29014381443823,6.71900004245075));
#49179=CARTESIAN_POINT('Ctrl Pts',(11.7028202575859,0.833804094392522,6.5619999150985));
#49180=CARTESIAN_POINT('Ctrl Pts',(13.8765851888231,3.21007214974851,6.40499978774624));
#49181=CARTESIAN_POINT('Ctrl Pts',(17.0577265919963,2.70783717227864,6.247999660394));
#49182=CARTESIAN_POINT('Ctrl Pts',(18.3936855340856,-0.22254032271463,6.09099953304174));
#49183=CARTESIAN_POINT('Ctrl Pts',(16.6864927068848,-2.95336582703543,5.93399940568949));
#49184=CARTESIAN_POINT('Ctrl Pts',(13.4670084055473,-3.03587586225233,5.77699927833723));
#49185=CARTESIAN_POINT('Ctrl Pts',(11.6221670810891,-0.396094680375534,
5.61999915098498));
#49186=CARTESIAN_POINT('Ctrl Pts',(12.806271256009,2.59888359083319,5.46299902363272));
#49187=CARTESIAN_POINT('Ctrl Pts',(15.957492936352,3.26338840924436,5.30599889628048));
#49188=CARTESIAN_POINT('Ctrl Pts',(18.250160699591,1.00163923251032,5.14899876892821));
#49189=CARTESIAN_POINT('Ctrl Pts',(17.6283018117366,-2.15840190895786,4.99199864157597));
#49190=CARTESIAN_POINT('Ctrl Pts',(14.6497683227587,-3.38276417310961,4.8349985142237));
#49191=CARTESIAN_POINT('Ctrl Pts',(11.9850008259279,-1.57419655568344,4.67799838687146));
#49192=CARTESIAN_POINT('Ctrl Pts',(12.0243775183933,1.64680110163074,4.5209982595192));
#49193=CARTESIAN_POINT('Ctrl Pts',(14.7309204882355,3.38947038628386,4.36399813216696));
#49194=CARTESIAN_POINT('Ctrl Pts',(17.6809073792564,2.09596659076089,4.20699800481469));
#49195=CARTESIAN_POINT('Ctrl Pts',(18.2226092220303,-1.08353816018628,4.04999787746244));
#49196=CARTESIAN_POINT('Ctrl Pts',(16.663399873782,-2.54489970653575,3.94533112589427));
#49197=CARTESIAN_POINT('Ctrl Pts',(15.7459328543469,-2.79017756984216,3.89299775011019));
#49198=CARTESIAN_POINT('Ctrl Pts',(17.3360626576962,1.99730155693062,12.3210067496694));
#49199=CARTESIAN_POINT('Ctrl Pts',(17.9928159504458,1.22915673814361,12.2686733738853));
#49200=CARTESIAN_POINT('Ctrl Pts',(18.4793242270491,-0.9923104492142,12.1640066223172));
#49201=CARTESIAN_POINT('Ctrl Pts',(16.087686466823,-3.45415431109555,12.0070064949649));
#49202=CARTESIAN_POINT('Ctrl Pts',(12.7208826080511,-2.81031447841596,11.8500063676127));
#49203=CARTESIAN_POINT('Ctrl Pts',(11.3977500448602,0.349456456775644,11.6930062402604));
#49204=CARTESIAN_POINT('Ctrl Pts',(13.3048024582519,3.19795728077006,11.5360061129082));
#49205=CARTESIAN_POINT('Ctrl Pts',(16.7319486542021,3.17774782202826,11.3790059855559));
#49206=CARTESIAN_POINT('Ctrl Pts',(18.606042966971,0.308570934784431,11.2220058582037));
#49207=CARTESIAN_POINT('Ctrl Pts',(17.246562375271,-2.83758641060089,11.0650057308514));
#49208=CARTESIAN_POINT('Ctrl Pts',(13.8725685599584,-3.4391081414099,10.9080056034992));
#49209=CARTESIAN_POINT('Ctrl Pts',(11.5095529170344,-0.956822829736598,
10.7510054761469));
#49210=CARTESIAN_POINT('Ctrl Pts',(12.276454872669,2.38349277433771,10.5940053487947));
#49211=CARTESIAN_POINT('Ctrl Pts',(15.4855857629831,3.58648800243424,10.4370052214424));
#49212=CARTESIAN_POINT('Ctrl Pts',(18.2592872973176,1.57345505668517,10.2800050940901));
#49213=CARTESIAN_POINT('Ctrl Pts',(18.1103546151327,-1.85051527716861,10.1230049667379));
#49214=CARTESIAN_POINT('Ctrl Pts',(15.1723371249586,-3.61510816978504,9.96600483938563));
#49215=CARTESIAN_POINT('Ctrl Pts',(12.0797832739173,-2.13800023888626,9.80900471203338));
#49216=CARTESIAN_POINT('Ctrl Pts',(11.6058157803393,1.25627371203762,9.65200458468112));
#49217=CARTESIAN_POINT('Ctrl Pts',(14.1754458368614,3.52403461675767,9.49500445732887));
#49218=CARTESIAN_POINT('Ctrl Pts',(17.4844615229107,2.63176005547664,9.33800432997661));
#49219=CARTESIAN_POINT('Ctrl Pts',(18.565636725993,-0.620439089359897,9.18100420262437));
#49220=CARTESIAN_POINT('Ctrl Pts',(16.4494712699821,-3.31628450238807,9.0240040752721));
#49221=CARTESIAN_POINT('Ctrl Pts',(13.033551020433,-3.03838581184986,8.86700394791986));
#49222=CARTESIAN_POINT('Ctrl Pts',(11.3809644362075,-0.0359374021709085,
8.7100038205676));
#49223=CARTESIAN_POINT('Ctrl Pts',(12.9736017614192,2.99873641424856,8.55300369321535));
#49224=CARTESIAN_POINT('Ctrl Pts',(16.383329827636,3.34441452287188,8.39600356586309));
#49225=CARTESIAN_POINT('Ctrl Pts',(18.5526127662067,0.691124042072478,8.23900343851084));
#49226=CARTESIAN_POINT('Ctrl Pts',(17.5362337553543,-2.58190399634584,8.08200331115859));
#49227=CARTESIAN_POINT('Ctrl Pts',(14.2455896040548,-3.53971395275292,7.92500318380633));
#49228=CARTESIAN_POINT('Ctrl Pts',(11.6314324932481,-1.32342844760082,7.76800305645409));
#49229=CARTESIAN_POINT('Ctrl Pts',(12.0379021804438,2.07958804003338,7.61100292910183));
#49230=CARTESIAN_POINT('Ctrl Pts',(15.1005134031695,3.61781798694653,7.45400280174957));
#49231=CARTESIAN_POINT('Ctrl Pts',(18.0729932858696,1.91191582667314,7.29700267439733));
#49232=CARTESIAN_POINT('Ctrl Pts',(18.2898906220475,-1.50841957701434,7.14000254704506));
#49233=CARTESIAN_POINT('Ctrl Pts',(15.5567114486024,-3.57614071471203,6.98300241969282));
#49234=CARTESIAN_POINT('Ctrl Pts',(12.3243238310711,-2.43710208794826,6.82600229234056));
#49235=CARTESIAN_POINT('Ctrl Pts',(11.4912406007353,0.887309210265594,6.66900216498831));
#49236=CARTESIAN_POINT('Ctrl Pts',(13.8044957855091,3.41606212207931,6.51200203763605));
#49237=CARTESIAN_POINT('Ctrl Pts',(17.1897706782275,2.88159878204111,6.35500191028381));
#49238=CARTESIAN_POINT('Ctrl Pts',(18.6114579568395,-0.236820710438023,
6.19800178293155));
#49239=CARTESIAN_POINT('Ctrl Pts',(16.7947147560542,-3.14288298322814,6.04100165557929));
#49240=CARTESIAN_POINT('Ctrl Pts',(13.3686365056666,-3.23068767821543,5.88400152822705));
#49241=CARTESIAN_POINT('Ctrl Pts',(11.4054119188853,-0.421512031900586,
5.72700140087479));
#49242=CARTESIAN_POINT('Ctrl Pts',(12.6654999268314,2.7656536614089,5.57000127352253));
#49243=CARTESIAN_POINT('Ctrl Pts',(16.0189351514379,3.47279968000896,5.41300114617029));
#49244=CARTESIAN_POINT('Ctrl Pts',(18.4587231497003,1.06591431050395,5.25600101881802));
#49245=CARTESIAN_POINT('Ctrl Pts',(17.7969596462713,-2.29690631906584,5.09900089146578));
#49246=CARTESIAN_POINT('Ctrl Pts',(14.6272939950368,-3.59983577334609,4.94200076411352));
#49247=CARTESIAN_POINT('Ctrl Pts',(11.7915286647202,-1.67521257333708,4.78500063676127));
#49248=CARTESIAN_POINT('Ctrl Pts',(11.8334321551556,1.75247614491157,4.62800050940901));
#49249=CARTESIAN_POINT('Ctrl Pts',(14.713653685934,3.60697232347283,4.47100038205677));
#49250=CARTESIAN_POINT('Ctrl Pts',(17.8529409071999,2.23046453345384,4.3140002547045));
#49251=CARTESIAN_POINT('Ctrl Pts',(18.4294036968932,-1.15306868324745,4.15700012735226));
#49252=CARTESIAN_POINT('Ctrl Pts',(16.7701400584231,-2.7082056372685,4.05233337578409));
#49253=CARTESIAN_POINT('Ctrl Pts',(15.7937992825329,-2.9692229537457,4.));
#49254=CARTESIAN_POINT('Ctrl Pts',(16.9134659966651,1.63598720337493,12.));
#49255=CARTESIAN_POINT('Ctrl Pts',(16.9751046175812,1.57806203522303,12.));
#49256=CARTESIAN_POINT('Ctrl Pts',(17.0333781400082,1.51698823254714,12.));
#49257=CARTESIAN_POINT('Ctrl Pts',(17.0882869575319,1.45315007481724,12.));
#49258=CARTESIAN_POINT('Ctrl Pts',(17.144646063235,1.38762578124011,12.));
#49259=CARTESIAN_POINT('Ctrl Pts',(17.1974608152615,1.31918874417436,12.));
#49260=CARTESIAN_POINT('Ctrl Pts',(17.246706209466,1.24820595309377,12.));
#49261=CARTESIAN_POINT('Ctrl Pts',(17.2968789923958,1.17588641486748,12.));
#49262=CARTESIAN_POINT('Ctrl Pts',(17.3433471915708,1.10092373974675,12.));
#49263=CARTESIAN_POINT('Ctrl Pts',(17.3860513180704,1.02366428011772,12.));
#49264=CARTESIAN_POINT('Ctrl Pts',(17.4053930048836,0.988671683523578,12.));
#49265=CARTESIAN_POINT('Ctrl Pts',(17.4239620441889,0.953207420756028,12.));
#49266=CARTESIAN_POINT('Ctrl Pts',(17.4417503295423,0.917301461090561,12.));
#49267=CARTESIAN_POINT('Ctrl Pts',(17.4518550628932,0.896904883178727,12.));
#49268=CARTESIAN_POINT('Ctrl Pts',(17.4617078263978,0.876365752925188,12.));
#49269=CARTESIAN_POINT('Ctrl Pts',(17.4713068826732,0.855689404786285,12.));
#49270=CARTESIAN_POINT('Ctrl Pts',(17.4795241183999,0.837989495363037,12.));
#49271=CARTESIAN_POINT('Ctrl Pts',(17.4875575606575,0.820183889043797,12.));
#49272=CARTESIAN_POINT('Ctrl Pts',(17.4953933345483,0.802305631697034,12.));
#49273=CARTESIAN_POINT('Ctrl Pts',(17.5320009593848,0.718780947752926,12.));
#49274=CARTESIAN_POINT('Ctrl Pts',(17.5643466650844,0.633572893252199,12.));
#49275=CARTESIAN_POINT('Ctrl Pts',(17.5924032599934,0.547079296293481,12.));
#49276=CARTESIAN_POINT('Ctrl Pts',(17.6209190605514,0.45917004827483,12.));
#49277=CARTESIAN_POINT('Ctrl Pts',(17.6450046970528,0.369932078122487,12.));
#49278=CARTESIAN_POINT('Ctrl Pts',(17.6645925974806,0.27974597155399,12.));
#49279=CARTESIAN_POINT('Ctrl Pts',(17.6832979692358,0.193623180766213,12.));
#49280=CARTESIAN_POINT('Ctrl Pts',(17.6979018128389,0.106634841931331,12.));
#49281=CARTESIAN_POINT('Ctrl Pts',(17.7083066964275,0.0190916104279826,
12.));
#49282=CARTESIAN_POINT('Ctrl Pts',(17.7128967523775,-0.0195275944118574,
12.));
#49283=CARTESIAN_POINT('Ctrl Pts',(17.7166691326112,-0.0582549851430788,
12.));
#49284=CARTESIAN_POINT('Ctrl Pts',(17.7196128778618,-0.0970645844891166,
12.));
#49285=CARTESIAN_POINT('Ctrl Pts',(17.720985220376,-0.115157204130783,12.));
#49286=CARTESIAN_POINT('Ctrl Pts',(17.7221774501012,-0.13326769426837,12.));
#49287=CARTESIAN_POINT('Ctrl Pts',(17.7231883308136,-0.151393437782305,
12.));
#49288=CARTESIAN_POINT('Ctrl Pts',(17.724162595519,-0.168862632662539,12.));
#49289=CARTESIAN_POINT('Ctrl Pts',(17.7249684090533,-0.186348823197974,
12.));
#49290=CARTESIAN_POINT('Ctrl Pts',(17.7256040109254,-0.203825085573831,
12.));
#49291=CARTESIAN_POINT('Ctrl Pts',(17.7290683171088,-0.299078303780242,
12.));
#49292=CARTESIAN_POINT('Ctrl Pts',(17.7274898676139,-0.394183686637061,
12.));
#49293=CARTESIAN_POINT('Ctrl Pts',(17.7208064378308,-0.488742644592356,
12.));
#49294=CARTESIAN_POINT('Ctrl Pts',(17.71415791669,-0.582807705707687,12.));
#49295=CARTESIAN_POINT('Ctrl Pts',(17.7024579548962,-0.676332990245415,
12.));
#49296=CARTESIAN_POINT('Ctrl Pts',(17.6855973100545,-0.768943912339204,
12.));
#49297=CARTESIAN_POINT('Ctrl Pts',(17.6690987547922,-0.859565975160523,
12.));
#49298=CARTESIAN_POINT('Ctrl Pts',(17.6476591367551,-0.949313458601225,
12.));
#49299=CARTESIAN_POINT('Ctrl Pts',(17.6215530748909,-1.03794459575461,12.));
#49300=CARTESIAN_POINT('Ctrl Pts',(17.6062284518588,-1.08997231149527,12.));
#49301=CARTESIAN_POINT('Ctrl Pts',(17.5892948213721,-1.14161533429799,12.));
#49302=CARTESIAN_POINT('Ctrl Pts',(17.5707996132467,-1.19282361176805,12.));
#49303=CARTESIAN_POINT('Ctrl Pts',(17.5660385338913,-1.20600576527691,12.));
#49304=CARTESIAN_POINT('Ctrl Pts',(17.5611731178881,-1.21916127939291,12.));
#49305=CARTESIAN_POINT('Ctrl Pts',(17.5562068240413,-1.23228215182306,12.));
#49306=CARTESIAN_POINT('Ctrl Pts',(17.5231582789659,-1.31959590274395,12.));
#49307=CARTESIAN_POINT('Ctrl Pts',(17.4857269461903,-1.40516846103908,12.));
#49308=CARTESIAN_POINT('Ctrl Pts',(17.4442438276358,-1.48876399852657,12.));
#49309=CARTESIAN_POINT('Ctrl Pts',(17.4011939593262,-1.57551680317371,12.));
#49310=CARTESIAN_POINT('Ctrl Pts',(17.3537803586004,-1.6601411473433,12.));
#49311=CARTESIAN_POINT('Ctrl Pts',(17.302316868041,-1.74237153203792,12.));
#49312=CARTESIAN_POINT('Ctrl Pts',(17.2502282381553,-1.82560078887907,12.));
#49313=CARTESIAN_POINT('Ctrl Pts',(17.1939903374979,-1.90637839472423,12.));
#49314=CARTESIAN_POINT('Ctrl Pts',(17.133876364298,-1.98441530832993,12.));
#49315=CARTESIAN_POINT('Ctrl Pts',(17.0944014617075,-2.03565962639887,12.));
#49316=CARTESIAN_POINT('Ctrl Pts',(17.0532540884055,-2.08572182092047,12.));
#49317=CARTESIAN_POINT('Ctrl Pts',(17.0105008848643,-2.13451422415292,12.));
#49318=CARTESIAN_POINT('Ctrl Pts',(16.9990423392555,-2.14759137233113,12.));
#49319=CARTESIAN_POINT('Ctrl Pts',(16.9874683992165,-2.16057727630897,12.));
#49320=CARTESIAN_POINT('Ctrl Pts',(16.9757802548447,-2.17347017426791,12.));
#49321=CARTESIAN_POINT('Ctrl Pts',(16.9646250327531,-2.18577521906894,12.));
#49322=CARTESIAN_POINT('Ctrl Pts',(16.953371454143,-2.19798925370335,12.));
#49323=CARTESIAN_POINT('Ctrl Pts',(16.942023959817,-2.2101077517839,12.));
#49324=CARTESIAN_POINT('Ctrl Pts',(16.8702005619852,-2.28681117932109,12.));
#49325=CARTESIAN_POINT('Ctrl Pts',(16.7945813632066,-2.35973107336475,12.));
#49326=CARTESIAN_POINT('Ctrl Pts',(16.7155099454751,-2.42853427108366,12.));
#49327=CARTESIAN_POINT('Ctrl Pts',(16.6562063821765,-2.48013666937285,12.));
#49328=CARTESIAN_POINT('Ctrl Pts',(16.5949596324728,-2.52942316838901,12.));
#49329=CARTESIAN_POINT('Ctrl Pts',(16.5318955908763,-2.57624166180053,12.));
#49330=CARTESIAN_POINT('Ctrl Pts',(16.509253132243,-2.59305133294597,12.));
#49331=CARTESIAN_POINT('Ctrl Pts',(16.4863762692883,-2.60954274193113,12.));
#49332=CARTESIAN_POINT('Ctrl Pts',(16.4632703841368,-2.62570843265804,12.));
#49333=CARTESIAN_POINT('Ctrl Pts',(16.4439550552025,-2.63922211680365,12.));
#49334=CARTESIAN_POINT('Ctrl Pts',(16.4244771453842,-2.65250971655999,12.));
#49335=CARTESIAN_POINT('Ctrl Pts',(16.4048604457735,-2.66555338685653,12.));
#49336=CARTESIAN_POINT('Ctrl Pts',(16.3198883986288,-2.72205358257614,12.));
#49337=CARTESIAN_POINT('Ctrl Pts',(16.2322397460524,-2.7740341002851,12.));
#49338=CARTESIAN_POINT('Ctrl Pts',(16.1422018474634,-2.82118285115376,12.));
#49339=CARTESIAN_POINT('Ctrl Pts',(16.0701250286698,-2.85892620174232,12.));
#49340=CARTESIAN_POINT('Ctrl Pts',(15.9965161480314,-2.89357290485328,12.));
#49341=CARTESIAN_POINT('Ctrl Pts',(15.9215058272316,-2.92494553699154,12.));
#49342=CARTESIAN_POINT('Ctrl Pts',(15.8800022019638,-2.94230418782848,12.));
#49343=CARTESIAN_POINT('Ctrl Pts',(15.8380692864041,-2.95866019100725,12.));
#49344=CARTESIAN_POINT('Ctrl Pts',(15.795740524146,-2.97402278592473,12.));
#49345=CARTESIAN_POINT('Ctrl Pts',(12.4833920687165,-0.00213593309729046,
10.387416697508));
#49346=CARTESIAN_POINT('Ctrl Pts',(12.4814996767346,-0.226800666605093,
10.4016107071645));
#49347=CARTESIAN_POINT('Ctrl Pts',(12.5091661046464,-0.451007239373056,
10.415804716821));
#49348=CARTESIAN_POINT('Ctrl Pts',(12.5682644306803,-0.666597124996037,
10.4299987264775));
#49349=CARTESIAN_POINT('Ctrl Pts',(12.7861602176632,-1.46147797773692,10.4823321022615));
#49350=CARTESIAN_POINT('Ctrl Pts',(13.4313412686974,-2.13922357419454,10.5346654780456));
#49351=CARTESIAN_POINT('Ctrl Pts',(14.2145374788331,-2.39597875638779,10.5869988538297));
#49352=CARTESIAN_POINT('Ctrl Pts',(14.9977336889687,-2.65273393858105,10.6393322296138));
#49353=CARTESIAN_POINT('Ctrl Pts',(15.9189450582056,-2.48849870650994,10.6916656053979));
#49354=CARTESIAN_POINT('Ctrl Pts',(16.5651422177769,-1.97687883370916,10.743998981182));
#49355=CARTESIAN_POINT('Ctrl Pts',(17.2113393773482,-1.46525896090837,10.7963323569661));
#49356=CARTESIAN_POINT('Ctrl Pts',(17.5825223272538,-0.60625444737792,10.8486657327501));
#49357=CARTESIAN_POINT('Ctrl Pts',(17.5122690848705,0.214937675101548,10.9009991085342));
#49358=CARTESIAN_POINT('Ctrl Pts',(17.4420158424871,1.03612979758102,10.9533324843183));
#49359=CARTESIAN_POINT('Ctrl Pts',(16.9303264078149,1.8195095290095,11.0056658601024));
#49360=CARTESIAN_POINT('Ctrl Pts',(16.206619831127,2.2139583184471,11.0579992358865));
#49361=CARTESIAN_POINT('Ctrl Pts',(15.4829132544392,2.60840710788471,11.1103326116706));
#49362=CARTESIAN_POINT('Ctrl Pts',(14.5471895357358,2.61392495533142,11.1626659874547));
#49363=CARTESIAN_POINT('Ctrl Pts',(13.8189836358921,2.22781663625852,11.2149993632387));
#49364=CARTESIAN_POINT('Ctrl Pts',(13.0907777360484,1.84170831718561,11.2673327390228));
#49365=CARTESIAN_POINT('Ctrl Pts',(12.5700896550643,1.06397383159308,11.3196661148069));
#49366=CARTESIAN_POINT('Ctrl Pts',(12.4903749854216,0.243745852972027,11.371999490591));
#49367=CARTESIAN_POINT('Ctrl Pts',(12.4825471092477,0.163200539545801,11.3771385595633));
#49368=CARTESIAN_POINT('Ctrl Pts',(12.4789715321031,0.0822454620963692,
11.3822776285357));
#49369=CARTESIAN_POINT('Ctrl Pts',(12.4794948718273,0.00124609658704006,
11.387416697508));
#49370=CARTESIAN_POINT('Ctrl Pts',(14.2062007174671,-2.96922295374568,12.));
#49371=CARTESIAN_POINT('Ctrl Pts',(13.2298599415769,-2.70820563726846,11.9476666242159));
#49372=CARTESIAN_POINT('Ctrl Pts',(11.5705939465555,-1.15308308242658,11.8429998726477));
#49373=CARTESIAN_POINT('Ctrl Pts',(12.1470611574329,2.23047193499529,11.6859997452955));
#49374=CARTESIAN_POINT('Ctrl Pts',(15.2863460006058,3.60696666543133,11.5289996179432));
#49375=CARTESIAN_POINT('Ctrl Pts',(18.1665668486981,1.75247841941832,11.371999490591));
#49376=CARTESIAN_POINT('Ctrl Pts',(18.2084706556688,-1.6752137223659,11.2149993632387));
#49377=CARTESIAN_POINT('Ctrl Pts',(15.3727057323674,-3.59983386165072,11.0579992358865));
#49378=CARTESIAN_POINT('Ctrl Pts',(12.2030412422492,-2.29690621757914,10.9009991085342));
#49379=CARTESIAN_POINT('Ctrl Pts',(11.5412777161188,1.06591431606771,10.743998981182));
#49380=CARTESIAN_POINT('Ctrl Pts',(13.9810651784412,3.47279856287599,10.5869988538297));
#49381=CARTESIAN_POINT('Ctrl Pts',(17.3344994031312,2.76565299665532,10.4299987264775));
#49382=CARTESIAN_POINT('Ctrl Pts',(18.5945871152999,-0.421511967551375,
10.2729985991252));
#49383=CARTESIAN_POINT('Ctrl Pts',(16.6313630370479,-3.23068676566348,10.115998471773));
#49384=CARTESIAN_POINT('Ctrl Pts',(13.205285741413,-3.14288213812672,9.9589983444207));
#49385=CARTESIAN_POINT('Ctrl Pts',(11.388543028433,-0.236820637232293,9.80199821706845));
#49386=CARTESIAN_POINT('Ctrl Pts',(12.8102299232355,2.88159798857394,9.6449980897162));
#49387=CARTESIAN_POINT('Ctrl Pts',(16.1955038860992,3.41606118929613,9.48799796236394));
#49388=CARTESIAN_POINT('Ctrl Pts',(18.5087584392439,0.887308966009096,9.3309978350117));
#49389=CARTESIAN_POINT('Ctrl Pts',(17.6756754360527,-2.43710142000481,9.17399770765943));
#49390=CARTESIAN_POINT('Ctrl Pts',(14.4432887039958,-3.57613973602564,9.0169975803072));
#49391=CARTESIAN_POINT('Ctrl Pts',(11.7101102785552,-1.50841916383422,8.85999745295492));
#49392=CARTESIAN_POINT('Ctrl Pts',(11.9270075555053,1.91191530312036,8.70299732560268));
#49393=CARTESIAN_POINT('Ctrl Pts',(14.8994866243195,3.61781699652394,8.54599719825042));
#49394=CARTESIAN_POINT('Ctrl Pts',(17.9620970086125,2.07958747065415,8.38899707089818));
#49395=CARTESIAN_POINT('Ctrl Pts',(18.3685665845007,-1.32342808525659,8.23199694354591));
#49396=CARTESIAN_POINT('Ctrl Pts',(15.7544101894084,-3.53971298366467,8.07499681619367));
#49397=CARTESIAN_POINT('Ctrl Pts',(12.4637669390099,-2.58190328946754,7.91799668884141));
#49398=CARTESIAN_POINT('Ctrl Pts',(11.4473882064255,0.691123852849571,7.76099656148916));
#49399=CARTESIAN_POINT('Ctrl Pts',(13.6166705510885,3.34441360725337,7.60399643413689));
#49400=CARTESIAN_POINT('Ctrl Pts',(17.0263976837988,2.99873559323853,7.44699630678466));
#49401=CARTESIAN_POINT('Ctrl Pts',(18.6190345729722,-0.0359373922966709,
7.2899961794324));
#49402=CARTESIAN_POINT('Ctrl Pts',(16.9664484412042,-3.03838498006983,7.13299605208014));
#49403=CARTESIAN_POINT('Ctrl Pts',(13.5505291268344,-3.3162835943375,6.97599592472789));
#49404=CARTESIAN_POINT('Ctrl Pts',(11.4343642502377,-0.620438919723572,
6.81899579737564));
#49405=CARTESIAN_POINT('Ctrl Pts',(12.5155391572145,2.63175933537736,6.66199567002338));
#49406=CARTESIAN_POINT('Ctrl Pts',(15.824553937525,3.52403365117268,6.50499554267113));
#49407=CARTESIAN_POINT('Ctrl Pts',(18.3941832901488,1.25627336953411,6.34799541531888));
#49408=CARTESIAN_POINT('Ctrl Pts',(17.9202159270872,-2.13799965619268,6.19099528796662));
#49409=CARTESIAN_POINT('Ctrl Pts',(14.8276629212552,-3.61510717519363,6.03399516061437));
#49410=CARTESIAN_POINT('Ctrl Pts',(11.889646238299,-1.85051477939823,5.87699503326212));
#49411=CARTESIAN_POINT('Ctrl Pts',(11.7407135913467,1.57345464202167,5.71999490590987));
#49412=CARTESIAN_POINT('Ctrl Pts',(14.5144143770745,3.58648699137295,5.56299477855761));
#49413=CARTESIAN_POINT('Ctrl Pts',(17.7235443678513,2.3834921742297,5.40599465120536));
#49414=CARTESIAN_POINT('Ctrl Pts',(18.4904461542425,-0.956822661448993,
5.2489945238531));
#49415=CARTESIAN_POINT('Ctrl Pts',(16.1274310791049,-3.43910703392132,5.09199439650085));
#49416=CARTESIAN_POINT('Ctrl Pts',(12.7534383414036,-2.83758592474999,4.9349942691486));
#49417=CARTESIAN_POINT('Ctrl Pts',(11.3939578227468,0.308571354444121,4.77799414179634));
#49418=CARTESIAN_POINT('Ctrl Pts',(13.2680522040149,3.17774609218688,4.62099401444409));
#49419=CARTESIAN_POINT('Ctrl Pts',(16.6951963308219,3.19795784272698,4.46399388709183));
#49420=CARTESIAN_POINT('Ctrl Pts',(18.6022504225887,0.349454018091392,4.30699375973959));
#49421=CARTESIAN_POINT('Ctrl Pts',(17.2791139286761,-2.8103099931699,4.14999363238733));
#49422=CARTESIAN_POINT('Ctrl Pts',(13.9123194271849,-3.45415924122653,3.99299350503508));
#49423=CARTESIAN_POINT('Ctrl Pts',(11.5206656746196,-0.992299917670973,
3.83599337768282));
#49424=CARTESIAN_POINT('Ctrl Pts',(12.0071840495542,1.22915673814367,3.73132662611465));
#49425=CARTESIAN_POINT('Ctrl Pts',(12.6639373423039,1.99730155693067,3.67899325033057));
#49426=CARTESIAN_POINT('Ctrl Pts',(14.254067145653,-2.79017756984214,12.1070022498898));
#49427=CARTESIAN_POINT('Ctrl Pts',(13.336600126218,-2.54489970653572,12.0546688741057));
#49428=CARTESIAN_POINT('Ctrl Pts',(11.7773885635194,-1.08355169108889,11.9500021225376));
#49429=CARTESIAN_POINT('Ctrl Pts',(12.3190945608781,2.0959735459863,11.7930019951853));
#49430=CARTESIAN_POINT('Ctrl Pts',(15.2690792172061,3.38946506942463,11.636001867833));
#49431=CARTESIAN_POINT('Ctrl Pts',(17.9756215455284,1.64680323898379,11.4790017404808));
#49432=CARTESIAN_POINT('Ctrl Pts',(18.014998535442,-1.57419763542533,11.3220016131285));
#49433=CARTESIAN_POINT('Ctrl Pts',(15.3502314210832,-3.38276237669027,11.1650014857763));
#49434=CARTESIAN_POINT('Ctrl Pts',(12.3716990232057,-2.15840181359085,11.008001358424));
#49435=CARTESIAN_POINT('Ctrl Pts',(11.7498401140189,1.00163923773859,10.8510012310718));
#49436=CARTESIAN_POINT('Ctrl Pts',(14.0425073736352,3.26338735947497,10.6940011037195));
#49437=CARTESIAN_POINT('Ctrl Pts',(17.1937281143572,2.59888296616453,10.5370009763673));
#49438=CARTESIAN_POINT('Ctrl Pts',(18.3778320113351,-0.396094619906611,
10.380000849015));
#49439=CARTESIAN_POINT('Ctrl Pts',(16.5329911647418,-3.03587500472764,10.2230007216628));
#49440=CARTESIAN_POINT('Ctrl Pts',(13.3135077605849,-2.95336503289398,10.0660005943105));
#49441=CARTESIAN_POINT('Ctrl Pts',(11.6063153917746,-0.222540253923235,
9.90900046695825));
#49442=CARTESIAN_POINT('Ctrl Pts',(12.9422739731982,2.70783642665787,9.75200033960602));
#49443=CARTESIAN_POINT('Ctrl Pts',(16.1234145025873,3.21007127321255,9.59500021225374));
#49444=CARTESIAN_POINT('Ctrl Pts',(18.297178840283,0.83380386486479,9.43800008490151));
#49445=CARTESIAN_POINT('Ctrl Pts',(17.5143310900362,-2.29014318677205,9.28099995754924));
#49446=CARTESIAN_POINT('Ctrl Pts',(14.4768586275985,-3.36049701673381,9.12399983019701));
#49447=CARTESIAN_POINT('Ctrl Pts',(11.9084920024447,-1.41746085841783,8.96699970284473));
#49448=CARTESIAN_POINT('Ctrl Pts',(12.1123102830297,1.79662601202607,8.8099995754925));
#49449=CARTESIAN_POINT('Ctrl Pts',(14.9055476228422,3.39966112102182,8.65299944814023));
#49450=CARTESIAN_POINT('Ctrl Pts',(17.7834813221759,1.95418747784641,8.49599932078799));
#49451=CARTESIAN_POINT('Ctrl Pts',(18.1654406129175,-1.24362481912106,8.33899919343572));
#49452=CARTESIAN_POINT('Ctrl Pts',(15.7089189399847,-3.32626681275013,8.18199906608348));
#49453=CARTESIAN_POINT('Ctrl Pts',(12.6167028515863,-2.42621344304447,8.02499893873122));
#49454=CARTESIAN_POINT('Ctrl Pts',(11.6616121809635,0.649448795945457,7.86799881137897));
#49455=CARTESIAN_POINT('Ctrl Pts',(13.7000858944641,3.14274407028327,7.71099868402671));
#49456=CARTESIAN_POINT('Ctrl Pts',(16.9042050573477,2.81791058485063,7.55399855667447));
#49457=CARTESIAN_POINT('Ctrl Pts',(18.4008052771018,-0.033770352535599,
7.3969984293222));
#49458=CARTESIAN_POINT('Ctrl Pts',(16.8478707791132,-2.85516909710049,7.23999830196996));
#49459=CARTESIAN_POINT('Ctrl Pts',(13.6379328257098,-3.11631030889185,7.08299817461769));
#49460=CARTESIAN_POINT('Ctrl Pts',(11.6493735747719,-0.583026193801301,
6.92599804726545));
#49461=CARTESIAN_POINT('Ctrl Pts',(12.6653531834158,2.47306314856864,6.76899791991319));
#49462=CARTESIAN_POINT('Ctrl Pts',(15.7748329908015,3.31153295055427,6.61199779256095));
#49463=CARTESIAN_POINT('Ctrl Pts',(18.1895126205188,1.18051956079695,6.45499766520868));
#49464=CARTESIAN_POINT('Ctrl Pts',(17.7441256873539,-2.00907738420709,6.29799753785643));
#49465=CARTESIAN_POINT('Ctrl Pts',(14.8380549190625,-3.39711470304921,6.14099741050418));
#49466=CARTESIAN_POINT('Ctrl Pts',(12.0772018688511,-1.73892796552204,5.98399728315193));
#49467=CARTESIAN_POINT('Ctrl Pts',(11.9372499226966,1.47857467011516,5.82699715579967));
#49468=CARTESIAN_POINT('Ctrl Pts',(14.5436953928922,3.3702203282632,5.66999702844742));
#49469=CARTESIAN_POINT('Ctrl Pts',(17.5593135052598,2.2397666009016,5.51299690109516));
#49470=CARTESIAN_POINT('Ctrl Pts',(18.2799707937134,-0.89912585544437,5.35599677374292));
#49471=CARTESIAN_POINT('Ctrl Pts',(16.0594465142784,-3.23172744378409,5.19899664639066));
#49472=CARTESIAN_POINT('Ctrl Pts',(12.888906947464,-2.66647830865965,5.04199651903841));
#49473=CARTESIAN_POINT('Ctrl Pts',(11.6114036717303,0.289964372927834,4.88499639168615));
#49474=CARTESIAN_POINT('Ctrl Pts',(13.3724893792839,2.98612667596695,4.72799626433391));
#49475=CARTESIAN_POINT('Ctrl Pts',(16.5929752842478,3.0051196495101,4.57099613698165));
#49476=CARTESIAN_POINT('Ctrl Pts',(18.3850332179946,0.328381794886706,4.41399600962939));
#49477=CARTESIAN_POINT('Ctrl Pts',(17.1416824071377,-2.64084712714285,4.25699588227714));
#49478=CARTESIAN_POINT('Ctrl Pts',(13.9779070198844,-3.24587199670379,4.09999575492489));
#49479=CARTESIAN_POINT('Ctrl Pts',(11.7304709872286,-0.932463818302713,
3.94299562757263));
#49480=CARTESIAN_POINT('Ctrl Pts',(12.1876521010099,1.15503807360185,3.83832887600446));
#49481=CARTESIAN_POINT('Ctrl Pts',(12.8048028959809,1.87686343907877,3.78599550022038));
#49482=CARTESIAN_POINT('Ctrl Pts',(14.3019335738389,-2.6111321859386,12.2140044997796));
#49483=CARTESIAN_POINT('Ctrl Pts',(13.4433403108591,-2.38159377580297,12.1616711239955));
#49484=CARTESIAN_POINT('Ctrl Pts',(11.9841831804832,-1.0140202997512,12.0570043724274));
#49485=CARTESIAN_POINT('Ctrl Pts',(12.4911279643235,1.96147515697731,11.9000042450751));
#49486=CARTESIAN_POINT('Ctrl Pts',(15.2518124338064,3.17196347341793,11.7430041177229));
#49487=CARTESIAN_POINT('Ctrl Pts',(17.7846762423587,1.54112805854926,11.5860039903706));
#49488=CARTESIAN_POINT('Ctrl Pts',(17.8215264152151,-1.47318154848477,11.4290038630184));
#49489=CARTESIAN_POINT('Ctrl Pts',(15.3277571097989,-3.16569089172983,11.2720037356661));
#49490=CARTESIAN_POINT('Ctrl Pts',(12.5403568041622,-2.01989740960257,11.1150036083138));
#49491=CARTESIAN_POINT('Ctrl Pts',(11.958402511919,0.937364159409468,10.9580034809616));
#49492=CARTESIAN_POINT('Ctrl Pts',(14.1039495688293,3.05397615607396,10.8010033536093));
#49493=CARTESIAN_POINT('Ctrl Pts',(17.0529568255832,2.43211293567374,10.6440032262571));
#49494=CARTESIAN_POINT('Ctrl Pts',(18.1610769073704,-0.370677272261844,
10.4870030989048));
#49495=CARTESIAN_POINT('Ctrl Pts',(16.4346192924356,-2.8410632437918,10.3300029715526));
#49496=CARTESIAN_POINT('Ctrl Pts',(13.4217297797568,-2.76384792766124,10.1730028442003));
#49497=CARTESIAN_POINT('Ctrl Pts',(11.8240877551162,-0.208259870614178,
10.0160027168481));
#49498=CARTESIAN_POINT('Ctrl Pts',(13.0743180231609,2.5340748647418,9.85900258949582));
#49499=CARTESIAN_POINT('Ctrl Pts',(16.0513251190755,3.00408135712897,9.70200246214356));
#49500=CARTESIAN_POINT('Ctrl Pts',(18.085599241322,0.780298763720488,9.54500233479132));
#49501=CARTESIAN_POINT('Ctrl Pts',(17.3529867440197,-2.14318495353929,9.38800220743906));
#49502=CARTESIAN_POINT('Ctrl Pts',(14.5104285512012,-3.14485429744199,9.23100208008681));
#49503=CARTESIAN_POINT('Ctrl Pts',(12.1068737263342,-1.32650255300144,9.07400195273456));
#49504=CARTESIAN_POINT('Ctrl Pts',(12.2976130105542,1.68133672093178,8.9170018253823));
#49505=CARTESIAN_POINT('Ctrl Pts',(14.9116086213649,3.1815052455197,8.76000169803005));
#49506=CARTESIAN_POINT('Ctrl Pts',(17.6048656357394,1.82878748503868,8.60300157067779));
#49507=CARTESIAN_POINT('Ctrl Pts',(17.9623146413344,-1.16382155298553,8.44600144332554));
#49508=CARTESIAN_POINT('Ctrl Pts',(15.663427690561,-3.11282064183558,8.28900131597329));
#49509=CARTESIAN_POINT('Ctrl Pts',(12.7696387641627,-2.27052359662139,8.13200118862103));
#49510=CARTESIAN_POINT('Ctrl Pts',(11.8758361555014,0.607773739041346,7.97500106126878));
#49511=CARTESIAN_POINT('Ctrl Pts',(13.7835012378397,2.94107453331316,7.81800093391652));
#49512=CARTESIAN_POINT('Ctrl Pts',(16.7820124308966,2.63708557646273,7.66100080656428));
#49513=CARTESIAN_POINT('Ctrl Pts',(18.1825759812315,-0.031603312774529,
7.50400067921202));
#49514=CARTESIAN_POINT('Ctrl Pts',(16.7292931170223,-2.67195321413115,7.34700055185977));
#49515=CARTESIAN_POINT('Ctrl Pts',(13.7253365245851,-2.9163370234462,7.1900004245075));
#49516=CARTESIAN_POINT('Ctrl Pts',(11.8643828993062,-0.545613467879027,
7.03300029715527));
#49517=CARTESIAN_POINT('Ctrl Pts',(12.8151672096171,2.31436696175991,6.876000169803));
#49518=CARTESIAN_POINT('Ctrl Pts',(15.725112044078,3.09903224993587,6.71900004245076));
#49519=CARTESIAN_POINT('Ctrl Pts',(17.9848419508889,1.10476575205979,6.56199991509849));
#49520=CARTESIAN_POINT('Ctrl Pts',(17.5680354476207,-1.8801551122215,6.40499978774625));
#49521=CARTESIAN_POINT('Ctrl Pts',(14.8484469168698,-3.17912223090478,6.24799966039399));
#49522=CARTESIAN_POINT('Ctrl Pts',(12.2647574994032,-1.62734115164585,6.09099953304174));
#49523=CARTESIAN_POINT('Ctrl Pts',(12.1337862540464,1.38369469820864,5.93399940568949));
#49524=CARTESIAN_POINT('Ctrl Pts',(14.5729764087098,3.15395366515346,5.77699927833723));
#49525=CARTESIAN_POINT('Ctrl Pts',(17.3950826426682,2.0960410275735,5.61999915098498));
#49526=CARTESIAN_POINT('Ctrl Pts',(18.0694954331843,-0.841429049439745,
5.46299902363272));
#49527=CARTESIAN_POINT('Ctrl Pts',(15.991461949452,-3.02434785364687,5.30599889628047));
#49528=CARTESIAN_POINT('Ctrl Pts',(13.0243755535244,-2.49537069256931,5.14899876892822));
#49529=CARTESIAN_POINT('Ctrl Pts',(11.8288495207139,0.271357391411547,4.99199864157596));
#49530=CARTESIAN_POINT('Ctrl Pts',(13.4769265545529,2.79450725974701,4.83499851422372));
#49531=CARTESIAN_POINT('Ctrl Pts',(16.4907542376736,2.81228145629323,4.67799838687145));
#49532=CARTESIAN_POINT('Ctrl Pts',(18.1678160134006,0.307309571682018,4.52099825951921));
#49533=CARTESIAN_POINT('Ctrl Pts',(17.0042508855994,-2.47138426111579,4.36399813216695));
#49534=CARTESIAN_POINT('Ctrl Pts',(14.0434946125838,-3.03758475218105,4.2069980048147));
#49535=CARTESIAN_POINT('Ctrl Pts',(11.9402762998377,-0.872627718934448,
4.04999787746244));
#49536=CARTESIAN_POINT('Ctrl Pts',(12.3681201524657,1.08091940906002,3.94533112589428));
#49537=CARTESIAN_POINT('Ctrl Pts',(12.9456684496579,1.75642532122687,3.89299775011019));
#49538=CARTESIAN_POINT('Ctrl Pts',(14.3498000020249,-2.43208680203506,12.3210067496694));
#49539=CARTESIAN_POINT('Ctrl Pts',(13.5500804955002,-2.21828784507023,12.2686733738853));
#49540=CARTESIAN_POINT('Ctrl Pts',(12.1909777974471,-0.944488908413503,
12.1640066223172));
#49541=CARTESIAN_POINT('Ctrl Pts',(12.6631613677687,1.82697676796832,12.0070064949649));
#49542=CARTESIAN_POINT('Ctrl Pts',(15.2345456504068,2.95446187741122,11.8500063676127));
#49543=CARTESIAN_POINT('Ctrl Pts',(17.593730939189,1.43545287811473,11.6930062402604));
#49544=CARTESIAN_POINT('Ctrl Pts',(17.6280542949882,-1.37216546154421,11.5360061129082));
#49545=CARTESIAN_POINT('Ctrl Pts',(15.3052827985147,-2.94861940676938,11.3790059855559));
#49546=CARTESIAN_POINT('Ctrl Pts',(12.7090145851187,-1.88139300561428,11.2220058582036));
#49547=CARTESIAN_POINT('Ctrl Pts',(12.1669649098191,0.873089081080348,11.0650057308514));
#49548=CARTESIAN_POINT('Ctrl Pts',(14.1653917640233,2.84456495267294,10.9080056034991));
#49549=CARTESIAN_POINT('Ctrl Pts',(16.9121855368091,2.26534290518294,10.7510054761469));
#49550=CARTESIAN_POINT('Ctrl Pts',(17.9443218034057,-0.345259924617078,
10.5940053487946));
#49551=CARTESIAN_POINT('Ctrl Pts',(16.3362474201295,-2.64625148285596,10.4370052214424));
#49552=CARTESIAN_POINT('Ctrl Pts',(13.5299517989286,-2.57433082242851,10.2800050940901));
#49553=CARTESIAN_POINT('Ctrl Pts',(12.0418601184578,-0.193979487305122,
10.1230049667379));
#49554=CARTESIAN_POINT('Ctrl Pts',(13.2063620731236,2.36031330282573,9.96600483938562));
#49555=CARTESIAN_POINT('Ctrl Pts',(15.9792357355636,2.79809144104539,9.80900471203338));
#49556=CARTESIAN_POINT('Ctrl Pts',(17.874019642361,0.726793662576183,9.65200458468112));
#49557=CARTESIAN_POINT('Ctrl Pts',(17.1916423980032,-1.99622672030653,9.49500445732887));
#49558=CARTESIAN_POINT('Ctrl Pts',(14.5439984748038,-2.92921157815017,9.33800432997662));
#49559=CARTESIAN_POINT('Ctrl Pts',(12.3052554502237,-1.23554424758505,9.18100420262436));
#49560=CARTESIAN_POINT('Ctrl Pts',(12.4829157380786,1.56604742983749,9.02400407527211));
#49561=CARTESIAN_POINT('Ctrl Pts',(14.9176696198875,2.96334937001758,8.86700394791986));
#49562=CARTESIAN_POINT('Ctrl Pts',(17.4262499493028,1.70338749223094,8.7100038205676));
#49563=CARTESIAN_POINT('Ctrl Pts',(17.7591886697512,-1.08401828684999,8.55300369321535));
#49564=CARTESIAN_POINT('Ctrl Pts',(15.6179364411373,-2.89937447092104,8.3960035658631));
#49565=CARTESIAN_POINT('Ctrl Pts',(12.922574676739,-2.11483375019832,8.23900343851085));
#49566=CARTESIAN_POINT('Ctrl Pts',(12.0900601300394,0.566098682137233,8.08200331115859));
#49567=CARTESIAN_POINT('Ctrl Pts',(13.8669165812153,2.73940499634305,7.92500318380633));
#49568=CARTESIAN_POINT('Ctrl Pts',(16.6598198044455,2.45626056807483,7.76800305645408));
#49569=CARTESIAN_POINT('Ctrl Pts',(17.9643466853611,-0.029436273013457,
7.61100292910183));
#49570=CARTESIAN_POINT('Ctrl Pts',(16.6107154549314,-2.4887373311618,7.45400280174958));
#49571=CARTESIAN_POINT('Ctrl Pts',(13.8127402234604,-2.71636373800054,7.29700267439732));
#49572=CARTESIAN_POINT('Ctrl Pts',(12.0793922238404,-0.508200741956758,
7.14000254704508));
#49573=CARTESIAN_POINT('Ctrl Pts',(12.9649812358183,2.15567077495119,6.98300241969281));
#49574=CARTESIAN_POINT('Ctrl Pts',(15.6753910973545,2.88653154931746,6.82600229234056));
#49575=CARTESIAN_POINT('Ctrl Pts',(17.780171281259,1.02901194332264,6.66900216498831));
#49576=CARTESIAN_POINT('Ctrl Pts',(17.3919452078874,-1.75123284023591,6.51200203763606));
#49577=CARTESIAN_POINT('Ctrl Pts',(14.8588389146771,-2.96112975876036,6.3550019102838));
#49578=CARTESIAN_POINT('Ctrl Pts',(12.4523131299553,-1.51575433776966,6.19800178293155));
#49579=CARTESIAN_POINT('Ctrl Pts',(12.3303225853962,1.28881472630212,6.04100165557929));
#49580=CARTESIAN_POINT('Ctrl Pts',(14.6022574245275,2.93768700204372,5.88400152822705));
#49581=CARTESIAN_POINT('Ctrl Pts',(17.2308517800767,1.95231545424541,5.72700140087478));
#49582=CARTESIAN_POINT('Ctrl Pts',(17.8590200726551,-0.783732243435121,
5.57000127352254));
#49583=CARTESIAN_POINT('Ctrl Pts',(15.9234773846255,-2.81696826350965,5.41300114617029));
#49584=CARTESIAN_POINT('Ctrl Pts',(13.1598441595847,-2.32426307647897,5.25600101881803));
#49585=CARTESIAN_POINT('Ctrl Pts',(12.0462953696974,0.252750409895257,5.09900089146578));
#49586=CARTESIAN_POINT('Ctrl Pts',(13.5813637298219,2.60288784352708,4.94200076411352));
#49587=CARTESIAN_POINT('Ctrl Pts',(16.3885331910994,2.61944326307635,4.78500063676127));
#49588=CARTESIAN_POINT('Ctrl Pts',(17.9505988088066,0.286237348477332,4.62800050940901));
#49589=CARTESIAN_POINT('Ctrl Pts',(16.8668193640612,-2.30192139508873,4.47100038205677));
#49590=CARTESIAN_POINT('Ctrl Pts',(14.1090822052833,-2.82929750765831,4.3140002547045));
#49591=CARTESIAN_POINT('Ctrl Pts',(12.1500816124467,-0.812791619566185,
4.15700012735226));
#49592=CARTESIAN_POINT('Ctrl Pts',(12.5485882039215,1.0068007445182,4.05233337578409));
#49593=CARTESIAN_POINT('Ctrl Pts',(13.086534003335,1.63598720337497,4.));
#49594=CARTESIAN_POINT('Ctrl Pts',(12.4841021658346,0.00201143405015815,
11.112583302492));
#49595=CARTESIAN_POINT('Ctrl Pts',(12.4821471482924,0.253216278985343,11.0967241119451));
#49596=CARTESIAN_POINT('Ctrl Pts',(12.5168205167969,0.503894392425629,11.0808649213983));
#49597=CARTESIAN_POINT('Ctrl Pts',(12.5903776647364,0.742588045230009,11.0650057308514));
#49598=CARTESIAN_POINT('Ctrl Pts',(12.8331071945538,1.53024770494455,11.0126723550673));
#49599=CARTESIAN_POINT('Ctrl Pts',(13.4992494792886,2.18740632880874,10.9603389792832));
#49600=CARTESIAN_POINT('Ctrl Pts',(14.2901195837869,2.41944863282584,10.9080056034991));
#49601=CARTESIAN_POINT('Ctrl Pts',(15.0809896882853,2.65149093684294,10.8556722277151));
#49602=CARTESIAN_POINT('Ctrl Pts',(15.9965876125472,2.45841692101294,10.803338851931));
#49603=CARTESIAN_POINT('Ctrl Pts',(16.6264092857776,1.92677944146461,10.7510054761469));
#49604=CARTESIAN_POINT('Ctrl Pts',(17.256230959008,1.39514196191627,10.6986721003628));
#49605=CARTESIAN_POINT('Ctrl Pts',(17.6002763812068,0.524941018649596,10.6463387245787));
#49606=CARTESIAN_POINT('Ctrl Pts',(17.5042866950936,-0.293658046023555,
10.5940053487946));
#49607=CARTESIAN_POINT('Ctrl Pts',(17.4082970089803,-1.11225711069671,10.5416719730106));
#49608=CARTESIAN_POINT('Ctrl Pts',(16.8722722145549,-1.87925429677634,10.4893385972265));
#49609=CARTESIAN_POINT('Ctrl Pts',(16.1365438804754,-2.25076611307824,10.4370052214424));
#49610=CARTESIAN_POINT('Ctrl Pts',(15.4008155463959,-2.62227792938014,10.3846718456583));
#49611=CARTESIAN_POINT('Ctrl Pts',(14.4653836726623,-2.59830437590432,10.3323384698742));
#49612=CARTESIAN_POINT('Ctrl Pts',(13.749652455717,-2.18959237664585,10.2800050940901));
#49613=CARTESIAN_POINT('Ctrl Pts',(13.0339212387717,-1.78088037738738,10.2276717183061));
#49614=CARTESIAN_POINT('Ctrl Pts',(12.5378906786147,-0.98742993234625,10.175338342522));
#49615=CARTESIAN_POINT('Ctrl Pts',(12.4839590576472,-0.164989244803877,
10.1230049667379));
#49616=CARTESIAN_POINT('Ctrl Pts',(12.4803790780928,-0.110395654006944,
10.1195310786559));
#49617=CARTESIAN_POINT('Ctrl Pts',(12.4787471194664,-0.0556743234800699,
10.1160571905739));
#49618=CARTESIAN_POINT('Ctrl Pts',(12.4790122776664,-0.000936909191352325,
10.112583302492));
#49619=CARTESIAN_POINT('Ctrl Pts',(14.2062007174671,-2.96922295374568,12.));
#49620=CARTESIAN_POINT('Ctrl Pts',(14.1131167498864,-2.9351724226013,12.));
#49621=CARTESIAN_POINT('Ctrl Pts',(14.0220959175279,-2.89635937351053,12.));
#49622=CARTESIAN_POINT('Ctrl Pts',(13.9333480734334,-2.85311020134011,12.));
#49623=CARTESIAN_POINT('Ctrl Pts',(13.8426550828426,-2.80891310782501,12.));
#49624=CARTESIAN_POINT('Ctrl Pts',(13.7543351402525,-2.76008268621842,12.));
#49625=CARTESIAN_POINT('Ctrl Pts',(13.6686411145779,-2.7069217762808,12.));
#49626=CARTESIAN_POINT('Ctrl Pts',(13.5868027530609,-2.65615275554924,12.));
#49627=CARTESIAN_POINT('Ctrl Pts',(13.5073590893475,-2.60143327816087,12.));
#49628=CARTESIAN_POINT('Ctrl Pts',(13.4305625059366,-2.54299781905995,12.));
#49629=CARTESIAN_POINT('Ctrl Pts',(13.3633654954521,-2.49186679234665,12.));
#49630=CARTESIAN_POINT('Ctrl Pts',(13.298195438544,-2.43789004325195,12.));
#49631=CARTESIAN_POINT('Ctrl Pts',(13.235245315039,-2.38121225533745,12.));
#49632=CARTESIAN_POINT('Ctrl Pts',(13.2201383978307,-2.36761058782836,12.));
#49633=CARTESIAN_POINT('Ctrl Pts',(13.2051557596309,-2.35384973663533,12.));
#49634=CARTESIAN_POINT('Ctrl Pts',(13.1903225084953,-2.33995287271397,12.));
#49635=CARTESIAN_POINT('Ctrl Pts',(13.1178922144325,-2.27209492767057,12.));
#49636=CARTESIAN_POINT('Ctrl Pts',(13.0489277577742,-2.20091637429481,12.));
#49637=CARTESIAN_POINT('Ctrl Pts',(12.9836701413723,-2.12670552844038,12.));
#49638=CARTESIAN_POINT('Ctrl Pts',(12.9187777778625,-2.05291004752833,12.));
#49639=CARTESIAN_POINT('Ctrl Pts',(12.8575503884276,-1.97611533073339,12.));
#49640=CARTESIAN_POINT('Ctrl Pts',(12.800268550456,-1.89657810132058,12.));
#49641=CARTESIAN_POINT('Ctrl Pts',(12.7459133734412,-1.82110461204208,12.));
#49642=CARTESIAN_POINT('Ctrl Pts',(12.6951108248742,-1.74316096291563,12.));
#49643=CARTESIAN_POINT('Ctrl Pts',(12.6481432361601,-1.66295348615981,12.));
#49644=CARTESIAN_POINT('Ctrl Pts',(12.6107661639977,-1.59912392350293,12.));
#49645=CARTESIAN_POINT('Ctrl Pts',(12.5758185286433,-1.533860318552,12.));
#49646=CARTESIAN_POINT('Ctrl Pts',(12.5434639629309,-1.46726456665475,12.));
#49647=CARTESIAN_POINT('Ctrl Pts',(12.5375614518629,-1.45511536440159,12.));
#49648=CARTESIAN_POINT('Ctrl Pts',(12.5317470084536,-1.4429252625298,12.));
#49649=CARTESIAN_POINT('Ctrl Pts',(12.5260248255016,-1.43070222232707,12.));
#49650=CARTESIAN_POINT('Ctrl Pts',(12.4854475610481,-1.34402594180728,12.));
#49651=CARTESIAN_POINT('Ctrl Pts',(12.4494522312093,-1.25558570069036,12.));
#49652=CARTESIAN_POINT('Ctrl Pts',(12.4183023908741,-1.16562505800954,12.));
#49653=CARTESIAN_POINT('Ctrl Pts',(12.3871525505389,-1.07566441532873,12.));
#49654=CARTESIAN_POINT('Ctrl Pts',(12.3608477335802,-0.984182637916221,
12.));
#49655=CARTESIAN_POINT('Ctrl Pts',(12.3397077040223,-0.891413467157708,
12.));
#49656=CARTESIAN_POINT('Ctrl Pts',(12.3185427547458,-0.798534940751147,
12.));
#49657=CARTESIAN_POINT('Ctrl Pts',(12.3025555503081,-0.704364799779564,
12.));
#49658=CARTESIAN_POINT('Ctrl Pts',(12.2916706351494,-0.609311329981899,
12.));
#49659=CARTESIAN_POINT('Ctrl Pts',(12.2861036872675,-0.560697472671795,
12.));
#49660=CARTESIAN_POINT('Ctrl Pts',(12.2818721595795,-0.511852737800975,
12.));
#49661=CARTESIAN_POINT('Ctrl Pts',(12.2789708979829,-0.462833545994333,
12.));
#49662=CARTESIAN_POINT('Ctrl Pts',(12.2781343831999,-0.448699943341852,
12.));
#49663=CARTESIAN_POINT('Ctrl Pts',(12.277408477694,-0.434551848133338,12.));
#49664=CARTESIAN_POINT('Ctrl Pts',(12.2767931065317,-0.42039064034991,12.));
#49665=CARTESIAN_POINT('Ctrl Pts',(12.2761719502385,-0.406096302442059,
12.));
#49666=CARTESIAN_POINT('Ctrl Pts',(12.2756638189297,-0.391797511344244,
12.));
#49667=CARTESIAN_POINT('Ctrl Pts',(12.2752682723578,-0.377498729044968,
12.));
#49668=CARTESIAN_POINT('Ctrl Pts',(12.2726875200461,-0.28420600930709,12.));
#49669=CARTESIAN_POINT('Ctrl Pts',(12.2748931639065,-0.190870392884388,
12.));
#49670=CARTESIAN_POINT('Ctrl Pts',(12.2817566653744,-0.0978690578159151,
12.));
#49671=CARTESIAN_POINT('Ctrl Pts',(12.2886243750566,-0.004810700899435,
12.));
#49672=CARTESIAN_POINT('Ctrl Pts',(12.3001560328895,0.0879139420894839,
12.));
#49673=CARTESIAN_POINT('Ctrl Pts',(12.3162734180046,0.179914286846824,12.));
#49674=CARTESIAN_POINT('Ctrl Pts',(12.3321476400437,0.270526621907842,12.));
#49675=CARTESIAN_POINT('Ctrl Pts',(12.3524707190227,0.360437184721369,12.));
#49676=CARTESIAN_POINT('Ctrl Pts',(12.3772105840448,0.449247114668589,12.));
#49677=CARTESIAN_POINT('Ctrl Pts',(12.387089561874,0.484710175124557,12.));
#49678=CARTESIAN_POINT('Ctrl Pts',(12.3976732487818,0.519997379566271,12.));
#49679=CARTESIAN_POINT('Ctrl Pts',(12.4089613041164,0.555081714039806,12.));
#49680=CARTESIAN_POINT('Ctrl Pts',(12.4149082466012,0.573565368933964,12.));
#49681=CARTESIAN_POINT('Ctrl Pts',(12.4210507056737,0.591992698996559,12.));
#49682=CARTESIAN_POINT('Ctrl Pts',(12.427388732547,0.610359631690939,12.));
#49683=CARTESIAN_POINT('Ctrl Pts',(12.4327450955641,0.62588180617673,12.));
#49684=CARTESIAN_POINT('Ctrl Pts',(12.4382385696775,0.641353302839583,12.));
#49685=CARTESIAN_POINT('Ctrl Pts',(12.4438669442654,0.656766888688516,12.));
#49686=CARTESIAN_POINT('Ctrl Pts',(12.4746822935363,0.741156266835812,12.));
#49687=CARTESIAN_POINT('Ctrl Pts',(12.5095548332415,0.823860554446091,12.));
#49688=CARTESIAN_POINT('Ctrl Pts',(12.5484325218527,0.904509504080283,12.));
#49689=CARTESIAN_POINT('Ctrl Pts',(12.5775387438767,0.964888253895875,12.));
#49690=CARTESIAN_POINT('Ctrl Pts',(12.6088907149234,1.02411455960934,12.));
#49691=CARTESIAN_POINT('Ctrl Pts',(12.6424801735134,1.08201977519688,12.));
#49692=CARTESIAN_POINT('Ctrl Pts',(12.6553986892758,1.10429013833142,12.));
#49693=CARTESIAN_POINT('Ctrl Pts',(12.6686482828058,1.12636495172308,12.));
#49694=CARTESIAN_POINT('Ctrl Pts',(12.6822288987083,1.1482340709878,12.));
#49695=CARTESIAN_POINT('Ctrl Pts',(12.6939913183076,1.16717531480961,12.));
#49696=CARTESIAN_POINT('Ctrl Pts',(12.706004041963,1.18596501264398,12.));
#49697=CARTESIAN_POINT('Ctrl Pts',(12.7182527989854,1.20457528100954,12.));
#49698=CARTESIAN_POINT('Ctrl Pts',(12.765524404259,1.27639785521913,12.));
#49699=CARTESIAN_POINT('Ctrl Pts',(12.8163473248132,1.34561526270953,12.));
#49700=CARTESIAN_POINT('Ctrl Pts',(12.8706925767079,1.41187353983322,12.));
#49701=CARTESIAN_POINT('Ctrl Pts',(12.9128273378038,1.46324466389474,12.));
#49702=CARTESIAN_POINT('Ctrl Pts',(12.9570801591186,1.51283644006015,12.));
#49703=CARTESIAN_POINT('Ctrl Pts',(13.0034499581199,1.56046614478315,12.));
#49704=CARTESIAN_POINT('Ctrl Pts',(13.0293158880168,1.58703487335031,12.));
#49705=CARTESIAN_POINT('Ctrl Pts',(13.0558407610521,1.61299275362867,12.));
#49706=CARTESIAN_POINT('Ctrl Pts',(13.0829974340784,1.63832794503775,12.));
#49707=CARTESIAN_POINT('Origin',(15.,0.,7.5));
#49708=CARTESIAN_POINT('Origin',(-7.5,12.9903810567666,4.));
#49709=CARTESIAN_POINT('Ctrl Pts',(-9.41346599666504,14.6263682601415,4.));
#49710=CARTESIAN_POINT('Ctrl Pts',(-9.47563132777586,14.5679481137415,4.));
#49711=CARTESIAN_POINT('Ctrl Pts',(-9.53442555802215,14.506276247837,4.));
#49712=CARTESIAN_POINT('Ctrl Pts',(-9.58983471826803,14.4417285757633,4.));
#49713=CARTESIAN_POINT('Ctrl Pts',(-9.64659435921208,14.3756076911582,4.));
#49714=CARTESIAN_POINT('Ctrl Pts',(-9.69980238305237,14.3064686172689,4.));
#49715=CARTESIAN_POINT('Ctrl Pts',(-9.7494149473681,14.2346691598829,4.));
#49716=CARTESIAN_POINT('Ctrl Pts',(-9.76242041292079,14.2158476096845,4.));
#49717=CARTESIAN_POINT('Ctrl Pts',(-9.77517863474719,14.1968430256296,4.));
#49718=CARTESIAN_POINT('Ctrl Pts',(-9.78768844229491,14.177661413676,4.));
#49719=CARTESIAN_POINT('Ctrl Pts',(-9.79776816908292,14.1622059074975,4.));
#49720=CARTESIAN_POINT('Ctrl Pts',(-9.80768698071961,14.1466346904616,4.));
#49721=CARTESIAN_POINT('Ctrl Pts',(-9.81743563533852,14.1309651390747,4.));
#49722=CARTESIAN_POINT('Ctrl Pts',(-9.86491280549081,14.0546524593777,4.));
#49723=CARTESIAN_POINT('Ctrl Pts',(-9.90840772399799,13.9759343990068,4.));
#49724=CARTESIAN_POINT('Ctrl Pts',(-9.94788354450479,13.8952025688597,4.));
#49725=CARTESIAN_POINT('Ctrl Pts',(-9.97942538424941,13.8306964885275,4.));
#49726=CARTESIAN_POINT('Ctrl Pts',(-10.0084008056984,13.7649036744675,4.));
#49727=CARTESIAN_POINT('Ctrl Pts',(-10.0347744493784,13.6980066802042,4.));
#49728=CARTESIAN_POINT('Ctrl Pts',(-10.0434535064654,13.6759921705975,4.));
#49729=CARTESIAN_POINT('Ctrl Pts',(-10.0518506786378,13.6538579807081,4.));
#49730=CARTESIAN_POINT('Ctrl Pts',(-10.0599643178554,13.6316103344208,4.));
#49731=CARTESIAN_POINT('Ctrl Pts',(-10.0673321856527,13.6114075977388,4.));
#49732=CARTESIAN_POINT('Ctrl Pts',(-10.0744676826305,13.591106675655,4.));
#49733=CARTESIAN_POINT('Ctrl Pts',(-10.0813601244641,13.5707407736482,4.));
#49734=CARTESIAN_POINT('Ctrl Pts',(-10.110937889366,13.4833439009404,4.));
#49735=CARTESIAN_POINT('Ctrl Pts',(-10.1360768470728,13.3946653712955,4.));
#49736=CARTESIAN_POINT('Ctrl Pts',(-10.1567422986514,13.3051020151044,4.));
#49737=CARTESIAN_POINT('Ctrl Pts',(-10.1777244132853,13.2141662521254,4.));
#49738=CARTESIAN_POINT('Ctrl Pts',(-10.194095376586,13.1223175335281,4.));
#49739=CARTESIAN_POINT('Ctrl Pts',(-10.205777094777,13.0299380601523,4.));
#49740=CARTESIAN_POINT('Ctrl Pts',(-10.2173678863481,12.938277637958,4.));
#49741=CARTESIAN_POINT('Ctrl Pts',(-10.2243424959595,12.8460937642312,4.));
#49742=CARTESIAN_POINT('Ctrl Pts',(-10.2265776894176,12.7537405691803,4.));
#49743=CARTESIAN_POINT('Ctrl Pts',(-10.2276571919675,12.7091379379498,4.));
#49744=CARTESIAN_POINT('Ctrl Pts',(-10.2276305022847,12.6644956114825,4.));
#49745=CARTESIAN_POINT('Ctrl Pts',(-10.226479393828,12.619852841063,4.));
#49746=CARTESIAN_POINT('Ctrl Pts',(-10.2261091350259,12.6054933090796,4.));
#49747=CARTESIAN_POINT('Ctrl Pts',(-10.2256225193086,12.5911337303501,4.));
#49748=CARTESIAN_POINT('Ctrl Pts',(-10.225018873735,12.5767754108853,4.));
#49749=CARTESIAN_POINT('Ctrl Pts',(-10.2243878291515,12.5617653783061,4.));
#49750=CARTESIAN_POINT('Ctrl Pts',(-10.2236292144324,12.5467651944381,4.));
#49751=CARTESIAN_POINT('Ctrl Pts',(-10.2227430773117,12.5317818464922,4.));
#49752=CARTESIAN_POINT('Ctrl Pts',(-10.21709364836,12.436257849471,4.));
#49753=CARTESIAN_POINT('Ctrl Pts',(-10.2062620470353,12.3413497626712,4.));
#49754=CARTESIAN_POINT('Ctrl Pts',(-10.1901757223778,12.2474518873064,4.));
#49755=CARTESIAN_POINT('Ctrl Pts',(-10.1886872627285,12.2387635634276,4.));
#49756=CARTESIAN_POINT('Ctrl Pts',(-10.1871537792193,12.2300838755081,4.));
#49757=CARTESIAN_POINT('Ctrl Pts',(-10.1855751929644,12.2214131286805,4.));
#49758=CARTESIAN_POINT('Ctrl Pts',(-10.1691864185716,12.1313940289104,4.));
#49759=CARTESIAN_POINT('Ctrl Pts',(-10.1479406949308,12.0423388878924,4.));
#49760=CARTESIAN_POINT('Ctrl Pts',(-10.1221403086027,11.9544825435439,4.));
#49761=CARTESIAN_POINT('Ctrl Pts',(-10.095748827746,11.8646133842016,4.));
#49762=CARTESIAN_POINT('Ctrl Pts',(-10.0645913960745,11.7759978814463,4.));
#49763=CARTESIAN_POINT('Ctrl Pts',(-10.0289372513566,11.6888902934565,4.));
#49764=CARTESIAN_POINT('Ctrl Pts',(-10.0090455594271,11.6402923725491,4.));
#49765=CARTESIAN_POINT('Ctrl Pts',(-9.98775327367975,11.5921639163278,4.));
#49766=CARTESIAN_POINT('Ctrl Pts',(-9.96510045219232,11.5445507349067,4.));
#49767=CARTESIAN_POINT('Ctrl Pts',(-9.95876521331174,11.5312349155799,4.));
#49768=CARTESIAN_POINT('Ctrl Pts',(-9.95232326498233,11.517959024353,4.));
#49769=CARTESIAN_POINT('Ctrl Pts',(-9.94578250287666,11.504737914807,4.));
#49770=CARTESIAN_POINT('Ctrl Pts',(-9.90302508933715,11.4183106087567,4.));
#49771=CARTESIAN_POINT('Ctrl Pts',(-9.85598190542476,11.3340799660434,4.));
#49772=CARTESIAN_POINT('Ctrl Pts',(-9.80499298346813,11.2522993127725,4.));
#49773=CARTESIAN_POINT('Ctrl Pts',(-9.75299886407878,11.1689064327755,4.));
#49774=CARTESIAN_POINT('Ctrl Pts',(-9.69690158938222,11.0880603146916,4.));
#49775=CARTESIAN_POINT('Ctrl Pts',(-9.63700679973682,11.0100365149775,4.));
#49776=CARTESIAN_POINT('Ctrl Pts',(-9.57664072131881,10.9313987763712,4.));
#49777=CARTESIAN_POINT('Ctrl Pts',(-9.5124166745289,10.855627103721,4.00000000000001));
#49778=CARTESIAN_POINT('Ctrl Pts',(-9.44459833298039,10.7830228983692,4.00000000000001));
#49779=CARTESIAN_POINT('Ctrl Pts',(-9.40866399637306,10.7445527161936,4.00000000000001));
#49780=CARTESIAN_POINT('Ctrl Pts',(-9.37171976510391,10.706972211061,4.));
#49781=CARTESIAN_POINT('Ctrl Pts',(-9.33380001260192,10.67032964942,4.));
#49782=CARTESIAN_POINT('Ctrl Pts',(-9.31851279266197,10.655557324655,4.));
#49783=CARTESIAN_POINT('Ctrl Pts',(-9.30306698875868,10.6409374727743,4.00000000000001));
#49784=CARTESIAN_POINT('Ctrl Pts',(-9.28746471547238,10.6264733925429,4.00000000000001));
#49785=CARTESIAN_POINT('Ctrl Pts',(-9.27676484992977,10.616554087142,4.00000000000001));
#49786=CARTESIAN_POINT('Ctrl Pts',(-9.265998221379,10.6067143856922,4.00000000000001));
#49787=CARTESIAN_POINT('Ctrl Pts',(-9.25516722641356,10.5969563651344,4.00000000000001));
#49788=CARTESIAN_POINT('Ctrl Pts',(-9.17938034347013,10.5286773229844,4.));
#49789=CARTESIAN_POINT('Ctrl Pts',(-9.10042408605055,10.4643755397515,4.));
#49790=CARTESIAN_POINT('Ctrl Pts',(-9.01862125042457,10.4043372079866,4.));
#49791=CARTESIAN_POINT('Ctrl Pts',(-8.9367488325877,10.344247807089,4.));
#49792=CARTESIAN_POINT('Ctrl Pts',(-8.85202442117708,10.2884282704825,4.));
#49793=CARTESIAN_POINT('Ctrl Pts',(-8.76472673601652,10.2371917535793,4.00000000000001));
#49794=CARTESIAN_POINT('Ctrl Pts',(-8.67911981959232,10.1869475780055,4.00000000000001));
#49795=CARTESIAN_POINT('Ctrl Pts',(-8.59103768625539,10.1411099279233,4.));
#49796=CARTESIAN_POINT('Ctrl Pts',(-8.50070929346997,10.1000104724858,4.));
#49797=CARTESIAN_POINT('Ctrl Pts',(-8.47449841652962,10.0880845128227,4.));
#49798=CARTESIAN_POINT('Ctrl Pts',(-8.4480982164028,10.0765577851635,4.));
#49799=CARTESIAN_POINT('Ctrl Pts',(-8.42151385798486,10.0654391093543,4.));
#49800=CARTESIAN_POINT('Ctrl Pts',(-8.38003010456224,10.0480888916659,4.));
#49801=CARTESIAN_POINT('Ctrl Pts',(-8.33809795636191,10.0317321930114,4.));
#49802=CARTESIAN_POINT('Ctrl Pts',(-8.29574920379127,10.0163624306404,4.));
#49803=CARTESIAN_POINT('Ctrl Pts',(-6.70620071746715,10.0211581030209,4.));
#49804=CARTESIAN_POINT('Ctrl Pts',(-6.61134536198573,10.0558566157721,4.));
#49805=CARTESIAN_POINT('Ctrl Pts',(-6.51853047906358,10.0955386450798,4.));
#49806=CARTESIAN_POINT('Ctrl Pts',(-6.42799833026157,10.1398859077314,4.));
#49807=CARTESIAN_POINT('Ctrl Pts',(-6.33621672682966,10.1848452169695,4.));
#49808=CARTESIAN_POINT('Ctrl Pts',(-6.24678063208038,10.2346001195317,4.));
#49809=CARTESIAN_POINT('Ctrl Pts',(-6.15997649545542,10.288859611306,4.));
#49810=CARTESIAN_POINT('Ctrl Pts',(-6.13531542249315,10.3042747440124,4.));
#49811=CARTESIAN_POINT('Ctrl Pts',(-6.11086702515844,10.3200536672633,4.));
#49812=CARTESIAN_POINT('Ctrl Pts',(-6.0866384800126,10.3361901726906,4.));
#49813=CARTESIAN_POINT('Ctrl Pts',(-6.06744058816026,10.3489762019054,4.));
#49814=CARTESIAN_POINT('Ctrl Pts',(-6.04837875428141,10.3619882719582,4.));
#49815=CARTESIAN_POINT('Ctrl Pts',(-6.0294755109822,10.37520976247,4.));
#49816=CARTESIAN_POINT('Ctrl Pts',(-5.9467711696009,10.43305563831,4.));
#49817=CARTESIAN_POINT('Ctrl Pts',(-5.86702033335456,10.4949586291912,4.));
#49818=CARTESIAN_POINT('Ctrl Pts',(-5.79049045427403,10.5606238082624,4.));
#49819=CARTESIAN_POINT('Ctrl Pts',(-5.73202499106291,10.6107891183003,4.));
#49820=CARTESIAN_POINT('Ctrl Pts',(-5.67544001899664,10.6631510546145,4.));
#49821=CARTESIAN_POINT('Ctrl Pts',(-5.62087181378523,10.7175895430331,4.));
#49822=CARTESIAN_POINT('Ctrl Pts',(-5.59237441395403,10.7460192002787,4.));
#49823=CARTESIAN_POINT('Ctrl Pts',(-5.56442730562685,10.7750153331146,4.));
#49824=CARTESIAN_POINT('Ctrl Pts',(-5.53705172637329,10.8045615976092,4.));
#49825=CARTESIAN_POINT('Ctrl Pts',(-5.52590399611565,10.8165932621689,4.));
#49826=CARTESIAN_POINT('Ctrl Pts',(-5.51485083286264,10.828716515658,4.));
#49827=CARTESIAN_POINT('Ctrl Pts',(-5.50390377375039,10.8409187451704,4.));
#49828=CARTESIAN_POINT('Ctrl Pts',(-5.43813900242605,10.9142239886428,4.));
#49829=CARTESIAN_POINT('Ctrl Pts',(-5.37610793089156,10.9904753850308,4.));
#49830=CARTESIAN_POINT('Ctrl Pts',(-5.31805547404601,11.0693968127291,4.));
#49831=CARTESIAN_POINT('Ctrl Pts',(-5.26107067938322,11.14686677001,4.));
#49832=CARTESIAN_POINT('Ctrl Pts',(-5.20791915062963,11.2269102402285,4.));
#49833=CARTESIAN_POINT('Ctrl Pts',(-5.15887680160751,11.3092877421736,4.));
#49834=CARTESIAN_POINT('Ctrl Pts',(-5.11076852001942,11.390096270703,4.));
#49835=CARTESIAN_POINT('Ctrl Pts',(-5.0666140967032,11.4731514387505,4.));
#49836=CARTESIAN_POINT('Ctrl Pts',(-5.0267215928916,11.558237595229,4.));
#49837=CARTESIAN_POINT('Ctrl Pts',(-5.00642757575884,11.6015224169963,4.));
#49838=CARTESIAN_POINT('Ctrl Pts',(-4.98723731004213,11.6453329516309,4.));
#49839=CARTESIAN_POINT('Ctrl Pts',(-4.96919657902753,11.6896410472644,4.));
#49840=CARTESIAN_POINT('Ctrl Pts',(-4.96034359773442,11.7113839988919,4.));
#49841=CARTESIAN_POINT('Ctrl Pts',(-4.95176748954608,11.7332467663051,4.));
#49842=CARTESIAN_POINT('Ctrl Pts',(-4.94347399674913,11.7552260059165,4.));
#49843=CARTESIAN_POINT('Ctrl Pts',(-4.93874124380541,11.7677686479032,4.));
#49844=CARTESIAN_POINT('Ctrl Pts',(-4.93410183231377,11.780345881655,4.));
#49845=CARTESIAN_POINT('Ctrl Pts',(-4.92955939125163,11.7929492290495,4.));
#49846=CARTESIAN_POINT('Ctrl Pts',(-4.89805310423436,11.8803658129868,4.));
#49847=CARTESIAN_POINT('Ctrl Pts',(-4.87116553516298,11.9691490179121,4.));
#49848=CARTESIAN_POINT('Ctrl Pts',(-4.84914983533523,12.059077444786,4.));
#49849=CARTESIAN_POINT('Ctrl Pts',(-4.84589756836606,12.0723621123006,4.));
#49850=CARTESIAN_POINT('Ctrl Pts',(-4.84275170968814,12.0856717889067,4.));
#49851=CARTESIAN_POINT('Ctrl Pts',(-4.83971317200452,12.0990057760668,4.));
#49852=CARTESIAN_POINT('Ctrl Pts',(-4.81880138299547,12.1907727887468,4.));
#49853=CARTESIAN_POINT('Ctrl Pts',(-4.80296850182884,12.2836914928978,4.));
#49854=CARTESIAN_POINT('Ctrl Pts',(-4.792106149773,12.377370023065,4.));
#49855=CARTESIAN_POINT('Ctrl Pts',(-4.78082380016171,12.4746706742486,4.));
#49856=CARTESIAN_POINT('Ctrl Pts',(-4.77490383217972,12.5727922441963,4.));
#49857=CARTESIAN_POINT('Ctrl Pts',(-4.77428144864228,12.6712822681824,4.));
#49858=CARTESIAN_POINT('Ctrl Pts',(-4.77410039443767,12.6999334645636,4.));
#49859=CARTESIAN_POINT('Ctrl Pts',(-4.77436800145517,12.72861569198,4.));
#49860=CARTESIAN_POINT('Ctrl Pts',(-4.77508351480076,12.7573173782009,4.));
#49861=CARTESIAN_POINT('Ctrl Pts',(-4.77547910205812,12.7731857353794,4.));
#49862=CARTESIAN_POINT('Ctrl Pts',(-4.77601160613275,12.7890600363428,4.));
#49863=CARTESIAN_POINT('Ctrl Pts',(-4.77668094646708,12.8049382921795,4.));
#49864=CARTESIAN_POINT('Ctrl Pts',(-4.77726157393708,12.8187120796562,4.));
#49865=CARTESIAN_POINT('Ctrl Pts',(-4.77794517105296,12.8324874411773,4.));
#49866=CARTESIAN_POINT('Ctrl Pts',(-4.77873077105928,12.846250960695,4.));
#49867=CARTESIAN_POINT('Ctrl Pts',(-4.7840331030193,12.9391465167459,4.));
#49868=CARTESIAN_POINT('Ctrl Pts',(-4.79398369008647,13.0316542436184,4.));
#49869=CARTESIAN_POINT('Ctrl Pts',(-4.80846381204201,13.1234011743035,4.));
#49870=CARTESIAN_POINT('Ctrl Pts',(-4.82290319752883,13.2148899962528,4.));
#49871=CARTESIAN_POINT('Ctrl Pts',(-4.84184707271793,13.3056232412176,4.));
#49872=CARTESIAN_POINT('Ctrl Pts',(-4.86522626081521,13.3952139858104,4.));
#49873=CARTESIAN_POINT('Ctrl Pts',(-4.88820180858057,13.4832579513734,4.));
#49874=CARTESIAN_POINT('Ctrl Pts',(-4.91546130118121,13.5701993091168,4.));
#49875=CARTESIAN_POINT('Ctrl Pts',(-4.94697947428434,13.6556416339958,4.));
#49876=CARTESIAN_POINT('Ctrl Pts',(-4.9623719301486,13.6973689006853,4.));
#49877=CARTESIAN_POINT('Ctrl Pts',(-4.97878066818245,13.7387381251278,4.));
#49878=CARTESIAN_POINT('Ctrl Pts',(-4.99620585058615,13.779699693788,4.));
#49879=CARTESIAN_POINT('Ctrl Pts',(-5.00196797407456,13.7932447810892,4.));
#49880=CARTESIAN_POINT('Ctrl Pts',(-5.00784125922211,13.8067452713773,4.));
#49881=CARTESIAN_POINT('Ctrl Pts',(-5.01382575727085,13.8201993070928,4.));
#49882=CARTESIAN_POINT('Ctrl Pts',(-5.01951346999181,13.8329861255467,4.));
#49883=CARTESIAN_POINT('Ctrl Pts',(-5.02529821878992,13.8457232464252,4.));
#49884=CARTESIAN_POINT('Ctrl Pts',(-5.03117811610162,13.8584059204054,4.));
#49885=CARTESIAN_POINT('Ctrl Pts',(-5.06862984407309,13.9391876127847,4.));
#49886=CARTESIAN_POINT('Ctrl Pts',(-5.10995846184345,14.0178080548726,4.));
#49887=CARTESIAN_POINT('Ctrl Pts',(-5.15509821873846,14.0939187469392,4.));
#49888=CARTESIAN_POINT('Ctrl Pts',(-5.19948177774165,14.1687544045606,4.));
#49889=CARTESIAN_POINT('Ctrl Pts',(-5.24755030145435,14.2411643668113,4.));
#49890=CARTESIAN_POINT('Ctrl Pts',(-5.299277628138,14.3107831411822,4.));
#49891=CARTESIAN_POINT('Ctrl Pts',(-5.34947359960038,14.37834089519,4.));
#49892=CARTESIAN_POINT('Ctrl Pts',(-5.40311538240653,14.4432707274223,4.));
#49893=CARTESIAN_POINT('Ctrl Pts',(-5.46020707398797,14.5051981890779,4.));
#49894=CARTESIAN_POINT('Ctrl Pts',(-5.47440626361873,14.5206000758857,4.));
#49895=CARTESIAN_POINT('Ctrl Pts',(-5.48881897228929,14.5358160294758,4.));
#49896=CARTESIAN_POINT('Ctrl Pts',(-5.50344549658044,14.5508398362218,4.));
#49897=CARTESIAN_POINT('Ctrl Pts',(-5.52930175835117,14.5773984001217,4.));
#49898=CARTESIAN_POINT('Ctrl Pts',(-5.55582619547196,14.603356583853,4.));
#49899=CARTESIAN_POINT('Ctrl Pts',(-5.58299280741585,14.6287008947316,4.));
#49900=CARTESIAN_POINT('Origin',(-7.5,12.9903810567666,14.2084234471775));
#49901=CARTESIAN_POINT('Ctrl Pts',(-10.5771718362758,12.9919049495641,11.7084234471775));
#49902=CARTESIAN_POINT('Ctrl Pts',(-10.5778105116372,13.0907937922778,11.7032843782051));
#49903=CARTESIAN_POINT('Ctrl Pts',(-10.5289894981275,14.1961054493059,11.6458119334487));
#49904=CARTESIAN_POINT('Ctrl Pts',(-9.19520332408216,16.188335839362,11.5360061129082));
#49905=CARTESIAN_POINT('Ctrl Pts',(-5.76804722455709,16.1681372027015,11.3790059855559));
#49906=CARTESIAN_POINT('Ctrl Pts',(-3.89395310615829,13.2989500353867,11.2220058582037));
#49907=CARTESIAN_POINT('Ctrl Pts',(-5.25343413560966,10.1527921984098,11.0650057308514));
#49908=CARTESIAN_POINT('Ctrl Pts',(-8.62743319586002,9.55126751773617,10.9080056034992));
#49909=CARTESIAN_POINT('Ctrl Pts',(-10.416413733365,11.4305453719444,10.7891448422745));
#49910=CARTESIAN_POINT('Ctrl Pts',(-10.5747253393417,12.713490324996,10.7226174568339));
#49911=CARTESIAN_POINT('Ctrl Pts',(-10.5724150045772,12.9877735244422,10.7084234471775));
#49912=CARTESIAN_POINT('Ctrl Pts',(-10.5702206634037,12.9870745539208,11.7915765528226));
#49913=CARTESIAN_POINT('Ctrl Pts',(-10.5655505963514,13.6681072977096,11.7563842836469));
#49914=CARTESIAN_POINT('Ctrl Pts',(-10.0102057878341,15.3711021382601,11.6688586386871));
#49915=CARTESIAN_POINT('Ctrl Pts',(-7.21365218567195,16.5973810760335,11.5289996179432));
#49916=CARTESIAN_POINT('Ctrl Pts',(-4.33342713054201,14.7428462583649,11.371999490591));
#49917=CARTESIAN_POINT('Ctrl Pts',(-4.29152522806557,11.3151739482887,11.2149993632387));
#49918=CARTESIAN_POINT('Ctrl Pts',(-7.12729264284838,9.39053585671186,11.0579992358865));
#49919=CARTESIAN_POINT('Ctrl Pts',(-9.97678331927841,10.5618592714599,10.9168582990811));
#49920=CARTESIAN_POINT('Ctrl Pts',(-10.5660598502819,12.2874997426315,10.8280507380598));
#49921=CARTESIAN_POINT('Ctrl Pts',(-10.5715490487462,12.9928368154298,10.7915765528225));
#49922=CARTESIAN_POINT('Ctrl Pts',(-5.58653400333492,14.6263682601415,12.));
#49923=CARTESIAN_POINT('Ctrl Pts',(-5.04858820392146,13.9971818012847,11.9476666242159));
#49924=CARTESIAN_POINT('Ctrl Pts',(-4.6501298356162,12.1775391083675,11.8429998726477));
#49925=CARTESIAN_POINT('Ctrl Pts',(-6.60905434274384,10.1611067275626,11.6859997452955));
#49926=CARTESIAN_POINT('Ctrl Pts',(-9.36683572422696,10.6884384302024,11.5289996179432));
#49927=CARTESIAN_POINT('Ctrl Pts',(-10.4505967777648,13.2766298839747,11.371999490591));
#49928=CARTESIAN_POINT('Ctrl Pts',(-8.88853891927017,15.609821813293,11.2149993632387));
#49929=CARTESIAN_POINT('Ctrl Pts',(-6.0813596511542,15.5932771353061,11.0579992358865));
#49930=CARTESIAN_POINT('Ctrl Pts',(-4.5462915063457,13.2431295206274,10.9009991085342));
#49931=CARTESIAN_POINT('Ctrl Pts',(-5.65984071462414,10.666115577374,10.743998981182));
#49932=CARTESIAN_POINT('Ctrl Pts',(-8.42347911845702,10.1734074649302,10.5869988538297));
#49933=CARTESIAN_POINT('Ctrl Pts',(-10.3590245740303,12.2066479805288,10.4299987264775));
#49934=CARTESIAN_POINT('Ctrl Pts',(-9.73085545152254,14.9426994258741,10.2729985991252));
#49935=CARTESIAN_POINT('Ctrl Pts',(-7.10225674886102,15.9280729453192,10.115998471773));
#49936=CARTESIAN_POINT('Ctrl Pts',(-4.8303182837872,14.2791977933351,9.9589983444207));
#49937=CARTESIAN_POINT('Ctrl Pts',(-4.95230900060974,11.4746243081013,9.80199821706846));
#49938=CARTESIAN_POINT('Ctrl Pts',(-7.35883869070172,10.0292464861065,9.64499808971619));
#49939=CARTESIAN_POINT('Ctrl Pts',(-9.89194907460283,11.2391453960705,9.48799796236395));
#49940=CARTESIAN_POINT('Ctrl Pts',(-10.2801757792987,14.0193946579201,9.33099783501168));
#49941=CARTESIAN_POINT('Ctrl Pts',(-8.17539218920641,15.8769172785782,9.17399770765945));
#49942=CARTESIAN_POINT('Ctrl Pts',(-5.46497794449781,15.1460553165716,9.01699758030717));
#49943=CARTESIAN_POINT('Ctrl Pts',(-4.57938749963505,12.4821794938336,8.85999745295494));
#49944=CARTESIAN_POINT('Ctrl Pts',(-6.31273830315983,10.2740129245224,8.70299732560267));
#49945=CARTESIAN_POINT('Ctrl Pts',(-9.11071806020523,10.501639700397,8.54599719825042));
#49946=CARTESIAN_POINT('Ctrl Pts',(-10.4643514801813,12.96094473598,8.38899707089817));
#49947=CARTESIAN_POINT('Ctrl Pts',(-9.15982248917363,15.4466455979041,8.23199694354592));
#49948=CARTESIAN_POINT('Ctrl Pts',(-6.36691474847379,15.7297904840163,8.07499681619367));
#49949=CARTESIAN_POINT('Ctrl Pts',(-4.59005542323444,13.5564806545976,7.91799668884141));
#49950=CARTESIAN_POINT('Ctrl Pts',(-5.42257131653894,10.8755438858135,7.76099656148916));
#49951=CARTESIAN_POINT('Ctrl Pts',(-8.11793744062105,10.0910018961859,7.6039964341369));
#49952=CARTESIAN_POINT('Ctrl Pts',(-10.2591931327486,11.9063610164495,7.44699630678465));
#49953=CARTESIAN_POINT('Ctrl Pts',(-9.92625387366264,14.6937713043528,7.2899961794324));
#49954=CARTESIAN_POINT('Ctrl Pts',(-7.41766948685395,15.953735219701,7.13299605208014));
#49955=CARTESIAN_POINT('Ctrl Pts',(-4.98291166647307,14.5564310201707,6.97599592472789));
#49956=CARTESIAN_POINT('Ctrl Pts',(-4.80525109196198,11.7548348097635,6.81899579737564));
#49957=CARTESIAN_POINT('Ctrl Pts',(-7.04399773638617,10.061164742401,6.66199567002339));
#49958=CARTESIAN_POINT('Ctrl Pts',(-9.69164594449512,10.9941511043189,6.50499554267113));
#49959=CARTESIAN_POINT('Ctrl Pts',(-10.3740242882686,13.7171759009976,6.34799541531889));
#49960=CARTESIAN_POINT('Ctrl Pts',(-8.47923732450549,15.7884770124268,6.19099528796661));
#49961=CARTESIAN_POINT('Ctrl Pts',(-5.70635916288519,15.3506981982192,6.03399516061438));
#49962=CARTESIAN_POINT('Ctrl Pts',(-4.54185534982472,12.7964012172524,5.87699503326211));
#49963=CARTESIAN_POINT('Ctrl Pts',(-6.02994939266268,10.4160461410637,5.71999490590986));
#49964=CARTESIAN_POINT('Ctrl Pts',(-8.83624963123305,10.3441251642037,5.56299477855761));
#49965=CARTESIAN_POINT('Ctrl Pts',(-10.4443264801503,12.6451208096654,5.40599465120535));
#49966=CARTESIAN_POINT('Ctrl Pts',(-9.41218877466708,15.2557271980297,5.24899452385311));
#49967=CARTESIAN_POINT('Ctrl Pts',(-6.66539017469168,15.834951382638,5.09199439650085));
#49968=CARTESIAN_POINT('Ctrl Pts',(-4.66696070971034,13.863470166724,4.9349942691486));
#49969=CARTESIAN_POINT('Ctrl Pts',(-5.20901029900842,11.1089874665202,4.77799414179634));
#49970=CARTESIAN_POINT('Ctrl Pts',(-7.8052841019297,10.0417525531808,4.62099401444409));
#49971=CARTESIAN_POINT('Ctrl Pts',(-10.128057595771,11.6182209055488,4.46399388709184));
#49972=CARTESIAN_POINT('Ctrl Pts',(-10.093735767433,14.4258233247707,4.30699375973958));
#49973=CARTESIAN_POINT('Ctrl Pts',(-7.73454710646218,15.9448696981551,4.14999363238733));
#49974=CARTESIAN_POINT('Ctrl Pts',(-5.16315153543426,14.8173229408266,3.99299350503507));
#49975=CARTESIAN_POINT('Ctrl Pts',(-4.69098902991507,12.045960940047,3.83599337768282));
#49976=CARTESIAN_POINT('Ctrl Pts',(-6.05008049550023,10.7720932116963,3.73132662611465));
#49977=CARTESIAN_POINT('Ctrl Pts',(-6.84980000202491,10.5582942547315,3.67899325033057));
#49978=CARTESIAN_POINT('Ctrl Pts',(-5.44566844965789,14.7468063779934,12.1070022498898));
#49979=CARTESIAN_POINT('Ctrl Pts',(-4.86812015246569,14.0713004658265,12.0546688741057));
#49980=CARTESIAN_POINT('Ctrl Pts',(-4.44032807310083,12.1176993038908,11.9500021225376));
#49981=CARTESIAN_POINT('Ctrl Pts',(-6.54346469885977,9.95282118939152,11.7930019951853));
#49982=CARTESIAN_POINT('Ctrl Pts',(-9.50426845016806,10.5189740011564,11.6360018678331));
#49983=CARTESIAN_POINT('Ctrl Pts',(-10.6678138328376,13.2977029522207,11.4790017404808));
#49984=CARTESIAN_POINT('Ctrl Pts',(-8.99076038754082,15.8026598219827,11.3220016131285));
#49985=CARTESIAN_POINT('Ctrl Pts',(-5.97692217562184,15.7848971577712,11.1650014857763));
#49986=CARTESIAN_POINT('Ctrl Pts',(-4.32884537294989,13.2617363588805,11.008001358424));
#49987=CARTESIAN_POINT('Ctrl Pts',(-5.52437185495265,10.4950077843859,10.8510012310718));
#49988=CARTESIAN_POINT('Ctrl Pts',(-8.49146381092469,9.96602748253219,10.6940011037195));
#49989=CARTESIAN_POINT('Ctrl Pts',(-10.5695002659417,12.1489511132149,10.5370009763673));
#49990=CARTESIAN_POINT('Ctrl Pts',(-9.89508658439861,15.0864252137885,10.380000849015));
#49991=CARTESIAN_POINT('Ctrl Pts',(-7.07297568330216,16.144339968164,10.2230007216628));
#49992=CARTESIAN_POINT('Ctrl Pts',(-4.63378163576147,14.3740779132334,10.0660005943105));
#49993=CARTESIAN_POINT('Ctrl Pts',(-4.76475306606344,11.3630373167398,9.90900046695826));
#49994=CARTESIAN_POINT('Ctrl Pts',(-7.34844667640581,9.81125365971957,9.75200033960601));
#49995=CARTESIAN_POINT('Ctrl Pts',(-10.068039598996,11.1102229164483,9.59500021225375));
#49996=CARTESIAN_POINT('Ctrl Pts',(-10.4848467800654,14.0951485887035,9.43800008490151));
#49997=CARTESIAN_POINT('Ctrl Pts',(-8.22511321630987,16.0894183231763,9.28099995754925));
#49998=CARTESIAN_POINT('Ctrl Pts',(-5.31516367599608,15.3047517599283,9.12399983019699));
#49999=CARTESIAN_POINT('Ctrl Pts',(-4.36437782731425,12.4447667074727,8.96699970284474));
#50000=CARTESIAN_POINT('Ctrl Pts',(-6.22533446291578,10.0740393155813,8.80999957549249));
#50001=CARTESIAN_POINT('Ctrl Pts',(-9.22929591409124,10.3184235210999,8.65299944814023));
#50002=CARTESIAN_POINT('Ctrl Pts',(-10.6825811290368,12.9587776927019,8.49599932078798));
#50003=CARTESIAN_POINT('Ctrl Pts',(-9.28201531326903,15.6274708987809,8.33899919343573));
#50004=CARTESIAN_POINT('Ctrl Pts',(-6.2834992701754,15.9314603471809,8.18199906608347));
#50005=CARTESIAN_POINT('Ctrl Pts',(-4.37583110219086,13.5981557789132,8.02499893873123));
#50006=CARTESIAN_POINT('Ctrl Pts',(-5.26963515659132,10.7198537875612,7.86799881137897));
#50007=CARTESIAN_POINT('Ctrl Pts',(-8.16342876362473,9.87755538002796,7.71099868402671));
#50008=CARTESIAN_POINT('Ctrl Pts',(-10.4623194328887,11.8265576212272,7.55399855667447));
#50009=CARTESIAN_POINT('Ctrl Pts',(-10.1048698490028,14.8191715000043,7.39699842932221));
#50010=CARTESIAN_POINT('Ctrl Pts',(-7.4116084785376,16.1718914480481,7.23999830196995));
#50011=CARTESIAN_POINT('Ctrl Pts',(-4.79760863920515,14.6717204977811,7.0829981746177));
#50012=CARTESIAN_POINT('Ctrl Pts',(-4.60686904722592,11.6638763571539,6.92599804726545));
#50013=CARTESIAN_POINT('Ctrl Pts',(-7.01042775842265,9.84552167443846,6.7689979199132));
#50014=CARTESIAN_POINT('Ctrl Pts',(-9.85299055159733,10.8471926331423,6.61199779256093));
#50015=CARTESIAN_POINT('Ctrl Pts',(-10.585604229252,13.770681089133,6.4549976652087));
#50016=CARTESIAN_POINT('Ctrl Pts',(-8.55132682499211,15.9944672608673,6.29799753785643));
#50017=CARTESIAN_POINT('Ctrl Pts',(-5.57431489867653,15.5244600427274,6.14099741050419));
#50018=CARTESIAN_POINT('Ctrl Pts',(-4.32408263542585,12.7821208080144,5.98399728315193));
#50019=CARTESIAN_POINT('Ctrl Pts',(-5.92172719634629,10.2265287344922,5.82699715579967));
#50020=CARTESIAN_POINT('Ctrl Pts',(-8.93462166631621,10.149313078634,5.66999702844742));
#50021=CARTESIAN_POINT('Ctrl Pts',(-10.6610819284076,12.61970343828,5.51299690109516));
#50022=CARTESIAN_POINT('Ctrl Pts',(-9.55296030180576,15.4224974667542,5.35599677374291));
#50023=CARTESIAN_POINT('Ctrl Pts',(-6.60394786249421,16.0443629816032,5.19899664639066));
#50024=CARTESIAN_POINT('Ctrl Pts',(-4.45839800260659,13.927745247179,5.04199651903841));
#50025=CARTESIAN_POINT('Ctrl Pts',(-5.04035220251703,10.9704830194925,4.88499639168615));
#50026=CARTESIAN_POINT('Ctrl Pts',(-7.82775850916875,9.82468039853088,4.7279962643339));
#50027=CARTESIAN_POINT('Ctrl Pts',(-10.3215299589949,11.5172052095439,4.57099613698165));
#50028=CARTESIAN_POINT('Ctrl Pts',(-10.2846814260484,14.53149772411,4.41399600962939));
#50029=CARTESIAN_POINT('Ctrl Pts',(-7.75181399705376,16.1623732644724,4.25699588227714));
#50030=CARTESIAN_POINT('Ctrl Pts',(-4.99111740815211,14.9518187617518,4.09999575492489));
#50031=CARTESIAN_POINT('Ctrl Pts',(-4.48419523986314,11.9764346130167,3.94299562757263));
#50032=CARTESIAN_POINT('Ctrl Pts',(-5.94334031085913,10.6087872809636,3.83832887600446));
#50033=CARTESIAN_POINT('Ctrl Pts',(-6.80193357383899,10.379248870828,3.78599550022038));
#50034=CARTESIAN_POINT('Ctrl Pts',(-5.30480289598085,14.8672444958453,12.2140044997796));
#50035=CARTESIAN_POINT('Ctrl Pts',(-4.68765210100993,14.1454191303684,12.1616711239955));
#50036=CARTESIAN_POINT('Ctrl Pts',(-4.23052631058544,12.0578594994142,12.0570043724274));
#50037=CARTESIAN_POINT('Ctrl Pts',(-6.47787505497571,9.74453565122039,11.9000042450751));
#50038=CARTESIAN_POINT('Ctrl Pts',(-9.64170117610916,10.3495095721105,11.7430041177229));
#50039=CARTESIAN_POINT('Ctrl Pts',(-10.8850308879103,13.3187760204667,11.5860039903706));
#50040=CARTESIAN_POINT('Ctrl Pts',(-9.09298185581149,15.9954978306723,11.4290038630184));
#50041=CARTESIAN_POINT('Ctrl Pts',(-5.87248470008946,15.9765171802363,11.2720037356661));
#50042=CARTESIAN_POINT('Ctrl Pts',(-4.11139923955409,13.2803431971336,11.1150036083138));
#50043=CARTESIAN_POINT('Ctrl Pts',(-5.38890299528115,10.3238999913978,10.9580034809616));
#50044=CARTESIAN_POINT('Ctrl Pts',(-8.55944850339236,9.75864750013418,10.8010033536093));
#50045=CARTESIAN_POINT('Ctrl Pts',(-10.7799759578531,12.091254245901,10.6440032262571));
#50046=CARTESIAN_POINT('Ctrl Pts',(-10.0593177172747,15.230151001703,10.4870030989048));
#50047=CARTESIAN_POINT('Ctrl Pts',(-7.04369461774331,16.3606069910088,10.3300029715526));
#50048=CARTESIAN_POINT('Ctrl Pts',(-4.43724498773573,14.4689580331317,10.1730028442003));
#50049=CARTESIAN_POINT('Ctrl Pts',(-4.57719713151714,11.2514503253782,10.0160027168481));
#50050=CARTESIAN_POINT('Ctrl Pts',(-7.33805466210989,9.59326083333269,9.85900258949581));
#50051=CARTESIAN_POINT('Ctrl Pts',(-10.2441301233891,10.9813004368261,9.70200246214358));
#50052=CARTESIAN_POINT('Ctrl Pts',(-10.689517780832,14.1709025194869,9.5450023347913));
#50053=CARTESIAN_POINT('Ctrl Pts',(-8.27483424341331,16.3019193677744,9.38800220743907));
#50054=CARTESIAN_POINT('Ctrl Pts',(-5.16534940749437,15.463448203285,9.2310020800868));
#50055=CARTESIAN_POINT('Ctrl Pts',(-4.14936815499344,12.4073539211118,9.07400195273456));
#50056=CARTESIAN_POINT('Ctrl Pts',(-6.13793062267174,9.87406570664018,8.9170018253823));
#50057=CARTESIAN_POINT('Ctrl Pts',(-9.34787376797726,10.1352073418028,8.76000169803005));
#50058=CARTESIAN_POINT('Ctrl Pts',(-10.9008107778922,12.9566106494239,8.6030015706778));
#50059=CARTESIAN_POINT('Ctrl Pts',(-9.40420813736444,15.8082961996578,8.44600144332554));
#50060=CARTESIAN_POINT('Ctrl Pts',(-6.20008379187702,16.1331302103455,8.28900131597328));
#50061=CARTESIAN_POINT('Ctrl Pts',(-4.16160678114728,13.6398309032289,8.13200118862104));
#50062=CARTESIAN_POINT('Ctrl Pts',(-5.1166989966437,10.564163689309,7.97500106126877));
#50063=CARTESIAN_POINT('Ctrl Pts',(-8.20892008662842,9.66410886387002,7.81800093391653));
#50064=CARTESIAN_POINT('Ctrl Pts',(-10.6654457330288,11.7467542260049,7.66100080656427));
#50065=CARTESIAN_POINT('Ctrl Pts',(-10.2834858243429,14.9445716956558,7.50400067921202));
#50066=CARTESIAN_POINT('Ctrl Pts',(-7.40554747022126,16.3900476763952,7.34700055185976));
#50067=CARTESIAN_POINT('Ctrl Pts',(-4.61230561193723,14.7870099753915,7.19000042450751));
#50068=CARTESIAN_POINT('Ctrl Pts',(-4.40848700248986,11.5729179045444,7.03300029715526));
#50069=CARTESIAN_POINT('Ctrl Pts',(-6.97685778045915,9.6298786064759,6.876000169803));
#50070=CARTESIAN_POINT('Ctrl Pts',(-10.0143351586995,10.7002341619658,6.71900004245076));
#50071=CARTESIAN_POINT('Ctrl Pts',(-10.7971841702354,13.8241862772684,6.5619999150985));
#50072=CARTESIAN_POINT('Ctrl Pts',(-8.62341632547871,16.2004575093079,6.40499978774625));
#50073=CARTESIAN_POINT('Ctrl Pts',(-5.44227063446788,15.6982218872355,6.24799966039399));
#50074=CARTESIAN_POINT('Ctrl Pts',(-4.10630992102698,12.7678403987764,6.09099953304174));
#50075=CARTESIAN_POINT('Ctrl Pts',(-5.81350500002991,10.0370113279208,5.93399940568948));
#50076=CARTESIAN_POINT('Ctrl Pts',(-9.03299370139936,9.95450099306433,5.77699927833723));
#50077=CARTESIAN_POINT('Ctrl Pts',(-10.877837376665,12.5942860668946,5.61999915098498));
#50078=CARTESIAN_POINT('Ctrl Pts',(-9.69373182894443,15.5892677354788,5.46299902363273));
#50079=CARTESIAN_POINT('Ctrl Pts',(-6.54250555029675,16.2537745805684,5.30599889628047));
#50080=CARTESIAN_POINT('Ctrl Pts',(-4.24983529550283,13.9920203276339,5.14899876892821));
#50081=CARTESIAN_POINT('Ctrl Pts',(-4.87169410602564,10.8319785724647,4.99199864157597));
#50082=CARTESIAN_POINT('Ctrl Pts',(-7.85023291640778,9.60760824388092,4.83499851422371));
#50083=CARTESIAN_POINT('Ctrl Pts',(-10.5150023222189,11.416189513539,4.67799838687146));
#50084=CARTESIAN_POINT('Ctrl Pts',(-10.4756270846638,14.6371721234493,4.52099825951921));
#50085=CARTESIAN_POINT('Ctrl Pts',(-7.76908088764536,16.3798768307898,4.36399813216695));
#50086=CARTESIAN_POINT('Ctrl Pts',(-4.81908328086994,15.086314582677,4.2069980048147));
#50087=CARTESIAN_POINT('Ctrl Pts',(-4.27740144981121,11.9069082859864,4.04999787746244));
#50088=CARTESIAN_POINT('Ctrl Pts',(-5.83660012621804,10.4454813502308,3.94533112589427));
#50089=CARTESIAN_POINT('Ctrl Pts',(-6.75406714565307,10.2002034869244,3.89299775011019));
#50090=CARTESIAN_POINT('Ctrl Pts',(-5.16393734230382,14.9876826136972,12.3210067496694));
#50091=CARTESIAN_POINT('Ctrl Pts',(-4.50718404955416,14.2195377949102,12.2686733738853));
#50092=CARTESIAN_POINT('Ctrl Pts',(-4.02072454807007,11.9980196949375,12.1640066223172));
#50093=CARTESIAN_POINT('Ctrl Pts',(-6.41228541109164,9.53625011304927,12.0070064949649));
#50094=CARTESIAN_POINT('Ctrl Pts',(-9.77913390205027,10.1800451430645,11.8500063676127));
#50095=CARTESIAN_POINT('Ctrl Pts',(-11.1022479429831,13.3398490887126,11.6930062402604));
#50096=CARTESIAN_POINT('Ctrl Pts',(-9.19520332408216,16.188335839362,11.5360061129082));
#50097=CARTESIAN_POINT('Ctrl Pts',(-5.76804722455709,16.1681372027015,11.3790059855559));
#50098=CARTESIAN_POINT('Ctrl Pts',(-3.89395310615829,13.2989500353867,11.2220058582037));
#50099=CARTESIAN_POINT('Ctrl Pts',(-5.25343413560966,10.1527921984098,11.0650057308514));
#50100=CARTESIAN_POINT('Ctrl Pts',(-8.62743319586002,9.55126751773617,10.9080056034992));
#50101=CARTESIAN_POINT('Ctrl Pts',(-10.9904516497645,12.0335573785871,10.7510054761469));
#50102=CARTESIAN_POINT('Ctrl Pts',(-10.2235488501508,15.3738767896174,10.5940053487946));
#50103=CARTESIAN_POINT('Ctrl Pts',(-7.01441355218445,16.5768740138536,10.4370052214424));
#50104=CARTESIAN_POINT('Ctrl Pts',(-4.24070833971001,14.56383815303,10.2800050940901));
#50105=CARTESIAN_POINT('Ctrl Pts',(-4.38964119697082,11.1398633340167,10.1230049667379));
#50106=CARTESIAN_POINT('Ctrl Pts',(-7.32766264781398,9.3752680069458,9.96600483938563));
#50107=CARTESIAN_POINT('Ctrl Pts',(-10.4202206477823,10.8523779572038,9.80900471203337));
#50108=CARTESIAN_POINT('Ctrl Pts',(-10.8941887815987,14.2466564502702,9.65200458468113));
#50109=CARTESIAN_POINT('Ctrl Pts',(-8.32455527051676,16.5144204123725,9.49500445732887));
#50110=CARTESIAN_POINT('Ctrl Pts',(-5.01553513899265,15.6221446466417,9.33800432997661));
#50111=CARTESIAN_POINT('Ctrl Pts',(-3.93435848267263,12.3699411347509,9.18100420262437));
#50112=CARTESIAN_POINT('Ctrl Pts',(-6.0505267824277,9.67409209769908,9.02400407527211));
#50113=CARTESIAN_POINT('Ctrl Pts',(-9.46645162186327,9.95199116250562,8.86700394791985));
#50114=CARTESIAN_POINT('Ctrl Pts',(-11.1190404267477,12.9544436061459,8.71000382056761));
#50115=CARTESIAN_POINT('Ctrl Pts',(-9.52640096145984,15.9891215005347,8.55300369321535));
#50116=CARTESIAN_POINT('Ctrl Pts',(-6.11666831357863,16.3348000735102,8.3960035658631));
#50117=CARTESIAN_POINT('Ctrl Pts',(-3.9473824601037,13.6815060275445,8.23900343851085));
#50118=CARTESIAN_POINT('Ctrl Pts',(-4.9637628366961,10.4084735910568,8.08200331115859));
#50119=CARTESIAN_POINT('Ctrl Pts',(-8.25441140963209,9.45066234771208,7.92500318380633));
#50120=CARTESIAN_POINT('Ctrl Pts',(-10.8685720331689,11.6669508307826,7.76800305645408));
#50121=CARTESIAN_POINT('Ctrl Pts',(-10.4621017996831,15.0699718913073,7.61100292910183));
#50122=CARTESIAN_POINT('Ctrl Pts',(-7.39948646190492,16.6082039047423,7.45400280174958));
#50123=CARTESIAN_POINT('Ctrl Pts',(-4.42700258466931,14.902299453002,7.29700267439732));
#50124=CARTESIAN_POINT('Ctrl Pts',(-4.21010495775379,11.4819594519348,7.14000254704507));
#50125=CARTESIAN_POINT('Ctrl Pts',(-6.94328780249567,9.41423553851335,6.98300241969282));
#50126=CARTESIAN_POINT('Ctrl Pts',(-10.1756797658017,10.5532756907892,6.82600229234056));
#50127=CARTESIAN_POINT('Ctrl Pts',(-11.0087641112188,13.8776914654038,6.66900216498831));
#50128=CARTESIAN_POINT('Ctrl Pts',(-8.69550582596531,16.4064477577484,6.51200203763606));
#50129=CARTESIAN_POINT('Ctrl Pts',(-5.31022637025923,15.8719837317436,6.3550019102838));
#50130=CARTESIAN_POINT('Ctrl Pts',(-3.88853720662811,12.7535599895385,6.19800178293155));
#50131=CARTESIAN_POINT('Ctrl Pts',(-5.70528280371351,9.84749392134933,6.04100165557929));
#50132=CARTESIAN_POINT('Ctrl Pts',(-9.13136573648253,9.75968890749465,5.88400152822705));
#50133=CARTESIAN_POINT('Ctrl Pts',(-11.0945928249223,12.5688686955092,5.72700140087479));
#50134=CARTESIAN_POINT('Ctrl Pts',(-9.83450335608313,15.7560380042034,5.57000127352253));
#50135=CARTESIAN_POINT('Ctrl Pts',(-6.48106323809927,16.4631861795336,5.41300114617029));
#50136=CARTESIAN_POINT('Ctrl Pts',(-4.04127258839909,14.0562954080889,5.25600101881802));
#50137=CARTESIAN_POINT('Ctrl Pts',(-4.70303600953422,10.693474125437,5.09900089146578));
#50138=CARTESIAN_POINT('Ctrl Pts',(-7.87270732364685,9.390536089231,4.94200076411351));
#50139=CARTESIAN_POINT('Ctrl Pts',(-10.7084746854428,11.3151738175341,4.78500063676127));
#50140=CARTESIAN_POINT('Ctrl Pts',(-10.6665727432792,14.7428465227886,4.62800050940901));
#50141=CARTESIAN_POINT('Ctrl Pts',(-7.78634777823694,16.5973803971072,4.47100038205676));
#50142=CARTESIAN_POINT('Ctrl Pts',(-4.64704915358778,15.2208104036021,4.31400025470451));
#50143=CARTESIAN_POINT('Ctrl Pts',(-4.07060765975928,11.8373819589561,4.15700012735225));
#50144=CARTESIAN_POINT('Ctrl Pts',(-5.72985994157694,10.2821754194981,4.05233337578409));
#50145=CARTESIAN_POINT('Ctrl Pts',(-6.70620071746715,10.0211581030209,4.));
#50146=CARTESIAN_POINT('Ctrl Pts',(-5.58653400333492,14.6263682601415,12.));
#50147=CARTESIAN_POINT('Ctrl Pts',(-5.52489667247578,14.5684443043264,12.));
#50148=CARTESIAN_POINT('Ctrl Pts',(-5.46662450511892,14.5073716307993,12.));
#50149=CARTESIAN_POINT('Ctrl Pts',(-5.41171706416437,14.4435345397783,12.));
#50150=CARTESIAN_POINT('Ctrl Pts',(-5.35535922399003,14.3780111697138,12.));
#50151=CARTESIAN_POINT('Ctrl Pts',(-5.30254577876706,14.3095749751578,12.));
#50152=CARTESIAN_POINT('Ctrl Pts',(-5.25330168675279,14.2385929714213,12.));
#50153=CARTESIAN_POINT('Ctrl Pts',(-5.20312907342738,14.1662725674732,12.));
#50154=CARTESIAN_POINT('Ctrl Pts',(-5.15666120991867,14.0913088475707,12.));
#50155=CARTESIAN_POINT('Ctrl Pts',(-5.1139575408143,14.0140482152174,12.));
#50156=CARTESIAN_POINT('Ctrl Pts',(-5.09461512222896,13.9790533887192,12.));
#50157=CARTESIAN_POINT('Ctrl Pts',(-5.07604545116087,13.9435868239722,12.));
#50158=CARTESIAN_POINT('Ctrl Pts',(-5.05825663128179,13.9076784991748,12.));
#50159=CARTESIAN_POINT('Ctrl Pts',(-5.04815176560046,13.887280923541,12.));
#50160=CARTESIAN_POINT('Ctrl Pts',(-5.03829889260597,13.8667407800149,12.));
#50161=CARTESIAN_POINT('Ctrl Pts',(-5.02869974914025,13.846063404379,12.));
#50162=CARTESIAN_POINT('Ctrl Pts',(-5.02048275827117,13.8283633035935,12.));
#50163=CARTESIAN_POINT('Ctrl Pts',(-5.0124495628302,13.8105575032607,12.));
#50164=CARTESIAN_POINT('Ctrl Pts',(-5.00461403680565,13.7926790499403,12.));
#50165=CARTESIAN_POINT('Ctrl Pts',(-4.96800796729637,13.7091543570335,12.));
#50166=CARTESIAN_POINT('Ctrl Pts',(-4.93566374876766,13.6239462866792,12.));
#50167=CARTESIAN_POINT('Ctrl Pts',(-4.90760852459924,13.5374526993157,12.));
#50168=CARTESIAN_POINT('Ctrl Pts',(-4.87909391214457,13.449542828816,12.));
#50169=CARTESIAN_POINT('Ctrl Pts',(-4.85500940725962,13.3603042433618,12.));
#50170=CARTESIAN_POINT('Ctrl Pts',(-4.83542253240114,13.2701175707646,12.));
#50171=CARTESIAN_POINT('Ctrl Pts',(-4.81671792757447,13.1839932613098,12.));
#50172=CARTESIAN_POINT('Ctrl Pts',(-4.80211484736484,13.0970034290495,12.));
#50173=CARTESIAN_POINT('Ctrl Pts',(-4.79171068325589,13.0094587764721,12.));
#50174=CARTESIAN_POINT('Ctrl Pts',(-4.78712088419529,12.9708384356209,12.));
#50175=CARTESIAN_POINT('Ctrl Pts',(-4.78334877386587,12.9321099201028,12.));
#50176=CARTESIAN_POINT('Ctrl Pts',(-4.78040530851934,12.893299212279,12.));
#50177=CARTESIAN_POINT('Ctrl Pts',(-4.77903296806464,12.8752043824944,12.));
#50178=CARTESIAN_POINT('Ctrl Pts',(-4.77784077628839,12.8570916824141,12.));
#50179=CARTESIAN_POINT('Ctrl Pts',(-4.77682996946529,12.8389637304098,12.));
#50180=CARTESIAN_POINT('Ctrl Pts',(-4.77585594563052,12.8214954497015,12.));
#50181=CARTESIAN_POINT('Ctrl Pts',(-4.7750503477527,12.8040101811658,12.));
#50182=CARTESIAN_POINT('Ctrl Pts',(-4.77441493543858,12.7865348449805,12.));
#50183=CARTESIAN_POINT('Ctrl Pts',(-4.77095144017316,12.6912805623749,12.));
#50184=CARTESIAN_POINT('Ctrl Pts',(-4.77253057533756,12.5961742600887,12.));
#50185=CARTESIAN_POINT('Ctrl Pts',(-4.77921451714525,12.501614579937,12.));
#50186=CARTESIAN_POINT('Ctrl Pts',(-4.78586350142022,12.4075494542275,12.));
#50187=CARTESIAN_POINT('Ctrl Pts',(-4.7975636844451,12.3140242926481,12.));
#50188=CARTESIAN_POINT('Ctrl Pts',(-4.81442425859455,12.2214137249389,12.));
#50189=CARTESIAN_POINT('Ctrl Pts',(-4.83092299201404,12.1307906503674,12.));
#50190=CARTESIAN_POINT('Ctrl Pts',(-4.85236265681916,12.0410424028911,12.));
#50191=CARTESIAN_POINT('Ctrl Pts',(-4.87846866601438,11.9524107169388,12.));
#50192=CARTESIAN_POINT('Ctrl Pts',(-4.89379308908251,11.9003832529699,12.));
#50193=CARTESIAN_POINT('Ctrl Pts',(-4.91072644984389,11.8487405476717,12.));
#50194=CARTESIAN_POINT('Ctrl Pts',(-4.92922132646561,11.7975326456,12.));
#50195=CARTESIAN_POINT('Ctrl Pts',(-4.93398223972469,11.7843508123318,12.));
#50196=CARTESIAN_POINT('Ctrl Pts',(-4.93884748217419,11.7711956209025,12.));
#50197=CARTESIAN_POINT('Ctrl Pts',(-4.94381359460063,11.7580750750315,12.));
#50198=CARTESIAN_POINT('Ctrl Pts',(-4.97686200318078,11.6707606682067,12.));
#50199=CARTESIAN_POINT('Ctrl Pts',(-5.01429316281797,11.5851876670551,12.));
#50200=CARTESIAN_POINT('Ctrl Pts',(-5.05577609967284,11.5015918684293,12.));
#50201=CARTESIAN_POINT('Ctrl Pts',(-5.09882544403038,11.414839468654,12.));
#50202=CARTESIAN_POINT('Ctrl Pts',(-5.14623844362019,11.330215691903,12.));
#50203=CARTESIAN_POINT('Ctrl Pts',(-5.19770129474244,11.2479859989681,12.));
#50204=CARTESIAN_POINT('Ctrl Pts',(-5.2497890294851,11.1647578384569,12.));
#50205=CARTESIAN_POINT('Ctrl Pts',(-5.30602595623937,11.0839814330439,12.));
#50206=CARTESIAN_POINT('Ctrl Pts',(-5.36613892032226,11.0059457826021,12.));
#50207=CARTESIAN_POINT('Ctrl Pts',(-5.4056128756235,10.9547026635106,12.));
#50208=CARTESIAN_POINT('Ctrl Pts',(-5.44675926231209,10.9046416780186,12.));
#50209=CARTESIAN_POINT('Ctrl Pts',(-5.48951145353165,10.8558504805206,12.));
#50210=CARTESIAN_POINT('Ctrl Pts',(-5.50097088386534,10.8427723361571,12.));
#50211=CARTESIAN_POINT('Ctrl Pts',(-5.5125457300662,10.8297854541688,12.));
#50212=CARTESIAN_POINT('Ctrl Pts',(-5.52423480193837,10.8168915966514,12.));
#50213=CARTESIAN_POINT('Ctrl Pts',(-5.53538763239833,10.8045892506277,12.));
#50214=CARTESIAN_POINT('Ctrl Pts',(-5.54663877351141,10.7923778862678,12.));
#50215=CARTESIAN_POINT('Ctrl Pts',(-5.55798379608792,10.7802620173577,12.));
#50216=CARTESIAN_POINT('Ctrl Pts',(-5.62980564817047,10.7035601739863,12.));
#50217=CARTESIAN_POINT('Ctrl Pts',(-5.70542329107336,10.630641847274,12.));
#50218=CARTESIAN_POINT('Ctrl Pts',(-5.78449319659024,10.5618401471187,12.));
#50219=CARTESIAN_POINT('Ctrl Pts',(-5.84379562572791,10.5102388720023,12.));
#50220=CARTESIAN_POINT('Ctrl Pts',(-5.90504126576837,10.4609534569649,12.));
#50221=CARTESIAN_POINT('Ctrl Pts',(-5.96810424452339,10.4141359861561,12.));
#50222=CARTESIAN_POINT('Ctrl Pts',(-5.99074689198795,10.39732625868,12.));
#50223=CARTESIAN_POINT('Ctrl Pts',(-6.01362396161954,10.3808348014861,12.));
#50224=CARTESIAN_POINT('Ctrl Pts',(-6.03673007192386,10.3646690702049,12.));
#50225=CARTESIAN_POINT('Ctrl Pts',(-6.05604446520068,10.351156138454,12.));
#50226=CARTESIAN_POINT('Ctrl Pts',(-6.07552143283976,10.3378692705033,12.));
#50227=CARTESIAN_POINT('Ctrl Pts',(-6.09513718668148,10.3248263089414,12.));
#50228=CARTESIAN_POINT('Ctrl Pts',(-6.18010809783264,10.2683272145418,12.));
#50229=CARTESIAN_POINT('Ctrl Pts',(-6.26775573276173,10.2163476819429,12.));
#50230=CARTESIAN_POINT('Ctrl Pts',(-6.35779277794461,10.1691997545039,12.));
#50231=CARTESIAN_POINT('Ctrl Pts',(-6.4298686728608,10.131457189133,12.));
#50232=CARTESIAN_POINT('Ctrl Pts',(-6.50347672461637,10.0968111469865,12.));
#50233=CARTESIAN_POINT('Ctrl Pts',(-6.57848633664494,10.0654390261441,12.));
#50234=CARTESIAN_POINT('Ctrl Pts',(-6.61998971216275,10.0480805986452,12.));
#50235=CARTESIAN_POINT('Ctrl Pts',(-6.6619224176942,10.0317247798523,12.));
#50236=CARTESIAN_POINT('Ctrl Pts',(-6.70425100699966,10.0163623331919,12.));
#50237=CARTESIAN_POINT('Ctrl Pts',(-10.0166112816083,12.988245230306,10.387416697508));
#50238=CARTESIAN_POINT('Ctrl Pts',(-10.0185036739199,12.7635802052187,10.4016107071645));
#50239=CARTESIAN_POINT('Ctrl Pts',(-9.99083720988162,12.539373330507,10.415804716821));
#50240=CARTESIAN_POINT('Ctrl Pts',(-9.93173881101679,12.3237831354866,10.4299987264775));
#50241=CARTESIAN_POINT('Ctrl Pts',(-9.71384275550587,11.5289011419959,10.4823321022615));
#50242=CARTESIAN_POINT('Ctrl Pts',(-9.06866093698144,10.8511543034631,10.5346654780456));
#50243=CARTESIAN_POINT('Ctrl Pts',(-8.28546362708042,10.5943989029373,10.5869988538297));
#50244=CARTESIAN_POINT('Ctrl Pts',(-7.50226631717939,10.3376435024115,10.6393322296138));
#50245=CARTESIAN_POINT('Ctrl Pts',(-6.58105351590176,10.5018795398927,10.6916656053979));
#50246=CARTESIAN_POINT('Ctrl Pts',(-5.93485558054988,11.0134998825089,10.743998981182));
#50247=CARTESIAN_POINT('Ctrl Pts',(-5.28865764519799,11.5251202251251,10.796332356966));
#50248=CARTESIAN_POINT('Ctrl Pts',(-4.91747457577184,12.3841248728762,10.8486657327501));
#50249=CARTESIAN_POINT('Ctrl Pts',(-4.98772773186019,13.2053184658649,10.9009991085342));
#50250=CARTESIAN_POINT('Ctrl Pts',(-5.05798088794854,14.0265120588536,10.9533324843183));
#50251=CARTESIAN_POINT('Ctrl Pts',(-5.56967026955137,14.8098945970798,11.0056658601024));
#50252=CARTESIAN_POINT('Ctrl Pts',(-6.29337817170545,15.2043433125241,11.0579992358865));
#50253=CARTESIAN_POINT('Ctrl Pts',(-7.01708607385953,15.5987920279684,11.1103326116706));
#50254=CARTESIAN_POINT('Ctrl Pts',(-7.95281249656485,15.6043069206307,11.1626659874546));
#50255=CARTESIAN_POINT('Ctrl Pts',(-8.68101868433327,15.2181990454088,11.2149993632387));
#50256=CARTESIAN_POINT('Ctrl Pts',(-9.4092248721017,14.8320911701869,11.2673327390228));
#50257=CARTESIAN_POINT('Ctrl Pts',(-9.92991082493323,14.0543605270808,11.3196661148069));
#50258=CARTESIAN_POINT('Ctrl Pts',(-10.0096269590927,13.2341299632324,11.371999490591));
#50259=CARTESIAN_POINT('Ctrl Pts',(-10.0174549790803,13.1535843959402,11.3771385595633));
#50260=CARTESIAN_POINT('Ctrl Pts',(-10.0210307346825,13.0726290026425,11.3822776285357));
#50261=CARTESIAN_POINT('Ctrl Pts',(-10.020507596494,12.9916292754481,11.387416697508));
#50262=CARTESIAN_POINT('Ctrl Pts',(-8.29379928253292,10.0211581030209,12.));
#50263=CARTESIAN_POINT('Ctrl Pts',(-9.27014005842312,10.2821754194981,11.9476666242159));
#50264=CARTESIAN_POINT('Ctrl Pts',(-10.9293920526294,11.8373837255142,11.8429998726477));
#50265=CARTESIAN_POINT('Ctrl Pts',(-10.3529510979028,15.2208095229378,11.6859997452955));
#50266=CARTESIAN_POINT('Ctrl Pts',(-7.21365218567195,16.5973810760335,11.5289996179432));
#50267=CARTESIAN_POINT('Ctrl Pts',(-4.33342713054201,14.7428462583649,11.371999490591));
#50268=CARTESIAN_POINT('Ctrl Pts',(-4.29152522806557,11.3151739482887,11.2149993632387));
#50269=CARTESIAN_POINT('Ctrl Pts',(-7.12729264284838,9.39053585671186,11.0579992358865));
#50270=CARTESIAN_POINT('Ctrl Pts',(-10.2969641018483,10.6934741072896,10.9009991085342));
#50271=CARTESIAN_POINT('Ctrl Pts',(-10.9587275214881,14.0562954105675,10.743998981182));
#50272=CARTESIAN_POINT('Ctrl Pts',(-8.5189368031419,16.4631863186891,10.5869988538297));
#50273=CARTESIAN_POINT('Ctrl Pts',(-5.16549655959477,15.7560380892136,10.4299987264775));
#50274=CARTESIAN_POINT('Ctrl Pts',(-3.90540705298465,12.5688686867556,10.2729985991252));
#50275=CARTESIAN_POINT('Ctrl Pts',(-5.86863420589283,9.75968879265402,10.115998471773));
#50276=CARTESIAN_POINT('Ctrl Pts',(-9.29471725902464,9.84749381445728,9.9589983444207));
#50277=CARTESIAN_POINT('Ctrl Pts',(-11.1114629177913,12.7535599804133,9.80199821706845));
#50278=CARTESIAN_POINT('Ctrl Pts',(-9.68977370564798,15.8719838318464,9.64499808971619));
#50279=CARTESIAN_POINT('Ctrl Pts',(-6.30449413259093,16.4064478755407,9.48799796236394));
#50280=CARTESIAN_POINT('Ctrl Pts',(-3.99123576757957,13.8776914962184,9.3309978350117));
#50281=CARTESIAN_POINT('Ctrl Pts',(-4.82432014168349,10.5532756064786,9.17399770765943));
#50282=CARTESIAN_POINT('Ctrl Pts',(-8.05671221676616,9.41423541495656,9.0169975803072));
#50283=CARTESIAN_POINT('Ctrl Pts',(-10.7898951559407,11.481959399778,8.85999745295492));
#50284=CARTESIAN_POINT('Ctrl Pts',(-10.572997521546,14.902299519094,8.70299732560269));
#50285=CARTESIAN_POINT('Ctrl Pts',(-7.60051354156566,16.6082040297755,8.54599719825042));
#50286=CARTESIAN_POINT('Ctrl Pts',(-4.53789809794217,15.0699719631857,8.38899707089818));
#50287=CARTESIAN_POINT('Ctrl Pts',(-4.1314278504052,11.6669507850401,8.23199694354592));
#50288=CARTESIAN_POINT('Ctrl Pts',(-6.74558856429446,9.45066222537301,8.07499681619367));
#50289=CARTESIAN_POINT('Ctrl Pts',(-10.0362372509614,10.4084735018199,7.91799668884141));
#50290=CARTESIAN_POINT('Ctrl Pts',(-11.0526176626825,13.6815060514322,7.76099656148917));
#50291=CARTESIAN_POINT('Ctrl Pts',(-8.88333173423194,16.3348001890992,7.6039964341369));
#50292=CARTESIAN_POINT('Ctrl Pts',(-5.47359896850368,15.9891216041795,7.44699630678466));
#50293=CARTESIAN_POINT('Ctrl Pts',(-3.88095944817013,12.9544436048999,7.28999617943239));
#50294=CARTESIAN_POINT('Ctrl Pts',(-5.53354831017302,9.95199105749957,7.13299605208015));
#50295=CARTESIAN_POINT('Ctrl Pts',(-8.9494732676674,9.67409198306777,6.97599592472789));
#50296=CARTESIAN_POINT('Ctrl Pts',(-11.0656416405671,12.3699411133323,6.81899579737564));
#50297=CARTESIAN_POINT('Ctrl Pts',(-9.98446494686864,15.6221447375545,6.66199567002338));
#50298=CARTESIAN_POINT('Ctrl Pts',(-6.67544470099851,16.5144205342573,6.50499554267113));
#50299=CARTESIAN_POINT('Ctrl Pts',(-4.10581110106408,14.2466564935293,6.34799541531888));
#50300=CARTESIAN_POINT('Ctrl Pts',(-4.57977925134152,10.8523778836063,6.19099528796662));
#50301=CARTESIAN_POINT('Ctrl Pts',(-7.67233735803906,9.3752678814539,6.03399516061438));
#50302=CARTESIAN_POINT('Ctrl Pts',(-10.6103589107324,11.1398632710606,5.87699503326211));
#50303=CARTESIAN_POINT('Ctrl Pts',(-10.7592917725406,14.5638382055826,5.71999490590987));
#50304=CARTESIAN_POINT('Ctrl Pts',(-7.98558646537732,16.576874141135,5.56299477855761));
#50305=CARTESIAN_POINT('Ctrl Pts',(-4.77645105419042,15.3738768659897,5.40599465120536));
#50306=CARTESIAN_POINT('Ctrl Pts',(-4.00954823259222,12.0335573562934,5.24899452385311));
#50307=CARTESIAN_POINT('Ctrl Pts',(-6.37256675930357,9.55126737969704,5.09199439650085));
#50308=CARTESIAN_POINT('Ctrl Pts',(-9.74656595354479,10.1527921341227,4.9349942691486));
#50309=CARTESIAN_POINT('Ctrl Pts',(-11.1060469959117,13.2989499872504,4.77799414179634));
#50310=CARTESIAN_POINT('Ctrl Pts',(-9.2319528795399,16.1681374132995,4.62099401444409));
#50311=CARTESIAN_POINT('Ctrl Pts',(-5.80479653057489,16.1883357805992,4.46399388709183));
#50312=CARTESIAN_POINT('Ctrl Pts',(-3.89775210281319,13.3398493780975,4.30699375973959));
#50313=CARTESIAN_POINT('Ctrl Pts',(-5.22086568363505,10.1800446040033,4.14999363238733));
#50314=CARTESIAN_POINT('Ctrl Pts',(-8.58771529500726,9.53625069635182,3.99299350503508));
#50315=CARTESIAN_POINT('Ctrl Pts',(-10.9792742142571,11.9980184020288,3.83599337768282));
#50316=CARTESIAN_POINT('Ctrl Pts',(-10.4928159504458,14.2195377949103,3.73132662611465));
#50317=CARTESIAN_POINT('Ctrl Pts',(-9.83606265769613,14.9876826136973,3.67899325033057));
#50318=CARTESIAN_POINT('Ctrl Pts',(-8.245932854347,10.2002034869244,12.1070022498898));
#50319=CARTESIAN_POINT('Ctrl Pts',(-9.16339987378202,10.4454813502309,12.0546688741057));
#50320=CARTESIAN_POINT('Ctrl Pts',(-10.7225982799205,11.9069099460203,11.9500021225376));
#50321=CARTESIAN_POINT('Ctrl Pts',(-10.1809169554557,15.086313755117,11.7930019951853));
#50322=CARTESIAN_POINT('Ctrl Pts',(-7.23091907843985,16.3798774687766,11.636001867833));
#50323=CARTESIAN_POINT('Ctrl Pts',(-4.52437279676603,14.6371718749705,11.4790017404808));
#50324=CARTESIAN_POINT('Ctrl Pts',(-4.48499759650499,11.4161896364091,11.3220016131285));
#50325=CARTESIAN_POINT('Ctrl Pts',(-7.14976705210776,9.60760802538281,11.1650014857763));
#50326=CARTESIAN_POINT('Ctrl Pts',(-10.1283059986405,10.8319785554116,11.008001358424));
#50327=CARTESIAN_POINT('Ctrl Pts',(-10.7501648077581,13.992020329963,10.8510012310718));
#50328=CARTESIAN_POINT('Ctrl Pts',(-8.45749448845756,16.2537747113328,10.6940011037195));
#50329=CARTESIAN_POINT('Ctrl Pts',(-5.30626809181812,15.5892678153629,10.5370009763673));
#50330=CARTESIAN_POINT('Ctrl Pts',(-4.12216250860425,12.5942860586688,10.380000849015));
#50331=CARTESIAN_POINT('Ctrl Pts',(-5.96700624445078,9.95450088514863,10.2230007216628));
#50332=CARTESIAN_POINT('Ctrl Pts',(-9.18649505892511,10.0370112274744,10.0660005943105));
#50333=CARTESIAN_POINT('Ctrl Pts',(-10.8936901958899,12.7678403902015,9.90900046695827));
#50334=CARTESIAN_POINT('Ctrl Pts',(-9.5577294368621,15.6982219813021,9.752000339606));
#50335=CARTESIAN_POINT('Ctrl Pts',(-6.3765836355766,16.2004576199972,9.59500021225376));
#50336=CARTESIAN_POINT('Ctrl Pts',(-4.20281571587151,13.8241863062249,9.4380000849015));
#50337=CARTESIAN_POINT('Ctrl Pts',(-4.98566475436435,10.7002340827391,9.28099995754925));
#50338=CARTESIAN_POINT('Ctrl Pts',(-8.02314223764118,9.62987849036962,9.123999830197));
#50339=CARTESIAN_POINT('Ctrl Pts',(-10.5915131043488,11.5729178555327,8.96699970284474));
#50340=CARTESIAN_POINT('Ctrl Pts',(-10.3876944878733,14.7870100374982,8.80999957549249));
#50341=CARTESIAN_POINT('Ctrl Pts',(-7.59445253304005,16.3900477938888,8.65299944814024));
#50342=CARTESIAN_POINT('Ctrl Pts',(-4.71651407945554,14.9445717631999,8.49599932078798));
#50343=CARTESIAN_POINT('Ctrl Pts',(-4.33455415756585,11.7467541830206,8.33899919343573));
#50344=CARTESIAN_POINT('Ctrl Pts',(-6.79107988887037,9.66410874890807,8.18199906608347));
#50345=CARTESIAN_POINT('Ctrl Pts',(-9.88330108572798,10.5641636054531,8.02499893873122));
#50346=CARTESIAN_POINT('Ctrl Pts',(-10.8383933342348,13.6398309256761,7.86799881137897));
#50347=CARTESIAN_POINT('Ctrl Pts',(-8.79991625305057,16.1331303189645,7.71099868402671));
#50348=CARTESIAN_POINT('Ctrl Pts',(-5.59579179682231,15.8082962970528,7.55399855667447));
#50349=CARTESIAN_POINT('Ctrl Pts',(-4.09918910456809,12.956610648253,7.39699842932221));
#50350=CARTESIAN_POINT('Ctrl Pts',(-5.65212616815729,10.1352072431286,7.23999830196996));
#50351=CARTESIAN_POINT('Ctrl Pts',(-8.86206942440258,9.8740655989212,7.0829981746177));
#50352=CARTESIAN_POINT('Ctrl Pts',(-10.8506319608149,12.4073539009847,6.92599804726545));
#50353=CARTESIAN_POINT('Ctrl Pts',(-9.83465067318943,15.4634482887157,6.76899791991319));
#50354=CARTESIAN_POINT('Ctrl Pts',(-6.72516572981961,16.3019194823095,6.61199779256095));
#50355=CARTESIAN_POINT('Ctrl Pts',(-4.3104821089062,14.1709025601374,6.45499766520868));
#50356=CARTESIAN_POINT('Ctrl Pts',(-4.75586978181755,10.9813003676665,6.29799753785644));
#50357=CARTESIAN_POINT('Ctrl Pts',(-7.6619453433902,9.59326071540802,6.14099741050417));
#50358=CARTESIAN_POINT('Ctrl Pts',(-10.4228029696916,11.2514502662184,5.98399728315193));
#50359=CARTESIAN_POINT('Ctrl Pts',(-10.5627551177461,14.4689580825154,5.82699715579967));
#50360=CARTESIAN_POINT('Ctrl Pts',(-7.95630539875948,16.360607110615,5.66999702844743));
#50361=CARTESIAN_POINT('Ctrl Pts',(-4.94068219283476,15.23015107347,5.51299690109516));
#50362=CARTESIAN_POINT('Ctrl Pts',(-4.22002393159755,12.0912542249516,5.35599677374292));
#50363=CARTESIAN_POINT('Ctrl Pts',(-6.44055145447491,9.75864737041887,5.19899664639066));
#50364=CARTESIAN_POINT('Ctrl Pts',(-9.61109708849724,10.3238999309873,5.04199651903841));
#50365=CARTESIAN_POINT('Ctrl Pts',(-10.8886008563611,13.2803431519,4.88499639168615));
#50366=CARTESIAN_POINT('Ctrl Pts',(-9.12751539773043,15.9765173781352,4.72799626433391));
#50367=CARTESIAN_POINT('Ctrl Pts',(-5.9070180076098,15.995497775453,4.57099613698164));
#50368=CARTESIAN_POINT('Ctrl Pts',(-4.11496915512444,13.3187762924015,4.4139960096294));
#50369=CARTESIAN_POINT('Ctrl Pts',(-5.35829843455949,10.3495090655549,4.25699588227714));
#50370=CARTESIAN_POINT('Ctrl Pts',(-8.52212560854514,9.74453619934955,4.09999575492489));
#50371=CARTESIAN_POINT('Ctrl Pts',(-10.7694725263739,12.0578582844684,3.94299562757263));
#50372=CARTESIAN_POINT('Ctrl Pts',(-10.31234789899,14.1454191303684,3.83832887600446));
#50373=CARTESIAN_POINT('Ctrl Pts',(-9.6951971040191,14.8672444958454,3.78599550022038));
#50374=CARTESIAN_POINT('Ctrl Pts',(-8.19806642616107,10.379248870828,12.2140044997796));
#50375=CARTESIAN_POINT('Ctrl Pts',(-9.05665968914092,10.6087872809636,12.1616711239955));
#50376=CARTESIAN_POINT('Ctrl Pts',(-10.5158045072117,11.9764361665263,12.0570043724274));
#50377=CARTESIAN_POINT('Ctrl Pts',(-10.0088828130085,14.9518179872963,11.9000042450751));
#50378=CARTESIAN_POINT('Ctrl Pts',(-7.24818597120775,16.1623738615197,11.7430041177229));
#50379=CARTESIAN_POINT('Ctrl Pts',(-4.71531846299006,14.531497491576,11.5860039903706));
#50380=CARTESIAN_POINT('Ctrl Pts',(-4.67846996494438,11.5172053245294,11.4290038630183));
#50381=CARTESIAN_POINT('Ctrl Pts',(-7.17224146136718,9.82468019405374,11.2720037356661));
#50382=CARTESIAN_POINT('Ctrl Pts',(-9.9596478954327,10.9704830035337,11.1150036083138));
#50383=CARTESIAN_POINT('Ctrl Pts',(-10.5416020940281,13.9277452493586,10.9580034809616));
#50384=CARTESIAN_POINT('Ctrl Pts',(-8.39605217377323,16.0443631039765,10.8010033536093));
#50385=CARTESIAN_POINT('Ctrl Pts',(-5.44703962404145,15.4224975415121,10.6440032262571));
#50386=CARTESIAN_POINT('Ctrl Pts',(-4.33891796422385,12.6197034305821,10.4870030989048));
#50387=CARTESIAN_POINT('Ctrl Pts',(-6.06537828300873,10.1493129776432,10.3300029715526));
#50388=CARTESIAN_POINT('Ctrl Pts',(-9.07827285882558,10.2265286404914,10.1730028442003));
#50389=CARTESIAN_POINT('Ctrl Pts',(-10.6759174739885,12.7821207999897,10.0160027168481));
#50390=CARTESIAN_POINT('Ctrl Pts',(-9.4256851680762,15.5244601307577,9.85900258949583));
#50391=CARTESIAN_POINT('Ctrl Pts',(-6.4486731385623,15.9944673644538,9.70200246214356));
#50392=CARTESIAN_POINT('Ctrl Pts',(-4.41439566416342,13.7706811162314,9.54500233479132));
#50393=CARTESIAN_POINT('Ctrl Pts',(-5.14700936704523,10.8471925589996,9.38800220743905));
#50394=CARTESIAN_POINT('Ctrl Pts',(-7.98957225851618,9.84552156578271,9.23100208008681));
#50395=CARTESIAN_POINT('Ctrl Pts',(-10.393131052757,11.6638763112873,9.07400195273455));
#50396=CARTESIAN_POINT('Ctrl Pts',(-10.2023914542005,14.6717205559024,8.9170018253823));
#50397=CARTESIAN_POINT('Ctrl Pts',(-7.58839152451442,16.1718915580022,8.76000169803004));
#50398=CARTESIAN_POINT('Ctrl Pts',(-4.89513006096893,14.8191715632141,8.6030015706778));
#50399=CARTESIAN_POINT('Ctrl Pts',(-4.53768046472649,11.8265575810012,8.44600144332554));
#50400=CARTESIAN_POINT('Ctrl Pts',(-6.83657121344629,9.87755527244308,8.28900131597329));
#50401=CARTESIAN_POINT('Ctrl Pts',(-9.73036492049458,10.7198537090864,8.13200118862103));
#50402=CARTESIAN_POINT('Ctrl Pts',(-10.6241690057872,13.59815579992,7.97500106126879));
#50403=CARTESIAN_POINT('Ctrl Pts',(-8.71650077186918,15.9314604488298,7.81800093391652));
#50404=CARTESIAN_POINT('Ctrl Pts',(-5.71798462514094,15.6274709899262,7.66100080656428));
#50405=CARTESIAN_POINT('Ctrl Pts',(-4.31741876096606,12.9587776916062,7.50400067921201));
#50406=CARTESIAN_POINT('Ctrl Pts',(-5.77070402614152,10.3184234287576,7.34700055185978));
#50407=CARTESIAN_POINT('Ctrl Pts',(-8.7746655811378,10.0740392147746,7.19000042450751));
#50408=CARTESIAN_POINT('Ctrl Pts',(-10.6356222810626,12.4447666886372,7.03300029715527));
#50409=CARTESIAN_POINT('Ctrl Pts',(-9.68483639951025,15.304751839877,6.876000169803));
#50410=CARTESIAN_POINT('Ctrl Pts',(-6.77488675864068,16.0894184303616,6.71900004245076));
#50411=CARTESIAN_POINT('Ctrl Pts',(-4.51515311674835,14.0951486267455,6.56199991509849));
#50412=CARTESIAN_POINT('Ctrl Pts',(-4.93196031229355,11.1102228517267,6.40499978774625));
#50413=CARTESIAN_POINT('Ctrl Pts',(-7.65155332874137,9.81125354936211,6.24799966039399));
#50414=CARTESIAN_POINT('Ctrl Pts',(-10.2352470286507,11.3630372613762,6.09099953304174));
#50415=CARTESIAN_POINT('Ctrl Pts',(-10.3662184629517,14.3740779594481,5.93399940568949));
#50416=CARTESIAN_POINT('Ctrl Pts',(-7.92702433214164,16.1443400800951,5.77699927833723));
#50417=CARTESIAN_POINT('Ctrl Pts',(-5.10491333147909,15.0864252809503,5.61999915098498));
#50418=CARTESIAN_POINT('Ctrl Pts',(-4.4304996306029,12.1489510936098,5.46299902363272));
#50419=CARTESIAN_POINT('Ctrl Pts',(-6.50853614964623,9.96602736114071,5.30599889628047));
#50420=CARTESIAN_POINT('Ctrl Pts',(-9.47562822344969,10.4950077278519,5.14899876892822));
#50421=CARTESIAN_POINT('Ctrl Pts',(-10.6711547168104,13.2617363165495,4.99199864157597));
#50422=CARTESIAN_POINT('Ctrl Pts',(-9.02307791592096,15.7848973429709,4.83499851422371));
#50423=CARTESIAN_POINT('Ctrl Pts',(-6.0092394846447,15.8026597703067,4.67799838687145));
#50424=CARTESIAN_POINT('Ctrl Pts',(-4.33218620743569,13.2977032067055,4.52099825951921));
#50425=CARTESIAN_POINT('Ctrl Pts',(-5.49573118548395,10.5189735271065,4.36399813216694));
#50426=CARTESIAN_POINT('Ctrl Pts',(-8.45653592208301,9.95282170234728,4.20699800481471));
#50427=CARTESIAN_POINT('Ctrl Pts',(-10.5596708384907,12.117698166908,4.04999787746244));
#50428=CARTESIAN_POINT('Ctrl Pts',(-10.1318798475343,14.0713004658266,3.94533112589427));
#50429=CARTESIAN_POINT('Ctrl Pts',(-9.55433155034207,14.7468063779934,3.89299775011019));
#50430=CARTESIAN_POINT('Ctrl Pts',(-8.15019999797515,10.5582942547315,12.3210067496694));
#50431=CARTESIAN_POINT('Ctrl Pts',(-8.94991950449982,10.7720932116964,12.2686733738853));
#50432=CARTESIAN_POINT('Ctrl Pts',(-10.3090107345028,12.0459623870324,12.1640066223172));
#50433=CARTESIAN_POINT('Ctrl Pts',(-9.83684867056136,14.8173222194755,12.0070064949649));
#50434=CARTESIAN_POINT('Ctrl Pts',(-7.26545286397565,15.9448702542628,11.8500063676127));
#50435=CARTESIAN_POINT('Ctrl Pts',(-4.90626412921408,14.4258231081815,11.6930062402604));
#50436=CARTESIAN_POINT('Ctrl Pts',(-4.87194233338379,11.6182210126498,11.5360061129081));
#50437=CARTESIAN_POINT('Ctrl Pts',(-7.19471587062657,10.0417523627247,11.3790059855559));
#50438=CARTESIAN_POINT('Ctrl Pts',(-9.79098979222489,11.1089874516557,11.2220058582036));
#50439=CARTESIAN_POINT('Ctrl Pts',(-10.3330393802981,13.8634701687541,11.0650057308514));
#50440=CARTESIAN_POINT('Ctrl Pts',(-8.33460985908889,15.8349514966202,10.9080056034991));
#50441=CARTESIAN_POINT('Ctrl Pts',(-5.5878111562648,15.2557272676614,10.7510054761469));
#50442=CARTESIAN_POINT('Ctrl Pts',(-4.55567341984345,12.6451208024954,10.5940053487946));
#50443=CARTESIAN_POINT('Ctrl Pts',(-6.16375032156668,10.3441250701379,10.4370052214424));
#50444=CARTESIAN_POINT('Ctrl Pts',(-8.97005065872605,10.4160460535085,10.2800050940901));
#50445=CARTESIAN_POINT('Ctrl Pts',(-10.4581447520871,12.796401209778,10.1230049667379));
#50446=CARTESIAN_POINT('Ctrl Pts',(-9.29364089929031,15.3506982802133,9.96600483938563));
#50447=CARTESIAN_POINT('Ctrl Pts',(-6.52076264154797,15.7884771089103,9.80900471203338));
#50448=CARTESIAN_POINT('Ctrl Pts',(-4.62597561245536,13.7171759262378,9.65200458468112));
#50449=CARTESIAN_POINT('Ctrl Pts',(-5.3083539797261,10.9941510352601,9.49500445732887));
#50450=CARTESIAN_POINT('Ctrl Pts',(-7.95600227939119,10.0611646411958,9.33800432997662));
#50451=CARTESIAN_POINT('Ctrl Pts',(-10.1947490011651,11.7548347670419,9.18100420262436));
#50452=CARTESIAN_POINT('Ctrl Pts',(-10.0170884205278,14.5564310743066,9.02400407527211));
#50453=CARTESIAN_POINT('Ctrl Pts',(-7.5823305159888,15.9537353221155,8.86700394791986));
#50454=CARTESIAN_POINT('Ctrl Pts',(-5.07374604248231,14.6937713632283,8.71000382056761));
#50455=CARTESIAN_POINT('Ctrl Pts',(-4.74080677188713,11.9063609789818,8.55300369321535));
#50456=CARTESIAN_POINT('Ctrl Pts',(-6.88206253802222,10.0910017959781,8.3960035658631));
#50457=CARTESIAN_POINT('Ctrl Pts',(-9.57742875526118,10.8755438127196,8.23900343851084));
#50458=CARTESIAN_POINT('Ctrl Pts',(-10.4099446773395,13.5564806741639,8.0820033111586));
#50459=CARTESIAN_POINT('Ctrl Pts',(-8.63308529068779,15.7297905786951,7.92500318380633));
#50460=CARTESIAN_POINT('Ctrl Pts',(-5.84017745345957,15.4466456827995,7.7680030564541));
#50461=CARTESIAN_POINT('Ctrl Pts',(-4.53564841736402,12.9609447349594,7.61100292910181));
#50462=CARTESIAN_POINT('Ctrl Pts',(-5.88928188412577,10.5016396143867,7.45400280174959));
#50463=CARTESIAN_POINT('Ctrl Pts',(-8.687261737873,10.2740128306281,7.29700267439731));
#50464=CARTESIAN_POINT('Ctrl Pts',(-10.4206126013104,12.4821794762896,7.14000254704508));
#50465=CARTESIAN_POINT('Ctrl Pts',(-9.53502212583107,15.1460553910382,6.98300241969281));
#50466=CARTESIAN_POINT('Ctrl Pts',(-6.82460778746177,15.8769173784138,6.82600229234057));
#50467=CARTESIAN_POINT('Ctrl Pts',(-4.71982412459047,14.0193946933536,6.66900216498831));
#50468=CARTESIAN_POINT('Ctrl Pts',(-5.10805084276957,11.2391453357869,6.51200203763605));
#50469=CARTESIAN_POINT('Ctrl Pts',(-7.64116131409251,10.0292463833162,6.35500191028381));
#50470=CARTESIAN_POINT('Ctrl Pts',(-10.0476910876099,11.474624256534,6.19800178293155));
#50471=CARTESIAN_POINT('Ctrl Pts',(-10.1696818081572,14.2791978363808,6.0410016555793));
#50472=CARTESIAN_POINT('Ctrl Pts',(-7.89774326552381,15.9280730495752,5.88400152822705));
#50473=CARTESIAN_POINT('Ctrl Pts',(-5.26914447012342,14.9426994884306,5.72700140087479));
#50474=CARTESIAN_POINT('Ctrl Pts',(-4.64097532960824,12.206647962268,5.57000127352254));
#50475=CARTESIAN_POINT('Ctrl Pts',(-6.57652084481755,10.1734073518625,5.41300114617028));
#50476=CARTESIAN_POINT('Ctrl Pts',(-9.34015935840215,10.6661155247165,5.25600101881803));
#50477=CARTESIAN_POINT('Ctrl Pts',(-10.4537085772597,13.243129481199,5.09900089146578));
#50478=CARTESIAN_POINT('Ctrl Pts',(-8.91864043411149,15.5932773078066,4.94200076411352));
#50479=CARTESIAN_POINT('Ctrl Pts',(-6.11146096167962,15.6098217651605,4.78500063676127));
#50480=CARTESIAN_POINT('Ctrl Pts',(-4.54940325974693,13.2766301210095,4.62800050940902));
#50481=CARTESIAN_POINT('Ctrl Pts',(-5.63316393640839,10.6884379886581,4.47100038205676));
#50482=CARTESIAN_POINT('Ctrl Pts',(-8.39094623562089,10.161107205345,4.31400025470451));
#50483=CARTESIAN_POINT('Ctrl Pts',(-10.3498691506075,12.1775380493476,4.15700012735225));
#50484=CARTESIAN_POINT('Ctrl Pts',(-9.95141179607851,13.9971818012848,4.05233337578409));
#50485=CARTESIAN_POINT('Ctrl Pts',(-9.41346599666504,14.6263682601415,4.));
#50486=CARTESIAN_POINT('Ctrl Pts',(-10.0159019782719,12.9923925656114,11.112583302492));
#50487=CARTESIAN_POINT('Ctrl Pts',(-10.017856950592,13.2435976299952,11.0967241119451));
#50488=CARTESIAN_POINT('Ctrl Pts',(-9.98318348246503,13.4942759769916,11.0808649213983));
#50489=CARTESIAN_POINT('Ctrl Pts',(-9.90962619541772,13.7329699372154,11.0650057308514));
#50490=CARTESIAN_POINT('Ctrl Pts',(-9.66689620656173,14.5206306113761,11.0126723550673));
#50491=CARTESIAN_POINT('Ctrl Pts',(-9.00075303282531,15.1777910539982,10.9603389792832));
#50492=CARTESIAN_POINT('Ctrl Pts',(-8.20988166215309,15.409833903816,10.9080056034991));
#50493=CARTESIAN_POINT('Ctrl Pts',(-7.41901029148087,15.6418767536339,10.8556722277151));
#50494=CARTESIAN_POINT('Ctrl Pts',(-6.50341072387283,15.4488020106477,10.803338851931));
#50495=CARTESIAN_POINT('Ctrl Pts',(-5.87358798399859,14.9171635616269,10.7510054761469));
#50496=CARTESIAN_POINT('Ctrl Pts',(-5.24376524412435,14.3855251126061,10.6986721003628));
#50497=CARTESIAN_POINT('Ctrl Pts',(-4.8997193319839,13.5153229575507,10.6463387245787));
#50498=CARTESIAN_POINT('Ctrl Pts',(-4.99570919286755,12.6967225912968,10.5940053487946));
#50499=CARTESIAN_POINT('Ctrl Pts',(-5.09169905375119,11.8781222250429,10.5416719730106));
#50500=CARTESIAN_POINT('Ctrl Pts',(-5.62772468765894,11.1111236475904,10.4893385972265));
#50501=CARTESIAN_POINT('Ctrl Pts',(-6.3634542274727,10.7396111894259,10.4370052214424));
#50502=CARTESIAN_POINT('Ctrl Pts',(-7.09918376728647,10.3680987312614,10.3846718456583));
#50503=CARTESIAN_POINT('Ctrl Pts',(-8.03461721300627,10.392072392385,10.3323384698742));
#50504=CARTESIAN_POINT('Ctrl Pts',(-8.750349618093,10.800785082325,10.2800050940901));
#50505=CARTESIAN_POINT('Ctrl Pts',(-9.46608202317973,11.209497772265,10.227671718306));
#50506=CARTESIAN_POINT('Ctrl Pts',(-9.9621133876334,12.0029494910215,10.175338342522));
#50507=CARTESIAN_POINT('Ctrl Pts',(-10.0160450943941,12.8253915288056,10.1230049667379));
#50508=CARTESIAN_POINT('Ctrl Pts',(-10.0196250796435,12.8799852092316,10.1195310786559));
#50509=CARTESIAN_POINT('Ctrl Pts',(-10.0212570407989,12.9347066297247,10.116057190574));
#50510=CARTESIAN_POINT('Ctrl Pts',(-10.0209918820407,12.9894441341194,10.112583302492));
#50511=CARTESIAN_POINT('Ctrl Pts',(-8.29379928253292,10.0211581030209,12.));
#50512=CARTESIAN_POINT('Ctrl Pts',(-8.38688154479599,10.0552080103525,12.));
#50513=CARTESIAN_POINT('Ctrl Pts',(-8.4779006806254,10.0940206699959,12.));
#50514=CARTESIAN_POINT('Ctrl Pts',(-8.56664686325615,10.1372696205127,12.));
#50515=CARTESIAN_POINT('Ctrl Pts',(-8.65733903335545,10.1814669150961,12.));
#50516=CARTESIAN_POINT('Ctrl Pts',(-8.74565814612796,10.2302978026812,12.));
#50517=CARTESIAN_POINT('Ctrl Pts',(-8.83135135493958,10.2834593640583,12.));
#50518=CARTESIAN_POINT('Ctrl Pts',(-8.91318992856164,10.3342296224599,12.));
#50519=CARTESIAN_POINT('Ctrl Pts',(-8.99263375816446,10.3889506025256,12.));
#50520=CARTESIAN_POINT('Ctrl Pts',(-9.06943047246088,10.4473877517771,12.));
#50521=CARTESIAN_POINT('Ctrl Pts',(-9.13662759747024,10.4985202573722,12.));
#50522=CARTESIAN_POINT('Ctrl Pts',(-9.20179774209257,10.5524986289602,12.));
#50523=CARTESIAN_POINT('Ctrl Pts',(-9.26474793392036,10.6091781306825,12.));
#50524=CARTESIAN_POINT('Ctrl Pts',(-9.27985634938565,10.6227815437226,12.));
#50525=CARTESIAN_POINT('Ctrl Pts',(-9.29484046111391,10.636544177759,12.));
#50526=CARTESIAN_POINT('Ctrl Pts',(-9.30967515586603,10.6504428556362,12.));
#50527=CARTESIAN_POINT('Ctrl Pts',(-9.38210515214773,10.718302774818,12.));
#50528=CARTESIAN_POINT('Ctrl Pts',(-9.45106930229927,10.7894833711807,12.));
#50529=CARTESIAN_POINT('Ctrl Pts',(-9.51632661790574,10.8636962448604,12.));
#50530=CARTESIAN_POINT('Ctrl Pts',(-9.58121902341258,10.9374941301685,12.));
#50531=CARTESIAN_POINT('Ctrl Pts',(-9.64244642197802,11.0142912680357,12.));
#50532=CARTESIAN_POINT('Ctrl Pts',(-9.69972824598415,11.0938308479656,12.));
#50533=CARTESIAN_POINT('Ctrl Pts',(-9.75408303717497,11.169306050327,12.));
#50534=CARTESIAN_POINT('Ctrl Pts',(-9.80488522775839,11.2472513152745,12.));
#50535=CARTESIAN_POINT('Ctrl Pts',(-9.85185250012922,11.3274602381139,12.));
#50536=CARTESIAN_POINT('Ctrl Pts',(-9.88922975528545,11.3912916940074,12.));
#50537=CARTESIAN_POINT('Ctrl Pts',(-9.92417754353756,11.4565571180282,12.));
#50538=CARTESIAN_POINT('Ctrl Pts',(-9.95653223361561,11.5231545729247,12.));
#50539=CARTESIAN_POINT('Ctrl Pts',(-9.96243512991986,11.5353048321122,12.));
#50540=CARTESIAN_POINT('Ctrl Pts',(-9.96824994557655,11.5474959894548,12.));
#50541=CARTESIAN_POINT('Ctrl Pts',(-9.97397248881904,11.5597200854486,12.));
#50542=CARTESIAN_POINT('Ctrl Pts',(-10.0145489524258,11.6463966845059,12.));
#50543=CARTESIAN_POINT('Ctrl Pts',(-10.0505436256048,11.7348369448931,12.));
#50544=CARTESIAN_POINT('Ctrl Pts',(-10.0816929753162,11.8247972357439,12.));
#50545=CARTESIAN_POINT('Ctrl Pts',(-10.1128423250276,11.9147575265948,12.));
#50546=CARTESIAN_POINT('Ctrl Pts',(-10.1391468173479,12.0062385811789,12.));
#50547=CARTESIAN_POINT('Ctrl Pts',(-10.1602867132728,12.0990065815937,12.));
#50548=CARTESIAN_POINT('Ctrl Pts',(-10.1814517508012,12.1918849106638,12.));
#50549=CARTESIAN_POINT('Ctrl Pts',(-10.197439126489,12.286054432468,12.));
#50550=CARTESIAN_POINT('Ctrl Pts',(-10.2083242813819,12.381106938598,12.));
#50551=CARTESIAN_POINT('Ctrl Pts',(-10.2138913557349,12.4297203367777,12.));
#50552=CARTESIAN_POINT('Ctrl Pts',(-10.2181230259612,12.4785645227018,12.));
#50553=CARTESIAN_POINT('Ctrl Pts',(-10.2210244442513,12.527583085919,12.));
#50554=CARTESIAN_POINT('Ctrl Pts',(-10.2218610165225,12.5417167152898,12.));
#50555=CARTESIAN_POINT('Ctrl Pts',(-10.2225869774383,12.5558648310221,12.));
#50556=CARTESIAN_POINT('Ctrl Pts',(-10.2232024018895,12.5700260533185,12.));
#50557=CARTESIAN_POINT('Ctrl Pts',(-10.2238236012139,12.5843201583174,12.));
#50558=CARTESIAN_POINT('Ctrl Pts',(-10.2243317772527,12.598618709654,12.));
#50559=CARTESIAN_POINT('Ctrl Pts',(-10.2247273702154,12.6129172463203,12.));
#50560=CARTESIAN_POINT('Ctrl Pts',(-10.227308430526,12.7062085557579,12.));
#50561=CARTESIAN_POINT('Ctrl Pts',(-10.2251031453087,12.7995425030326,12.));
#50562=CARTESIAN_POINT('Ctrl Pts',(-10.2182400386914,12.8925419864032,12.));
#50563=CARTESIAN_POINT('Ctrl Pts',(-10.2113727169558,12.985598587323,12.));
#50564=CARTESIAN_POINT('Ctrl Pts',(-10.1998414736524,13.0783212906945,12.));
#50565=CARTESIAN_POINT('Ctrl Pts',(-10.1837245157332,13.1703195860503,12.));
#50566=CARTESIAN_POINT('Ctrl Pts',(-10.167850633777,13.2609303630954,12.));
#50567=CARTESIAN_POINT('Ctrl Pts',(-10.1475278620093,13.3508392541549,12.));
#50568=CARTESIAN_POINT('Ctrl Pts',(-10.1227882581427,13.4396474637383,12.));
#50569=CARTESIAN_POINT('Ctrl Pts',(-10.1129089853156,13.4751112705354,12.));
#50570=CARTESIAN_POINT('Ctrl Pts',(-10.102324939091,13.5103991993701,12.));
#50571=CARTESIAN_POINT('Ctrl Pts',(-10.0910364592447,13.5454842372103,12.));
#50572=CARTESIAN_POINT('Ctrl Pts',(-10.0850885997417,13.5639704176856,12.));
#50573=CARTESIAN_POINT('Ctrl Pts',(-10.0789451599571,13.5824002543575,12.));
#50574=CARTESIAN_POINT('Ctrl Pts',(-10.0726060885077,13.6007696733809,12.));
#50575=CARTESIAN_POINT('Ctrl Pts',(-10.0672512100823,13.6162870888888,12.));
#50576=CARTESIAN_POINT('Ctrl Pts',(-10.0617593012071,13.6317538427315,12.));
#50577=CARTESIAN_POINT('Ctrl Pts',(-10.05613256518,13.6471627242414,12.));
#50578=CARTESIAN_POINT('Ctrl Pts',(-10.0253173594462,13.7315505205696,12.));
#50579=CARTESIAN_POINT('Ctrl Pts',(-9.99044489732798,13.8142532308756,12.));
#50580=CARTESIAN_POINT('Ctrl Pts',(-9.95156720789968,13.8949006686344,12.));
#50581=CARTESIAN_POINT('Ctrl Pts',(-9.92246136322671,13.9552775025255,12.));
#50582=CARTESIAN_POINT('Ctrl Pts',(-9.89110978386257,14.0145019588769,12.));
#50583=CARTESIAN_POINT('Ctrl Pts',(-9.85752072526523,14.0724054243587,12.));
#50584=CARTESIAN_POINT('Ctrl Pts',(-9.84460176992236,14.0946761373823,12.));
#50585=CARTESIAN_POINT('Ctrl Pts',(-9.83135170762611,14.1167512973966,12.));
#50586=CARTESIAN_POINT('Ctrl Pts',(-9.81777059343282,14.1386207605303,12.));
#50587=CARTESIAN_POINT('Ctrl Pts',(-9.80600921691784,14.1575599275555,12.));
#50588=CARTESIAN_POINT('Ctrl Pts',(-9.79399757751539,14.1763475835755,12.));
#50589=CARTESIAN_POINT('Ctrl Pts',(-9.78174994291027,14.194955852553,12.));
#50590=CARTESIAN_POINT('Ctrl Pts',(-9.73447804437696,14.2667777374594,12.));
#50591=CARTESIAN_POINT('Ctrl Pts',(-9.68365470418875,14.3359945738428,12.));
#50592=CARTESIAN_POINT('Ctrl Pts',(-9.62930889486242,14.4022524491644,12.));
#50593=CARTESIAN_POINT('Ctrl Pts',(-9.58717510546268,14.453621550103,12.));
#50594=CARTESIAN_POINT('Ctrl Pts',(-9.54292331405751,14.5032115233845,12.));
#50595=CARTESIAN_POINT('Ctrl Pts',(-9.49655459700825,14.5508396884611,12.));
#50596=CARTESIAN_POINT('Ctrl Pts',(-9.47068873424204,14.5774081091567,12.));
#50597=CARTESIAN_POINT('Ctrl Pts',(-9.44416391721335,14.6033657382126,12.));
#50598=CARTESIAN_POINT('Ctrl Pts',(-9.41700728965907,14.6287007311509,12.));
#50599=CARTESIAN_POINT('Origin',(-7.5,12.9903810567666,7.5));
#50600=CARTESIAN_POINT('Origin',(-7.50000000000001,-12.9903810567666,4.));
#50601=CARTESIAN_POINT('Ctrl Pts',(-9.41346599666503,-11.3543938533916,
4.));
#50602=CARTESIAN_POINT('Ctrl Pts',(-9.47563125999352,-11.4128139360928,
4.));
#50603=CARTESIAN_POINT('Ctrl Pts',(-9.5344254182292,-11.4744857433087,4.));
#50604=CARTESIAN_POINT('Ctrl Pts',(-9.58983450470078,-11.5390333604437,
4.));
#50605=CARTESIAN_POINT('Ctrl Pts',(-9.64659408185619,-11.6051542024983,
4.));
#50606=CARTESIAN_POINT('Ctrl Pts',(-9.69980203857783,-11.6742932390243,
4.));
#50607=CARTESIAN_POINT('Ctrl Pts',(-9.74941453503823,-11.7460926626337,
4.));
#50608=CARTESIAN_POINT('Ctrl Pts',(-9.76241984954432,-11.7649140111248,
4.));
#50609=CARTESIAN_POINT('Ctrl Pts',(-9.77517792533989,-11.7839183899685,
4.));
#50610=CARTESIAN_POINT('Ctrl Pts',(-9.78768759195629,-11.8030997933617,
4.));
#50611=CARTESIAN_POINT('Ctrl Pts',(-9.79776752365911,-11.8185556198114,
4.));
#50612=CARTESIAN_POINT('Ctrl Pts',(-9.8076865335191,-11.8341271625133,4.));
#50613=CARTESIAN_POINT('Ctrl Pts',(-9.81743537915168,-11.8497970439193,
4.));
#50614=CARTESIAN_POINT('Ctrl Pts',(-9.86491247379083,-11.9261097142127,
4.));
#50615=CARTESIAN_POINT('Ctrl Pts',(-9.90840731623012,-12.0048277686438,
4.));
#50616=CARTESIAN_POINT('Ctrl Pts',(-9.94788306281372,-12.0855595944701,
4.));
#50617=CARTESIAN_POINT('Ctrl Pts',(-9.97942487229752,-12.150065730259,4.));
#50618=CARTESIAN_POINT('Ctrl Pts',(-10.0084002601673,-12.2158586031585,
4.));
#50619=CARTESIAN_POINT('Ctrl Pts',(-10.034773868227,-12.2827556582142,4.));
#50620=CARTESIAN_POINT('Ctrl Pts',(-10.0434527794708,-12.3047698476261,
4.));
#50621=CARTESIAN_POINT('Ctrl Pts',(-10.0518498142904,-12.326903713834,4.));
#50622=CARTESIAN_POINT('Ctrl Pts',(-10.0599633247681,-12.3491510331904,
4.));
#50623=CARTESIAN_POINT('Ctrl Pts',(-10.0673313519173,-12.369354230495,4.));
#50624=CARTESIAN_POINT('Ctrl Pts',(-10.0744669979504,-12.3896556179549,
4.));
#50625=CARTESIAN_POINT('Ctrl Pts',(-10.0813595780794,-12.4100219884372,
4.));
#50626=CARTESIAN_POINT('Ctrl Pts',(-10.110937259752,-12.4974188719965,4.));
#50627=CARTESIAN_POINT('Ctrl Pts',(-10.1360761396945,-12.5860974112731,
4.));
#50628=CARTESIAN_POINT('Ctrl Pts',(-10.1567415216565,-12.6756607739627,
4.));
#50629=CARTESIAN_POINT('Ctrl Pts',(-10.1777235800004,-12.7665966059193,
4.));
#50630=CARTESIAN_POINT('Ctrl Pts',(-10.194094489083,-12.8584453915162,4.));
#50631=CARTESIAN_POINT('Ctrl Pts',(-10.205776157801,-12.9508249271276,4.));
#50632=CARTESIAN_POINT('Ctrl Pts',(-10.2173669041142,-13.0424854413619,
4.));
#50633=CARTESIAN_POINT('Ctrl Pts',(-10.2243414700862,-13.1346694027891,
4.00000000000001));
#50634=CARTESIAN_POINT('Ctrl Pts',(-10.2265766240073,-13.2270226781325,
4.00000000000001));
#50635=CARTESIAN_POINT('Ctrl Pts',(-10.2276561070688,-13.2716253318781,
4.00000000000001));
#50636=CARTESIAN_POINT('Ctrl Pts',(-10.2276293996605,-13.3162676791034,
4.00000000000001));
#50637=CARTESIAN_POINT('Ctrl Pts',(-10.2264782755414,-13.360910468216,4.00000000000001));
#50638=CARTESIAN_POINT('Ctrl Pts',(-10.2261080116976,-13.3752700063553,
4.00000000000001));
#50639=CARTESIAN_POINT('Ctrl Pts',(-10.2256213911499,-13.3896295910271,
4.00000000000001));
#50640=CARTESIAN_POINT('Ctrl Pts',(-10.2250177409671,-13.40398791621,4.00000000000001));
#50641=CARTESIAN_POINT('Ctrl Pts',(-10.2243866916487,-13.4189979527825,
4.00000000000001));
#50642=CARTESIAN_POINT('Ctrl Pts',(-10.2236280724728,-13.4339981404011,
4.));
#50643=CARTESIAN_POINT('Ctrl Pts',(-10.2227419311859,-13.4489814918393,
4.));
#50644=CARTESIAN_POINT('Ctrl Pts',(-10.2170924746832,-13.5445055278686,
4.));
#50645=CARTESIAN_POINT('Ctrl Pts',(-10.2062608557766,-13.6394136430286,
4.));
#50646=CARTESIAN_POINT('Ctrl Pts',(-10.1901745261949,-13.7333115332678,
4.));
#50647=CARTESIAN_POINT('Ctrl Pts',(-10.1886860667379,-13.74199985474,4.));
#50648=CARTESIAN_POINT('Ctrl Pts',(-10.1871525835688,-13.7506795401449,
4.));
#50649=CARTESIAN_POINT('Ctrl Pts',(-10.1855739978038,-13.7593502843482,
4.));
#50650=CARTESIAN_POINT('Ctrl Pts',(-10.1691852106353,-13.8493694549782,
4.));
#50651=CARTESIAN_POINT('Ctrl Pts',(-10.1479394797701,-13.9384246529327,
4.));
#50652=CARTESIAN_POINT('Ctrl Pts',(-10.1221390901744,-14.0262810420052,
4.));
#50653=CARTESIAN_POINT('Ctrl Pts',(-10.0957476132678,-14.1161502222633,
4.));
#50654=CARTESIAN_POINT('Ctrl Pts',(-10.0645901923201,-14.2047657338476,
4.));
#50655=CARTESIAN_POINT('Ctrl Pts',(-10.0289360631668,-14.2918733204662,
4.));
#50656=CARTESIAN_POINT('Ctrl Pts',(-10.0090443370482,-14.3404713453517,
4.));
#50657=CARTESIAN_POINT('Ctrl Pts',(-9.98775201258348,-14.3885999003503,
4.));
#50658=CARTESIAN_POINT('Ctrl Pts',(-9.96509914777034,-14.4362131753606,
4.));
#50659=CARTESIAN_POINT('Ctrl Pts',(-9.95876399288502,-14.4495288188465,
4.));
#50660=CARTESIAN_POINT('Ctrl Pts',(-9.95232213153922,-14.4628045348086,
4.));
#50661=CARTESIAN_POINT('Ctrl Pts',(-9.94578145907892,-14.4760254702856,
4.));
#50662=CARTESIAN_POINT('Ctrl Pts',(-9.90302407067229,-14.562452772175,4.));
#50663=CARTESIAN_POINT('Ctrl Pts',(-9.85598091444247,-14.6466834011242,
4.));
#50664=CARTESIAN_POINT('Ctrl Pts',(-9.80499202080536,-14.7284640330205,
4.));
#50665=CARTESIAN_POINT('Ctrl Pts',(-9.75299794500559,-14.8118568676255,
4.));
#50666=CARTESIAN_POINT('Ctrl Pts',(-9.69690071688324,-14.8927029338428,
4.));
#50667=CARTESIAN_POINT('Ctrl Pts',(-9.63700597453379,-14.9707266774082,
4.));
#50668=CARTESIAN_POINT('Ctrl Pts',(-9.57663995749172,-15.049364341567,4.));
#50669=CARTESIAN_POINT('Ctrl Pts',(-9.51241597456512,-15.1251359367173,
4.));
#50670=CARTESIAN_POINT('Ctrl Pts',(-9.44459769690279,-15.1977400638646,
4.));
#50671=CARTESIAN_POINT('Ctrl Pts',(-9.40866340733751,-15.2362101904805,
4.));
#50672=CARTESIAN_POINT('Ctrl Pts',(-9.37171922385876,-15.2737906405076,
4.));
#50673=CARTESIAN_POINT('Ctrl Pts',(-9.33379951949355,-15.3104331478965,
4.));
#50674=CARTESIAN_POINT('Ctrl Pts',(-9.31851290781191,-15.3252048817713,
4.));
#50675=CARTESIAN_POINT('Ctrl Pts',(-9.30306772443973,-15.339824154646,4.));
#50676=CARTESIAN_POINT('Ctrl Pts',(-9.28746608368795,-15.3542876681649,
4.));
#50677=CARTESIAN_POINT('Ctrl Pts',(-9.27676581806402,-15.3642073579572,
4.));
#50678=CARTESIAN_POINT('Ctrl Pts',(-9.26599878272636,-15.3740474389504,
4.));
#50679=CARTESIAN_POINT('Ctrl Pts',(-9.25516737653956,-15.3838058321128,
4.));
#50680=CARTESIAN_POINT('Ctrl Pts',(-9.17938057199806,-15.452084818468,4.));
#50681=CARTESIAN_POINT('Ctrl Pts',(-9.10042438929677,-15.5163865482147,
4.));
#50682=CARTESIAN_POINT('Ctrl Pts',(-9.01862162231471,-15.5764248312756,
4.));
#50683=CARTESIAN_POINT('Ctrl Pts',(-8.93674927983158,-15.636514178546,4.));
#50684=CARTESIAN_POINT('Ctrl Pts',(-8.8520249381574,-15.6923336670045,4.));
#50685=CARTESIAN_POINT('Ctrl Pts',(-8.76472731465809,-15.7435701437727,
4.));
#50686=CARTESIAN_POINT('Ctrl Pts',(-8.67912044767158,-15.7938142864623,
4.));
#50687=CARTESIAN_POINT('Ctrl Pts',(-8.59103835537406,-15.8396519102272,
4.));
#50688=CARTESIAN_POINT('Ctrl Pts',(-8.50070999295064,-15.8807513482254,
4.));
#50689=CARTESIAN_POINT('Ctrl Pts',(-8.47449902628609,-15.8926773476613,
4.));
#50690=CARTESIAN_POINT('Ctrl Pts',(-8.44809873411205,-15.9042041128398,
4.));
#50691=CARTESIAN_POINT('Ctrl Pts',(-8.42151428132428,-15.9153228238725,
4.));
#50692=CARTESIAN_POINT('Ctrl Pts',(-8.38003054177093,-15.9326730291346,
4.));
#50693=CARTESIAN_POINT('Ctrl Pts',(-8.3380984052677,-15.9490297174903,4.));
#50694=CARTESIAN_POINT('Ctrl Pts',(-8.29574966236114,-15.9643994715412,
4.));
#50695=CARTESIAN_POINT('Ctrl Pts',(-6.7062007174672,-15.9596040105123,4.));
#50696=CARTESIAN_POINT('Ctrl Pts',(-6.61134542475377,-15.9249055207219,
4.));
#50697=CARTESIAN_POINT('Ctrl Pts',(-6.51853060534356,-15.8852234998271,
4.));
#50698=CARTESIAN_POINT('Ctrl Pts',(-6.42799851956089,-15.8408762347418,
4.));
#50699=CARTESIAN_POINT('Ctrl Pts',(-6.33621693362306,-15.7959169003098,
4.));
#50700=CARTESIAN_POINT('Ctrl Pts',(-6.24678085823289,-15.7461619565544,
4.));
#50701=CARTESIAN_POINT('Ctrl Pts',(-6.15997674190851,-15.691902411869,4.));
#50702=CARTESIAN_POINT('Ctrl Pts',(-6.13531568434349,-15.6764872701499,
4.));
#50703=CARTESIAN_POINT('Ctrl Pts',(-6.11086730231581,-15.6607083372246,
4.));
#50704=CARTESIAN_POINT('Ctrl Pts',(-6.08663877235659,-15.6445718215519,
4.));
#50705=CARTESIAN_POINT('Ctrl Pts',(-6.06744081682964,-15.6317857337964,
4.));
#50706=CARTESIAN_POINT('Ctrl Pts',(-6.0483789202221,-15.6187736030245,4.));
#50707=CARTESIAN_POINT('Ctrl Pts',(-6.02947561532874,-15.6055520498285,
4.));
#50708=CARTESIAN_POINT('Ctrl Pts',(-5.94677128184633,-15.5477060937462,
4.));
#50709=CARTESIAN_POINT('Ctrl Pts',(-5.86702045523495,-15.485803012119,4.));
#50710=CARTESIAN_POINT('Ctrl Pts',(-5.79049058680189,-15.4201377361794,
4.));
#50711=CARTESIAN_POINT('Ctrl Pts',(-5.73202513270763,-15.3699723529815,
4.));
#50712=CARTESIAN_POINT('Ctrl Pts',(-5.67544017028651,-15.3176103400047,
4.));
#50713=CARTESIAN_POINT('Ctrl Pts',(-5.62087197491949,-15.2631717733717,
4.));
#50714=CARTESIAN_POINT('Ctrl Pts',(-5.59237459351674,-15.2347420885356,
4.));
#50715=CARTESIAN_POINT('Ctrl Pts',(-5.56442750315923,-15.2057459282144,
4.));
#50716=CARTESIAN_POINT('Ctrl Pts',(-5.53705194133909,-15.1761996365986,
4.));
#50717=CARTESIAN_POINT('Ctrl Pts',(-5.52590419986363,-15.1641679412254,
4.));
#50718=CARTESIAN_POINT('Ctrl Pts',(-5.51485102559337,-15.1520446566585,
4.));
#50719=CARTESIAN_POINT('Ctrl Pts',(-5.50390395570898,-15.1398423958921,
4.));
#50720=CARTESIAN_POINT('Ctrl Pts',(-5.43813919199008,-15.0665370452716,
4.));
#50721=CARTESIAN_POINT('Ctrl Pts',(-5.37610812852687,-14.9902855415477,
4.));
#50722=CARTESIAN_POINT('Ctrl Pts',(-5.31805567958009,-14.9113640105217,
4.));
#50723=CARTESIAN_POINT('Ctrl Pts',(-5.26107088016972,-14.8338939348183,
4.));
#50724=CARTESIAN_POINT('Ctrl Pts',(-5.20791934818337,-14.7538503489036,
4.));
#50725=CARTESIAN_POINT('Ctrl Pts',(-5.15887699703074,-14.6714727381725,
4.));
#50726=CARTESIAN_POINT('Ctrl Pts',(-5.11076871641508,-14.5906641080731,
4.));
#50727=CARTESIAN_POINT('Ctrl Pts',(-5.0666142946296,-14.5076088453843,4.));
#50728=CARTESIAN_POINT('Ctrl Pts',(-5.02672179249125,-14.4225226052514,
4.));
#50729=CARTESIAN_POINT('Ctrl Pts',(-5.00642778712802,-14.3792377642152,
4.));
#50730=CARTESIAN_POINT('Ctrl Pts',(-4.98723753203067,-14.3354272137238,
4.));
#50731=CARTESIAN_POINT('Ctrl Pts',(-4.96919681035721,-14.2911191061582,
4.));
#50732=CARTESIAN_POINT('Ctrl Pts',(-4.96034382211253,-14.2693761203441,
4.));
#50733=CARTESIAN_POINT('Ctrl Pts',(-4.95176770738618,-14.2475133193776,
4.));
#50734=CARTESIAN_POINT('Ctrl Pts',(-4.94347420847157,-14.2255340469214,
4.));
#50735=CARTESIAN_POINT('Ctrl Pts',(-4.93874143956184,-14.2129913531307,
4.));
#50736=CARTESIAN_POINT('Ctrl Pts',(-4.93410201278753,-14.2004140677721,
4.));
#50737=CARTESIAN_POINT('Ctrl Pts',(-4.92955955708199,-14.1878106688628,
4.));
#50738=CARTESIAN_POINT('Ctrl Pts',(-4.89805327414987,-14.1003940207578,
4.));
#50739=CARTESIAN_POINT('Ctrl Pts',(-4.87116570943181,-14.0116107665047,
4.));
#50740=CARTESIAN_POINT('Ctrl Pts',(-4.8491500138814,-13.9216823090563,4.));
#50741=CARTESIAN_POINT('Ctrl Pts',(-4.84589778208928,-13.9083977781333,
4.));
#50742=CARTESIAN_POINT('Ctrl Pts',(-4.84275195632634,-13.8950882390595,
4.));
#50743=CARTESIAN_POINT('Ctrl Pts',(-4.8397134492654,-13.8817543903633,4.));
#50744=CARTESIAN_POINT('Ctrl Pts',(-4.81880165443801,-13.7899873802489,
4.));
#50745=CARTESIAN_POINT('Ctrl Pts',(-4.80296876416446,-13.6970686989268,
4.));
#50746=CARTESIAN_POINT('Ctrl Pts',(-4.7921064004091,-13.6033902081318,4.));
#50747=CARTESIAN_POINT('Ctrl Pts',(-4.78082403916422,-13.5060896023125,
4.));
#50748=CARTESIAN_POINT('Ctrl Pts',(-4.77490405625791,-13.4079680956598,
4.));
#50749=CARTESIAN_POINT('Ctrl Pts',(-4.77428165528829,-13.3094781487529,
4.));
#50750=CARTESIAN_POINT('Ctrl Pts',(-4.77410059584044,-13.2808269475559,
4.));
#50751=CARTESIAN_POINT('Ctrl Pts',(-4.77436819825548,-13.2521447164312,
4.));
#50752=CARTESIAN_POINT('Ctrl Pts',(-4.77508370765677,-13.2234430275403,
4.));
#50753=CARTESIAN_POINT('Ctrl Pts',(-4.77547928901581,-13.2075748180131,
4.));
#50754=CARTESIAN_POINT('Ctrl Pts',(-4.77601178481995,-13.19170066513,4.));
#50755=CARTESIAN_POINT('Ctrl Pts',(-4.77668111451686,-13.175822557735,4.));
#50756=CARTESIAN_POINT('Ctrl Pts',(-4.77726173830688,-13.1620487674244,
4.));
#50757=CARTESIAN_POINT('Ctrl Pts',(-4.77794533193815,-13.1482734031105,
4.));
#50758=CARTESIAN_POINT('Ctrl Pts',(-4.77873092865176,-13.1345098810533,
4.));
#50759=CARTESIAN_POINT('Ctrl Pts',(-4.78403323232826,-13.0416144140266,
4.));
#50760=CARTESIAN_POINT('Ctrl Pts',(-4.79398378921199,-12.9491067853577,
4.));
#50761=CARTESIAN_POINT('Ctrl Pts',(-4.8084638797429,-12.8573599583,4.));
#50762=CARTESIAN_POINT('Ctrl Pts',(-4.82290323568455,-12.7658712283383,
4.));
#50763=CARTESIAN_POINT('Ctrl Pts',(-4.84184708120934,-12.6751380809488,
4.));
#50764=CARTESIAN_POINT('Ctrl Pts',(-4.86522624014646,-12.5855474359577,
4.));
#50765=CARTESIAN_POINT('Ctrl Pts',(-4.88820176586815,-12.4975035429353,
4.));
#50766=CARTESIAN_POINT('Ctrl Pts',(-4.9154612393753,-12.4105622603287,4.));
#50767=CARTESIAN_POINT('Ctrl Pts',(-4.94697939694318,-12.3251200100783,
4.));
#50768=CARTESIAN_POINT('Ctrl Pts',(-4.96237184169077,-12.2833927894037,
4.));
#50769=CARTESIAN_POINT('Ctrl Pts',(-4.9787805689918,-12.2420236106898,4.));
#50770=CARTESIAN_POINT('Ctrl Pts',(-4.99620574112456,-12.2010620870672,
4.));
#50771=CARTESIAN_POINT('Ctrl Pts',(-5.00196784663073,-12.1875170489459,
4.));
#50772=CARTESIAN_POINT('Ctrl Pts',(-5.00784111328384,-12.1740166075363,
4.));
#50773=CARTESIAN_POINT('Ctrl Pts',(-5.01382559232837,-12.160562620369,4.));
#50774=CARTESIAN_POINT('Ctrl Pts',(-5.01951333079912,-12.1477757495608,
4.));
#50775=CARTESIAN_POINT('Ctrl Pts',(-5.02529810648898,-12.135038576554,4.));
#50776=CARTESIAN_POINT('Ctrl Pts',(-5.0311780316899,-12.1223558509962,4.));
#50777=CARTESIAN_POINT('Ctrl Pts',(-5.06862974733614,-12.0415742398394,
4.));
#50778=CARTESIAN_POINT('Ctrl Pts',(-5.10995835566621,-11.9629538753605,
4.));
#50779=CARTESIAN_POINT('Ctrl Pts',(-5.15509810659155,-11.8868432541903,
4.));
#50780=CARTESIAN_POINT('Ctrl Pts',(-5.19948167106006,-11.8120076471655,
4.));
#50781=CARTESIAN_POINT('Ctrl Pts',(-5.24755020547363,-11.739597730264,4.));
#50782=CARTESIAN_POINT('Ctrl Pts',(-5.29927754869182,-11.6699789932549,
4.));
#50783=CARTESIAN_POINT('Ctrl Pts',(-5.34947355289339,-11.6024212530347,
4.));
#50784=CARTESIAN_POINT('Ctrl Pts',(-5.40311537622297,-11.5374914288171,
4.));
#50785=CARTESIAN_POINT('Ctrl Pts',(-5.46020711675472,-11.4755639671884,
4.));
#50786=CARTESIAN_POINT('Ctrl Pts',(-5.47440621920022,-11.4601621881628,
4.));
#50787=CARTESIAN_POINT('Ctrl Pts',(-5.48881883821923,-11.4449463392586,
4.));
#50788=CARTESIAN_POINT('Ctrl Pts',(-5.50344527039708,-11.4299226339363,
4.));
#50789=CARTESIAN_POINT('Ctrl Pts',(-5.52930152881858,-11.4033640855126,
4.));
#50790=CARTESIAN_POINT('Ctrl Pts',(-5.55582596313967,-11.37740591447,4.));
#50791=CARTESIAN_POINT('Ctrl Pts',(-5.58299257280551,-11.3520616136783,
4.));
#50792=CARTESIAN_POINT('Origin',(-7.50000000000001,-12.9903810567666,14.2084234471775));
#50793=CARTESIAN_POINT('Ctrl Pts',(-10.5771720267767,-12.9888570081198,
11.7084234471775));
#50794=CARTESIAN_POINT('Ctrl Pts',(-10.5778106872988,-12.8899681384638,
11.7032843782051));
#50795=CARTESIAN_POINT('Ctrl Pts',(-10.5289895265855,-11.7846562178796,
11.6458119334487));
#50796=CARTESIAN_POINT('Ctrl Pts',(-9.19520367525283,-9.79242641580684,
11.5360061129082));
#50797=CARTESIAN_POINT('Ctrl Pts',(-5.76804697299906,-9.81262440187857,
11.3790059855559));
#50798=CARTESIAN_POINT('Ctrl Pts',(-3.89395285925593,-12.6818121943635,
11.2220058582037));
#50799=CARTESIAN_POINT('Ctrl Pts',(-5.25343392007517,-15.8279700706855,
11.0650057308514));
#50800=CARTESIAN_POINT('Ctrl Pts',(-8.62743330425189,-16.429494929522,10.9080056034992));
#50801=CARTESIAN_POINT('Ctrl Pts',(-10.4164139750736,-14.5502168635008,
10.7891448422745));
#50802=CARTESIAN_POINT('Ctrl Pts',(-10.5747255939164,-13.2672718029744,
10.7226174568339));
#50803=CARTESIAN_POINT('Ctrl Pts',(-10.5724152591149,-12.9929885813497,
10.7084234471775));
#50804=CARTESIAN_POINT('Ctrl Pts',(-10.5702205181091,-12.9936861301783,
11.7915765528225));
#50805=CARTESIAN_POINT('Ctrl Pts',(-10.5655505854978,-12.3126539838428,
11.7563842836469));
#50806=CARTESIAN_POINT('Ctrl Pts',(-10.0102062672903,-10.6096615213504,
11.6688586386871));
#50807=CARTESIAN_POINT('Ctrl Pts',(-7.21365210721562,-9.38337955935061,
11.5289996179432));
#50808=CARTESIAN_POINT('Ctrl Pts',(-4.33342685529555,-11.2379164301912,
11.371999490591));
#50809=CARTESIAN_POINT('Ctrl Pts',(-4.29152503935676,-14.6655878811314,
11.2149993632387));
#50810=CARTESIAN_POINT('Ctrl Pts',(-7.12729256983938,-16.5902267633183,
11.0579992358865));
#50811=CARTESIAN_POINT('Ctrl Pts',(-9.97678353025252,-15.4189029291823,
10.9168582990811));
#50812=CARTESIAN_POINT('Ctrl Pts',(-10.5660600868159,-13.6932623961271,
10.8280507380598));
#50813=CARTESIAN_POINT('Ctrl Pts',(-10.5715492796759,-12.9879252940133,
10.7915765528226));
#50814=CARTESIAN_POINT('Ctrl Pts',(-5.5865340033349,-11.3543938533917,12.));
#50815=CARTESIAN_POINT('Ctrl Pts',(-5.04858820392145,-11.9835803122485,
11.9476666242159));
#50816=CARTESIAN_POINT('Ctrl Pts',(-4.6501322858494,-13.8032255648209,11.8429998726477));
#50817=CARTESIAN_POINT('Ctrl Pts',(-6.60905294539631,-15.8196542318734,
11.6859997452955));
#50818=CARTESIAN_POINT('Ctrl Pts',(-9.36683654413216,-15.2923247501818,
11.5289996179432));
#50819=CARTESIAN_POINT('Ctrl Pts',(-10.4505966874647,-12.7041316569579,
11.371999490591));
#50820=CARTESIAN_POINT('Ctrl Pts',(-8.88853920691362,-10.3709404162538,
11.2149993632387));
#50821=CARTESIAN_POINT('Ctrl Pts',(-6.08135944510335,-10.3874845613442,
11.0579992358865));
#50822=CARTESIAN_POINT('Ctrl Pts',(-4.54629130410829,-12.737632688099,10.9009991085342));
#50823=CARTESIAN_POINT('Ctrl Pts',(-5.65984053808011,-15.31464666358,10.743998981182));
#50824=CARTESIAN_POINT('Ctrl Pts',(-8.42347920724065,-15.8073549219566,
10.5869988538297));
#50825=CARTESIAN_POINT('Ctrl Pts',(-10.3590248070529,-13.7741141771921,
10.4299987264775));
#50826=CARTESIAN_POINT('Ctrl Pts',(-9.73085564098287,-11.0380625363732,
10.2729985991252));
#50827=CARTESIAN_POINT('Ctrl Pts',(-7.1022567140806,-10.0526889161244,10.115998471773));
#50828=CARTESIAN_POINT('Ctrl Pts',(-4.83031806145553,-11.7015642161036,
9.9589983444207));
#50829=CARTESIAN_POINT('Ctrl Pts',(-4.95230878728804,-14.5061379301299,
9.80199821706846));
#50830=CARTESIAN_POINT('Ctrl Pts',(-7.35883867910848,-15.9515158759806,
9.64499808971619));
#50831=CARTESIAN_POINT('Ctrl Pts',(-9.89194927440413,-14.7416168632348,
9.48799796236395));
#50832=CARTESIAN_POINT('Ctrl Pts',(-10.2801760117029,-11.961367369931,9.33099783501168));
#50833=CARTESIAN_POINT('Ctrl Pts',(-8.17539224562471,-10.1038445935438,
9.17399770765945));
#50834=CARTESIAN_POINT('Ctrl Pts',(-5.46497777443614,-10.8347066168947,
9.01699758030717));
#50835=CARTESIAN_POINT('Ctrl Pts',(-4.57938725553999,-13.4985826621227,
8.85999745295493));
#50836=CARTESIAN_POINT('Ctrl Pts',(-6.31273820393898,-15.7067494160557,
8.70299732560268));
#50837=CARTESIAN_POINT('Ctrl Pts',(-9.11071819481798,-15.4791226211167,
8.54599719825042));
#50838=CARTESIAN_POINT('Ctrl Pts',(-10.4643517279258,-13.0198173800209,
8.38899707089818));
#50839=CARTESIAN_POINT('Ctrl Pts',(-9.15982262789147,-10.5341163103444,
8.23199694354591));
#50840=CARTESIAN_POINT('Ctrl Pts',(-6.3669146537774,-10.2509714005752,8.07499681619367));
#50841=CARTESIAN_POINT('Ctrl Pts',(-4.59005518003756,-12.4242814116226,
7.9179966888414));
#50842=CARTESIAN_POINT('Ctrl Pts',(-5.42257114292002,-15.1052184044673,
7.76099656148916));
#50843=CARTESIAN_POINT('Ctrl Pts',(-8.11793749226372,-15.8897604596585,
7.60399643413691));
#50844=CARTESIAN_POINT('Ctrl Pts',(-10.259193363348,-14.0744011876836,7.44699630678465));
#50845=CARTESIAN_POINT('Ctrl Pts',(-9.92625407643148,-11.286990666814,7.2899961794324));
#50846=CARTESIAN_POINT('Ctrl Pts',(-7.4176694799797,-10.0270266461848,7.13299605208014));
#50847=CARTESIAN_POINT('Ctrl Pts',(-4.98291145609725,-11.4243309624572,
6.97599592472789));
#50848=CARTESIAN_POINT('Ctrl Pts',(-4.80525086677252,-14.2259274070742,
6.81899579737564));
#50849=CARTESIAN_POINT('Ctrl Pts',(-7.04399769823543,-15.9195976158556,
6.66199567002339));
#50850=CARTESIAN_POINT('Ctrl Pts',(-9.69164612773492,-14.986611176204,6.50499554267113));
#50851=CARTESIAN_POINT('Ctrl Pts',(-10.3740245283272,-12.2635861515028,
6.34799541531888));
#50852=CARTESIAN_POINT('Ctrl Pts',(-8.47923740659063,-10.1922848677994,
6.19099528796662));
#50853=CARTESIAN_POINT('Ctrl Pts',(-5.70635901253982,-10.630063717047,6.03399516061437));
#50854=CARTESIAN_POINT('Ctrl Pts',(-4.54185510339179,-13.1843609143513,
5.87699503326211));
#50855=CARTESIAN_POINT('Ctrl Pts',(-6.02994926840226,-15.5647161841919,
5.71999490590987));
#50856=CARTESIAN_POINT('Ctrl Pts',(-8.83624974536451,-15.636637176778,5.5629947785576));
#50857=CARTESIAN_POINT('Ctrl Pts',(-10.4443267219795,-13.3356413212244,
5.40599465120536));
#50858=CARTESIAN_POINT('Ctrl Pts',(-9.41218894167164,-10.7250347470945,
5.2489945238531));
#50859=CARTESIAN_POINT('Ctrl Pts',(-6.66539009301951,-10.1458104553331,
5.09199439650085));
#50860=CARTESIAN_POINT('Ctrl Pts',(-4.66696049204361,-12.1172919418034,
4.93499426914859));
#50861=CARTESIAN_POINT('Ctrl Pts',(-5.20901007842283,-14.8717746831197,
4.77799414179635));
#50862=CARTESIAN_POINT('Ctrl Pts',(-7.80528416826264,-15.9390100206221,
4.62099401444409));
#50863=CARTESIAN_POINT('Ctrl Pts',(-10.1280577671037,-14.362540949444,4.46399388709183));
#50864=CARTESIAN_POINT('Ctrl Pts',(-10.0937360173612,-11.5549393117934,
4.30699375973958));
#50865=CARTESIAN_POINT('Ctrl Pts',(-7.73454717783886,-10.0358910717557,
4.14999363238733));
#50866=CARTESIAN_POINT('Ctrl Pts',(-5.16315103760592,-11.163440915316,3.99299350503507));
#50867=CARTESIAN_POINT('Ctrl Pts',(-4.69098959926211,-13.9347976761557,
3.83599337768283));
#50868=CARTESIAN_POINT('Ctrl Pts',(-6.05008049550027,-15.2086689018369,
3.73132662611465));
#50869=CARTESIAN_POINT('Ctrl Pts',(-6.84980000202495,-15.4224678588017,
3.67899325033057));
#50870=CARTESIAN_POINT('Ctrl Pts',(-5.44566844965787,-11.2339557355398,
12.1070022498898));
#50871=CARTESIAN_POINT('Ctrl Pts',(-4.86812015246569,-11.9094616477066,
12.0546688741057));
#50872=CARTESIAN_POINT('Ctrl Pts',(-4.44033070371531,-13.8630655577342,
11.9500021225376));
#50873=CARTESIAN_POINT('Ctrl Pts',(-6.54346319864229,-16.0279396850822,
11.7930019951853));
#50874=CARTESIAN_POINT('Ctrl Pts',(-9.50426933043305,-15.4617892577673,
11.6360018678331));
#50875=CARTESIAN_POINT('Ctrl Pts',(-10.6678137358898,-12.6830585465582,
11.4790017404808));
#50876=CARTESIAN_POINT('Ctrl Pts',(-8.99076069636001,-10.1781024161048,
11.3220016131285));
#50877=CARTESIAN_POINT('Ctrl Pts',(-5.97692195440192,-10.195864508189,11.1650014857763));
#50878=CARTESIAN_POINT('Ctrl Pts',(-4.32884515582416,-12.7190258568539,
11.008001358424));
#50879=CARTESIAN_POINT('Ctrl Pts',(-5.52437166541181,-15.4857544659485,
10.8510012310718));
#50880=CARTESIAN_POINT('Ctrl Pts',(-8.49146390624439,-16.0147349244784,
10.6940011037195));
#50881=CARTESIAN_POINT('Ctrl Pts',(-10.569500516119,-13.831811047759,10.5370009763673));
#50882=CARTESIAN_POINT('Ctrl Pts',(-9.89508678780663,-10.8943367373214,
10.380000849015));
#50883=CARTESIAN_POINT('Ctrl Pts',(-7.07297564596128,-9.83642187472128,
10.2230007216628));
#50884=CARTESIAN_POINT('Ctrl Pts',(-4.6337813970622,-11.606684088542,10.0660005943105));
#50885=CARTESIAN_POINT('Ctrl Pts',(-4.76475283703741,-14.6177249306714,
9.90900046695826));
#50886=CARTESIAN_POINT('Ctrl Pts',(-7.34844666395912,-16.1695087206656,
9.75200033960601));
#50887=CARTESIAN_POINT('Ctrl Pts',(-10.0680398135062,-14.8705393535885,
9.59500021225375));
#50888=CARTESIAN_POINT('Ctrl Pts',(-10.4848470295787,-11.8856134328399,
9.43800008490151));
#50889=CARTESIAN_POINT('Ctrl Pts',(-8.22511327688156,-9.89134353117351,
9.28099995754925));
#50890=CARTESIAN_POINT('Ctrl Pts',(-5.31516349341482,-10.6760101602818,
9.123999830197));
#50891=CARTESIAN_POINT('Ctrl Pts',(-4.36437756524938,-13.5359954516068,
8.96699970284473));
#50892=CARTESIAN_POINT('Ctrl Pts',(-6.22533435639049,-15.9067230417114,
8.80999957549251));
#50893=CARTESIAN_POINT('Ctrl Pts',(-9.22929605861391,-15.6623388157249,
8.65299944814021));
#50894=CARTESIAN_POINT('Ctrl Pts',(-10.6825813950197,-13.0219844234806,
8.495999320788));
#50895=CARTESIAN_POINT('Ctrl Pts',(-9.28201546219901,-10.3532909943549,
8.33899919343572));
#50896=CARTESIAN_POINT('Ctrl Pts',(-6.28349916850765,-10.0493015205563,
8.18199906608348));
#50897=CARTESIAN_POINT('Ctrl Pts',(-4.37583084109032,-12.3826062838239,
8.02499893873122));
#50898=CARTESIAN_POINT('Ctrl Pts',(-5.26963497019092,-15.2609085157313,
7.86799881137897));
#50899=CARTESIAN_POINT('Ctrl Pts',(-8.16342881906923,-16.1032069936549,
7.71099868402671));
#50900=CARTESIAN_POINT('Ctrl Pts',(-10.4623196804644,-14.1542045895756,
7.55399855667447));
#50901=CARTESIAN_POINT('Ctrl Pts',(-10.1048700666991,-11.1615904606817,
7.3969984293222));
#50902=CARTESIAN_POINT('Ctrl Pts',(-7.41160847115729,-9.80887039960631,
7.23999830196995));
#50903=CARTESIAN_POINT('Ctrl Pts',(-4.79760841334188,-11.3090414752098,
7.08299817461771));
#50904=CARTESIAN_POINT('Ctrl Pts',(-4.60686880545846,-14.3168858672889,
6.92599804726544));
#50905=CARTESIAN_POINT('Ctrl Pts',(-7.01042771746335,-16.1352407018342,
6.7689979199132));
#50906=CARTESIAN_POINT('Ctrl Pts',(-9.85299074832685,-15.133569659674,6.61199779256094));
#50907=CARTESIAN_POINT('Ctrl Pts',(-10.5856044869832,-12.2100809588743,
6.45499766520869));
#50908=CARTESIAN_POINT('Ctrl Pts',(-8.55132691312017,-9.98629460218332,
6.29799753785643));
#50909=CARTESIAN_POINT('Ctrl Pts',(-5.57431473726304,-10.4563018579429,
6.14099741050418));
#50910=CARTESIAN_POINT('Ctrl Pts',(-4.32408237085103,-13.1986413249196,
5.98399728315193));
#50911=CARTESIAN_POINT('Ctrl Pts',(-5.92172706293806,-15.75423360635,5.82699715579966));
#50912=CARTESIAN_POINT('Ctrl Pts',(-8.9346217888498,-15.831449279092,5.66999702844743));
#50913=CARTESIAN_POINT('Ctrl Pts',(-10.6610821880398,-13.3610586938876,
5.51299690109516));
#50914=CARTESIAN_POINT('Ctrl Pts',(-9.55296048110486,-10.558264465972,5.35599677374292));
#50915=CARTESIAN_POINT('Ctrl Pts',(-6.60394777480949,-9.93639883608159,
5.19899664639066));
#50916=CARTESIAN_POINT('Ctrl Pts',(-4.45839776891566,-12.0530168609799,
5.04199651903841));
#50917=CARTESIAN_POINT('Ctrl Pts',(-5.04035196569236,-15.0102791328056,
4.88499639168615));
#50918=CARTESIAN_POINT('Ctrl Pts',(-7.82775858038497,-16.1560822091562,
4.72799626433391));
#50919=CARTESIAN_POINT('Ctrl Pts',(-10.3215301429408,-14.4635566264157,
4.57099613698164));
#50920=CARTESIAN_POINT('Ctrl Pts',(-10.2846816943758,-11.4492649509585,
4.4139960096294));
#50921=CARTESIAN_POINT('Ctrl Pts',(-7.75181407368507,-9.81838740652354,
4.25699588227714));
#50922=CARTESIAN_POINT('Ctrl Pts',(-4.99111687367461,-11.0289452226782,
4.09999575492489));
#50923=CARTESIAN_POINT('Ctrl Pts',(-4.48419585112438,-14.0043237457194,
3.94299562757263));
#50924=CARTESIAN_POINT('Ctrl Pts',(-5.94334031085918,-15.3719748325696,
3.83832887600446));
#50925=CARTESIAN_POINT('Ctrl Pts',(-6.80193357383903,-15.6015132427052,
3.78599550022038));
#50926=CARTESIAN_POINT('Ctrl Pts',(-5.30480289598084,-11.1135176176879,
12.2140044997796));
#50927=CARTESIAN_POINT('Ctrl Pts',(-4.68765210100992,-11.8353429831648,
12.1616711239955));
#50928=CARTESIAN_POINT('Ctrl Pts',(-4.23052912158122,-13.9229055506476,
12.0570043724274));
#50929=CARTESIAN_POINT('Ctrl Pts',(-6.47787345188828,-16.2362251382909,
11.9000042450751));
#50930=CARTESIAN_POINT('Ctrl Pts',(-9.64170211673396,-15.6312537653527,
11.7430041177229));
#50931=CARTESIAN_POINT('Ctrl Pts',(-10.8850307843148,-12.6619854361585,
11.5860039903706));
#50932=CARTESIAN_POINT('Ctrl Pts',(-9.09298218580643,-9.98526441595581,
11.4290038630183));
#50933=CARTESIAN_POINT('Ctrl Pts',(-5.87248446370049,-10.0042444550338,
11.2720037356661));
#50934=CARTESIAN_POINT('Ctrl Pts',(-4.11139900754004,-12.7004190256087,
11.1150036083138));
#50935=CARTESIAN_POINT('Ctrl Pts',(-5.3889027927435,-15.656862268317,10.9580034809616));
#50936=CARTESIAN_POINT('Ctrl Pts',(-8.55944860524813,-16.2221149270002,
10.8010033536093));
#50937=CARTESIAN_POINT('Ctrl Pts',(-10.7799762251851,-13.889507918326,10.6440032262571));
#50938=CARTESIAN_POINT('Ctrl Pts',(-10.0593179346304,-10.7506109382696,
10.4870030989048));
#50939=CARTESIAN_POINT('Ctrl Pts',(-7.04369457784195,-9.62015483331818,
10.3300029715526));
#50940=CARTESIAN_POINT('Ctrl Pts',(-4.43724473266885,-11.5118039609805,
10.1730028442003));
#50941=CARTESIAN_POINT('Ctrl Pts',(-4.57719688678678,-14.7293119312129,
10.0160027168481));
#50942=CARTESIAN_POINT('Ctrl Pts',(-7.33805464880973,-16.3875015653505,
9.85900258949582));
#50943=CARTESIAN_POINT('Ctrl Pts',(-10.2441303526083,-14.9994618439422,
9.70200246214357));
#50944=CARTESIAN_POINT('Ctrl Pts',(-10.6895180474545,-11.8098594957488,
9.5450023347913));
#50945=CARTESIAN_POINT('Ctrl Pts',(-8.2748343081384,-9.6788424688032,9.38800220743907));
#50946=CARTESIAN_POINT('Ctrl Pts',(-5.1653492123935,-10.517313703669,9.2310020800868));
#50947=CARTESIAN_POINT('Ctrl Pts',(-4.14936787495879,-13.5734082410908,
9.07400195273456));
#50948=CARTESIAN_POINT('Ctrl Pts',(-6.137930508842,-16.1066966673671,8.9170018253823));
#50949=CARTESIAN_POINT('Ctrl Pts',(-9.34787392240984,-15.8455550103332,
8.76000169803005));
#50950=CARTESIAN_POINT('Ctrl Pts',(-10.9008110621136,-13.0241514669403,
8.60300157067779));
#50951=CARTESIAN_POINT('Ctrl Pts',(-9.40420829650654,-10.1724656783654,
8.44600144332554));
#50952=CARTESIAN_POINT('Ctrl Pts',(-6.20008368323791,-9.84763164053746,
8.28900131597328));
#50953=CARTESIAN_POINT('Ctrl Pts',(-4.16160650214306,-12.3409311560251,
8.13200118862103));
#50954=CARTESIAN_POINT('Ctrl Pts',(-5.11669879746183,-15.4165986269953,
7.97500106126878));
#50955=CARTESIAN_POINT('Ctrl Pts',(-8.20892014587475,-16.3166535276513,
7.81800093391653));
#50956=CARTESIAN_POINT('Ctrl Pts',(-10.6654459975808,-14.2340079914677,
7.66100080656427));
#50957=CARTESIAN_POINT('Ctrl Pts',(-10.2834860569666,-11.0361902545495,
7.50400067921202));
#50958=CARTESIAN_POINT('Ctrl Pts',(-7.40554746233487,-9.59071415302789,
7.34700055185976));
#50959=CARTESIAN_POINT('Ctrl Pts',(-4.61230537058651,-11.1937519879624,
7.19000042450751));
#50960=CARTESIAN_POINT('Ctrl Pts',(-4.40848674414439,-14.4078443275035,
7.03300029715526));
#50961=CARTESIAN_POINT('Ctrl Pts',(-6.97685773669127,-16.3508837878128,
6.876000169803));
#50962=CARTESIAN_POINT('Ctrl Pts',(-10.0143353689188,-15.280528143144,6.71900004245075));
#50963=CARTESIAN_POINT('Ctrl Pts',(-10.7971844456393,-12.1565757662458,
6.5619999150985));
#50964=CARTESIAN_POINT('Ctrl Pts',(-8.62341641964973,-9.78030433656719,
6.40499978774624));
#50965=CARTESIAN_POINT('Ctrl Pts',(-5.44227046198626,-10.2825399988388,
6.24799966039399));
#50966=CARTESIAN_POINT('Ctrl Pts',(-4.10630963831026,-13.2129217354879,
6.09099953304174));
#50967=CARTESIAN_POINT('Ctrl Pts',(-5.81350485747386,-15.943751028508,5.93399940568949));
#50968=CARTESIAN_POINT('Ctrl Pts',(-9.0329938323351,-16.026261381406,5.77699927833723));
#50969=CARTESIAN_POINT('Ctrl Pts',(-10.8778376541001,-13.3864760665508,
5.61999915098497));
#50970=CARTESIAN_POINT('Ctrl Pts',(-9.69373202053811,-10.3914941848495,
5.46299902363273));
#50971=CARTESIAN_POINT('Ctrl Pts',(-6.54250545659946,-9.72698721683007,
5.30599889628047));
#50972=CARTESIAN_POINT('Ctrl Pts',(-4.24983504578773,-11.9887417801564,
5.14899876892822));
#50973=CARTESIAN_POINT('Ctrl Pts',(-4.87169385296189,-15.1487835824914,
4.99199864157596));
#50974=CARTESIAN_POINT('Ctrl Pts',(-7.85023299250732,-16.3731543976903,
4.83499851422371));
#50975=CARTESIAN_POINT('Ctrl Pts',(-10.5150025187778,-14.5645723033874,
4.67799838687146));
#50976=CARTESIAN_POINT('Ctrl Pts',(-10.4756273713904,-11.3435905901237,
4.5209982595192));
#50977=CARTESIAN_POINT('Ctrl Pts',(-7.76908096953125,-9.60088374129137,
4.36399813216695));
#50978=CARTESIAN_POINT('Ctrl Pts',(-4.81908270974332,-10.8944495300405,
4.2069980048147));
#50979=CARTESIAN_POINT('Ctrl Pts',(-4.27740210298664,-14.0738498152832,
4.04999787746244));
#50980=CARTESIAN_POINT('Ctrl Pts',(-5.83660012621808,-15.5352807633023,
3.94533112589427));
#50981=CARTESIAN_POINT('Ctrl Pts',(-6.75406714565312,-15.7805586266087,
3.89299775011019));
#50982=CARTESIAN_POINT('Ctrl Pts',(-5.1639373423038,-10.993079499836,12.3210067496694));
#50983=CARTESIAN_POINT('Ctrl Pts',(-4.50718404955416,-11.761224318623,12.2686733738853));
#50984=CARTESIAN_POINT('Ctrl Pts',(-4.02072753944713,-13.9827455435609,
12.1640066223172));
#50985=CARTESIAN_POINT('Ctrl Pts',(-6.41228370513427,-16.4445105914997,
12.0070064949649));
#50986=CARTESIAN_POINT('Ctrl Pts',(-9.77913490303484,-15.8007182729381,
11.8500063676127));
#50987=CARTESIAN_POINT('Ctrl Pts',(-11.1022478327399,-12.6409123257588,
11.6930062402604));
#50988=CARTESIAN_POINT('Ctrl Pts',(-9.19520367525283,-9.79242641580684,
11.5360061129082));
#50989=CARTESIAN_POINT('Ctrl Pts',(-5.76804697299906,-9.81262440187857,
11.3790059855559));
#50990=CARTESIAN_POINT('Ctrl Pts',(-3.89395285925593,-12.6818121943635,
11.2220058582037));
#50991=CARTESIAN_POINT('Ctrl Pts',(-5.25343392007517,-15.8279700706855,
11.0650057308514));
#50992=CARTESIAN_POINT('Ctrl Pts',(-8.62743330425189,-16.429494929522,10.9080056034992));
#50993=CARTESIAN_POINT('Ctrl Pts',(-10.9904519342511,-13.9472047888929,
10.7510054761469));
#50994=CARTESIAN_POINT('Ctrl Pts',(-10.2235490814542,-10.6068851392178,
10.5940053487946));
#50995=CARTESIAN_POINT('Ctrl Pts',(-7.01441350972263,-9.40388779191504,
10.4370052214424));
#50996=CARTESIAN_POINT('Ctrl Pts',(-4.2407080682755,-11.4169238334189,10.2800050940901));
#50997=CARTESIAN_POINT('Ctrl Pts',(-4.38964093653616,-14.8408989317544,
10.1230049667379));
#50998=CARTESIAN_POINT('Ctrl Pts',(-7.32766263366035,-16.6054944100355,
9.96600483938563));
#50999=CARTESIAN_POINT('Ctrl Pts',(-10.4202208917104,-15.1283843342959,
9.80900471203338));
#51000=CARTESIAN_POINT('Ctrl Pts',(-10.8941890653303,-11.7341055586577,
9.65200458468112));
#51001=CARTESIAN_POINT('Ctrl Pts',(-8.32455533939524,-9.46634140643289,
9.49500445732887));
#51002=CARTESIAN_POINT('Ctrl Pts',(-5.01553493137219,-10.3586172470561,
9.33800432997662));
#51003=CARTESIAN_POINT('Ctrl Pts',(-3.93435818466818,-13.6108210305748,
9.18100420262436));
#51004=CARTESIAN_POINT('Ctrl Pts',(-6.05052666129351,-16.3066702930228,
9.02400407527212));
#51005=CARTESIAN_POINT('Ctrl Pts',(-9.46645178620579,-16.0287712049414,
8.86700394791984));
#51006=CARTESIAN_POINT('Ctrl Pts',(-11.1190407292075,-13.0263185104,8.71000382056762));
#51007=CARTESIAN_POINT('Ctrl Pts',(-9.52640113081409,-9.99164036237588,
8.55300369321534));
#51008=CARTESIAN_POINT('Ctrl Pts',(-6.11666819796815,-9.64596176051859,
8.3960035658631));
#51009=CARTESIAN_POINT('Ctrl Pts',(-3.94738216319582,-12.2992560282264,
8.23900343851084));
#51010=CARTESIAN_POINT('Ctrl Pts',(-4.96376262473273,-15.5722887382593,
8.0820033111586));
#51011=CARTESIAN_POINT('Ctrl Pts',(-8.25441147268027,-16.5301000616477,
7.92500318380633));
#51012=CARTESIAN_POINT('Ctrl Pts',(-10.8685723146971,-14.3138113933598,
7.76800305645408));
#51013=CARTESIAN_POINT('Ctrl Pts',(-10.4621020472342,-10.9107900484173,
7.61100292910183));
#51014=CARTESIAN_POINT('Ctrl Pts',(-7.39948645351245,-9.37255790644949,
7.45400280174957));
#51015=CARTESIAN_POINT('Ctrl Pts',(-4.42700232783115,-11.078462500715,7.29700267439732));
#51016=CARTESIAN_POINT('Ctrl Pts',(-4.21010468283033,-14.4988027877182,
7.14000254704507));
#51017=CARTESIAN_POINT('Ctrl Pts',(-6.94328775591919,-16.5665268737914,
6.98300241969282));
#51018=CARTESIAN_POINT('Ctrl Pts',(-10.1756799895107,-15.427486626614,6.82600229234056));
#51019=CARTESIAN_POINT('Ctrl Pts',(-11.0087644042953,-12.1030705736173,
6.66900216498831));
#51020=CARTESIAN_POINT('Ctrl Pts',(-8.69550592617927,-9.57431407095109,
6.51200203763606));
#51021=CARTESIAN_POINT('Ctrl Pts',(-5.31022618670948,-10.1087781397346,
6.3550019102838));
#51022=CARTESIAN_POINT('Ctrl Pts',(-3.88853690576949,-13.2272021460562,
6.19800178293155));
#51023=CARTESIAN_POINT('Ctrl Pts',(-5.70528265200966,-16.133268450666,6.0410016555793));
#51024=CARTESIAN_POINT('Ctrl Pts',(-9.13136587582039,-16.22107348372,5.88400152822704));
#51025=CARTESIAN_POINT('Ctrl Pts',(-11.0945931201605,-13.4118934392139,
5.72700140087479));
#51026=CARTESIAN_POINT('Ctrl Pts',(-9.83450355997132,-10.224723903727,5.57000127352253));
#51027=CARTESIAN_POINT('Ctrl Pts',(-6.48106313838945,-9.51757559757857,
5.41300114617028));
#51028=CARTESIAN_POINT('Ctrl Pts',(-4.04127232265978,-11.9244666993329,
5.25600101881803));
#51029=CARTESIAN_POINT('Ctrl Pts',(-4.70303574023142,-15.2872880321773,
5.09900089146577));
#51030=CARTESIAN_POINT('Ctrl Pts',(-7.87270740462966,-16.5902265862243,
4.94200076411352));
#51031=CARTESIAN_POINT('Ctrl Pts',(-10.7084748946149,-14.6655879803591,
4.78500063676127));
#51032=CARTESIAN_POINT('Ctrl Pts',(-10.666573048405,-11.2379162292888,4.62800050940902));
#51033=CARTESIAN_POINT('Ctrl Pts',(-7.78634786537746,-9.38338007605921,
4.47100038205676));
#51034=CARTESIAN_POINT('Ctrl Pts',(-4.64704854581202,-10.7599538374027,
4.31400025470451));
#51035=CARTESIAN_POINT('Ctrl Pts',(-4.0706083548489,-14.143375884847,4.15700012735225));
#51036=CARTESIAN_POINT('Ctrl Pts',(-5.72985994157699,-15.6985866940351,
4.05233337578409));
#51037=CARTESIAN_POINT('Ctrl Pts',(-6.7062007174672,-15.9596040105123,4.));
#51038=CARTESIAN_POINT('Ctrl Pts',(-5.5865340033349,-11.3543938533917,12.));
#51039=CARTESIAN_POINT('Ctrl Pts',(-5.52489675159201,-11.412317734857,12.));
#51040=CARTESIAN_POINT('Ctrl Pts',(-5.46662466733851,-11.4733903391465,
12.));
#51041=CARTESIAN_POINT('Ctrl Pts',(-5.41171731080853,-11.5372273647712,
12.));
#51042=CARTESIAN_POINT('Ctrl Pts',(-5.35535954826471,-11.6027506782036,
12.));
#51043=CARTESIAN_POINT('Ctrl Pts',(-5.30254618320446,-11.6711868211063,
12.));
#51044=CARTESIAN_POINT('Ctrl Pts',(-5.25330217107373,-11.7421687765855,
12.));
#51045=CARTESIAN_POINT('Ctrl Pts',(-5.20312956815832,-11.8144892336791,
12.));
#51046=CARTESIAN_POINT('Ctrl Pts',(-5.1566617252503,-11.8894530177238,12.));
#51047=CARTESIAN_POINT('Ctrl Pts',(-5.11395808422126,-11.9667137220828,
12.));
#51048=CARTESIAN_POINT('Ctrl Pts',(-5.09461562078295,-12.0017086853522,
12.));
#51049=CARTESIAN_POINT('Ctrl Pts',(-5.07604591099636,-12.0371753912937,
12.));
#51050=CARTESIAN_POINT('Ctrl Pts',(-5.05825705836343,-12.0730838611618,
12.));
#51051=CARTESIAN_POINT('Ctrl Pts',(-5.04815218455416,-12.093481498052,12.));
#51052=CARTESIAN_POINT('Ctrl Pts',(-5.03829930483427,-12.1140217037901,
12.));
#51053=CARTESIAN_POINT('Ctrl Pts',(-5.02870015601257,-12.1346991425122,
12.));
#51054=CARTESIAN_POINT('Ctrl Pts',(-5.02048318017586,-12.1523992550431,
12.));
#51055=CARTESIAN_POINT('Ctrl Pts',(-5.01244999988763,-12.1702050672847,
12.));
#51056=CARTESIAN_POINT('Ctrl Pts',(-5.00461448908043,-12.1880835326347,
12.));
#51057=CARTESIAN_POINT('Ctrl Pts',(-4.96800851502513,-12.2716082261557,
12.));
#51058=CARTESIAN_POINT('Ctrl Pts',(-4.93566438777708,-12.3568162975634,
12.));
#51059=CARTESIAN_POINT('Ctrl Pts',(-4.9076092477584,-12.4433098844385,12.));
#51060=CARTESIAN_POINT('Ctrl Pts',(-4.87909470826589,-12.531219793181,12.));
#51061=CARTESIAN_POINT('Ctrl Pts',(-4.85501027288513,-12.6204584164563,
12.));
#51062=CARTESIAN_POINT('Ctrl Pts',(-4.83542346103633,-12.7106451238744,
12.));
#51063=CARTESIAN_POINT('Ctrl Pts',(-4.81671890332471,-12.7967695266993,
12.));
#51064=CARTESIAN_POINT('Ctrl Pts',(-4.80211587003395,-12.8837594508039,
12.));
#51065=CARTESIAN_POINT('Ctrl Pts',(-4.79171175017421,-12.9713041908118,
12.));
#51066=CARTESIAN_POINT('Ctrl Pts',(-4.7871219669274,-13.0099246014234,12.));
#51067=CARTESIAN_POINT('Ctrl Pts',(-4.78334987321312,-13.0486531860177,
12.));
#51068=CARTESIAN_POINT('Ctrl Pts',(-4.78040642509842,-13.0874639619222,
12.));
#51069=CARTESIAN_POINT('Ctrl Pts',(-4.7790340847621,-13.1055589278201,12.));
#51070=CARTESIAN_POINT('Ctrl Pts',(-4.77784189531648,-13.1236717640034,
12.));
#51071=CARTESIAN_POINT('Ctrl Pts',(-4.77683109303951,-13.1417998520234,
12.));
#51072=CARTESIAN_POINT('Ctrl Pts',(-4.7758570840318,-13.1592680764492,12.));
#51073=CARTESIAN_POINT('Ctrl Pts',(-4.77505149943043,-13.1767532882224,
12.));
#51074=CARTESIAN_POINT('Ctrl Pts',(-4.77441609878784,-13.1942285673893,
12.));
#51075=CARTESIAN_POINT('Ctrl Pts',(-4.77095265346117,-13.2894829154418,
12.));
#51076=CARTESIAN_POINT('Ctrl Pts',(-4.77253183089421,-13.3845892743107,
12.));
#51077=CARTESIAN_POINT('Ctrl Pts',(-4.77921580433521,-13.4791489989792,
12.));
#51078=CARTESIAN_POINT('Ctrl Pts',(-4.78586481725455,-13.5732141290278,
12.));
#51079=CARTESIAN_POINT('Ctrl Pts',(-4.79756501411883,-13.6667392834721,
12.));
#51080=CARTESIAN_POINT('Ctrl Pts',(-4.81442558423848,-13.7593498298833,
12.));
#51081=CARTESIAN_POINT('Ctrl Pts',(-4.830924328857,-13.8499729667865,12.));
#51082=CARTESIAN_POINT('Ctrl Pts',(-4.85236399681968,-13.9397212614334,
12.));
#51083=CARTESIAN_POINT('Ctrl Pts',(-4.87847000308199,-14.0283529813775,
12.));
#51084=CARTESIAN_POINT('Ctrl Pts',(-4.89379441408366,-14.0803804301784,
12.));
#51085=CARTESIAN_POINT('Ctrl Pts',(-4.91072775850773,-14.1320231162836,
12.));
#51086=CARTESIAN_POINT('Ctrl Pts',(-4.92922261500886,-14.1832309956159,
12.));
#51087=CARTESIAN_POINT('Ctrl Pts',(-4.93398351814407,-14.1964128093404,
12.));
#51088=CARTESIAN_POINT('Ctrl Pts',(-4.93884875001307,-14.2095679810762,
12.));
#51089=CARTESIAN_POINT('Ctrl Pts',(-4.94381485137731,-14.2226885070165,
12.));
#51090=CARTESIAN_POINT('Ctrl Pts',(-4.97686325186981,-14.310002954335,12.));
#51091=CARTESIAN_POINT('Ctrl Pts',(-5.01429440116268,-14.3955759829307,
12.));
#51092=CARTESIAN_POINT('Ctrl Pts',(-5.05577732713123,-14.4791717978631,
12.));
#51093=CARTESIAN_POINT('Ctrl Pts',(-5.09882663969929,-14.5659241732654,
12.));
#51094=CARTESIAN_POINT('Ctrl Pts',(-5.1462396027634,-14.6505479156747,12.));
#51095=CARTESIAN_POINT('Ctrl Pts',(-5.19770241499811,-14.7327775666312,
12.));
#51096=CARTESIAN_POINT('Ctrl Pts',(-5.24979009521262,-14.8160056604173,
12.));
#51097=CARTESIAN_POINT('Ctrl Pts',(-5.30602696260126,-14.8967819927061,
12.));
#51098=CARTESIAN_POINT('Ctrl Pts',(-5.36613986514052,-14.9748175661494,
12.));
#51099=CARTESIAN_POINT('Ctrl Pts',(-5.40561376259492,-15.0260606120477,
12.));
#51100=CARTESIAN_POINT('Ctrl Pts',(-5.44676008901899,-15.076121523717,12.));
#51101=CARTESIAN_POINT('Ctrl Pts',(-5.48951221838806,-15.1249126475777,
12.));
#51102=CARTESIAN_POINT('Ctrl Pts',(-5.50097170290556,-15.1379908529612,
12.));
#51103=CARTESIAN_POINT('Ctrl Pts',(-5.51254660460158,-15.1509777948558,
12.));
#51104=CARTESIAN_POINT('Ctrl Pts',(-5.52423573327417,-15.1638717111488,
12.));
#51105=CARTESIAN_POINT('Ctrl Pts',(-5.5353884173992,-15.1761738920537,12.));
#51106=CARTESIAN_POINT('Ctrl Pts',(-5.54663940936984,-15.1883850930378,
12.));
#51107=CARTESIAN_POINT('Ctrl Pts',(-5.55798428070717,-15.2005008010861,
12.));
#51108=CARTESIAN_POINT('Ctrl Pts',(-5.62980603833238,-15.2772025477193,
12.));
#51109=CARTESIAN_POINT('Ctrl Pts',(-5.70542358612169,-15.3501207786779,
12.));
#51110=CARTESIAN_POINT('Ctrl Pts',(-5.7844933991545,-15.4189223872958,12.));
#51111=CARTESIAN_POINT('Ctrl Pts',(-5.8437957589291,-15.4705235937591,12.));
#51112=CARTESIAN_POINT('Ctrl Pts',(-5.90504133108183,-15.519808942512,12.));
#51113=CARTESIAN_POINT('Ctrl Pts',(-5.968104244788,-15.5666263507592,12.));
#51114=CARTESIAN_POINT('Ctrl Pts',(-5.99074690383604,-15.5834360817113,
12.));
#51115=CARTESIAN_POINT('Ctrl Pts',(-6.01362398614045,-15.5999275418789,
12.));
#51116=CARTESIAN_POINT('Ctrl Pts',(-6.03673011024537,-15.6160932756601,
12.));
#51117=CARTESIAN_POINT('Ctrl Pts',(-6.05604444624562,-15.6296061613575,
12.));
#51118=CARTESIAN_POINT('Ctrl Pts',(-6.07552135620629,-15.6428929845117,
12.));
#51119=CARTESIAN_POINT('Ctrl Pts',(-6.09513705214722,-15.655935902686,12.));
#51120=CARTESIAN_POINT('Ctrl Pts',(-6.1801078936968,-15.7124349296322,12.));
#51121=CARTESIAN_POINT('Ctrl Pts',(-6.26775546621735,-15.7644144018326,
12.));
#51122=CARTESIAN_POINT('Ctrl Pts',(-6.3577924589883,-15.8115622787044,12.));
#51123=CARTESIAN_POINT('Ctrl Pts',(-6.42986829724945,-15.8493047958986,
12.));
#51124=CARTESIAN_POINT('Ctrl Pts',(-6.50347629812978,-15.8839507974289,
12.));
#51125=CARTESIAN_POINT('Ctrl Pts',(-6.57848586659695,-15.9153228867674,
12.));
#51126=CARTESIAN_POINT('Ctrl Pts',(-6.61998922672564,-15.9326813004793,
12.));
#51127=CARTESIAN_POINT('Ctrl Pts',(-6.66192191928759,-15.9490371078547,
12.));
#51128=CARTESIAN_POINT('Ctrl Pts',(-6.70425049788235,-15.9643995452955,
12.));
#51129=CARTESIAN_POINT('Ctrl Pts',(-10.0166114900998,-12.9925168768863,
10.387416697508));
#51130=CARTESIAN_POINT('Ctrl Pts',(-10.0185038824417,-13.21718192014,10.4016107071645));
#51131=CARTESIAN_POINT('Ctrl Pts',(-9.99083741615502,-13.441388813634,10.415804716821));
#51132=CARTESIAN_POINT('Ctrl Pts',(-9.93173901273922,-13.6569790278497,
10.4299987264775));
#51133=CARTESIAN_POINT('Ctrl Pts',(-9.71384294044885,-14.4518610921136,
10.4823321022616));
#51134=CARTESIAN_POINT('Ctrl Pts',(-9.06866107384475,-15.1296080070351,
10.5346654780456));
#51135=CARTESIAN_POINT('Ctrl Pts',(-8.28546369568261,-15.3863634214331,
10.5869988538297));
#51136=CARTESIAN_POINT('Ctrl Pts',(-7.50226631752047,-15.6431188358311,
10.6393322296138));
#51137=CARTESIAN_POINT('Ctrl Pts',(-6.58105342780029,-15.4788827497055,
10.6916656053979));
#51138=CARTESIAN_POINT('Ctrl Pts',(-5.9348554439449,-14.9672623773959,10.743998981182));
#51139=CARTESIAN_POINT('Ctrl Pts',(-5.2886574600895,-14.4556420050863,10.7963323569661));
#51140=CARTESIAN_POINT('Ctrl Pts',(-4.91747438209889,-13.5966373465927,
10.8486657327501));
#51141=CARTESIAN_POINT('Ctrl Pts',(-4.98772753326943,-12.7754436628867,
10.9009991085342));
#51142=CARTESIAN_POINT('Ctrl Pts',(-5.05798068443997,-11.9542499791808,
10.9533324843183));
#51143=CARTESIAN_POINT('Ctrl Pts',(-5.56967006477166,-11.1708672702625,
11.0056658601024));
#51144=CARTESIAN_POINT('Ctrl Pts',(-6.29337804857255,-10.7764185582883,
11.0579992358865));
#51145=CARTESIAN_POINT('Ctrl Pts',(-7.01708603237344,-10.3819698463141,
11.1103326116706));
#51146=CARTESIAN_POINT('Ctrl Pts',(-7.95281261964353,-10.3764551312839,
11.1626659874547));
#51147=CARTESIAN_POINT('Ctrl Pts',(-8.68101882670376,-10.7625629805529,
11.2149993632387));
#51148=CARTESIAN_POINT('Ctrl Pts',(-9.40922503376398,-11.1486708298218,
11.2673327390228));
#51149=CARTESIAN_POINT('Ctrl Pts',(-9.92991086061434,-11.9264012433898,
11.3196661148069));
#51150=CARTESIAN_POINT('Ctrl Pts',(-10.0096270834841,-12.7466319657112,
11.371999490591));
#51151=CARTESIAN_POINT('Ctrl Pts',(-10.0174551121829,-12.8271775485652,
11.3771385595633));
#51152=CARTESIAN_POINT('Ctrl Pts',(-10.0210308785667,-12.9081329611663,
11.3822776285357));
#51153=CARTESIAN_POINT('Ctrl Pts',(-10.0205077525331,-12.989132710429,11.387416697508));
#51154=CARTESIAN_POINT('Ctrl Pts',(-8.29379928253297,-15.9596040105122,
12.));
#51155=CARTESIAN_POINT('Ctrl Pts',(-9.27014005842316,-15.698586694035,11.9476666242159));
#51156=CARTESIAN_POINT('Ctrl Pts',(-10.9293914260692,-14.1433745388278,
11.8429998726477));
#51157=CARTESIAN_POINT('Ctrl Pts',(-10.3529516457367,-10.7599545073216,
11.6859997452955));
#51158=CARTESIAN_POINT('Ctrl Pts',(-7.21365210721562,-9.38337955935061,
11.5289996179432));
#51159=CARTESIAN_POINT('Ctrl Pts',(-4.33342685529555,-11.2379164301912,
11.371999490591));
#51160=CARTESIAN_POINT('Ctrl Pts',(-4.29152503935676,-14.6655878811314,
11.2149993632387));
#51161=CARTESIAN_POINT('Ctrl Pts',(-7.12729256983938,-16.5902267633183,
11.0579992358865));
#51162=CARTESIAN_POINT('Ctrl Pts',(-10.296964344732,-15.2872880462285,10.9009991085342));
#51163=CARTESIAN_POINT('Ctrl Pts',(-10.9587277612158,-11.9244666973206,
10.743998981182));
#51164=CARTESIAN_POINT('Ctrl Pts',(-8.51893689306524,-9.51757549146244,
10.5869988538297));
#51165=CARTESIAN_POINT('Ctrl Pts',(-5.16549637569413,-10.2247238388162,
10.4299987264775));
#51166=CARTESIAN_POINT('Ctrl Pts',(-3.90540678666615,-13.4118934459175,
10.2729985991252));
#51167=CARTESIAN_POINT('Ctrl Pts',(-5.86863408021139,-16.2210735713392,
10.115998471773));
#51168=CARTESIAN_POINT('Ctrl Pts',(-9.29471739586239,-16.133268532241,9.9589983444207));
#51169=CARTESIAN_POINT('Ctrl Pts',(-11.1114631891741,-13.227202153015,9.80199821706844));
#51170=CARTESIAN_POINT('Ctrl Pts',(-9.68977387121298,-10.1087780633504,
9.64499808971621));
#51171=CARTESIAN_POINT('Ctrl Pts',(-6.30449404219616,-9.57431398106461,
9.48799796236394));
#51172=CARTESIAN_POINT('Ctrl Pts',(-3.99123550321764,-12.1030705501041,
9.33099783501171));
#51173=CARTESIAN_POINT('Ctrl Pts',(-4.82431993989319,-15.4274866909495,
9.17399770765942));
#51174=CARTESIAN_POINT('Ctrl Pts',(-8.05671225877921,-16.5665269680756,
9.0169975803072));
#51175=CARTESIAN_POINT('Ctrl Pts',(-10.789895403928,-14.4988028275178,8.85999745295491));
#51176=CARTESIAN_POINT('Ctrl Pts',(-10.5729977532197,-11.0784624502813,
8.70299732560269));
#51177=CARTESIAN_POINT('Ctrl Pts',(-7.60051354913579,-9.37255781103892,
8.54599719825042));
#51178=CARTESIAN_POINT('Ctrl Pts',(-4.53789787464541,-10.9107899935683,
8.38899707089818));
#51179=CARTESIAN_POINT('Ctrl Pts',(-4.13142759646044,-14.3138114282651,
8.23199694354591));
#51180=CARTESIAN_POINT('Ctrl Pts',(-6.74558850742372,-16.5301001550025,
8.07499681619368));
#51181=CARTESIAN_POINT('Ctrl Pts',(-10.0362374421571,-15.5722888063543,
7.9179966888414));
#51182=CARTESIAN_POINT('Ctrl Pts',(-11.0526179305001,-12.2992560099981,
7.76099656148917));
#51183=CARTESIAN_POINT('Ctrl Pts',(-8.88333183851511,-9.64596167231467,
7.60399643413689));
#51184=CARTESIAN_POINT('Ctrl Pts',(-5.47359881574229,-9.99164028328652,
7.44699630678467));
#51185=CARTESIAN_POINT('Ctrl Pts',(-3.88095917534459,-13.0263185113509,
7.28999617943238));
#51186=CARTESIAN_POINT('Ctrl Pts',(-5.53354816193247,-16.0287712850697,
7.13299605208016));
#51187=CARTESIAN_POINT('Ctrl Pts',(-8.94947337693327,-16.3066703804957,
6.97599592472788));
#51188=CARTESIAN_POINT('Ctrl Pts',(-11.0656419093738,-13.610821046919,6.81899579737565));
#51189=CARTESIAN_POINT('Ctrl Pts',(-9.98446513414696,-10.3586171776818,
6.66199567002337));
#51190=CARTESIAN_POINT('Ctrl Pts',(-6.67544463886838,-9.46634131342536,
6.50499554267114));
#51191=CARTESIAN_POINT('Ctrl Pts',(-4.10581084513197,-11.7341055256468,
6.34799541531887));
#51192=CARTESIAN_POINT('Ctrl Pts',(-4.57977903131249,-15.1283843904584,
6.19099528796663));
#51193=CARTESIAN_POINT('Ctrl Pts',(-7.67233737080682,-16.6054945057935,
6.03399516061437));
#51194=CARTESIAN_POINT('Ctrl Pts',(-10.610359145649,-14.8408989797994,5.87699503326212));
#51195=CARTESIAN_POINT('Ctrl Pts',(-10.7592920173832,-11.4169237933092,
5.71999490590986));
#51196=CARTESIAN_POINT('Ctrl Pts',(-7.98558650367391,-9.40388769480238,
5.56299477855761));
#51197=CARTESIAN_POINT('Ctrl Pts',(-4.77645084555843,-10.6068850809164,
5.40599465120535));
#51198=CARTESIAN_POINT('Ctrl Pts',(-4.00954797596254,-13.9472048059447,
5.24899452385311));
#51199=CARTESIAN_POINT('Ctrl Pts',(-6.37256666156175,-16.4294950347898,
5.09199439650084));
#51200=CARTESIAN_POINT('Ctrl Pts',(-9.74656614790733,-15.8279701198543,
4.9349942691486));
#51201=CARTESIAN_POINT('Ctrl Pts',(-11.1060472187217,-12.6818122309103,
4.77799414179634));
#51202=CARTESIAN_POINT('Ctrl Pts',(-9.23195310627391,-9.81262424147309,
4.62099401444409));
#51203=CARTESIAN_POINT('Ctrl Pts',(-5.80479621412607,-9.79242646017958,
4.46399388709183));
#51204=CARTESIAN_POINT('Ctrl Pts',(-3.89775220169895,-12.6409121056472,
4.30699375973959));
#51205=CARTESIAN_POINT('Ctrl Pts',(-5.22086478169416,-15.8007186832344,
4.14999363238732));
#51206=CARTESIAN_POINT('Ctrl Pts',(-8.58771683219162,-16.4445101479194,
3.99299350503508));
#51207=CARTESIAN_POINT('Ctrl Pts',(-10.979271517566,-13.9827465287205,3.83599337768283));
#51208=CARTESIAN_POINT('Ctrl Pts',(-10.4928159504458,-11.7612243186229,
3.73132662611465));
#51209=CARTESIAN_POINT('Ctrl Pts',(-9.83606265769611,-10.9930794998359,
3.67899325033057));
#51210=CARTESIAN_POINT('Ctrl Pts',(-8.24593285434704,-15.7805586266087,
12.1070022498898));
#51211=CARTESIAN_POINT('Ctrl Pts',(-9.16339987378206,-15.5352807633023,
12.0546688741057));
#51212=CARTESIAN_POINT('Ctrl Pts',(-10.7225976911422,-14.0738485504296,
11.9500021225376));
#51213=CARTESIAN_POINT('Ctrl Pts',(-10.180917470255,-10.8944501595629,11.7930019951853));
#51214=CARTESIAN_POINT('Ctrl Pts',(-7.23091900471447,-9.60088325574055,
11.6360018678331));
#51215=CARTESIAN_POINT('Ctrl Pts',(-4.52437253811706,-11.3435907789116,
11.4790017404808));
#51216=CARTESIAN_POINT('Ctrl Pts',(-4.48499741917537,-14.5645722101431,
11.3220016131286));
#51217=CARTESIAN_POINT('Ctrl Pts',(-7.14976698350127,-16.3731545641054,
11.1650014857763));
#51218=CARTESIAN_POINT('Ctrl Pts',(-10.1283062268782,-15.1487835956953,
11.008001358424));
#51219=CARTESIAN_POINT('Ctrl Pts',(-10.7501650330301,-11.9887417782655,
10.8510012310718));
#51220=CARTESIAN_POINT('Ctrl Pts',(-8.45749457295849,-9.72698711711278,
10.6940011037196));
#51221=CARTESIAN_POINT('Ctrl Pts',(-5.30626791900676,-10.3914941238528,
10.5370009763673));
#51222=CARTESIAN_POINT('Ctrl Pts',(-4.12216225834487,-13.3864760728501,
10.380000849015));
#51223=CARTESIAN_POINT('Ctrl Pts',(-5.96700612634799,-16.0262614637418,
10.2230007216628));
#51224=CARTESIAN_POINT('Ctrl Pts',(-9.18649518751149,-15.9437511051639,
10.0660005943105));
#51225=CARTESIAN_POINT('Ctrl Pts',(-10.8936904509082,-13.2129217420271,
9.90900046695826));
#51226=CARTESIAN_POINT('Ctrl Pts',(-9.55772959244346,-10.2825399270605,
9.75200033960601));
#51227=CARTESIAN_POINT('Ctrl Pts',(-6.37658355063268,-9.78030425210093,
9.59500021225375));
#51228=CARTESIAN_POINT('Ctrl Pts',(-4.20281546745071,-12.1565757441505,
9.43800008490151));
#51229=CARTESIAN_POINT('Ctrl Pts',(-4.9856645647421,-15.2805282036001,9.28099995754924));
#51230=CARTESIAN_POINT('Ctrl Pts',(-8.02314227712081,-16.3508838764116,
9.12399983019701));
#51231=CARTESIAN_POINT('Ctrl Pts',(-10.5915133373824,-14.4078443649032,
8.96699970284473));
#51232=CARTESIAN_POINT('Ctrl Pts',(-10.387694705577,-11.1937519405699,8.8099995754925));
#51233=CARTESIAN_POINT('Ctrl Pts',(-7.59445254015368,-9.59071406337065,
8.65299944814022));
#51234=CARTESIAN_POINT('Ctrl Pts',(-4.71651386962368,-11.0361902030079,
8.49599932078799));
#51235=CARTESIAN_POINT('Ctrl Pts',(-4.33455391893407,-14.2340080242683,
8.33899919343572));
#51236=CARTESIAN_POINT('Ctrl Pts',(-6.79107983542896,-16.3166536153767,
8.18199906608348));
#51237=CARTESIAN_POINT('Ctrl Pts',(-9.88330126539458,-15.4165986909841,
8.02499893873122));
#51238=CARTESIAN_POINT('Ctrl Pts',(-10.8383935859029,-12.340931138896,7.86799881137898));
#51239=CARTESIAN_POINT('Ctrl Pts',(-8.79991635104542,-9.84763155765228,
7.7109986840267));
#51240=CARTESIAN_POINT('Ctrl Pts',(-5.59579165327249,-10.1724656040451,
7.55399855667448));
#51241=CARTESIAN_POINT('Ctrl Pts',(-4.09918884819405,-13.0241514678338,
7.3969984293222));
#51242=CARTESIAN_POINT('Ctrl Pts',(-5.65212602885569,-15.8455550856297,
7.23999830196996));
#51243=CARTESIAN_POINT('Ctrl Pts',(-8.8620695270797,-16.1066967495653,7.0829981746177));
#51244=CARTESIAN_POINT('Ctrl Pts',(-10.8506322134124,-13.5734082564495,
6.92599804726545));
#51245=CARTESIAN_POINT('Ctrl Pts',(-9.83465084917482,-10.517313638478,6.76899791991319));
#51246=CARTESIAN_POINT('Ctrl Pts',(-6.72516567143593,-9.67884238140407,
6.61199779256095));
#51247=CARTESIAN_POINT('Ctrl Pts',(-4.31048186840692,-11.8098594647285,
6.45499766520868));
#51248=CARTESIAN_POINT('Ctrl Pts',(-4.75586957505634,-14.999461896718,6.29799753785644));
#51249=CARTESIAN_POINT('Ctrl Pts',(-7.66194535538809,-16.3875016553343,
6.14099741050417));
#51250=CARTESIAN_POINT('Ctrl Pts',(-10.4228031904426,-14.7293119763608,
5.98399728315194));
#51251=CARTESIAN_POINT('Ctrl Pts',(-10.5627553478246,-11.5118039232893,
5.82699715579966));
#51252=CARTESIAN_POINT('Ctrl Pts',(-7.95630543474677,-9.62015474206144,
5.66999702844743));
#51253=CARTESIAN_POINT('Ctrl Pts',(-4.94068199678335,-10.7506108834838,
5.51299690109516));
#51254=CARTESIAN_POINT('Ctrl Pts',(-4.22002369044277,-13.8895079343495,
5.35599677374291));
#51255=CARTESIAN_POINT('Ctrl Pts',(-6.44055136262695,-16.2221150259203,
5.19899664639066));
#51256=CARTESIAN_POINT('Ctrl Pts',(-9.61109727113964,-15.6568623145209,
5.04199651903841));
#51257=CARTESIAN_POINT('Ctrl Pts',(-10.8886010657355,-12.7004190599517,
4.88499639168614));
#51258=CARTESIAN_POINT('Ctrl Pts',(-9.12751561079228,-10.0042443043008,
4.72799626433391));
#51259=CARTESIAN_POINT('Ctrl Pts',(-5.90701771024297,-9.98526445765287,
4.57099613698164));
#51260=CARTESIAN_POINT('Ctrl Pts',(-4.11496924804734,-12.6619852293197,
4.4139960096294));
#51261=CARTESIAN_POINT('Ctrl Pts',(-5.35829758700603,-15.631254150908,4.25699588227714));
#51262=CARTESIAN_POINT('Ctrl Pts',(-8.52212705303664,-16.2362247214587,
4.09999575492489));
#51263=CARTESIAN_POINT('Ctrl Pts',(-10.7694699922944,-13.9229064764016,
3.94299562757263));
#51264=CARTESIAN_POINT('Ctrl Pts',(-10.31234789899,-11.8353429831647,3.83832887600446));
#51265=CARTESIAN_POINT('Ctrl Pts',(-9.69519710401908,-11.1135176176878,
3.78599550022038));
#51266=CARTESIAN_POINT('Ctrl Pts',(-8.19806642616111,-15.6015132427052,
12.2140044997796));
#51267=CARTESIAN_POINT('Ctrl Pts',(-9.05665968914096,-15.3719748325695,
12.1616711239955));
#51268=CARTESIAN_POINT('Ctrl Pts',(-10.5158039562152,-14.0043225620313,
12.0570043724274));
#51269=CARTESIAN_POINT('Ctrl Pts',(-10.0088832947732,-11.0289458118043,
11.9000042450751));
#51270=CARTESIAN_POINT('Ctrl Pts',(-7.24818590221332,-9.81838695213045,
11.7430041177229));
#51271=CARTESIAN_POINT('Ctrl Pts',(-4.71531822093855,-11.4492651276319,
11.5860039903706));
#51272=CARTESIAN_POINT('Ctrl Pts',(-4.67846979899401,-14.4635565391549,
11.4290038630183));
#51273=CARTESIAN_POINT('Ctrl Pts',(-7.17224139716313,-16.1560823648925,
11.2720037356661));
#51274=CARTESIAN_POINT('Ctrl Pts',(-9.95964810902439,-15.0102791451622,
11.1150036083138));
#51275=CARTESIAN_POINT('Ctrl Pts',(-10.5416023048445,-12.0530168592103,
10.9580034809616));
#51276=CARTESIAN_POINT('Ctrl Pts',(-8.39605225285175,-9.93639874276315,
10.8010033536093));
#51277=CARTESIAN_POINT('Ctrl Pts',(-5.44703946231937,-10.5582644088895,
10.6440032262571));
#51278=CARTESIAN_POINT('Ctrl Pts',(-4.3389177300236,-13.3610586997827,10.4870030989048));
#51279=CARTESIAN_POINT('Ctrl Pts',(-6.06537817248458,-15.8314493561443,
10.3300029715526));
#51280=CARTESIAN_POINT('Ctrl Pts',(-9.07827297916059,-15.7542336780869,
10.1730028442003));
#51281=CARTESIAN_POINT('Ctrl Pts',(-10.6759177126423,-13.1986413310391,
10.0160027168481));
#51282=CARTESIAN_POINT('Ctrl Pts',(-9.42568531367393,-10.4563017907707,
9.85900258949582));
#51283=CARTESIAN_POINT('Ctrl Pts',(-6.44867305906919,-9.98629452313723,
9.70200246214357));
#51284=CARTESIAN_POINT('Ctrl Pts',(-4.41439543168378,-12.2100809381968,
9.54500233479132));
#51285=CARTESIAN_POINT('Ctrl Pts',(-5.14700918959101,-15.1335697162506,
9.38800220743905));
#51286=CARTESIAN_POINT('Ctrl Pts',(-7.98957229546242,-16.1352407847476,
9.23100208008682));
#51287=CARTESIAN_POINT('Ctrl Pts',(-10.3931312708367,-14.3168859022886,
9.07400195273454));
#51288=CARTESIAN_POINT('Ctrl Pts',(-10.2023916579342,-11.3090414308585,
8.91700182538231));
#51289=CARTESIAN_POINT('Ctrl Pts',(-7.58839153117158,-9.80887031570234,
8.76000169803004));
#51290=CARTESIAN_POINT('Ctrl Pts',(-4.89512986460196,-11.1615904124476,
8.6030015706778));
#51291=CARTESIAN_POINT('Ctrl Pts',(-4.53768024140768,-14.1542046202714,
8.44600144332553));
#51292=CARTESIAN_POINT('Ctrl Pts',(-6.83657116343421,-16.103207075751,8.28900131597329));
#51293=CARTESIAN_POINT('Ctrl Pts',(-9.730365088632,-15.2609085756139,8.13200118862103));
#51294=CARTESIAN_POINT('Ctrl Pts',(-10.6241692413057,-12.3826062677939,
7.97500106126879));
#51295=CARTESIAN_POINT('Ctrl Pts',(-8.71650086357571,-10.0493014429898,
7.81800093391652));
#51296=CARTESIAN_POINT('Ctrl Pts',(-5.7179844908027,-10.3532909248038,7.66100080656428));
#51297=CARTESIAN_POINT('Ctrl Pts',(-4.31741852104351,-13.0219844243168,
7.50400067921201));
#51298=CARTESIAN_POINT('Ctrl Pts',(-5.7707038957789,-15.6623388861897,7.34700055185977));
#51299=CARTESIAN_POINT('Ctrl Pts',(-8.77466567722613,-15.9067231186349,
7.19000042450751));
#51300=CARTESIAN_POINT('Ctrl Pts',(-10.635622517451,-13.5359954659799,7.03300029715527));
#51301=CARTESIAN_POINT('Ctrl Pts',(-9.68483656420267,-10.6760100992742,
6.87600016980299));
#51302=CARTESIAN_POINT('Ctrl Pts',(-6.77488670400349,-9.89134344938279,
6.71900004245076));
#51303=CARTESIAN_POINT('Ctrl Pts',(-4.51515289168187,-11.8856134038101,
6.56199991509849));
#51304=CARTESIAN_POINT('Ctrl Pts',(-4.93196011880019,-14.8705394029777,
6.40499978774625));
#51305=CARTESIAN_POINT('Ctrl Pts',(-7.65155333996934,-16.1695088048751,
6.24799966039398));
#51306=CARTESIAN_POINT('Ctrl Pts',(-10.2352472352362,-14.6177249729221,
6.09099953304175));
#51307=CARTESIAN_POINT('Ctrl Pts',(-10.366218678266,-11.6066840532695,5.93399940568948));
#51308=CARTESIAN_POINT('Ctrl Pts',(-7.92702436581964,-9.83642178932047,
5.77699927833724));
#51309=CARTESIAN_POINT('Ctrl Pts',(-5.10491314800829,-10.8943366860512,
5.61999915098497));
#51310=CARTESIAN_POINT('Ctrl Pts',(-4.43049940492298,-13.8318110627544,
5.46299902363273));
#51311=CARTESIAN_POINT('Ctrl Pts',(-6.50853606369215,-16.0147350170509,
5.30599889628046));
#51312=CARTESIAN_POINT('Ctrl Pts',(-9.47562839437195,-15.4857545091874,
5.14899876892823));
#51313=CARTESIAN_POINT('Ctrl Pts',(-10.6711549127493,-12.7190258889931,
4.99199864157595));
#51314=CARTESIAN_POINT('Ctrl Pts',(-9.02307811531067,-10.1958643671286,
4.83499851422372));
#51315=CARTESIAN_POINT('Ctrl Pts',(-6.00923920635987,-10.1781024551261,
4.67799838687145));
#51316=CARTESIAN_POINT('Ctrl Pts',(-4.33218629439574,-12.6830583529922,
4.52099825951921));
#51317=CARTESIAN_POINT('Ctrl Pts',(-5.49573039231789,-15.4617896185815,
4.36399813216695));
#51318=CARTESIAN_POINT('Ctrl Pts',(-8.45653727388165,-16.027939294998,4.2069980048147));
#51319=CARTESIAN_POINT('Ctrl Pts',(-10.5596684670228,-13.8630664240827,
4.04999787746245));
#51320=CARTESIAN_POINT('Ctrl Pts',(-10.1318798475343,-11.9094616477065,
3.94533112589428));
#51321=CARTESIAN_POINT('Ctrl Pts',(-9.55433155034205,-11.2339557355397,
3.89299775011019));
#51322=CARTESIAN_POINT('Ctrl Pts',(-8.15019999797519,-15.4224678588016,
12.3210067496694));
#51323=CARTESIAN_POINT('Ctrl Pts',(-8.94991950449986,-15.2086689018368,
12.2686733738853));
#51324=CARTESIAN_POINT('Ctrl Pts',(-10.3090102212882,-13.934796573633,12.1640066223172));
#51325=CARTESIAN_POINT('Ctrl Pts',(-9.83684911929144,-11.1634414640457,
12.0070064949649));
#51326=CARTESIAN_POINT('Ctrl Pts',(-7.26545279971217,-10.0358906485204,
11.8500063676127));
#51327=CARTESIAN_POINT('Ctrl Pts',(-4.90626390376006,-11.5549394763523,
11.6930062402604));
#51328=CARTESIAN_POINT('Ctrl Pts',(-4.87194217881263,-14.3625408681667,
11.5360061129082));
#51329=CARTESIAN_POINT('Ctrl Pts',(-7.19471581082501,-15.9390101656796,
11.3790059855559));
#51330=CARTESIAN_POINT('Ctrl Pts',(-9.7909899911706,-14.871774694629,11.2220058582037));
#51331=CARTESIAN_POINT('Ctrl Pts',(-10.3330395766588,-12.1172919401552,
11.0650057308514));
#51332=CARTESIAN_POINT('Ctrl Pts',(-8.334609932745,-10.1458103684135,10.9080056034992));
#51333=CARTESIAN_POINT('Ctrl Pts',(-5.587811005632,-10.7250346939262,10.7510054761469));
#51334=CARTESIAN_POINT('Ctrl Pts',(-4.55567320170231,-13.3356413267153,
10.5940053487946));
#51335=CARTESIAN_POINT('Ctrl Pts',(-6.16375021862117,-15.6366372485469,
10.4370052214424));
#51336=CARTESIAN_POINT('Ctrl Pts',(-8.97005077080969,-15.5647162510099,
10.2800050940901));
#51337=CARTESIAN_POINT('Ctrl Pts',(-10.4581449743764,-13.1843609200512,
10.1230049667379));
#51338=CARTESIAN_POINT('Ctrl Pts',(-9.29364103490441,-10.6300636544808,
9.96600483938564));
#51339=CARTESIAN_POINT('Ctrl Pts',(-6.52076256750571,-10.1922847941736,
9.80900471203337));
#51340=CARTESIAN_POINT('Ctrl Pts',(-4.62597539591685,-12.2635861322432,
9.65200458468114));
#51341=CARTESIAN_POINT('Ctrl Pts',(-5.30835381443992,-14.9866112289011,
9.49500445732886));
#51342=CARTESIAN_POINT('Ctrl Pts',(-7.95600231380402,-15.9195976930836,
9.33800432997663));
#51343=CARTESIAN_POINT('Ctrl Pts',(-10.1947492042911,-14.2259274396741,
9.18100420262435));
#51344=CARTESIAN_POINT('Ctrl Pts',(-10.0170886102914,-11.424330921147,9.02400407527213));
#51345=CARTESIAN_POINT('Ctrl Pts',(-7.58233052218947,-10.0270265680341,
8.86700394791983));
#51346=CARTESIAN_POINT('Ctrl Pts',(-5.07374585958023,-11.2869906218872,
8.71000382056763));
#51347=CARTESIAN_POINT('Ctrl Pts',(-4.7408065638813,-14.0744012162745,8.55300369321533));
#51348=CARTESIAN_POINT('Ctrl Pts',(-6.88206249143947,-15.8897605361253,
8.39600356586311));
#51349=CARTESIAN_POINT('Ctrl Pts',(-9.57742891186941,-15.1052184602437,
8.23900343851083));
#51350=CARTESIAN_POINT('Ctrl Pts',(-10.4099448967086,-12.4242813966918,
8.0820033111586));
#51351=CARTESIAN_POINT('Ctrl Pts',(-8.633085376106,-10.2509713283274,7.92500318380633));
#51352=CARTESIAN_POINT('Ctrl Pts',(-5.84017732833291,-10.5341162455624,
7.7680030564541));
#51353=CARTESIAN_POINT('Ctrl Pts',(-4.53564819389297,-13.0198173807997,
7.61100292910182));
#51354=CARTESIAN_POINT('Ctrl Pts',(-5.88928176270212,-15.4791226867497,
7.45400280174959));
#51355=CARTESIAN_POINT('Ctrl Pts',(-8.68726182737255,-15.7067494877046,
7.29700267439731));
#51356=CARTESIAN_POINT('Ctrl Pts',(-10.4206128214897,-13.4985826755103,
7.14000254704508));
#51357=CARTESIAN_POINT('Ctrl Pts',(-9.53502227923051,-10.8347065600703,
6.9830024196928));
#51358=CARTESIAN_POINT('Ctrl Pts',(-6.82460773657105,-10.1038445173615,
6.82600229234058));
#51359=CARTESIAN_POINT('Ctrl Pts',(-4.71982391495681,-11.9613673428918,
6.66900216498829));
#51360=CARTESIAN_POINT('Ctrl Pts',(-5.10805066254405,-14.7416169092374,
6.51200203763607));
#51361=CARTESIAN_POINT('Ctrl Pts',(-7.64116132455058,-15.9515159544159,
6.35500191028379));
#51362=CARTESIAN_POINT('Ctrl Pts',(-10.0476912800297,-14.5061379694834,
6.19800178293156));
#51363=CARTESIAN_POINT('Ctrl Pts',(-10.1696820087074,-11.7015641832497,
6.04100165557928));
#51364=CARTESIAN_POINT('Ctrl Pts',(-7.8977432968925,-10.0526888365795,5.88400152822706));
#51365=CARTESIAN_POINT('Ctrl Pts',(-5.26914429923322,-11.0380624886186,
5.72700140087478));
#51366=CARTESIAN_POINT('Ctrl Pts',(-4.6409751194032,-13.7741141911592,5.57000127352254));
#51367=CARTESIAN_POINT('Ctrl Pts',(-6.57652076475734,-15.8073550081814,
5.41300114617028));
#51368=CARTESIAN_POINT('Ctrl Pts',(-9.34015951760427,-15.314646703854,5.25600101881803));
#51369=CARTESIAN_POINT('Ctrl Pts',(-10.4537087597631,-12.7376327180345,
5.09900089146577));
#51370=CARTESIAN_POINT('Ctrl Pts',(-8.91864061982905,-10.3874844299563,
4.94200076411353));
#51371=CARTESIAN_POINT('Ctrl Pts',(-6.11146070247677,-10.3709404525994,
4.78500063676126));
#51372=CARTESIAN_POINT('Ctrl Pts',(-4.54940334074414,-12.7041314766647,
4.62800050940902));
#51373=CARTESIAN_POINT('Ctrl Pts',(-5.63316319762975,-15.2923250862551,
4.47100038205676));
#51374=CARTESIAN_POINT('Ctrl Pts',(-8.39094749472666,-15.8196538685372,
4.31400025470451));
#51375=CARTESIAN_POINT('Ctrl Pts',(-10.3498669417512,-13.8032263717638,
4.15700012735226));
#51376=CARTESIAN_POINT('Ctrl Pts',(-9.95141179607851,-11.9835803122483,
4.05233337578409));
#51377=CARTESIAN_POINT('Ctrl Pts',(-9.41346599666503,-11.3543938533916,
4.));
#51378=CARTESIAN_POINT('Ctrl Pts',(-10.0159021674261,-12.9883695445715,
11.112583302492));
#51379=CARTESIAN_POINT('Ctrl Pts',(-10.0178571377502,-12.737164469747,11.0967241119451));
#51380=CARTESIAN_POINT('Ctrl Pts',(-9.98318366513377,-12.4864861117061,
11.0808649213983));
#51381=CARTESIAN_POINT('Ctrl Pts',(-9.90962637175846,-12.2477921372772,
11.0650057308514));
#51382=CARTESIAN_POINT('Ctrl Pts',(-9.66689636202086,-11.4601314162413,
11.0126723550673));
#51383=CARTESIAN_POINT('Ctrl Pts',(-9.00075314738293,-10.8029708923274,
10.9603389792832));
#51384=CARTESIAN_POINT('Ctrl Pts',(-8.20988171887847,-10.5709280179559,
10.9080056034991));
#51385=CARTESIAN_POINT('Ctrl Pts',(-7.419010290374,-10.3388851435844,10.8556722277151));
#51386=CARTESIAN_POINT('Ctrl Pts',(-6.503410648003,-10.5319599187553,10.803338851931));
#51387=CARTESIAN_POINT('Ctrl Pts',(-5.87358785949589,-11.0635984118056,
10.7510054761469));
#51388=CARTESIAN_POINT('Ctrl Pts',(-5.24376507098877,-11.5952369048559,
10.6986721003628));
#51389=CARTESIAN_POINT('Ctrl Pts',(-4.89971913634554,-12.4654391157856,
10.6463387245787));
#51390=CARTESIAN_POINT('Ctrl Pts',(-4.99570900517707,-13.2840395415557,
10.5940053487946));
#51391=CARTESIAN_POINT('Ctrl Pts',(-5.0916988740086,-14.1026399673258,10.5416719730106));
#51392=CARTESIAN_POINT('Ctrl Pts',(-5.62772454631489,-14.8696386079364,
10.4893385972265));
#51393=CARTESIAN_POINT('Ctrl Pts',(-6.36345414116612,-15.2411510953188,
10.4370052214424));
#51394=CARTESIAN_POINT('Ctrl Pts',(-7.09918373601734,-15.6126635827012,
10.3846718456583));
#51395=CARTESIAN_POINT('Ctrl Pts',(-8.03461725341351,-15.5886899168556,
10.3323384698742));
#51396=CARTESIAN_POINT('Ctrl Pts',(-8.75034971270605,-15.1799771954396,
10.2800050940901));
#51397=CARTESIAN_POINT('Ctrl Pts',(-9.46608217199859,-14.7712644740237,
10.2276717183061));
#51398=CARTESIAN_POINT('Ctrl Pts',(-9.96211357318751,-13.9778126970374,
10.175338342522));
#51399=CARTESIAN_POINT('Ctrl Pts',(-10.01604528387,-13.1553705976159,10.1230049667379));
#51400=CARTESIAN_POINT('Ctrl Pts',(-10.0196252693796,-13.1007769130985,
10.1195310786559));
#51401=CARTESIAN_POINT('Ctrl Pts',(-10.0212572306508,-13.0460554884989,
10.1160571905739));
#51402=CARTESIAN_POINT('Ctrl Pts',(-10.0209920718673,-12.9913179799917,
10.112583302492));
#51403=CARTESIAN_POINT('Ctrl Pts',(-8.29379928253297,-15.9596040105122,
12.));
#51404=CARTESIAN_POINT('Ctrl Pts',(-8.38688146826619,-15.9255541311756,
12.));
#51405=CARTESIAN_POINT('Ctrl Pts',(-8.47790052796864,-15.8867414890058,
12.));
#51406=CARTESIAN_POINT('Ctrl Pts',(-8.56664663605253,-15.843492548424,12.));
#51407=CARTESIAN_POINT('Ctrl Pts',(-8.65733876929825,-15.7992952448277,
12.));
#51408=CARTESIAN_POINT('Ctrl Pts',(-8.74565784480789,-15.750464336337,12.));
#51409=CARTESIAN_POINT('Ctrl Pts',(-8.83135101694567,-15.6973027457218,
12.));
#51410=CARTESIAN_POINT('Ctrl Pts',(-8.91318960012018,-15.6465324317433,
12.));
#51411=CARTESIAN_POINT('Ctrl Pts',(-8.99263343720554,-15.5918113841942,
12.));
#51412=CARTESIAN_POINT('Ctrl Pts',(-9.069430157416,-15.533374159028,12.));
#51413=CARTESIAN_POINT('Ctrl Pts',(-9.13662728760015,-15.4822415870076,
12.));
#51414=CARTESIAN_POINT('Ctrl Pts',(-9.20179743619592,-15.4282631425356,
12.));
#51415=CARTESIAN_POINT('Ctrl Pts',(-9.26474763112753,-15.3715835638146,
12.));
#51416=CARTESIAN_POINT('Ctrl Pts',(-9.27985611388604,-15.3579800723751,
12.));
#51417=CARTESIAN_POINT('Ctrl Pts',(-9.29484029179697,-15.3442173582628,
12.));
#51418=CARTESIAN_POINT('Ctrl Pts',(-9.30967505138841,-15.3303185989115,
12.));
#51419=CARTESIAN_POINT('Ctrl Pts',(-9.38210503428163,-15.26245859108,12.));
#51420=CARTESIAN_POINT('Ctrl Pts',(-9.45106917065939,-15.1912779029607,
12.));
#51421=CARTESIAN_POINT('Ctrl Pts',(-9.51632647275336,-15.1170649381822,
12.));
#51422=CARTESIAN_POINT('Ctrl Pts',(-9.58121888012541,-15.0432669448824,
12.));
#51423=CARTESIAN_POINT('Ctrl Pts',(-9.64244627908667,-14.9664696982533,
12.));
#51424=CARTESIAN_POINT('Ctrl Pts',(-9.69972810245665,-14.8869300127004,
12.));
#51425=CARTESIAN_POINT('Ctrl Pts',(-9.75408287639578,-14.81145473323,12.));
#51426=CARTESIAN_POINT('Ctrl Pts',(-9.80488505097158,-14.7335093955071,
12.));
#51427=CARTESIAN_POINT('Ctrl Pts',(-9.85185230919616,-14.6533004074739,
12.));
#51428=CARTESIAN_POINT('Ctrl Pts',(-9.8892295724543,-14.5894688666365,12.));
#51429=CARTESIAN_POINT('Ctrl Pts',(-9.92417736747258,-14.5242033609892,
12.));
#51430=CARTESIAN_POINT('Ctrl Pts',(-9.95653206305223,-14.4576058296606,
12.));
#51431=CARTESIAN_POINT('Ctrl Pts',(-9.96243497650182,-14.4454555233034,
12.));
#51432=CARTESIAN_POINT('Ctrl Pts',(-9.9682498087257,-14.4332643188572,12.));
#51433=CARTESIAN_POINT('Ctrl Pts',(-9.97397236800321,-14.4210401757467,
12.));
#51434=CARTESIAN_POINT('Ctrl Pts',(-10.014548795905,-14.3343635617469,12.));
#51435=CARTESIAN_POINT('Ctrl Pts',(-10.0505434398104,-14.2459232997935,
12.));
#51436=CARTESIAN_POINT('Ctrl Pts',(-10.0816927676552,-14.1559630239742,
12.));
#51437=CARTESIAN_POINT('Ctrl Pts',(-10.1128420955,-14.0660027481548,12.));
#51438=CARTESIAN_POINT('Ctrl Pts',(-10.1391465733587,-13.9745217251954,
12.));
#51439=CARTESIAN_POINT('Ctrl Pts',(-10.1602864633442,-13.8817537764296,
12.));
#51440=CARTESIAN_POINT('Ctrl Pts',(-10.1814515048034,-13.7888754557256,
12.));
#51441=CARTESIAN_POINT('Ctrl Pts',(-10.1974388881398,-13.6947059611701,
12.));
#51442=CARTESIAN_POINT('Ctrl Pts',(-10.2083240537505,-13.5996534977197,
12.));
#51443=CARTESIAN_POINT('Ctrl Pts',(-10.2138911337605,-13.5510401198348,
12.));
#51444=CARTESIAN_POINT('Ctrl Pts',(-10.2181228103627,-13.5021959582282,
12.));
#51445=CARTESIAN_POINT('Ctrl Pts',(-10.221024235662,-13.4531774228974,12.));
#51446=CARTESIAN_POINT('Ctrl Pts',(-10.2218608104944,-13.4390437924411,
12.));
#51447=CARTESIAN_POINT('Ctrl Pts',(-10.2225867738812,-13.4248956759012,
12.));
#51448=CARTESIAN_POINT('Ctrl Pts',(-10.2232022007112,-13.410734453067,12.));
#51449=CARTESIAN_POINT('Ctrl Pts',(-10.2238234019696,-13.3964403582763,
12.));
#51450=CARTESIAN_POINT('Ctrl Pts',(-10.2243315800161,-13.3821418174545,
12.));
#51451=CARTESIAN_POINT('Ctrl Pts',(-10.2247271750585,-13.3678432915664,
12.));
#51452=CARTESIAN_POINT('Ctrl Pts',(-10.2273082491492,-13.2745520448321,
12.));
#51453=CARTESIAN_POINT('Ctrl Pts',(-10.2251029799825,-13.1812181718667,
12.));
#51454=CARTESIAN_POINT('Ctrl Pts',(-10.2182398910409,-13.0882187710056,
12.));
#51455=CARTESIAN_POINT('Ctrl Pts',(-10.2113725866781,-12.9951622483964,
12.));
#51456=CARTESIAN_POINT('Ctrl Pts',(-10.1998413619504,-12.902439631583,12.));
#51457=CARTESIAN_POINT('Ctrl Pts',(-10.1837244231874,-12.810441427736,12.));
#51458=CARTESIAN_POINT('Ctrl Pts',(-10.1678505565058,-12.7198307203121,
12.));
#51459=CARTESIAN_POINT('Ctrl Pts',(-10.1475277985646,-12.629921903999,12.));
#51460=CARTESIAN_POINT('Ctrl Pts',(-10.1227882064871,-12.5411137713789,
12.));
#51461=CARTESIAN_POINT('Ctrl Pts',(-10.1129089207081,-12.5056499319226,
12.));
#51462=CARTESIAN_POINT('Ctrl Pts',(-10.1023248586868,-12.4703619714101,
12.));
#51463=CARTESIAN_POINT('Ctrl Pts',(-10.0910363601597,-12.435276902831,12.));
#51464=CARTESIAN_POINT('Ctrl Pts',(-10.0850884600019,-12.4167906103951,
12.));
#51465=CARTESIAN_POINT('Ctrl Pts',(-10.0789449767355,-12.398360662607,12.));
#51466=CARTESIAN_POINT('Ctrl Pts',(-10.0726058589696,-12.3799911333697,
12.));
#51467=CARTESIAN_POINT('Ctrl Pts',(-10.0672510463096,-12.3644739287129,
12.));
#51468=CARTESIAN_POINT('Ctrl Pts',(-10.0617592067699,-12.349007385008,12.));
#51469=CARTESIAN_POINT('Ctrl Pts',(-10.0561325433239,-12.3335987119335,
12.));
#51470=CARTESIAN_POINT('Ctrl Pts',(-10.0253173441252,-12.2492109864665,
12.));
#51471=CARTESIAN_POINT('Ctrl Pts',(-9.99044488561477,-12.166508346864,12.));
#51472=CARTESIAN_POINT('Ctrl Pts',(-9.95156719631022,-12.0858609769308,
12.));
#51473=CARTESIAN_POINT('Ctrl Pts',(-9.92246136851044,-12.0254842286268,
12.));
#51474=CARTESIAN_POINT('Ctrl Pts',(-9.89110980665403,-11.9662598549223,
12.));
#51475=CARTESIAN_POINT('Ctrl Pts',(-9.85752076592995,-11.9083564676894,
12.));
#51476=CARTESIAN_POINT('Ctrl Pts',(-9.84460179101728,-11.8860857391751,
12.));
#51477=CARTESIAN_POINT('Ctrl Pts',(-9.83135170784992,-11.8640105638195,
12.));
#51478=CARTESIAN_POINT('Ctrl Pts',(-9.81777057146904,-11.8421410854707,
12.));
#51479=CARTESIAN_POINT('Ctrl Pts',(-9.80600924137691,-11.8232020109641,
12.));
#51480=CARTESIAN_POINT('Ctrl Pts',(-9.79399765022805,-11.8044144459084,
12.));
#51481=CARTESIAN_POINT('Ctrl Pts',(-9.78175006557354,-11.7858062660097,
12.));
#51482=CARTESIAN_POINT('Ctrl Pts',(-9.73447815410214,-11.7139844123438,
12.));
#51483=CARTESIAN_POINT('Ctrl Pts',(-9.68365479534874,-11.6447676019631,
12.));
#51484=CARTESIAN_POINT('Ctrl Pts',(-9.62930896131935,-11.578509745124,12.));
#51485=CARTESIAN_POINT('Ctrl Pts',(-9.58717521523442,-11.5271407346737,
12.));
#51486=CARTESIAN_POINT('Ctrl Pts',(-9.54292346973057,-11.477550842089,12.));
#51487=CARTESIAN_POINT('Ctrl Pts',(-9.49655480089338,-11.4299227460007,
12.));
#51488=CARTESIAN_POINT('Ctrl Pts',(-9.47068894114788,-11.4033543392671,
12.));
#51489=CARTESIAN_POINT('Ctrl Pts',(-9.44416412664311,-11.377396721654,12.));
#51490=CARTESIAN_POINT('Ctrl Pts',(-9.41700750114215,-11.3520617378123,
12.));
#51491=CARTESIAN_POINT('Origin',(-7.50000000000001,-12.9903810567666,7.5));
#51492=CARTESIAN_POINT('Origin',(-7.5,12.9903810567666,3.));
#51493=CARTESIAN_POINT('Origin',(15.,0.,3.));
#51494=CARTESIAN_POINT('Origin',(-7.50000000000001,-12.9903810567666,3.));
#51495=CARTESIAN_POINT('Origin',(5.55111512312578E-16,0.,14.));
#51496=CARTESIAN_POINT('',(-5.65685424949238,-6.92764844988394E-16,12.));
#51497=CARTESIAN_POINT('Origin',(5.55111512312578E-16,0.,12.));
#51498=CARTESIAN_POINT('',(1.87717472568372E-16,-4.49927934798557E-32,8.));
#51499=CARTESIAN_POINT('Origin',(5.55111512312578E-16,0.,14.));
#51500=CARTESIAN_POINT('Origin',(0.,0.,0.));
#51501=CARTESIAN_POINT('',(-30.,-3.67394039744206E-15,12.));
#51502=CARTESIAN_POINT('Origin',(0.,0.,12.));
#51503=CARTESIAN_POINT('',(-30.,-3.67394039744206E-15,0.));
#51504=CARTESIAN_POINT('',(-30.,-3.67394039744206E-15,0.));
#51505=CARTESIAN_POINT('Origin',(0.,0.,0.));
#51506=CARTESIAN_POINT('Origin',(0.,0.,12.));
#51507=CARTESIAN_POINT('Origin',(0.,0.,0.));
#51508=CARTESIAN_POINT('',(0.,0.,0.));
#51509=CARTESIAN_POINT('Origin',(-7.5,12.9903810567666,15.));
#51510=CARTESIAN_POINT('',(-11.,12.9903810567666,18.));
#51511=CARTESIAN_POINT('Origin',(-7.5,12.9903810567666,18.));
#51512=CARTESIAN_POINT('',(-11.,12.9903810567666,12.));
#51513=CARTESIAN_POINT('',(-11.,12.9903810567666,15.));
#51514=CARTESIAN_POINT('Origin',(-7.5,12.9903810567666,12.));
#51515=CARTESIAN_POINT('Origin',(15.,0.,15.));
#51516=CARTESIAN_POINT('',(11.5,4.28626379701574E-16,18.));
#51517=CARTESIAN_POINT('Origin',(15.,0.,18.));
#51518=CARTESIAN_POINT('',(11.5,4.28626379701574E-16,12.));
#51519=CARTESIAN_POINT('',(11.5,4.28626379701574E-16,15.));
#51520=CARTESIAN_POINT('Origin',(15.,0.,12.));
#51521=CARTESIAN_POINT('Origin',(-7.50000000000001,-12.9903810567666,15.));
#51522=CARTESIAN_POINT('',(-11.,-12.9903810567666,18.));
#51523=CARTESIAN_POINT('Origin',(-7.50000000000001,-12.9903810567666,18.));
#51524=CARTESIAN_POINT('',(-11.,-12.9903810567666,12.));
#51525=CARTESIAN_POINT('',(-11.,-12.9903810567666,15.));
#51526=CARTESIAN_POINT('Origin',(-7.50000000000001,-12.9903810567666,12.));
#51527=CARTESIAN_POINT('Origin',(5.55111512312578E-16,0.,14.));
#51528=CARTESIAN_POINT('',(-5.65685424949238,-6.92764844988394E-16,12.));
#51529=CARTESIAN_POINT('Origin',(5.55111512312578E-16,0.,12.));
#51530=CARTESIAN_POINT('',(-5.5,6.73555739531044E-16,16.3979157616564));
#51531=CARTESIAN_POINT('Origin',(5.55111512312578E-16,0.,14.));
#51532=CARTESIAN_POINT('Origin',(0.,0.,16.3979157616564));
#51533=CARTESIAN_POINT('Origin',(0.,0.,12.));
#51534=CARTESIAN_POINT('',(-5.5,-6.73555739531044E-16,18.));
#51535=CARTESIAN_POINT('Origin',(0.,0.,18.));
#51536=CARTESIAN_POINT('',(-5.5,-6.73555739531044E-16,12.));
#51537=CARTESIAN_POINT('Origin',(0.,0.,12.));
#51538=CARTESIAN_POINT('',(-22.,-2.69422295812418E-15,18.));
#51539=CARTESIAN_POINT('Origin',(0.,0.,18.));
#51540=CARTESIAN_POINT('',(-22.,-2.69422295812418E-15,12.));
#51541=CARTESIAN_POINT('',(-22.,-2.69422295812418E-15,12.));
#51542=CARTESIAN_POINT('Origin',(0.,0.,12.));
#51543=CARTESIAN_POINT('Origin',(0.,0.,18.));
#51544=CARTESIAN_POINT('Origin',(0.,0.,12.));
#51545=CARTESIAN_POINT('',(0.,0.,0.));
#51546=CARTESIAN_POINT('Origin',(0.,0.,16.));
#51547=CARTESIAN_POINT('',(-4.94751652564198,0.00256483971322934,26.3223204546569));
#51548=CARTESIAN_POINT('',(-4.94433041235646,0.00147179461986118,26.1776795453432));
#51549=CARTESIAN_POINT('',(-4.942,-6.05220448138622E-16,16.));
#51550=CARTESIAN_POINT('',(2.16917135428601,4.44050218283304,26.));
#51551=CARTESIAN_POINT('Ctrl Pts',(-4.94751652564198,0.00256483971322934,
26.3223204546569));
#51552=CARTESIAN_POINT('Ctrl Pts',(-4.94869886604438,0.171401137605494,
26.3168647682864));
#51553=CARTESIAN_POINT('Ctrl Pts',(-4.9408321732254,0.340133662244093,26.311409081916));
#51554=CARTESIAN_POINT('Ctrl Pts',(-4.92355817442292,0.507901950004805,
26.3059533955455));
#51555=CARTESIAN_POINT('Ctrl Pts',(-4.75600008116697,2.13525730225587,26.2530331414635));
#51556=CARTESIAN_POINT('Ctrl Pts',(-3.70330534691493,3.67188727651734,26.2001128873815));
#51557=CARTESIAN_POINT('Ctrl Pts',(-2.24451326222463,4.41286251356918,26.1471926332996));
#51558=CARTESIAN_POINT('Ctrl Pts',(-0.892016301737719,5.09984646860033,
26.0981284221997));
#51559=CARTESIAN_POINT('Ctrl Pts',(0.80955341496604,5.10290231670094,26.0490642110999));
#51560=CARTESIAN_POINT('Ctrl Pts',(2.17574200330363,4.4448669900444,26.));
#51561=CARTESIAN_POINT('',(-2.16917135428577,4.44050218283316,26.));
#51562=CARTESIAN_POINT('Origin',(0.,0.,26.));
#51563=CARTESIAN_POINT('Ctrl Pts',(-2.16917135428577,4.44050218283316,26.));
#51564=CARTESIAN_POINT('Ctrl Pts',(-2.90742207776898,4.07986902565299,26.026460127041));
#51565=CARTESIAN_POINT('Ctrl Pts',(-3.54838487149729,3.53163056089739,26.0529202540819));
#51566=CARTESIAN_POINT('Ctrl Pts',(-4.02597159025063,2.86203897562359,26.0793803811229));
#51567=CARTESIAN_POINT('Ctrl Pts',(-4.50355830900396,2.19244739034978,26.1058405081639));
#51568=CARTESIAN_POINT('Ctrl Pts',(-4.81776895278232,1.40150268455777,26.1323006352049));
#51569=CARTESIAN_POINT('Ctrl Pts',(-4.91302280979298,0.586752670320857,
26.1587607622459));
#51570=CARTESIAN_POINT('Ctrl Pts',(-4.93572472976967,0.39257271577962,26.1650670232783));
#51571=CARTESIAN_POINT('Ctrl Pts',(-4.94598956917588,0.197040583288091,
26.1713732843108));
#51572=CARTESIAN_POINT('Ctrl Pts',(-4.94433041235646,0.00147179461986118,
26.1776795453432));
#51573=CARTESIAN_POINT('Origin',(0.,0.,16.));
#51574=CARTESIAN_POINT('',(-4.93516121822955,0.00250487983550263,27.3223204546569));
#51575=CARTESIAN_POINT('',(-4.93474635697119,0.00209204260276723,27.1776795453432));
#51576=CARTESIAN_POINT('',(-4.942,-6.05220448138622E-16,16.));
#51577=CARTESIAN_POINT('Ctrl Pts',(-4.93516121822955,0.00250487983550263,
27.3223204546569));
#51578=CARTESIAN_POINT('Ctrl Pts',(-4.93820686879495,0.665010559781625,
27.3010529594449));
#51579=CARTESIAN_POINT('Ctrl Pts',(-4.81416865933799,1.32642295622759,27.2797854642328));
#51580=CARTESIAN_POINT('Ctrl Pts',(-4.55764236207275,1.93168318346768,27.2585179690208));
#51581=CARTESIAN_POINT('Ctrl Pts',(-3.91932380623715,3.43776204663053,27.2055977149389));
#51582=CARTESIAN_POINT('Ctrl Pts',(-2.46067639950694,4.59616252449921,27.1526774608569));
#51583=CARTESIAN_POINT('Ctrl Pts',(-0.849145821918294,4.87674835967949,
27.0997572067749));
#51584=CARTESIAN_POINT('Ctrl Pts',(0.762384755670364,5.15733419485977,27.046836952693));
#51585=CARTESIAN_POINT('Ctrl Pts',(2.52679850411746,4.56010538735165,26.993916698611));
#51586=CARTESIAN_POINT('Ctrl Pts',(3.63656998987608,3.35842905030792,26.940996444529));
#51587=CARTESIAN_POINT('Ctrl Pts',(4.7463414756347,2.15675271326421,26.8880761904471));
#51588=CARTESIAN_POINT('Ctrl Pts',(5.20147069870486,0.350628846684903,26.8351559363651));
#51589=CARTESIAN_POINT('Ctrl Pts',(4.79388038130065,-1.23355926618448,26.7822356822831));
#51590=CARTESIAN_POINT('Ctrl Pts',(4.38629006389643,-2.81774737905389,26.7293154282012));
#51591=CARTESIAN_POINT('Ctrl Pts',(3.11598020601782,-4.17999973821337,26.6763951741192));
#51592=CARTESIAN_POINT('Ctrl Pts',(1.56388702368888,-4.69668637868557,26.6234749200373));
#51593=CARTESIAN_POINT('Ctrl Pts',(0.011793841359943,-5.21337301915776,
26.5705546659553));
#51594=CARTESIAN_POINT('Ctrl Pts',(-1.82208266541932,-4.88449394094269,
26.5176344118733));
#51595=CARTESIAN_POINT('Ctrl Pts',(-3.09781019267902,-3.86101403671482,
26.4647141577914));
#51596=CARTESIAN_POINT('Ctrl Pts',(-4.24201965745686,-2.94304733269382,
26.4172495900799));
#51597=CARTESIAN_POINT('Ctrl Pts',(-4.93723014327371,-1.46631393177114,
26.3697850223684));
#51598=CARTESIAN_POINT('Ctrl Pts',(-4.94751652564198,0.00256483971322934,
26.3223204546569));
#51599=CARTESIAN_POINT('Ctrl Pts',(-4.94433041235646,0.00147179461986118,
26.1776795453432));
#51600=CARTESIAN_POINT('Ctrl Pts',(-4.93206642200618,-1.44411412527272,
26.2242935383928));
#51601=CARTESIAN_POINT('Ctrl Pts',(-4.26830822622625,-2.89170283737207,
26.2709075314422));
#51602=CARTESIAN_POINT('Ctrl Pts',(-3.16027114216866,-3.81000496542323,
26.3175215244917));
#51603=CARTESIAN_POINT('Ctrl Pts',(-1.90233119357243,-4.85254131044005,
26.3704417785737));
#51604=CARTESIAN_POINT('Ctrl Pts',(-0.071770729429417,-5.21289273822024,
26.4233620326557));
#51605=CARTESIAN_POINT('Ctrl Pts',(1.48894305049924,-4.72167819128264,26.4762822867377));
#51606=CARTESIAN_POINT('Ctrl Pts',(3.0496568304279,-4.23046364434503,26.5292025408196));
#51607=CARTESIAN_POINT('Ctrl Pts',(4.34052392614221,-2.88768312268964,26.5821227949016));
#51608=CARTESIAN_POINT('Ctrl Pts',(4.77319109373772,-1.30997581823277,26.6350430489835));
#51609=CARTESIAN_POINT('Ctrl Pts',(5.20585826133323,0.267731486224089,26.6879633030655));
#51610=CARTESIAN_POINT('Ctrl Pts',(4.78032550080995,2.08036557348242,26.7408835571475));
#51611=CARTESIAN_POINT('Ctrl Pts',(3.69010138443177,3.29954694578963,26.7938038112294));
#51612=CARTESIAN_POINT('Ctrl Pts',(2.59987726805358,4.51872831809683,26.8467240653114));
#51613=CARTESIAN_POINT('Ctrl Pts',(0.844961795820489,5.14445697545292,26.8996443193934));
#51614=CARTESIAN_POINT('Ctrl Pts',(-0.770932625263734,4.88981277963295,
26.9525645734753));
#51615=CARTESIAN_POINT('Ctrl Pts',(-2.38682704634796,4.63516858381299,27.0054848275573));
#51616=CARTESIAN_POINT('Ctrl Pts',(-3.86370041628332,3.50015153481698,27.0584050816393));
#51617=CARTESIAN_POINT('Ctrl Pts',(-4.52604495623161,2.00446386165791,27.1113253357212));
#51618=CARTESIAN_POINT('Ctrl Pts',(-4.80287247849846,1.37933979454018,27.1334434055952));
#51619=CARTESIAN_POINT('Ctrl Pts',(-4.93741567156095,0.691212705388757,
27.1555614754692));
#51620=CARTESIAN_POINT('Ctrl Pts',(-4.93474635697119,0.00209204260276723,
27.1776795453432));
#51621=CARTESIAN_POINT('Origin',(0.,0.,16.));
#51622=CARTESIAN_POINT('',(-4.93883733219525,-0.00423015144557837,28.3223204546569));
#51623=CARTESIAN_POINT('',(-4.93956784471338,-0.00436622746695347,28.1776795453432));
#51624=CARTESIAN_POINT('',(-4.942,-6.05220448138622E-16,16.));
#51625=CARTESIAN_POINT('Ctrl Pts',(-4.93883733219525,-0.00423015144557837,
28.3223204546569));
#51626=CARTESIAN_POINT('Ctrl Pts',(-4.92943499320705,1.14867573667121,28.2852411506033));
#51627=CARTESIAN_POINT('Ctrl Pts',(-4.52687920768094,2.30749865084404,28.2481618465497));
#51628=CARTESIAN_POINT('Ctrl Pts',(-3.78946858460819,3.18489002165513,28.2110825424962));
#51629=CARTESIAN_POINT('Ctrl Pts',(-2.73702279222337,4.43711887162355,28.1581622884142));
#51630=CARTESIAN_POINT('Ctrl Pts',(-1.00249392936347,5.11608531143494,28.1052420343322));
#51631=CARTESIAN_POINT('Ctrl Pts',(0.62037219239006,4.91108322945104,28.0523217802503));
#51632=CARTESIAN_POINT('Ctrl Pts',(2.2432383141436,4.70608114746714,27.9994015261683));
#51633=CARTESIAN_POINT('Ctrl Pts',(3.75444169479077,3.61711054368793,27.9464812720863));
#51634=CARTESIAN_POINT('Ctrl Pts',(4.46243050532182,2.1425023369291,27.8935610180044));
#51635=CARTESIAN_POINT('Ctrl Pts',(5.17041931585287,0.667894130170271,27.8406407639224));
#51636=CARTESIAN_POINT('Ctrl Pts',(5.07519355626782,-1.19235167956817,27.7877205098404));
#51637=CARTESIAN_POINT('Ctrl Pts',(4.22033397580047,-2.58696076330049,27.7348002557585));
#51638=CARTESIAN_POINT('Ctrl Pts',(3.36547439533311,-3.98156984703282,27.6818800016765));
#51639=CARTESIAN_POINT('Ctrl Pts',(1.75098099398345,-4.91054220475902,27.6289597475946));
#51640=CARTESIAN_POINT('Ctrl Pts',(0.115662973237938,-4.94876098597613,
27.5760394935126));
#51641=CARTESIAN_POINT('Ctrl Pts',(-1.51965504750756,-4.98697976719323,
27.5231192394306));
#51642=CARTESIAN_POINT('Ctrl Pts',(-3.17579768764892,-4.13444497190124,
27.4701989853487));
#51643=CARTESIAN_POINT('Ctrl Pts',(-4.09487415524911,-2.78129895002674,
27.4172787312667));
#51644=CARTESIAN_POINT('Ctrl Pts',(-4.6445938479574,-1.97195278400361,27.3856259723968));
#51645=CARTESIAN_POINT('Ctrl Pts',(-4.9306283269799,-0.98351309398954,27.3539732135268));
#51646=CARTESIAN_POINT('Ctrl Pts',(-4.93516121822955,0.00250487983550263,
27.3223204546569));
#51647=CARTESIAN_POINT('Ctrl Pts',(-4.93474635697119,0.00209204260276723,
27.1776795453432));
#51648=CARTESIAN_POINT('Ctrl Pts',(-4.93102900187776,-0.957594843168012,
27.2084817295512));
#51649=CARTESIAN_POINT('Ctrl Pts',(-4.66120098345796,-1.91920867090262,
27.2392839137591));
#51650=CARTESIAN_POINT('Ctrl Pts',(-4.13896060662357,-2.7152702966968,27.2700860979671));
#51651=CARTESIAN_POINT('Ctrl Pts',(-3.24171600710599,-4.08295848457032,
27.3230063520491));
#51652=CARTESIAN_POINT('Ctrl Pts',(-1.59941109810958,-4.96197656299522,
27.375926606131));
#51653=CARTESIAN_POINT('Ctrl Pts',(0.0363198151755977,-4.94999037586593,
27.428846860213));
#51654=CARTESIAN_POINT('Ctrl Pts',(1.67205072846078,-4.93800418873663,27.481767114295));
#51655=CARTESIAN_POINT('Ctrl Pts',(3.30120764603473,-4.03501373605313,27.5346873683769));
#51656=CARTESIAN_POINT('Ctrl Pts',(4.17831072893992,-2.65428408264511,27.5876076224589));
#51657=CARTESIAN_POINT('Ctrl Pts',(5.0554138118451,-1.27355442923711,27.6405278765408));
#51658=CARTESIAN_POINT('Ctrl Pts',(5.18046306008153,0.584914424895401,27.6934481306228));
#51659=CARTESIAN_POINT('Ctrl Pts',(4.49620935947501,2.07068111644173,27.7463683847048));
#51660=CARTESIAN_POINT('Ctrl Pts',(3.81195565886849,3.55644780798807,27.7992886387867));
#51661=CARTESIAN_POINT('Ctrl Pts',(2.318399009419,4.66951233694822,27.8522088928687));
#51662=CARTESIAN_POINT('Ctrl Pts',(0.69902662395141,4.900507696898,27.9051291469507));
#51663=CARTESIAN_POINT('Ctrl Pts',(-0.920345761516168,5.13150305684779,
27.9580494010326));
#51664=CARTESIAN_POINT('Ctrl Pts',(-2.66553388300184,4.48042924778721,28.0109696551146));
#51665=CARTESIAN_POINT('Ctrl Pts',(-3.73791972674343,3.24523368575399,28.0638899091965));
#51666=CARTESIAN_POINT('Ctrl Pts',(-4.5065378238221,2.35992391786528,28.1018197879121));
#51667=CARTESIAN_POINT('Ctrl Pts',(-4.92952982972571,1.17454424098757,28.1397496666277));
#51668=CARTESIAN_POINT('Ctrl Pts',(-4.93956784471338,-0.00436622746695347,
28.1776795453432));
#51669=CARTESIAN_POINT('Origin',(0.,0.,16.));
#51670=CARTESIAN_POINT('',(-4.95011095070931,-1.6828919353247E-5,29.3223204546569));
#51671=CARTESIAN_POINT('',(-4.9500545842803,0.000473333830474247,29.1776795453432));
#51672=CARTESIAN_POINT('',(-4.942,-6.05220448138622E-16,16.));
#51673=CARTESIAN_POINT('Ctrl Pts',(-4.95011089075521,-1.68287949581236E-5,
29.3223204546569));
#51674=CARTESIAN_POINT('Ctrl Pts',(-4.95002830796364,1.63484509113909,29.2694293417618));
#51675=CARTESIAN_POINT('Ctrl Pts',(-4.06015814856933,3.2697840224184,29.2165382288666));
#51676=CARTESIAN_POINT('Ctrl Pts',(-2.68714856385847,4.15726245203154,29.1636471159715));
#51677=CARTESIAN_POINT('Ctrl Pts',(-1.31338249801809,5.04522985178176,29.1107268618895));
#51678=CARTESIAN_POINT('Ctrl Pts',(0.544055526265072,5.1849128728298,29.0578066078076));
#51679=CARTESIAN_POINT('Ctrl Pts',(2.03517352301083,4.51239041724249,29.0048863537256));
#51680=CARTESIAN_POINT('Ctrl Pts',(3.52629151975661,3.83986796165517,28.9519660996436));
#51681=CARTESIAN_POINT('Ctrl Pts',(4.65108948896497,2.3551400294325,28.8990458455617));
#51682=CARTESIAN_POINT('Ctrl Pts',(4.89484265904535,0.737640825291349,28.8461255914797));
#51683=CARTESIAN_POINT('Ctrl Pts',(5.13859582912572,-0.879858378849781,
28.7932053373978));
#51684=CARTESIAN_POINT('Ctrl Pts',(4.50130420007813,-2.63012885490939,28.7402850833158));
#51685=CARTESIAN_POINT('Ctrl Pts',(3.27460223530322,-3.71222015364772,28.6873648292338));
#51686=CARTESIAN_POINT('Ctrl Pts',(2.04790027052829,-4.79431145238607,28.6344445751519));
#51687=CARTESIAN_POINT('Ctrl Pts',(0.231787970026049,-5.20822357380314,
28.5815243210699));
#51688=CARTESIAN_POINT('Ctrl Pts',(-1.34265409528112,-4.76454391006902,
28.5286040669879));
#51689=CARTESIAN_POINT('Ctrl Pts',(-2.91709616058829,-4.3208642463349,28.475683812906));
#51690=CARTESIAN_POINT('Ctrl Pts',(-4.24986799070038,-3.01959279744957,
28.422763558824));
#51691=CARTESIAN_POINT('Ctrl Pts',(-4.73107254480156,-1.45621144294418,
28.369843304742));
#51692=CARTESIAN_POINT('Ctrl Pts',(-4.87511450807598,-0.988234742120547,
28.3540023547137));
#51693=CARTESIAN_POINT('Ctrl Pts',(-4.94285418164439,-0.496772420704347,
28.3381614046853));
#51694=CARTESIAN_POINT('Ctrl Pts',(-4.93883733219525,-0.00423015144557837,
28.3223204546569));
#51695=CARTESIAN_POINT('Ctrl Pts',(-4.93956784471338,-0.00436622746695347,
28.1776795453432));
#51696=CARTESIAN_POINT('Ctrl Pts',(-4.9435349971983,-0.470286790462875,
28.1926699207096));
#51697=CARTESIAN_POINT('Ctrl Pts',(-4.88300154657712,-0.935196907127989,
28.207660296076));
#51698=CARTESIAN_POINT('Ctrl Pts',(-4.75381137141076,-1.38017405347592,
28.2226506714425));
#51699=CARTESIAN_POINT('Ctrl Pts',(-4.29773360633903,-2.95106891566672,
28.2755709255244));
#51700=CARTESIAN_POINT('Ctrl Pts',(-2.98599451019808,-4.27354132504245,
28.3284911796064));
#51701=CARTESIAN_POINT('Ctrl Pts',(-1.41886776017779,-4.74240604726615,
28.3814114336883));
#51702=CARTESIAN_POINT('Ctrl Pts',(0.148258989842506,-5.21127076948986,
28.4343316877703));
#51703=CARTESIAN_POINT('Ctrl Pts',(1.97077339374215,-4.82652780456152,28.4872519418523));
#51704=CARTESIAN_POINT('Ctrl Pts',(3.21466598259635,-3.76424227707361,28.5401721959342));
#51705=CARTESIAN_POINT('Ctrl Pts',(4.45855857145055,-2.7019567495857,28.5930924500162));
#51706=CARTESIAN_POINT('Ctrl Pts',(5.1238293452593,-0.962128659538206,28.6460127040981));
#51707=CARTESIAN_POINT('Ctrl Pts',(4.90603973778863,0.659070540261458,28.6989329581801));
#51708=CARTESIAN_POINT('Ctrl Pts',(4.68825013031796,2.28026974006111,28.7518532122621));
#51709=CARTESIAN_POINT('Ctrl Pts',(3.58740014156788,3.78284004961294,28.8047734663441));
#51710=CARTESIAN_POINT('Ctrl Pts',(2.10725580021387,4.47918211041389,28.857693720426));
#51711=CARTESIAN_POINT('Ctrl Pts',(0.627111458859856,5.17552417121484,28.910613974508));
#51712=CARTESIAN_POINT('Ctrl Pts',(-1.23232723509808,5.0656379832649,28.9635342285899));
#51713=CARTESIAN_POINT('Ctrl Pts',(-2.62015287286002,4.19980926793105,29.0164544826719));
#51714=CARTESIAN_POINT('Ctrl Pts',(-4.00797851062198,3.33398055259719,29.0693747367538));
#51715=CARTESIAN_POINT('Ctrl Pts',(-4.92419109218792,1.71220930987939,29.1222949908358));
#51716=CARTESIAN_POINT('Ctrl Pts',(-4.94951767608282,0.0766427647882502,
29.1752152449178));
#51717=CARTESIAN_POINT('Ctrl Pts',(-4.94991079785034,0.0512553373413882,
29.1760366783929));
#51718=CARTESIAN_POINT('Ctrl Pts',(-4.95008927347619,0.0258645861152391,
29.1768581118681));
#51719=CARTESIAN_POINT('Ctrl Pts',(-4.9500545842803,0.000473333830474247,
29.1776795453432));
#51720=CARTESIAN_POINT('Origin',(0.,0.,16.));
#51721=CARTESIAN_POINT('',(-4.93888642291793,0.00424076360118208,30.3223204546569));
#51722=CARTESIAN_POINT('',(-4.93818673588435,0.0040670116119004,30.1776795453432));
#51723=CARTESIAN_POINT('',(-4.942,-6.05220448138622E-16,16.));
#51724=CARTESIAN_POINT('Ctrl Pts',(-4.93888642291793,0.00424076360118208,
30.3223204546569));
#51725=CARTESIAN_POINT('Ctrl Pts',(-4.94290141421135,0.49495855667818,30.3065377870022));
#51726=CARTESIAN_POINT('Ctrl Pts',(-4.87566910369714,0.984600773625852,
30.2907551193474));
#51727=CARTESIAN_POINT('Ctrl Pts',(-4.7326693925228,1.45101307944963,30.2749724516927));
#51728=CARTESIAN_POINT('Ctrl Pts',(-4.25318257733109,3.01492218981842,30.2220521976108));
#51729=CARTESIAN_POINT('Ctrl Pts',(-2.92184129195003,4.31765692360063,30.1691319435288));
#51730=CARTESIAN_POINT('Ctrl Pts',(-1.3478876419775,4.76306597049205,30.1162116894468));
#51731=CARTESIAN_POINT('Ctrl Pts',(0.226066007995039,5.20847501738348,30.0632914353649));
#51732=CARTESIAN_POINT('Ctrl Pts',(2.04263202255905,4.79655837738413,30.0103711812829));
#51733=CARTESIAN_POINT('Ctrl Pts',(3.27052205003055,3.71581539574951,29.9574509272009));
#51734=CARTESIAN_POINT('Ctrl Pts',(4.49841207750204,2.6350724141149,29.904530673119));
#51735=CARTESIAN_POINT('Ctrl Pts',(5.13762611788102,0.885503090845023,29.851610419037));
#51736=CARTESIAN_POINT('Ctrl Pts',(4.89565006291192,-0.732262930536752,
29.798690164955));
#51737=CARTESIAN_POINT('Ctrl Pts',(4.65367400794282,-2.35002895191851,29.7457699108731));
#51738=CARTESIAN_POINT('Ctrl Pts',(3.53050785762567,-3.83599167141216,29.6928496567911));
#51739=CARTESIAN_POINT('Ctrl Pts',(2.04012959776072,-4.51015185496902,29.6399294027091));
#51740=CARTESIAN_POINT('Ctrl Pts',(0.549751337895761,-5.18431203852589,
29.5870091486272));
#51741=CARTESIAN_POINT('Ctrl Pts',(-1.307839031517,-5.04666968614595,29.5340888945452));
#51742=CARTESIAN_POINT('Ctrl Pts',(-2.68257979015076,-4.16021203843222,
29.4811686404633));
#51743=CARTESIAN_POINT('Ctrl Pts',(-4.05807756664059,-3.27326625194488,
29.4282192451945));
#51744=CARTESIAN_POINT('Ctrl Pts',(-4.95019356454733,-1.6366802542765,29.3752698499257));
#51745=CARTESIAN_POINT('Ctrl Pts',(-4.95011089075521,-1.68287949581236E-5,
29.3223204546569));
#51746=CARTESIAN_POINT('Ctrl Pts',(-4.9500545842803,0.000473333830474247,
29.1776795453432));
#51747=CARTESIAN_POINT('Ctrl Pts',(-4.94785444726563,-1.60994837137546,
29.2297783659501));
#51748=CARTESIAN_POINT('Ctrl Pts',(-4.08816932384676,-3.22238565418073,
29.2818771865568));
#51749=CARTESIAN_POINT('Ctrl Pts',(-2.74893267905414,-4.11666957233305,
29.3339760071636));
#51750=CARTESIAN_POINT('Ctrl Pts',(-1.38858051190673,-5.0250535168987,29.3868962612456));
#51751=CARTESIAN_POINT('Ctrl Pts',(0.466564408611941,-5.19245955856552,
29.4398165153276));
#51752=CARTESIAN_POINT('Ctrl Pts',(1.96755945318719,-4.54228015350161,29.4927367694096));
#51753=CARTESIAN_POINT('Ctrl Pts',(3.46855449776245,-3.8921007484377,29.5456570234915));
#51754=CARTESIAN_POINT('Ctrl Pts',(4.61539966639428,-2.42433589664307,29.5985772775735));
#51755=CARTESIAN_POINT('Ctrl Pts',(4.88328108437524,-0.810657201852559,
29.6514975316554));
#51756=CARTESIAN_POINT('Ctrl Pts',(5.15116250235621,0.803021492937955,29.7044177857374));
#51757=CARTESIAN_POINT('Ctrl Pts',(4.54008016968629,2.56261403072434,29.7573380398194));
#51758=CARTESIAN_POINT('Ctrl Pts',(3.3296746999557,3.66290398769728,29.8102582939013));
#51759=CARTESIAN_POINT('Ctrl Pts',(2.11926923022511,4.76319394467022,29.8631785479833));
#51760=CARTESIAN_POINT('Ctrl Pts',(0.309540623433855,5.20418132082974,29.9160988020653));
#51761=CARTESIAN_POINT('Ctrl Pts',(-1.27135167326916,4.78406356027939,29.9690190561472));
#51762=CARTESIAN_POINT('Ctrl Pts',(-2.85224396997218,4.36394579972904,30.0219393102292));
#51763=CARTESIAN_POINT('Ctrl Pts',(-4.20429995658695,3.0827229024688,30.0748595643112));
#51764=CARTESIAN_POINT('Ctrl Pts',(-4.70879816265426,1.5267020327104,30.1277798183931));
#51765=CARTESIAN_POINT('Ctrl Pts',(-4.86736582366476,1.03763272218799,30.1444130607098));
#51766=CARTESIAN_POINT('Ctrl Pts',(-4.94220382950374,0.521416307353422,
30.1610463030265));
#51767=CARTESIAN_POINT('Ctrl Pts',(-4.93818673588435,0.0040670116119004,
30.1776795453432));
#51768=CARTESIAN_POINT('Origin',(0.,0.,16.));
#51769=CARTESIAN_POINT('',(-4.9351415428321,-0.00248504100164359,31.3223204546569));
#51770=CARTESIAN_POINT('',(-4.93557330743154,-0.0028385321285674,31.1776795453432));
#51771=CARTESIAN_POINT('',(-4.942,-6.05220448138622E-16,16.));
#51772=CARTESIAN_POINT('Ctrl Pts',(-4.9351415428321,-0.00248504100164359,
31.3223204546569));
#51773=CARTESIAN_POINT('Ctrl Pts',(-4.93066017409234,0.981733357670619,
31.2907259781606));
#51774=CARTESIAN_POINT('Ctrl Pts',(-4.6457448695693,1.96834170751759,31.2591315016643));
#51775=CARTESIAN_POINT('Ctrl Pts',(-4.09792294976925,2.77680140323666,31.227537025168));
#51776=CARTESIAN_POINT('Ctrl Pts',(-3.18032980050788,4.13095875151604,31.1746167710861));
#51777=CARTESIAN_POINT('Ctrl Pts',(-1.52513305096331,4.98530711426681,31.1216965170041));
#51778=CARTESIAN_POINT('Ctrl Pts',(0.110223986946674,4.94888363249201,31.0687762629222));
#51779=CARTESIAN_POINT('Ctrl Pts',(1.74558102485669,4.91246015071721,31.0158560088402));
#51780=CARTESIAN_POINT('Ctrl Pts',(3.36109835113211,3.98526482441679,30.9629357547582));
#51781=CARTESIAN_POINT('Ctrl Pts',(4.2174905639687,2.59159639567501,30.9100155006763));
#51782=CARTESIAN_POINT('Ctrl Pts',(5.0738827768053,1.19792796693324,30.8570952465943));
#51783=CARTESIAN_POINT('Ctrl Pts',(5.17114987620307,-0.662213564249888,
30.8041749925123));
#51784=CARTESIAN_POINT('Ctrl Pts',(4.46478095192916,-2.13759902381238,30.7512547384304));
#51785=CARTESIAN_POINT('Ctrl Pts',(3.75841202765526,-3.61298448337487,30.6983344843484));
#51786=CARTESIAN_POINT('Ctrl Pts',(2.2484070797097,-4.70361387131672,30.6454142302665));
#51787=CARTESIAN_POINT('Ctrl Pts',(0.625767434156371,-4.91039852288288,
30.5924939761845));
#51788=CARTESIAN_POINT('Ctrl Pts',(-0.996872211396971,-5.11718317444904,
30.5395737221025));
#51789=CARTESIAN_POINT('Ctrl Pts',(-2.73214655455809,-4.44012308963949,
30.4866534680206));
#51790=CARTESIAN_POINT('Ctrl Pts',(-3.78596755363747,-3.18905130375701,
30.4337332139386));
#51791=CARTESIAN_POINT('Ctrl Pts',(-4.52550233311024,-2.31109280977609,
30.3965956275114));
#51792=CARTESIAN_POINT('Ctrl Pts',(-4.92943890178742,-1.1504483453926,30.3594580410841));
#51793=CARTESIAN_POINT('Ctrl Pts',(-4.93888642291793,0.00424076360118208,
30.3223204546569));
#51794=CARTESIAN_POINT('Ctrl Pts',(-4.93818673588435,0.0040670116119004,
30.1776795453432));
#51795=CARTESIAN_POINT('Ctrl Pts',(-4.92942306127099,-1.12458004491972,
30.2139665571085));
#51796=CARTESIAN_POINT('Ctrl Pts',(-4.54535955813864,-2.25861888984588,
30.2502535688737));
#51797=CARTESIAN_POINT('Ctrl Pts',(-3.83660874069347,-3.12794382961597,
30.286540580639));
#51798=CARTESIAN_POINT('Ctrl Pts',(-2.80298068714555,-4.39574997992736,
30.339460834721));
#51799=CARTESIAN_POINT('Ctrl Pts',(-1.0787841545299,-5.10054343829356,30.3923810888029));
#51800=CARTESIAN_POINT('Ctrl Pts',(0.546962191086786,-4.91979995442398,
30.4453013428849));
#51801=CARTESIAN_POINT('Ctrl Pts',(2.17270853670347,-4.73905647055441,30.4982215969669));
#51802=CARTESIAN_POINT('Ctrl Pts',(3.7000046953212,-3.67277604444905,30.5511418510488));
#51803=CARTESIAN_POINT('Ctrl Pts',(4.4299366186172,-2.20890488388769,30.6040621051308));
#51804=CARTESIAN_POINT('Ctrl Pts',(5.1598685419132,-0.745033723326325,30.6569823592128));
#51805=CARTESIAN_POINT('Ctrl Pts',(5.09243622988746,1.11642817169105,30.7099026132947));
#51806=CARTESIAN_POINT('Ctrl Pts',(4.25849773850338,2.52364740836047,30.7628228673767));
#51807=CARTESIAN_POINT('Ctrl Pts',(3.42455924711931,3.93086664502988,30.8157431214587));
#51808=CARTESIAN_POINT('Ctrl Pts',(1.8241145763769,4.88384322335134,30.8686633755406));
#51809=CARTESIAN_POINT('Ctrl Pts',(0.189551650661496,4.9464805066113,30.9215836296226));
#51810=CARTESIAN_POINT('Ctrl Pts',(-1.44501127505389,5.00911778987126,30.9745038837045));
#51811=CARTESIAN_POINT('Ctrl Pts',(-3.11369245574226,4.18141577806974,31.0274241377865));
#51812=CARTESIAN_POINT('Ctrl Pts',(-4.05287789782628,2.84214355302423,31.0803443918685));
#51813=CARTESIAN_POINT('Ctrl Pts',(-4.62868616337827,2.0210447769463,31.1127894430267));
#51814=CARTESIAN_POINT('Ctrl Pts',(-4.93028912913986,1.0076552769297,31.145234494185));
#51815=CARTESIAN_POINT('Ctrl Pts',(-4.93557330743154,-0.0028385321285674,
31.1776795453432));
#51816=CARTESIAN_POINT('Origin',(0.,0.,16.));
#51817=CARTESIAN_POINT('',(-4.94795422753399,-0.0028972882267797,32.3223204546569));
#51818=CARTESIAN_POINT('',(-4.94851874366221,-0.00251525819571033,32.1776795453432));
#51819=CARTESIAN_POINT('',(-4.942,-6.05220448138622E-16,16.));
#51820=CARTESIAN_POINT('Ctrl Pts',(-4.94795422753399,-0.0028972882267797,
32.3223204546569));
#51821=CARTESIAN_POINT('Ctrl Pts',(-4.93774012235113,1.46412544671205,32.2749141693191));
#51822=CARTESIAN_POINT('Ctrl Pts',(-4.24380482164535,2.93954073272814,32.2275078839812));
#51823=CARTESIAN_POINT('Ctrl Pts',(-3.10183998936669,3.85774379859783,32.1801015986434));
#51824=CARTESIAN_POINT('Ctrl Pts',(-1.82704976595674,4.88274584628794,32.1271813445614));
#51825=CARTESIAN_POINT('Ctrl Pts',(0.00605460139836145,5.21337522038518,
32.0742610904795));
#51826=CARTESIAN_POINT('Ctrl Pts',(1.55861655774584,4.69833086969986,32.0213408363975));
#51827=CARTESIAN_POINT('Ctrl Pts',(3.11117851409333,4.18328651901453,31.9684205823155));
#51828=CARTESIAN_POINT('Ctrl Pts',(4.38319805943319,2.82256844354664,31.9155003282335));
#51829=CARTESIAN_POINT('Ctrl Pts',(4.79257962264663,1.23886201646757,31.8625800741516));
#51830=CARTESIAN_POINT('Ctrl Pts',(5.20196118586006,-0.344844410611489,
31.8096598200696));
#51831=CARTESIAN_POINT('Ctrl Pts',(4.74870476694708,-2.15153918930172,31.7567395659877));
#51832=CARTESIAN_POINT('Ctrl Pts',(3.64022742565071,-3.35445119576896,31.7038193119057));
#51833=CARTESIAN_POINT('Ctrl Pts',(2.53175008435434,-4.5573632022362,31.6508990578238));
#51834=CARTESIAN_POINT('Ctrl Pts',(0.768051820674579,-5.15649243648045,
31.5979788037418));
#51835=CARTESIAN_POINT('Ctrl Pts',(-0.843772103495588,-4.87766821059161,
31.5450585496598));
#51836=CARTESIAN_POINT('Ctrl Pts',(-2.45559602766576,-4.59884398470276,
31.4921382955779));
#51837=CARTESIAN_POINT('Ctrl Pts',(-3.91554561232635,-3.44206629868081,
31.4392180414959));
#51838=CARTESIAN_POINT('Ctrl Pts',(-4.55552563016757,-1.93669428876581,
31.386297787414));
#51839=CARTESIAN_POINT('Ctrl Pts',(-4.81342445844275,-1.33006022730727,
31.3649720098283));
#51840=CARTESIAN_POINT('Ctrl Pts',(-4.93816639665535,-0.66681706968053,
31.3436462322426));
#51841=CARTESIAN_POINT('Ctrl Pts',(-4.9351415428321,-0.00248504100164359,
31.3223204546569));
#51842=CARTESIAN_POINT('Ctrl Pts',(-4.93557330743154,-0.0028385321285674,
31.1776795453432));
#51843=CARTESIAN_POINT('Ctrl Pts',(-4.93890801084376,-0.640534114505631,
31.1981547482669));
#51844=CARTESIAN_POINT('Ctrl Pts',(-4.82423274680824,-1.27707647808528,
31.2186299511906));
#51845=CARTESIAN_POINT('Ctrl Pts',(-4.58598979744053,-1.86340999470999,
31.2391051541143));
#51846=CARTESIAN_POINT('Ctrl Pts',(-3.97022655149108,-3.3788488791092,31.2920254081963));
#51847=CARTESIAN_POINT('Ctrl Pts',(-2.5290103561125,-4.55888420961813,31.3449456622783));
#51848=CARTESIAN_POINT('Ctrl Pts',(-0.921863753563045,-4.86351379667883,
31.3978659163602));
#51849=CARTESIAN_POINT('Ctrl Pts',(0.685282848986421,-5.16814338373953,
31.4507861704422));
#51850=CARTESIAN_POINT('Ctrl Pts',(2.45835985870677,-4.59736722735202,31.5037064245242));
#51851=CARTESIAN_POINT('Ctrl Pts',(3.5859801562746,-3.4123812139678,31.5566266786061));
#51852=CARTESIAN_POINT('Ctrl Pts',(4.71360045384243,-2.22739520058358,31.6095469326881));
#51853=CARTESIAN_POINT('Ctrl Pts',(5.19576403925773,-0.428199330202661,
31.6624671867701));
#51854=CARTESIAN_POINT('Ctrl Pts',(4.81182549189739,1.16186688830996,31.715387440852));
#51855=CARTESIAN_POINT('Ctrl Pts',(4.42788694453706,2.75193310682255,31.768307694934));
#51856=CARTESIAN_POINT('Ctrl Pts',(3.17784626440109,4.13286967346687,31.8212279490159));
#51857=CARTESIAN_POINT('Ctrl Pts',(1.63374115821347,4.67273892471915,31.8741482030979));
#51858=CARTESIAN_POINT('Ctrl Pts',(0.0896360520258116,5.21260817597145,
31.9270684571799));
#51859=CARTESIAN_POINT('Ctrl Pts',(-1.74853348021352,4.91141011183171,31.9799887112618));
#51860=CARTESIAN_POINT('Ctrl Pts',(-3.0395929867415,3.90697756655707,32.0329089653438));
#51861=CARTESIAN_POINT('Ctrl Pts',(-4.21688283424399,2.99105678050979,32.0811658253436));
#51862=CARTESIAN_POINT('Ctrl Pts',(-4.93923809973741,1.49038033345358,32.1294226853434));
#51863=CARTESIAN_POINT('Ctrl Pts',(-4.94851874366221,-0.00251525819571033,
32.1776795453432));
#51864=CARTESIAN_POINT('Origin',(0.,0.,16.));
#51865=CARTESIAN_POINT('',(-4.94391378591308,0.00432614989180041,33.3223204546569));
#51866=CARTESIAN_POINT('',(-4.943114998001,0.00443591996608837,33.1776795453432));
#51867=CARTESIAN_POINT('',(-4.942,-6.05220448138622E-16,16.));
#51868=CARTESIAN_POINT('Ctrl Pts',(-4.94391378591308,0.00432614989180041,
33.3223204546569));
#51869=CARTESIAN_POINT('Ctrl Pts',(-4.94684012248784,0.323678273041629,
33.3120226145595));
#51870=CARTESIAN_POINT('Ctrl Pts',(-4.91854579890533,0.642514059921896,
33.3017247744621));
#51871=CARTESIAN_POINT('Ctrl Pts',(-4.8571468315969,0.954841972036427,33.2914269343646));
#51872=CARTESIAN_POINT('Ctrl Pts',(-4.54161960262542,2.55988461298029,33.2385066802827));
#51873=CARTESIAN_POINT('Ctrl Pts',(-3.3518326489115,3.99306094874791,33.1855864262007));
#51874=CARTESIAN_POINT('Ctrl Pts',(-1.83225065173251,4.59852759962142,33.1326661721187));
#51875=CARTESIAN_POINT('Ctrl Pts',(-0.312668654553525,5.20399425049493,
33.0797459180367));
#51876=CARTESIAN_POINT('Ctrl Pts',(1.53670838609054,4.98175121647435,33.0268256639548));
#51877=CARTESIAN_POINT('Ctrl Pts',(2.86957729142234,4.03350030417842,32.9739054098728));
#51878=CARTESIAN_POINT('Ctrl Pts',(4.20244619675414,3.0852493918825,32.9209851557909));
#51879=CARTESIAN_POINT('Ctrl Pts',(5.01880696677368,1.41099060131123,32.8680649017089));
#51880=CARTESIAN_POINT('Ctrl Pts',(4.94508044508782,-0.223109674519649,
32.8151446476269));
#51881=CARTESIAN_POINT('Ctrl Pts',(4.87135392340196,-1.85720995035054,32.762224393545));
#51882=CARTESIAN_POINT('Ctrl Pts',(3.90754011001068,-3.45115171144104,32.709304139463));
#51883=CARTESIAN_POINT('Ctrl Pts',(2.49469492595997,-4.27552286412362,32.6563838853811));
#51884=CARTESIAN_POINT('Ctrl Pts',(1.08184974190924,-5.0998940168062,32.6034636312991));
#51885=CARTESIAN_POINT('Ctrl Pts',(-0.780026812800927,-5.15469456108083,
32.5505433772171));
#51886=CARTESIAN_POINT('Ctrl Pts',(-2.2389115908552,-4.41484693093525,32.4976231231352));
#51887=CARTESIAN_POINT('Ctrl Pts',(-3.69779636890945,-3.67499930078968,
32.4447028690532));
#51888=CARTESIAN_POINT('Ctrl Pts',(-4.75368937030783,-2.14050349622394,
32.3917826149712));
#51889=CARTESIAN_POINT('Ctrl Pts',(-4.92339783127462,-0.513568233299591,
32.3388623608893));
#51890=CARTESIAN_POINT('Ctrl Pts',(-4.94108042115667,-0.344051469933491,
32.3333483921451));
#51891=CARTESIAN_POINT('Ctrl Pts',(-4.94914226106849,-0.173531149322059,
32.327834423401));
#51892=CARTESIAN_POINT('Ctrl Pts',(-4.94795422753399,-0.0028972882267797,
32.3223204546569));
#51893=CARTESIAN_POINT('Ctrl Pts',(-4.94851874366221,-0.00251525819571033,
32.1776795453432));
#51894=CARTESIAN_POINT('Ctrl Pts',(-4.94941559646112,-0.146784082719192,
32.1823429394254));
#51895=CARTESIAN_POINT('Ctrl Pts',(-4.9436532640282,-0.290980244219974,
32.1870063335075));
#51896=CARTESIAN_POINT('Ctrl Pts',(-4.93099878465363,-0.434569000702025,
32.1916697275897));
#51897=CARTESIAN_POINT('Ctrl Pts',(-4.78739559522113,-2.06401599627693,
32.2445899816717));
#51898=CARTESIAN_POINT('Ctrl Pts',(-3.75623973553951,-3.61524296101718,
32.2975102357536));
#51899=CARTESIAN_POINT('Ctrl Pts',(-2.30940387553184,-4.3783847444355,32.3504304898356));
#51900=CARTESIAN_POINT('Ctrl Pts',(-0.862568015524189,-5.14152652785381,
32.4033507439175));
#51901=CARTESIAN_POINT('Ctrl Pts',(0.999947844809495,-5.11658312995021,
32.4562709979995));
#51902=CARTESIAN_POINT('Ctrl Pts',(2.4258280021366,-4.3149690305583,32.5091912520815));
#51903=CARTESIAN_POINT('Ctrl Pts',(3.85170815946372,-3.51335493116639,32.5621115061634));
#51904=CARTESIAN_POINT('Ctrl Pts',(4.84095261378425,-1.93507013028614,32.6150317602454));
#51905=CARTESIAN_POINT('Ctrl Pts',(4.9408679943685,-0.30236185746891,32.6679520143274));
#51906=CARTESIAN_POINT('Ctrl Pts',(5.04078337495275,1.33034641534833,32.7208722684093));
#51907=CARTESIAN_POINT('Ctrl Pts',(4.25136968180072,3.01747816010256,32.7737925224913));
#51908=CARTESIAN_POINT('Ctrl Pts',(2.93387467737636,3.9869761233392,32.8267127765732));
#51909=CARTESIAN_POINT('Ctrl Pts',(1.616379672952,4.95647408657584,32.8796330306552));
#51910=CARTESIAN_POINT('Ctrl Pts',(-0.229196642744684,5.20833826829488,
32.9325532847372));
#51911=CARTESIAN_POINT('Ctrl Pts',(-1.75829036071957,4.62731177229585,32.9854735388191));
#51912=CARTESIAN_POINT('Ctrl Pts',(-3.28738407869442,4.04628527629685,33.0383937929011));
#51913=CARTESIAN_POINT('Ctrl Pts',(-4.49999519894748,2.63236810257984,33.091314046983));
#51914=CARTESIAN_POINT('Ctrl Pts',(-4.8412143530065,1.03259034416892,33.144234301065));
#51915=CARTESIAN_POINT('Ctrl Pts',(-4.91309708900794,0.695574086725974,
33.1553827158244));
#51916=CARTESIAN_POINT('Ctrl Pts',(-4.94630788623483,0.350309429675576,
33.1665311305838));
#51917=CARTESIAN_POINT('Ctrl Pts',(-4.943114998001,0.00443591996608837,
33.1776795453432));
#51918=CARTESIAN_POINT('Origin',(0.,0.,16.));
#51919=CARTESIAN_POINT('',(-4.93390856647989,0.000179243442527399,34.3223204546569));
#51920=CARTESIAN_POINT('',(-4.93391474235666,-0.000255694835337854,34.1776795453433));
#51921=CARTESIAN_POINT('',(-4.942,-6.05220448138622E-16,16.));
#51922=CARTESIAN_POINT('Ctrl Pts',(-4.93390856647989,0.000179243442527399,
34.3223204546569));
#51923=CARTESIAN_POINT('Ctrl Pts',(-4.93417188922503,0.81404442559312,34.2962108057179));
#51924=CARTESIAN_POINT('Ctrl Pts',(-4.7439659144325,1.62779374632659,34.2701011567789));
#51925=CARTESIAN_POINT('Ctrl Pts',(-4.36261434797766,2.33905848282458,34.24399150784));
#51926=CARTESIAN_POINT('Ctrl Pts',(-3.58967320891792,3.780683020289,34.191071253758));
#51927=CARTESIAN_POINT('Ctrl Pts',(-2.03148547319181,4.80128989115793,34.138150999676));
#51928=CARTESIAN_POINT('Ctrl Pts',(-0.401101646399658,4.93383380390034,
34.0852307455941));
#51929=CARTESIAN_POINT('Ctrl Pts',(1.22928218039249,5.06637771664275,34.0323104915121));
#51930=CARTESIAN_POINT('Ctrl Pts',(2.93186209825069,4.31085867125863,33.9793902374301));
#51931=CARTESIAN_POINT('Ctrl Pts',(3.92751153377263,3.01301372173064,33.9264699833482));
#51932=CARTESIAN_POINT('Ctrl Pts',(4.92316096929458,1.71516877220265,33.8735497292662));
#51933=CARTESIAN_POINT('Ctrl Pts',(5.21187992248028,-0.125002081469193,
33.8206294751842));
#51934=CARTESIAN_POINT('Ctrl Pts',(4.66154619083434,-1.6654085522694,33.7677092211023));
#51935=CARTESIAN_POINT('Ctrl Pts',(4.1112124591884,-3.2058150230696,33.7147889670203));
#51936=CARTESIAN_POINT('Ctrl Pts',(2.72182604271081,-4.44645711099814,33.6618687129384));
#51937=CARTESIAN_POINT('Ctrl Pts',(1.12919138526205,-4.8195980486659,33.6089484588564));
#51938=CARTESIAN_POINT('Ctrl Pts',(-0.463443272186686,-5.19273898633366,
33.5560282047744));
#51939=CARTESIAN_POINT('Ctrl Pts',(-2.25932617060659,-4.69837877374066,
33.5031079506925));
#51940=CARTESIAN_POINT('Ctrl Pts',(-3.43663386770201,-3.56274419438412,
33.4501876966105));
#51941=CARTESIAN_POINT('Ctrl Pts',(-4.384847305511,-2.64809463314952,33.407565282626));
#51942=CARTESIAN_POINT('Ctrl Pts',(-4.93180177720373,-1.3174615522823,33.3649428686414));
#51943=CARTESIAN_POINT('Ctrl Pts',(-4.94391378591308,0.00432614989180041,
33.3223204546569));
#51944=CARTESIAN_POINT('Ctrl Pts',(-4.943114998001,0.00443591996608837,
33.1776795453432));
#51945=CARTESIAN_POINT('Ctrl Pts',(-4.93115160973848,-1.2915126956278,33.2194513846658));
#51946=CARTESIAN_POINT('Ctrl Pts',(-4.40811124636647,-2.59600908794704,
33.2612232239884));
#51947=CARTESIAN_POINT('Ctrl Pts',(-3.49331109260409,-3.50718930782419,
33.3029950633109));
#51948=CARTESIAN_POINT('Ctrl Pts',(-2.33436149027767,-4.6615528583015,33.3559153173929));
#51949=CARTESIAN_POINT('Ctrl Pts',(-0.54663509775989,-5.18464161615124,
33.4088355714748));
#51950=CARTESIAN_POINT('Ctrl Pts',(1.0517771843263,-4.83708217680429,33.4617558255568));
#51951=CARTESIAN_POINT('Ctrl Pts',(2.65018946641248,-4.48952273745735,33.5146760796387));
#51952=CARTESIAN_POINT('Ctrl Pts',(4.05928763806706,-3.27131510091373,33.5675963337207));
#51953=CARTESIAN_POINT('Ctrl Pts',(4.63424685520885,-1.73992968697417,33.6205165878027));
#51954=CARTESIAN_POINT('Ctrl Pts',(5.20920607235062,-0.208544273034641,
33.6734368418847));
#51955=CARTESIAN_POINT('Ctrl Pts',(4.95002633497964,1.63601891830083,33.7263570959666));
#51956=CARTESIAN_POINT('Ctrl Pts',(3.97531224929094,2.94965959921896,33.7792773500486));
#51957=CARTESIAN_POINT('Ctrl Pts',(3.00059816360222,4.26330028013712,33.8321976041305));
#51958=CARTESIAN_POINT('Ctrl Pts',(1.31034972959575,5.04601845063795,33.8851178582125));
#51959=CARTESIAN_POINT('Ctrl Pts',(-0.321949554671762,4.93963032168135,
33.9380381122945));
#51960=CARTESIAN_POINT('Ctrl Pts',(-1.95424883893928,4.83324219272475,33.9909583663764));
#51961=CARTESIAN_POINT('Ctrl Pts',(-3.52859897346783,3.83774776431073,34.0438786204584));
#51962=CARTESIAN_POINT('Ctrl Pts',(-4.32455329212167,2.40870049076816,34.0967988745404));
#51963=CARTESIAN_POINT('Ctrl Pts',(-4.73005222214988,1.68067235297088,34.1237590981413));
#51964=CARTESIAN_POINT('Ctrl Pts',(-4.93352684267558,0.840120210825594,
34.1507193217423));
#51965=CARTESIAN_POINT('Ctrl Pts',(-4.93391474235666,-0.000255694835337854,
34.1776795453433));
#51966=CARTESIAN_POINT('Origin',(0.,0.,16.));
#51967=CARTESIAN_POINT('',(-4.94325592752636,-0.00441992691212867,35.3223204546569));
#51968=CARTESIAN_POINT('',(-4.94405342481732,-0.00430212276008984,35.1776795453432));
#51969=CARTESIAN_POINT('',(-4.942,-6.05220448138622E-16,16.));
#51970=CARTESIAN_POINT('Ctrl Pts',(-4.94325592752636,-0.00441992691212867,
35.3223204546569));
#51971=CARTESIAN_POINT('Ctrl Pts',(-4.93125773853651,1.29607520943411,35.2803989968764));
#51972=CARTESIAN_POINT('Ctrl Pts',(-4.40405811483643,2.60517623543917,35.2384775390958));
#51973=CARTESIAN_POINT('Ctrl Pts',(-3.48340604301779,3.51702727807467,35.1965560813153));
#51974=CARTESIAN_POINT('Ctrl Pts',(-2.32120548652017,4.66811770803537,35.1436358272333));
#51975=CARTESIAN_POINT('Ctrl Pts',(-0.53201099429802,5.18616256481328,35.0907155731514));
#51976=CARTESIAN_POINT('Ctrl Pts',(1.06541470817911,4.83409661000376,35.0377953190694));
#51977=CARTESIAN_POINT('Ctrl Pts',(2.66284041065621,4.48203065519423,34.9848750649874));
#51978=CARTESIAN_POINT('Ctrl Pts',(4.0684973233883,3.25985388879729,34.9319548109055));
#51979=CARTESIAN_POINT('Ctrl Pts',(4.63913537493446,1.72685306505386,34.8790345568235));
#51980=CARTESIAN_POINT('Ctrl Pts',(5.20977342648062,0.193852241310417,34.8261143027416));
#51981=CARTESIAN_POINT('Ctrl Pts',(4.94539261684082,-1.64997263977952,34.7731940486596));
#51982=CARTESIAN_POINT('Ctrl Pts',(3.96697764231472,-2.96085915244703,34.7202737945776));
#51983=CARTESIAN_POINT('Ctrl Pts',(2.98856266778862,-4.27174566511454,34.6673535404957));
#51984=CARTESIAN_POINT('Ctrl Pts',(1.29611352837622,-5.04969380935962,34.6144332864137));
#51985=CARTESIAN_POINT('Ctrl Pts',(-0.335879201461312,-4.93870263300798,
34.5615130323317));
#51986=CARTESIAN_POINT('Ctrl Pts',(-1.96787193129885,-4.82771145665634,
34.5085927782498));
#51987=CARTESIAN_POINT('Ctrl Pts',(-3.53940825156152,-3.82778095970798,
34.4556725241678));
#51988=CARTESIAN_POINT('Ctrl Pts',(-4.33132914049615,-2.39649460920384,
34.4027522700858));
#51989=CARTESIAN_POINT('Ctrl Pts',(-4.73253428635246,-1.67137236904084,
34.3759416649429));
#51990=CARTESIAN_POINT('Ctrl Pts',(-4.93363817440523,-0.835535479848384,
34.3491310597999));
#51991=CARTESIAN_POINT('Ctrl Pts',(-4.93390856647989,0.000179243442527399,
34.3223204546569));
#51992=CARTESIAN_POINT('Ctrl Pts',(-4.93391474235666,-0.000255694835337854,
34.1776795453433));
#51993=CARTESIAN_POINT('Ctrl Pts',(-4.93428825140812,-0.80945462617062,
34.2036395758242));
#51994=CARTESIAN_POINT('Ctrl Pts',(-4.7463640914517,-1.61849015480256,34.2295996063052));
#51995=CARTESIAN_POINT('Ctrl Pts',(-4.36919376142154,-2.32674560401052,
34.2555596367863));
#51996=CARTESIAN_POINT('Ctrl Pts',(-3.60032140928848,-3.77054430657554,
34.3084798908682));
#51997=CARTESIAN_POINT('Ctrl Pts',(-2.04501820224325,-4.79554159303451,
34.3614001449502));
#51998=CARTESIAN_POINT('Ctrl Pts',(-0.415014641507274,-4.93268305062891,
34.4143203990321));
#51999=CARTESIAN_POINT('Ctrl Pts',(1.21498891922872,-5.0698245082233,34.4672406531141));
#52000=CARTESIAN_POINT('Ctrl Pts',(2.91969283365546,-4.31911013695313,34.5201609071961));
#52001=CARTESIAN_POINT('Ctrl Pts',(3.91899855510175,-3.02407829854611,34.573081161278));
#52002=CARTESIAN_POINT('Ctrl Pts',(4.91830427654803,-1.72904646013911,34.62600141536));
#52003=CARTESIAN_POINT('Ctrl Pts',(5.21221180501386,0.110302845404735,34.678921669442));
#52004=CARTESIAN_POINT('Ctrl Pts',(4.66622456671209,1.65225528404048,34.7318419235239));
#52005=CARTESIAN_POINT('Ctrl Pts',(4.12023732841032,3.19420772267622,34.7847621776059));
#52006=CARTESIAN_POINT('Ctrl Pts',(2.73435532334095,4.43876329440389,34.8376824316879));
#52007=CARTESIAN_POINT('Ctrl Pts',(1.14277932318225,4.81639436187842,34.8906026857698));
#52008=CARTESIAN_POINT('Ctrl Pts',(-0.448796676976434,5.19402542935295,
34.9435229398518));
#52009=CARTESIAN_POINT('Ctrl Pts',(-2.24606667222443,4.70473199257438,34.9964431939337));
#52010=CARTESIAN_POINT('Ctrl Pts',(-3.42657246357288,3.57242220104389,35.0493634480157));
#52011=CARTESIAN_POINT('Ctrl Pts',(-4.38069925079363,2.65724913586347,35.0921354804582));
#52012=CARTESIAN_POINT('Ctrl Pts',(-4.93192805452064,1.32202900724285,35.1349075129007));
#52013=CARTESIAN_POINT('Ctrl Pts',(-4.94405342481732,-0.00430212276008983,
35.1776795453432));
#52014=CARTESIAN_POINT('Origin',(0.,0.,16.));
#52015=CARTESIAN_POINT('',(-4.94842418382236,0.0025848059749288,36.3223204546569));
#52016=CARTESIAN_POINT('',(-4.9478484900732,0.00296101277178129,36.1776795453433));
#52017=CARTESIAN_POINT('',(-4.942,-6.05220448138622E-16,16.));
#52018=CARTESIAN_POINT('Ctrl Pts',(-4.94842418382236,0.0025848059749288,
36.3223204546569));
#52019=CARTESIAN_POINT('Ctrl Pts',(-4.94937063025513,0.151489796715591,
36.3175074421168));
#52020=CARTESIAN_POINT('Ctrl Pts',(-4.94323189211144,0.300315679824302,
36.3126944295766));
#52021=CARTESIAN_POINT('Ctrl Pts',(-4.92975351682066,0.448473855033485,
36.3078814170365));
#52022=CARTESIAN_POINT('Ctrl Pts',(-4.78155547265312,2.07750935224505,36.2549611629546));
#52023=CARTESIAN_POINT('Ctrl Pts',(-3.74602889959972,3.62582202129232,36.2020409088726));
#52024=CARTESIAN_POINT('Ctrl Pts',(-2.2970465727752,4.38488033790615,36.1491206547906));
#52025=CARTESIAN_POINT('Ctrl Pts',(-0.848064245950652,5.14393865451998,
36.0962004007087));
#52026=CARTESIAN_POINT('Ctrl Pts',(1.01437383464502,5.11374261870034,36.0432801466267));
#52027=CARTESIAN_POINT('Ctrl Pts',(2.43798755887529,4.30811039761326,35.9903598925447));
#52028=CARTESIAN_POINT('Ctrl Pts',(3.86160128310556,3.50247817652618,35.9374396384628));
#52029=CARTESIAN_POINT('Ctrl Pts',(4.84639065097043,1.92140977017166,35.8845193843808));
#52030=CARTESIAN_POINT('Ctrl Pts',(4.94170100734347,0.28842622847917,35.8315991302989));
#52031=CARTESIAN_POINT('Ctrl Pts',(5.03701136371651,-1.34455731321331,35.7786788762169));
#52032=CARTESIAN_POINT('Ctrl Pts',(4.24284270859772,-3.02945599024377,35.7257586221349));
#52033=CARTESIAN_POINT('Ctrl Pts',(2.92261874766819,-3.99523443505293,35.6728383680529));
#52034=CARTESIAN_POINT('Ctrl Pts',(1.60239478673866,-4.96101287986208,35.619918113971));
#52035=CARTESIAN_POINT('Ctrl Pts',(-0.243884480001596,-5.20767109244996,
35.566997859889));
#52036=CARTESIAN_POINT('Ctrl Pts',(-1.77133346242501,-4.62233450759977,
35.5140776058071));
#52037=CARTESIAN_POINT('Ctrl Pts',(-3.29878244484848,-4.03699792274956,
35.4611573517251));
#52038=CARTESIAN_POINT('Ctrl Pts',(-4.50740114295507,-2.61966654046123,
35.4082370976431));
#52039=CARTESIAN_POINT('Ctrl Pts',(-4.84410718162179,-1.01893284774532,
35.3553168435612));
#52040=CARTESIAN_POINT('Ctrl Pts',(-4.91408721473011,-0.686240873293583,
35.3443180472597));
#52041=CARTESIAN_POINT('Ctrl Pts',(-4.94640385328257,-0.345626598935659,
35.3333192509583));
#52042=CARTESIAN_POINT('Ctrl Pts',(-4.94325592752636,-0.00441992691212867,
35.3223204546569));
#52043=CARTESIAN_POINT('Ctrl Pts',(-4.94405342481732,-0.00430212276008983,
35.1776795453432));
#52044=CARTESIAN_POINT('Ctrl Pts',(-4.94693032680687,-0.318991453753773,
35.1878277669827));
#52045=CARTESIAN_POINT('Ctrl Pts',(-4.91945907962359,-0.633180389759553,
35.1979759886221));
#52046=CARTESIAN_POINT('Ctrl Pts',(-4.85982046564743,-0.941139879242983,
35.2081242102616));
#52047=CARTESIAN_POINT('Ctrl Pts',(-4.54882108892463,-2.5470660217169,35.2610444643436));
#52048=CARTESIAN_POINT('Ctrl Pts',(-3.36308074803015,-3.98359216038229,
35.3139647184255));
#52049=CARTESIAN_POINT('Ctrl Pts',(-1.84521233241245,-4.59334199455474,
35.3668849725075));
#52050=CARTESIAN_POINT('Ctrl Pts',(-0.327343916794751,-5.2030918287272,
35.4198052265894));
#52051=CARTESIAN_POINT('Ctrl Pts',(1.52265257354617,-4.98606535840671,35.4727254806714));
#52052=CARTESIAN_POINT('Ctrl Pts',(2.858190490191,-4.04157721099188,35.5256457347534));
#52053=CARTESIAN_POINT('Ctrl Pts',(4.19372840683581,-3.09708906357705,35.5785659888353));
#52054=CARTESIAN_POINT('Ctrl Pts',(5.01480774978454,-1.42513923906789,35.6314862429173));
#52055=CARTESIAN_POINT('Ctrl Pts',(4.94569007160633,0.20916248765404,35.6844064969993));
#52056=CARTESIAN_POINT('Ctrl Pts',(4.87657239342812,1.843464214376,35.7373267510812));
#52057=CARTESIAN_POINT('Ctrl Pts',(3.91725769412294,3.44011784331073,35.7902470051632));
#52058=CARTESIAN_POINT('Ctrl Pts',(2.50674303141734,4.26847028864764,35.8431672592451));
#52059=CARTESIAN_POINT('Ctrl Pts',(1.09622836871175,5.09682273398456,35.8960875133271));
#52060=CARTESIAN_POINT('Ctrl Pts',(-0.765486257394255,5.15687399572365,
35.9490077674091));
#52061=CARTESIAN_POINT('Ctrl Pts',(-2.2264518005877,4.42114369934827,36.001928021491));
#52062=CARTESIAN_POINT('Ctrl Pts',(-3.68741734378115,3.68541340297289,36.054848275573));
#52063=CARTESIAN_POINT('Ctrl Pts',(-4.74763380406204,2.15390154848305,36.107768529655));
#52064=CARTESIAN_POINT('Ctrl Pts',(-4.92192993683911,0.527451350812649,
36.1606887837369));
#52065=CARTESIAN_POINT('Ctrl Pts',(-4.94058331188609,0.353386757129483,
36.166352370939));
#52066=CARTESIAN_POINT('Ctrl Pts',(-4.94908977224877,0.178234784323597,
36.1720159581411));
#52067=CARTESIAN_POINT('Ctrl Pts',(-4.9478484900732,0.00296101277178129,
36.1776795453433));
#52068=CARTESIAN_POINT('Origin',(0.,0.,16.));
#52069=CARTESIAN_POINT('',(-4.93549302535697,0.00277814199197368,37.3223204546569));
#52070=CARTESIAN_POINT('',(-4.9350718820976,0.00242042316235142,37.1776795453432));
#52071=CARTESIAN_POINT('',(-4.942,-6.05220448138622E-16,16.));
#52072=CARTESIAN_POINT('Ctrl Pts',(-4.93549302535697,0.00277814199197368,
37.3223204546569));
#52073=CARTESIAN_POINT('Ctrl Pts',(-4.93877741300468,0.645159704289348,
37.3016956332752));
#52074=CARTESIAN_POINT('Ctrl Pts',(-4.82236482292357,1.2863972760676,37.2810708118936));
#52075=CARTESIAN_POINT('Ctrl Pts',(-4.5807162353096,1.87633613908203,37.2604459905119));
#52076=CARTESIAN_POINT('Ctrl Pts',(-3.96068154902433,3.39003237653315,37.2075257364299));
#52077=CARTESIAN_POINT('Ctrl Pts',(-2.51614312549289,4.56599842518147,37.1546054823479));
#52078=CARTESIAN_POINT('Ctrl Pts',(-0.908143809323614,4.86609426099016,
37.101685228266));
#52079=CARTESIAN_POINT('Ctrl Pts',(0.699855506845637,5.16619009679885,37.048764974184));
#52080=CARTESIAN_POINT('Ctrl Pts',(2.47131571565271,4.59041571976794,36.995844720102));
#52081=CARTESIAN_POINT('Ctrl Pts',(3.59558957056917,3.40225427845545,36.9429244660201));
#52082=CARTESIAN_POINT('Ctrl Pts',(4.71986342548563,2.21409283714297,36.8900042119381));
#52083=CARTESIAN_POINT('Ctrl Pts',(5.19695092651147,0.413544331548897,36.8370839578562));
#52084=CARTESIAN_POINT('Ctrl Pts',(4.80852954676355,-1.17543274293179,36.7841637037742));
#52085=CARTESIAN_POINT('Ctrl Pts',(4.42010816701563,-2.76440981741246,36.7312434496922));
#52086=CARTESIAN_POINT('Ctrl Pts',(3.16617790649396,-4.14181546077975,36.6783231956103));
#52087=CARTESIAN_POINT('Ctrl Pts',(1.6205564033125,-4.67732781392721,36.6254029415283));
#52088=CARTESIAN_POINT('Ctrl Pts',(0.0749349001310295,-5.21284016707467,
36.5724826874463));
#52089=CARTESIAN_POINT('Ctrl Pts',(-1.76237784571023,-4.90645923000227,
36.5195624333644));
#52090=CARTESIAN_POINT('Ctrl Pts',(-3.05059946099004,-3.89838959877812,
36.4666421792824));
#52091=CARTESIAN_POINT('Ctrl Pts',(-4.22165937898849,-2.98200228957926,
36.4185349377406));
#52092=CARTESIAN_POINT('Ctrl Pts',(-4.93896421945116,-1.48575712054711,
36.3704276961987));
#52093=CARTESIAN_POINT('Ctrl Pts',(-4.94842418382236,0.0025848059749288,
36.3223204546569));
#52094=CARTESIAN_POINT('Ctrl Pts',(-4.9478484900732,0.00296101277178129,
36.1776795453433));
#52095=CARTESIAN_POINT('Ctrl Pts',(-4.93749129838862,-1.4595139062905,36.2249362122231));
#52096=CARTESIAN_POINT('Ctrl Pts',(-4.24848225306339,-2.93046862920176,
36.2721928791029));
#52097=CARTESIAN_POINT('Ctrl Pts',(-3.11270745258791,-3.84898058519796,
36.3194495459828));
#52098=CARTESIAN_POINT('Ctrl Pts',(-1.84081303028634,-4.87757378268728,
36.3723698000648));
#52099=CARTESIAN_POINT('Ctrl Pts',(-0.00864838040995825,-5.21337163681495,
36.4252900541467));
#52100=CARTESIAN_POINT('Ctrl Pts',(1.54535997115889,-4.70270792099264,36.4782103082287));
#52101=CARTESIAN_POINT('Ctrl Pts',(3.09936832272773,-4.19204420517033,36.5311305623107));
#52102=CARTESIAN_POINT('Ctrl Pts',(4.37522037598902,-2.83491891939801,36.5840508163926));
#52103=CARTESIAN_POINT('Ctrl Pts',(4.78906674566614,-1.25237332141095,36.6369710704746));
#52104=CARTESIAN_POINT('Ctrl Pts',(5.20291311534324,0.330172276576089,36.6898913245566));
#52105=CARTESIAN_POINT('Ctrl Pts',(4.75475380143625,2.13813818677785,36.7428115786385));
#52106=CARTESIAN_POINT('Ctrl Pts',(3.64967335059123,3.34417159616718,36.7957318327205));
#52107=CARTESIAN_POINT('Ctrl Pts',(2.54459289974621,4.55020500555648,36.8486520868024));
#52108=CARTESIAN_POINT('Ctrl Pts',(0.782591311963154,5.15430591413334,36.9015723408844));
#52109=CARTESIAN_POINT('Ctrl Pts',(-0.830012575668756,4.88002851988171,
36.9544925949664));
#52110=CARTESIAN_POINT('Ctrl Pts',(-2.44261646330071,4.60575112563006,37.0074128490484));
#52111=CARTESIAN_POINT('Ctrl Pts',(-3.9058226507815,3.45309542854993,37.0603331031303));
#52112=CARTESIAN_POINT('Ctrl Pts',(-4.5500456396125,1.94953427978849,37.1132533572123));
#52113=CARTESIAN_POINT('Ctrl Pts',(-4.81147567364344,1.33937902438292,37.1347287532559));
#52114=CARTESIAN_POINT('Ctrl Pts',(-4.93803628002896,0.671436970049187,
37.1562041492996));
#52115=CARTESIAN_POINT('Ctrl Pts',(-4.9350718820976,0.00242042316235142,
37.1776795453432));
#52116=CARTESIAN_POINT('Origin',(0.,0.,16.));
#52117=CARTESIAN_POINT('',(-4.93830712716952,-0.00410043205665789,38.3223204546569));
#52118=CARTESIAN_POINT('',(-4.93901314208066,-0.00426717980477184,38.1776795453432));
#52119=CARTESIAN_POINT('',(-4.942,-6.05220448138622E-16,16.));
#52120=CARTESIAN_POINT('Ctrl Pts',(-4.93830712716952,-0.00410043205665789,
38.3223204546569));
#52121=CARTESIAN_POINT('Ctrl Pts',(-4.92941979674321,1.12913042651997,38.2858838244337));
#52122=CARTESIAN_POINT('Ctrl Pts',(-4.54190399082784,2.26785272885638,38.2494471942104));
#52123=CARTESIAN_POINT('Ctrl Pts',(-3.8277718834972,3.13875149433059,38.2130105639872));
#52124=CARTESIAN_POINT('Ctrl Pts',(-2.79057244061549,4.40363750783395,38.1600903099052));
#52125=CARTESIAN_POINT('Ctrl Pts',(-1.06439510407127,5.10356550944081,38.1071700558233));
#52126=CARTESIAN_POINT('Ctrl Pts',(0.560835013546147,4.91823775582626,38.0542498017413));
#52127=CARTESIAN_POINT('Ctrl Pts',(2.18606513116352,4.73291000221171,38.0013295476593));
#52128=CARTESIAN_POINT('Ctrl Pts',(3.71034802985413,3.66232649337579,37.9484092935774));
#52129=CARTESIAN_POINT('Ctrl Pts',(4.43614857526344,2.19640259366137,37.8954890394954));
#52130=CARTESIAN_POINT('Ctrl Pts',(5.16194912067276,0.730478693946923,37.8425687854135));
#52131=CARTESIAN_POINT('Ctrl Pts',(5.08926731280079,-1.13078559664599,37.7896485313315));
#52132=CARTESIAN_POINT('Ctrl Pts',(4.25136345697712,-2.53564731221314,37.7367282772495));
#52133=CARTESIAN_POINT('Ctrl Pts',(3.41345960115345,-3.94050902778028,37.6838080231676));
#52134=CARTESIAN_POINT('Ctrl Pts',(1.81033369737808,-4.88896816832161,37.6308877690856));
#52135=CARTESIAN_POINT('Ctrl Pts',(0.175600643277768,-4.9469953455946,37.5779675150036));
#52136=CARTESIAN_POINT('Ctrl Pts',(-1.45913241082256,-5.00502252286759,
37.5250472609217));
#52137=CARTESIAN_POINT('Ctrl Pts',(-3.12547261524786,-4.17261773687219,
37.4721270068397));
#52138=CARTESIAN_POINT('Ctrl Pts',(-4.06087724294093,-2.83070213074755,
37.4192067527577));
#52139=CARTESIAN_POINT('Ctrl Pts',(-4.63172289977408,-2.01177663806308,
37.3869113200575));
#52140=CARTESIAN_POINT('Ctrl Pts',(-4.93035015801884,-1.00309677586341,
37.3546158873572));
#52141=CARTESIAN_POINT('Ctrl Pts',(-4.93549302535697,0.00277814199197368,
37.3223204546569));
#52142=CARTESIAN_POINT('Ctrl Pts',(-4.9350718820976,0.00242042316235142,
37.1776795453432));
#52143=CARTESIAN_POINT('Ctrl Pts',(-4.93073133015009,-0.977171771522589,
37.2091244033815));
#52144=CARTESIAN_POINT('Ctrl Pts',(-4.64869419974499,-1.95906763650772,
37.2405692614198));
#52145=CARTESIAN_POINT('Ctrl Pts',(-4.10573795122914,-2.76523328246712,
37.2720141194581));
#52146=CARTESIAN_POINT('Ctrl Pts',(-3.19196748383364,-4.12197309551857,
37.3249343735401));
#52147=CARTESIAN_POINT('Ctrl Pts',(-1.53918675886144,-4.9809861211788,37.3778546276221));
#52148=CARTESIAN_POINT('Ctrl Pts',(0.0962665215178138,-4.94917487945839,
37.4307748817041));
#52149=CARTESIAN_POINT('Ctrl Pts',(1.73171980189707,-4.91736363773799,37.483695135786));
#52150=CARTESIAN_POINT('Ctrl Pts',(3.34984563768341,-3.99472812863699,37.536615389868));
#52151=CARTESIAN_POINT('Ctrl Pts',(4.21016493327244,-2.60348045225429,37.5895356439499));
#52152=CARTESIAN_POINT('Ctrl Pts',(5.07048422886148,-1.21223277587156,37.6424558980319));
#52153=CARTESIAN_POINT('Ctrl Pts',(5.17299698425316,0.64762706779285,37.6953761521139));
#52154=CARTESIAN_POINT('Ctrl Pts',(4.47079179693381,2.12499880919883,37.7482964061958));
#52155=CARTESIAN_POINT('Ctrl Pts',(3.76858660961448,3.60237055060479,37.8012166602778));
#52156=CARTESIAN_POINT('Ctrl Pts',(2.26166347958414,4.69725418975229,37.8541369143597));
#52157=CARTESIAN_POINT('Ctrl Pts',(0.639613445927835,4.90861425153937,37.9070571684417));
#52158=CARTESIAN_POINT('Ctrl Pts',(-0.982436587728495,5.11997431332645,
37.9599774225237));
#52159=CARTESIAN_POINT('Ctrl Pts',(-2.71961352501084,4.44781079775303,38.0128976766056));
#52160=CARTESIAN_POINT('Ctrl Pts',(-3.77695866803847,3.19971599529649,38.0658179306876));
#52161=CARTESIAN_POINT('Ctrl Pts',(-4.52195594113156,2.32031797609409,38.1031051355728));
#52162=CARTESIAN_POINT('Ctrl Pts',(-4.92945048540112,1.15499867080211,38.140392340458));
#52163=CARTESIAN_POINT('Ctrl Pts',(-4.93901314208066,-0.00426717980477184,
38.1776795453432));
#52164=CARTESIAN_POINT('Origin',(0.,0.,16.));
#52165=CARTESIAN_POINT('',(-4.95007301157197,-0.000387401246429997,39.3223204546569));
#52166=CARTESIAN_POINT('',(-4.95010830192917,0.000103228088722096,39.1776795453432));
#52167=CARTESIAN_POINT('',(-4.942,-6.05220448138622E-16,16.));
#52168=CARTESIAN_POINT('Ctrl Pts',(-4.95007301157197,-0.000387401246429997,
39.3223204546569));
#52169=CARTESIAN_POINT('Ctrl Pts',(-4.94825412650634,1.61464285750734,39.2700720155921));
#52170=CARTESIAN_POINT('Ctrl Pts',(-4.08291838964434,3.23134503628798,39.2178235765273));
#52171=CARTESIAN_POINT('Ctrl Pts',(-2.73731172677047,4.12440578092639,39.1655751374625));
#52172=CARTESIAN_POINT('Ctrl Pts',(-1.37440313527419,5.0289495790347,39.1126548833806));
#52173=CARTESIAN_POINT('Ctrl Pts',(0.481206517102607,5.19112301285789,39.0597346292986));
#52174=CARTESIAN_POINT('Ctrl Pts',(1.98036191326499,4.53671304225247,39.0068143752166));
#52175=CARTESIAN_POINT('Ctrl Pts',(3.47951730942733,3.88230307164706,38.9538941211347));
#52176=CARTESIAN_POINT('Ctrl Pts',(4.62221844937522,2.41130969661302,38.9009738670527));
#52177=CARTESIAN_POINT('Ctrl Pts',(4.88554783933805,0.796881951604831,38.8480536129708));
#52178=CARTESIAN_POINT('Ctrl Pts',(5.14887722930088,-0.817545793403355,
38.7951333588888));
#52179=CARTESIAN_POINT('Ctrl Pts',(4.53283486927871,-2.57540790838573,38.7422131048068));
#52180=CARTESIAN_POINT('Ctrl Pts',(3.31933115184711,-3.67227984222765,38.6892928507249));
#52181=CARTESIAN_POINT('Ctrl Pts',(2.10582743441549,-4.76915177606959,38.6363725966429));
#52182=CARTESIAN_POINT('Ctrl Pts',(0.294862359574459,-5.20503352877106,
38.5834523425609));
#52183=CARTESIAN_POINT('Ctrl Pts',(-1.28483879610452,-4.78045895320511,
38.530532088479));
#52184=CARTESIAN_POINT('Ctrl Pts',(-2.86453995178352,-4.35588437763916,
38.477611834397));
#52185=CARTESIAN_POINT('Ctrl Pts',(-4.21297718830044,-3.07085347380577,
38.424691580315));
#52186=CARTESIAN_POINT('Ctrl Pts',(-4.71308503194927,-1.51341600918913,
38.3717713262331));
#52187=CARTESIAN_POINT('Ctrl Pts',(-4.86885884155228,-1.02830470737132,
38.3552877023743));
#52188=CARTESIAN_POINT('Ctrl Pts',(-4.94232768041382,-0.516764503992941,
38.3388040785156));
#52189=CARTESIAN_POINT('Ctrl Pts',(-4.93830712716952,-0.00410043205665789,
38.3223204546569));
#52190=CARTESIAN_POINT('Ctrl Pts',(-4.93901314208066,-0.00426717980477184,
38.1776795453432));
#52191=CARTESIAN_POINT('Ctrl Pts',(-4.94302238554053,-0.490301467717737,
38.19331259454));
#52192=CARTESIAN_POINT('Ctrl Pts',(-4.87708344029753,-0.975271683602742,
38.2089456437367));
#52193=CARTESIAN_POINT('Ctrl Pts',(-4.7367428403112,-1.43766007643938,38.2245786929335));
#52194=CARTESIAN_POINT('Ctrl Pts',(-4.26166852078334,-3.00291525637914,
38.2774989470154));
#52195=CARTESIAN_POINT('Ctrl Pts',(-2.9340065329546,-4.30939952691902,38.3304192010974));
#52196=CARTESIAN_POINT('Ctrl Pts',(-1.36131527943717,-4.75924573231914,
38.3833394551794));
#52197=CARTESIAN_POINT('Ctrl Pts',(0.211375974080253,-5.20909193771926,
38.4362597092614));
#52198=CARTESIAN_POINT('Ctrl Pts',(2.0290964932864,-4.80230007797962,38.4891799633433));
#52199=CARTESIAN_POINT('Ctrl Pts',(3.2600296070944,-3.72502432092665,38.5421002174252));
#52200=CARTESIAN_POINT('Ctrl Pts',(4.4909627209024,-2.64774856387368,38.5950204715072));
#52201=CARTESIAN_POINT('Ctrl Pts',(5.13510842931226,-0.899988909507443,
38.6479407255892));
#52202=CARTESIAN_POINT('Ctrl Pts',(4.89769581831224,0.718453131327276,38.7008609796712));
#52203=CARTESIAN_POINT('Ctrl Pts',(4.66028320731222,2.33689517216197,38.7537812337531));
#52204=CARTESIAN_POINT('Ctrl Pts',(3.54131227690224,3.82601959946517,38.8067014878351));
#52205=CARTESIAN_POINT('Ctrl Pts',(2.05284121454405,4.50438033235388,38.859621741917));
#52206=CARTESIAN_POINT('Ctrl Pts',(0.564370152185806,5.18274106524261,38.912541995999));
#52207=CARTESIAN_POINT('Ctrl Pts',(-1.29360104212064,5.05033810371689,38.965462250081));
#52208=CARTESIAN_POINT('Ctrl Pts',(-2.67083637362622,4.16776106512145,39.0183825041629));
#52209=CARTESIAN_POINT('Ctrl Pts',(-4.04807170513178,3.28518402652602,39.0713027582449));
#52210=CARTESIAN_POINT('Ctrl Pts',(-4.94457117383642,1.65243291086087,39.1242230123269));
#52211=CARTESIAN_POINT('Ctrl Pts',(-4.95008293089447,0.0166795651704946,
39.1771432664088));
#52212=CARTESIAN_POINT('Ctrl Pts',(-4.95010154909182,0.0111541440981086,
39.1773220260536));
#52213=CARTESIAN_POINT('Ctrl Pts',(-4.95011000089745,0.00562868876953041,
39.1775007856984));
#52214=CARTESIAN_POINT('Ctrl Pts',(-4.95010830192917,0.000103228088722096,
39.1776795453432));
#52215=CARTESIAN_POINT('Origin',(0.,0.,16.));
#52216=CARTESIAN_POINT('',(-4.93943724668283,0.00434520414469897,40.3223204546569));
#52217=CARTESIAN_POINT('',(-4.9387122051873,0.0042019715207839,40.1776795453432));
#52218=CARTESIAN_POINT('',(-4.942,-6.05220448138622E-16,16.));
#52219=CARTESIAN_POINT('Ctrl Pts',(-4.93943724668283,0.00434520414469897,
40.3223204546569));
#52220=CARTESIAN_POINT('Ctrl Pts',(-4.94341650816428,0.474947915493244,
40.3071804608325));
#52221=CARTESIAN_POINT('Ctrl Pts',(-4.88164614501736,0.944527111103383,
40.2920404670082));
#52222=CARTESIAN_POINT('Ctrl Pts',(-4.74989944410437,1.39357590613184,40.2769004731838));
#52223=CARTESIAN_POINT('Ctrl Pts',(-4.28939272477215,2.96317868165193,40.2239802191018));
#52224=CARTESIAN_POINT('Ctrl Pts',(-2.97393022079225,4.28194545604953,40.1710599650198));
#52225=CARTESIAN_POINT('Ctrl Pts',(-1.40548766464857,4.74638841223249,40.1181397109379));
#52226=CARTESIAN_POINT('Ctrl Pts',(0.162954891495088,5.21083136841545,40.0652194568559));
#52227=CARTESIAN_POINT('Ctrl Pts',(1.98437749980252,4.82095050638379,40.012299202774));
#52228=CARTESIAN_POINT('Ctrl Pts',(3.22526935667327,3.75516126313619,39.959378948692));
#52229=CARTESIAN_POINT('Ctrl Pts',(4.46616121354403,2.68937201988858,39.90645869461));
#52230=CARTESIAN_POINT('Ctrl Pts',(5.1265223189781,0.947674395425016,39.8535384405281));
#52231=CARTESIAN_POINT('Ctrl Pts',(4.90416134563252,-0.672904176876648,
39.8006181864461));
#52232=CARTESIAN_POINT('Ctrl Pts',(4.68180037228695,-2.29348274917834,39.7476979323641));
#52233=CARTESIAN_POINT('Ctrl Pts',(3.57671732016171,-3.79294226931812,39.6947776782822));
#52234=CARTESIAN_POINT('Ctrl Pts',(2.09461507151,-4.4851071600863,39.6418574242002));
#52235=CARTESIAN_POINT('Ctrl Pts',(0.612512822858338,-5.17727205085446,
39.5889371701182));
#52236=CARTESIAN_POINT('Ctrl Pts',(-1.24660862231976,-5.06214231225107,
39.5360169160363));
#52237=CARTESIAN_POINT('Ctrl Pts',(-2.63198689690885,-4.19240307100288,
39.4830966619543));
#52238=CARTESIAN_POINT('Ctrl Pts',(-4.01736517149795,-3.32266382975467,
39.4301764078723));
#52239=CARTESIAN_POINT('Ctrl Pts',(-4.92900027549801,-1.69831508586162,
39.3772561537904));
#52240=CARTESIAN_POINT('Ctrl Pts',(-4.9497140621902,-0.0626836327184169,
39.3243358997084));
#52241=CARTESIAN_POINT('Ctrl Pts',(-4.94997702073422,-0.0419195265770804,
39.3236640846913));
#52242=CARTESIAN_POINT('Ctrl Pts',(-4.95009639895585,-0.0211536021213772,
39.3229922696741));
#52243=CARTESIAN_POINT('Ctrl Pts',(-4.95007301157197,-0.000387401246429997,
39.3223204546569));
#52244=CARTESIAN_POINT('Ctrl Pts',(-4.95010830192917,0.000103228088722096,
39.1776795453432));
#52245=CARTESIAN_POINT('Ctrl Pts',(-4.94960703596349,-1.6301363826534,39.2304210397804));
#52246=CARTESIAN_POINT('Ctrl Pts',(-4.06548675829959,-3.26084190194751,
39.2831625342175));
#52247=CARTESIAN_POINT('Ctrl Pts',(-2.6988623875562,-4.14966758230844,39.3359040286547));
#52248=CARTESIAN_POINT('Ctrl Pts',(-1.32760604174843,-5.04150580838138,
39.3888242827367));
#52249=CARTESIAN_POINT('Ctrl Pts',(0.529430695278565,-5.18642668481171,
39.4417445368187));
#52250=CARTESIAN_POINT('Ctrl Pts',(2.02243945069843,-4.51811220521201,39.4946647909006));
#52251=CARTESIAN_POINT('Ctrl Pts',(3.51544820611836,-3.84979772561229,39.5475850449826));
#52252=CARTESIAN_POINT('Ctrl Pts',(4.6444289799311,-2.36824788998248,39.6005052990645));
#52253=CARTESIAN_POINT('Ctrl Pts',(4.89274292745657,-0.751442530371268,
39.6534255531465));
#52254=CARTESIAN_POINT('Ctrl Pts',(5.14105687498204,0.865362829239897,39.7063458072285));
#52255=CARTESIAN_POINT('Ctrl Pts',(4.50870399622024,2.61742371283248,39.7592660613104));
#52256=CARTESIAN_POINT('Ctrl Pts',(3.2850586262277,3.70297030137619,39.8121863153924));
#52257=CARTESIAN_POINT('Ctrl Pts',(2.06141325623513,4.78851688991993,39.8651065694743));
#52258=CARTESIAN_POINT('Ctrl Pts',(0.246475395011777,5.2075491834148,39.9180268235563));
#52259=CARTESIAN_POINT('Ctrl Pts',(-1.32921167314713,4.76831160460351,39.9709470776383));
#52260=CARTESIAN_POINT('Ctrl Pts',(-2.90489874130597,4.32907402579225,40.0238673317202));
#52261=CARTESIAN_POINT('Ctrl Pts',(-4.24133501640037,3.03156657467491,40.0767875858022));
#52262=CARTESIAN_POINT('Ctrl Pts',(-4.72694684795839,1.46954847732333,40.1297078398842));
#52263=CARTESIAN_POINT('Ctrl Pts',(-4.87368101212714,0.997563642860038,
40.1456984083705));
#52264=CARTESIAN_POINT('Ctrl Pts',(-4.94273254556439,0.501428253000672,
40.1616889768569));
#52265=CARTESIAN_POINT('Ctrl Pts',(-4.9387122051873,0.0042019715207839,
40.1776795453432));
#52266=CARTESIAN_POINT('Origin',(0.,0.,16.));
#52267=CARTESIAN_POINT('',(-4.93485552516168,-0.00220275864159403,41.3223204546569));
#52268=CARTESIAN_POINT('',(-4.93524162710697,-0.00257366327817901,41.1776795453432));
#52269=CARTESIAN_POINT('',(-4.942,-6.05220448138622E-16,16.));
#52270=CARTESIAN_POINT('Ctrl Pts',(-4.93485552516168,-0.00220275864159403,
41.3223204546569));
#52271=CARTESIAN_POINT('Ctrl Pts',(-4.93097721826847,0.962135133190097,
41.291368651991));
#52272=CARTESIAN_POINT('Ctrl Pts',(-4.65830472720369,1.92849849558568,41.2604168493251));
#52273=CARTESIAN_POINT('Ctrl Pts',(-4.13125993704044,2.72695615437044,41.2294650466591));
#52274=CARTESIAN_POINT('Ctrl Pts',(-3.23013813457067,4.09212969959618,41.1765447925771));
#52275=CARTESIAN_POINT('Ctrl Pts',(-1.58541225739997,4.96646613003761,41.1236245384952));
#52276=CARTESIAN_POINT('Ctrl Pts',(0.0502660136753988,4.94985574164777,
41.0707042844132));
#52277=CARTESIAN_POINT('Ctrl Pts',(1.68594428475072,4.93324535325794,41.0177840303312));
#52278=CARTESIAN_POINT('Ctrl Pts',(3.31257494973071,4.0256881460368,40.9648637762493));
#52279=CARTESIAN_POINT('Ctrl Pts',(4.18578697328013,2.64249615885673,40.9119435221673));
#52280=CARTESIAN_POINT('Ctrl Pts',(5.05899899682956,1.25930417167664,40.8590232680854));
#52281=CARTESIAN_POINT('Ctrl Pts',(5.17879237894847,-0.599522595462416,
40.8061030140034));
#52282=CARTESIAN_POINT('Ctrl Pts',(4.49034783841098,-2.08335662461616,40.7531827599214));
#52283=CARTESIAN_POINT('Ctrl Pts',(3.8019032978735,-3.56719065376989,40.7002625058395));
#52284=CARTESIAN_POINT('Ctrl Pts',(2.30522083467963,-4.67603194493831,40.6473422517575));
#52285=CARTESIAN_POINT('Ctrl Pts',(0.685205202367444,-4.90245778828362,
40.5944219976755));
#52286=CARTESIAN_POINT('Ctrl Pts',(-0.93481042994472,-5.12888363162893,
40.5415017435936));
#52287=CARTESIAN_POINT('Ctrl Pts',(-2.6781592313752,-4.47289402715115,40.4885814895116));
#52288=CARTESIAN_POINT('Ctrl Pts',(-3.74705816474816,-3.23467983659099,
40.4356612354296));
#52289=CARTESIAN_POINT('Ctrl Pts',(-4.51015502798955,-2.35070724073872,
40.397880975172));
#52290=CARTESIAN_POINT('Ctrl Pts',(-4.92950741869571,-1.16999430476845,
40.3601007149145));
#52291=CARTESIAN_POINT('Ctrl Pts',(-4.93943724668283,0.00434520414469897,
40.3223204546569));
#52292=CARTESIAN_POINT('Ctrl Pts',(-4.9387122051873,0.0042019715207839,
40.1776795453432));
#52293=CARTESIAN_POINT('Ctrl Pts',(-4.92942736292292,-1.14412557296836,
40.2146092309388));
#52294=CARTESIAN_POINT('Ctrl Pts',(-4.53040370843391,-2.2982715368062,40.2515389165345));
#52295=CARTESIAN_POINT('Ctrl Pts',(-3.79843588104676,-3.17419030434592,
40.2884686021301));
#52296=CARTESIAN_POINT('Ctrl Pts',(-2.74952569455548,-4.42938224507769,
40.341388856212));
#52297=CARTESIAN_POINT('Ctrl Pts',(-1.01691793355136,-5.11323738295533,
40.394309110294));
#52298=CARTESIAN_POINT('Ctrl Pts',(0.606519628933596,-4.91281316257247,
40.4472293643759));
#52299=CARTESIAN_POINT('Ctrl Pts',(2.22995719141853,-4.71238894218962,40.5001496184579));
#52300=CARTESIAN_POINT('Ctrl Pts',(3.74422455538428,-3.62768536354625,40.5530698725399));
#52301=CARTESIAN_POINT('Ctrl Pts',(4.45636984813063,-2.15507935058069,40.6059901266218));
#52302=CARTESIAN_POINT('Ctrl Pts',(5.16851514087698,-0.682473337615157,
40.6589103807038));
#52303=CARTESIAN_POINT('Ctrl Pts',(5.07853836240398,1.17803510967258,40.7118306347858));
#52304=CARTESIAN_POINT('Ctrl Pts',(4.22761426072911,2.57504891081838,40.7647508888677));
#52305=CARTESIAN_POINT('Ctrl Pts',(3.37669015905424,3.97206271196421,40.8176711429497));
#52306=CARTESIAN_POINT('Ctrl Pts',(1.76481873417747,4.90558186696812,40.8705913970317));
#52307=CARTESIAN_POINT('Ctrl Pts',(0.12961696774931,4.94841375314338,40.9235116511136));
#52308=CARTESIAN_POINT('Ctrl Pts',(-1.50558479867887,4.99124563931864,40.9764319051956));
#52309=CARTESIAN_POINT('Ctrl Pts',(-3.16411690665841,4.14339025666527,41.0293521592775));
#52310=CARTESIAN_POINT('Ctrl Pts',(-4.0870097333165,2.79283917732535,41.0822724133595));
#52311=CARTESIAN_POINT('Ctrl Pts',(-4.6416213166461,1.98122676595515,41.1140747906874));
#52312=CARTESIAN_POINT('Ctrl Pts',(-4.93056429073029,0.988070940573039,
41.1458771680153));
#52313=CARTESIAN_POINT('Ctrl Pts',(-4.93524162710697,-0.00257366327817901,
41.1776795453432));
#52314=CARTESIAN_POINT('Origin',(0.,0.,16.));
#52315=CARTESIAN_POINT('',(-4.94748713622925,-0.00316321289392352,42.3223204546569));
#52316=CARTESIAN_POINT('',(-4.94809820533655,-0.00280696805152256,42.1776795453432));
#52317=CARTESIAN_POINT('',(-4.942,-6.05220448138622E-16,16.));
#52318=CARTESIAN_POINT('Ctrl Pts',(-4.94748713622925,-0.00316321289392352,
42.3223204546569));
#52319=CARTESIAN_POINT('Ctrl Pts',(-4.93670139323051,1.44433029491444,42.2755568431494));
#52320=CARTESIAN_POINT('Ctrl Pts',(-4.26377312667576,2.9005508041267,42.2287932316419));
#52321=CARTESIAN_POINT('Ctrl Pts',(-3.14834440585587,3.81988560527279,42.1820296201344));
#52322=CARTESIAN_POINT('Ctrl Pts',(-1.88606441050834,4.8602550227471,42.1291093660525));
#52323=CARTESIAN_POINT('Ctrl Pts',(-0.0570997319322858,5.21306603328002,
42.0761891119705));
#52324=CARTESIAN_POINT('Ctrl Pts',(1.50158745972911,4.71686693007535,42.0232688578886));
#52325=CARTESIAN_POINT('Ctrl Pts',(3.06027465139055,4.22066782687068,41.9703486038066));
#52326=CARTESIAN_POINT('Ctrl Pts',(4.34868435613734,2.87545860992836,41.9174283497246));
#52327=CARTESIAN_POINT('Ctrl Pts',(4.77722061558389,1.29682756189652,41.8645080956427));
#52328=CARTESIAN_POINT('Ctrl Pts',(5.20575687503042,-0.281803486135251,
41.8115878415607));
#52329=CARTESIAN_POINT('Ctrl Pts',(4.77441968917683,-2.09385636525649,41.7586675874787));
#52330=CARTESIAN_POINT('Ctrl Pts',(3.68059554195264,-3.31010800304349,41.7057473333968));
#52331=CARTESIAN_POINT('Ctrl Pts',(2.58677139472839,-4.52635964083055,41.6528270793148));
#52332=CARTESIAN_POINT('Ctrl Pts',(0.830460286133465,-5.14681003728328,
41.5999068252328));
#52333=CARTESIAN_POINT('Ctrl Pts',(-0.78462299692839,-4.88753161503282,
41.5469865711509));
#52334=CARTESIAN_POINT('Ctrl Pts',(-2.39970627999022,-4.62825319278237,
41.4940663170689));
#52335=CARTESIAN_POINT('Ctrl Pts',(-3.87356173751901,-3.48924595182876,
41.4411460629869));
#52336=CARTESIAN_POINT('Ctrl Pts',(-4.531730602399,-1.99173700134697,41.388225808905));
#52337=CARTESIAN_POINT('Ctrl Pts',(-4.80495209353668,-1.37008555249385,
41.366257357489));
#52338=CARTESIAN_POINT('Ctrl Pts',(-4.93760820478682,-0.686654334984092,
41.3442889060729));
#52339=CARTESIAN_POINT('Ctrl Pts',(-4.93485552516168,-0.00220275864159403,
41.3223204546569));
#52340=CARTESIAN_POINT('Ctrl Pts',(-4.93524162710697,-0.00257366327817901,
41.1776795453432));
#52341=CARTESIAN_POINT('Ctrl Pts',(-4.93834753998013,-0.660395889443513,
41.1987974220973));
#52342=CARTESIAN_POINT('Ctrl Pts',(-4.81610883381463,-1.31711081291602,
41.2199152988513));
#52343=CARTESIAN_POINT('Ctrl Pts',(-4.56308028711322,-1.91882712196431,
41.2410331756054));
#52344=CARTESIAN_POINT('Ctrl Pts',(-3.92900446891528,-3.42669556588764,
41.2939534296874));
#52345=CARTESIAN_POINT('Ctrl Pts',(-2.47359928718284,-4.58918567770784,
41.3468736837693));
#52346=CARTESIAN_POINT('Ctrl Pts',(-0.862880381041693,-4.87432422789462,
41.3997939378513));
#52347=CARTESIAN_POINT('Ctrl Pts',(0.74783852509941,-5.15946277808138,41.4527141919333));
#52348=CARTESIAN_POINT('Ctrl Pts',(2.51387115564923,-4.56724976663472,41.5056344460152));
#52349=CARTESIAN_POINT('Ctrl Pts',(3.62705400678358,-3.36869091228363,41.5585547000972));
#52350=CARTESIAN_POINT('Ctrl Pts',(4.74023685791794,-2.17013205793252,41.6114749541791));
#52351=CARTESIAN_POINT('Ctrl Pts',(5.20056992963686,-0.36522736067698,41.6643952082611));
#52352=CARTESIAN_POINT('Ctrl Pts',(4.79739777779339,1.22007122425299,41.7173154623431));
#52353=CARTESIAN_POINT('Ctrl Pts',(4.3942256259499,2.80536980918301,41.770235716425));
#52354=CARTESIAN_POINT('Ctrl Pts',(3.12754825054399,4.17106228178741,41.823155970507));
#52355=CARTESIAN_POINT('Ctrl Pts',(1.57701656414349,4.69218690879255,41.8760762245889));
#52356=CARTESIAN_POINT('Ctrl Pts',(0.0264848777430365,5.21331153579767,
41.9289964786709));
#52357=CARTESIAN_POINT('Ctrl Pts',(-1.80790111965202,4.88986831720356,41.9819167327529));
#52358=CARTESIAN_POINT('Ctrl Pts',(-3.08669837960869,3.86986980968975,42.0348369868349));
#52359=CARTESIAN_POINT('Ctrl Pts',(-4.2372765819408,2.95214181174547,42.0824511730043));
#52360=CARTESIAN_POINT('Ctrl Pts',(-4.93809323584742,1.47053667915491,42.1300653591738));
#52361=CARTESIAN_POINT('Ctrl Pts',(-4.94809820533655,-0.00280696805152256,
42.1776795453432));
#52362=CARTESIAN_POINT('Origin',(0.,0.,16.));
#52363=CARTESIAN_POINT('',(-4.94451025515232,0.00421302333877771,43.3223204546569));
#52364=CARTESIAN_POINT('',(-4.94371934458518,0.00435719887056521,43.1776795453432));
#52365=CARTESIAN_POINT('',(-4.942,-6.05220448138622E-16,16.));
#52366=CARTESIAN_POINT('Ctrl Pts',(-4.94451025515232,0.00421302333877771,
43.3223204546569));
#52367=CARTESIAN_POINT('Ctrl Pts',(-4.94721961825891,0.30354166338666,43.3126652883898));
#52368=CARTESIAN_POINT('Ctrl Pts',(-4.9223727794906,0.602421473877891,43.3030101221227));
#52369=CARTESIAN_POINT('Ctrl Pts',(-4.8683572221906,0.895933308008362,43.2933549558557));
#52370=CARTESIAN_POINT('Ctrl Pts',(-4.57229634269635,2.50468041899365,43.2404347017737));
#52371=CARTESIAN_POINT('Ctrl Pts',(-3.39995792978838,3.95216446044364,43.1875144476917));
#52372=CARTESIAN_POINT('Ctrl Pts',(-1.88782194598489,4.57599462800297,43.1345941936098));
#52373=CARTESIAN_POINT('Ctrl Pts',(-0.375685962181428,5.19982479556229,
43.0816739395278));
#52374=CARTESIAN_POINT('Ctrl Pts',(1.47624759251752,5.00000108923096,43.0287536854458));
#52375=CARTESIAN_POINT('Ctrl Pts',(2.82050563945827,4.06796588887349,42.9758334313639));
#52376=CARTESIAN_POINT('Ctrl Pts',(4.16476368639908,3.13593068851599,42.9229131772819));
#52377=CARTESIAN_POINT('Ctrl Pts',(5.00134622558163,1.47168399413228,42.8699929231999));
#52378=CARTESIAN_POINT('Ctrl Pts',(4.9474203102028,-0.163189489389038,42.817072669118));
#52379=CARTESIAN_POINT('Ctrl Pts',(4.89349439482397,-1.79806297291028,42.764152415036));
#52380=CARTESIAN_POINT('Ctrl Pts',(3.94906002488378,-3.40356324556919,42.7112321609541));
#52381=CARTESIAN_POINT('Ctrl Pts',(2.54630479212863,-4.24498886227479,42.6583119068721));
#52382=CARTESIAN_POINT('Ctrl Pts',(1.14354955937346,-5.0864144789804,42.6053916527901));
#52383=CARTESIAN_POINT('Ctrl Pts',(-0.717526536196703,-5.16376543973274,
42.5524713987082));
#52384=CARTESIAN_POINT('Ctrl Pts',(-2.18526664959422,-4.44164476353361,
42.4995511446262));
#52385=CARTESIAN_POINT('Ctrl Pts',(-3.65300676299177,-3.71952408733446,
42.4466308905442));
#52386=CARTESIAN_POINT('Ctrl Pts',(-4.72741089421663,-2.19793177418379,
42.3937106364623));
#52387=CARTESIAN_POINT('Ctrl Pts',(-4.91681530376954,-0.573171705400564,
42.3407903823803));
#52388=CARTESIAN_POINT('Ctrl Pts',(-4.93885025563959,-0.38415018261489,
42.3346337398059));
#52389=CARTESIAN_POINT('Ctrl Pts',(-4.94890712844976,-0.19373232997381,
42.3284770972314));
#52390=CARTESIAN_POINT('Ctrl Pts',(-4.94748713622925,-0.00316321289392352,
42.3223204546569));
#52391=CARTESIAN_POINT('Ctrl Pts',(-4.94809820533655,-0.00280696805152256,
42.1776795453432));
#52392=CARTESIAN_POINT('Ctrl Pts',(-4.94921314716046,-0.166994620502292,
42.1829856132557));
#52393=CARTESIAN_POINT('Ctrl Pts',(-4.94174917029318,-0.331079676814377,
42.1882916811682));
#52394=CARTESIAN_POINT('Ctrl Pts',(-4.92537268191333,-0.494270345953525,
42.1935977490807));
#52395=CARTESIAN_POINT('Ctrl Pts',(-4.76204120174297,-2.12185819764955,
42.2465180031627));
#52396=CARTESIAN_POINT('Ctrl Pts',(-3.71216971888389,-3.6604801046081,42.2994382572447));
#52397=CARTESIAN_POINT('Ctrl Pts',(-2.25619545826342,-4.40603918329588,
42.3523585113266));
#52398=CARTESIAN_POINT('Ctrl Pts',(-0.800221197642949,-5.15159826198366,
42.4052787654086));
#52399=CARTESIAN_POINT('Ctrl Pts',(1.06185584073894,-5.10409451240069,42.4581990194906));
#52400=CARTESIAN_POINT('Ctrl Pts',(2.4779207651768,-4.28526637586659,42.5111192735725));
#52401=CARTESIAN_POINT('Ctrl Pts',(3.89398568961467,-3.46643823933247,42.5640395276545));
#52402=CARTESIAN_POINT('Ctrl Pts',(4.8640385001085,-1.87628571584728,42.6169597817364));
#52403=CARTESIAN_POINT('Ctrl Pts',(4.9441682152519,-0.242486886078373,42.6698800358184));
#52404=CARTESIAN_POINT('Ctrl Pts',(5.02429793039529,1.39131194369048,42.7228002899004));
#52405=CARTESIAN_POINT('Ctrl Pts',(4.21450455018825,3.06875707974299,42.7757205439823));
#52406=CARTESIAN_POINT('Ctrl Pts',(2.88536189314395,4.02222400870711,42.8286407980643));
#52407=CARTESIAN_POINT('Ctrl Pts',(1.55621923609964,4.97569093767124,42.8815610521463));
#52408=CARTESIAN_POINT('Ctrl Pts',(-0.292272697781964,5.20517965954696,
42.9344813062282));
#52409=CARTESIAN_POINT('Ctrl Pts',(-1.81421576809595,4.60567263029181,42.9874015603102));
#52410=CARTESIAN_POINT('Ctrl Pts',(-3.33615883840994,4.00616560103666,43.0403218143921));
#52411=CARTESIAN_POINT('Ctrl Pts',(-4.53155304515633,2.57766282065063,43.0932420684741));
#52412=CARTESIAN_POINT('Ctrl Pts',(-4.85336774243223,0.97386897853116,43.1461623225561));
#52413=CARTESIAN_POINT('Ctrl Pts',(-4.91725446964838,0.655483458634976,
43.1566680634851));
#52414=CARTESIAN_POINT('Ctrl Pts',(-4.94671318283581,0.330189668722103,
43.1671738044142));
#52415=CARTESIAN_POINT('Ctrl Pts',(-4.94371934458518,0.00435719887056521,
43.1776795453432));
#52416=CARTESIAN_POINT('Origin',(0.,0.,16.));
#52417=CARTESIAN_POINT('',(-4.93394997286128,0.000507016503537849,44.3223204546569));
#52418=CARTESIAN_POINT('',(-4.93390371744476,7.29331094537614E-5,44.1776795453432));
#52419=CARTESIAN_POINT('',(-4.942,-6.05220448138622E-16,16.));
#52420=CARTESIAN_POINT('Ctrl Pts',(-4.93394997286128,0.000507016503537849,
44.3223204546569));
#52421=CARTESIAN_POINT('Ctrl Pts',(-4.93467682586532,0.794322762801275,
44.2968534795483));
#52422=CARTESIAN_POINT('Ctrl Pts',(-4.75416264908751,1.58782655048687,44.2713865044396));
#52423=CARTESIAN_POINT('Ctrl Pts',(-4.39062917456631,2.28603892939324,44.245919529331));
#52424=CARTESIAN_POINT('Ctrl Pts',(-3.63520833024163,3.73692095748179,44.192999275249));
#52425=CARTESIAN_POINT('Ctrl Pts',(-2.08949837449215,4.77632854708712,44.1400790211671));
#52426=CARTESIAN_POINT('Ctrl Pts',(-0.460839790231528,4.92861291064672,
44.0871587670851));
#52427=CARTESIAN_POINT('Ctrl Pts',(1.16781879402907,5.08089727420631,44.0342385130031));
#52428=CARTESIAN_POINT('Ctrl Pts',(2.8794260068008,4.3460584117202,43.9813182589212));
#52429=CARTESIAN_POINT('Ctrl Pts',(3.8907242466578,3.06036980963467,43.9283980048392));
#52430=CARTESIAN_POINT('Ctrl Pts',(4.90202248651478,1.77468120754915,43.8754777507573));
#52431=CARTESIAN_POINT('Ctrl Pts',(5.21301175345704,-0.0618571341358118,
43.8225574966753));
#52432=CARTESIAN_POINT('Ctrl Pts',(4.68137860928635,-1.60881722136807,43.7696372425933));
#52433=CARTESIAN_POINT('Ctrl Pts',(4.14974546511566,-3.15577730860032,43.7167169885114));
#52434=CARTESIAN_POINT('Ctrl Pts',(2.77548990983206,-4.41315914137991,43.6637967344294));
#52435=CARTESIAN_POINT('Ctrl Pts',(1.18749227412456,-4.80556558941283,43.6108764803475));
#52436=CARTESIAN_POINT('Ctrl Pts',(-0.400505361582988,-5.19797203744577,
43.5579562262655));
#52437=CARTESIAN_POINT('Ctrl Pts',(-2.20224507771443,-4.72540310073197,
43.5050359721835));
#52438=CARTESIAN_POINT('Ctrl Pts',(-3.3932232627399,-3.60411354211475,43.4521157181016));
#52439=CARTESIAN_POINT('Ctrl Pts',(-4.36691049562677,-2.68740042232609,
43.4088506302867));
#52440=CARTESIAN_POINT('Ctrl Pts',(-4.93236951831919,-1.33708753420181,
43.3655855424718));
#52441=CARTESIAN_POINT('Ctrl Pts',(-4.94451025515232,0.00421302333877771,
43.3223204546569));
#52442=CARTESIAN_POINT('Ctrl Pts',(-4.94371934458518,0.00435719887056521,
43.1776795453432));
#52443=CARTESIAN_POINT('Ctrl Pts',(-4.93163241109647,-1.31111647133373,
43.2200940584961));
#52444=CARTESIAN_POINT('Ctrl Pts',(-4.39058351177215,-2.63537038181765,
43.262508571649));
#52445=CARTESIAN_POINT('Ctrl Pts',(-3.45056931084653,-3.5492493095965,43.3049230848019));
#52446=CARTESIAN_POINT('Ctrl Pts',(-2.27772099417954,-4.68948885175174,
43.3578433388839));
#52447=CARTESIAN_POINT('Ctrl Pts',(-0.483789173040172,-5.19088303220938,
43.4107635929659));
#52448=CARTESIAN_POINT('Ctrl Pts',(1.11029555303778,-4.82398621634968,43.4636838470478));
#52449=CARTESIAN_POINT('Ctrl Pts',(2.70438027911579,-4.45708940048996,43.5166041011298));
#52450=CARTESIAN_POINT('Ctrl Pts',(4.09861791013234,-3.22190158831284,43.5695243552118));
#52451=CARTESIAN_POINT('Ctrl Pts',(4.65498401236277,-1.68366358732205,43.6224446092938));
#52452=CARTESIAN_POINT('Ctrl Pts',(5.21135011459319,-0.145425586331283,
43.6753648633757));
#52453=CARTESIAN_POINT('Ctrl Pts',(4.92984468803749,1.69586260347318,43.7282851174576));
#52454=CARTESIAN_POINT('Ctrl Pts',(3.93928891523517,2.99759938499667,43.7812053715396));
#52455=CARTESIAN_POINT('Ctrl Pts',(2.94873314243287,4.29933616652015,43.8341256256216));
#52456=CARTESIAN_POINT('Ctrl Pts',(1.24912702338399,5.06152153976273,43.8870458797035));
#52457=CARTESIAN_POINT('Ctrl Pts',(-0.381763724262289,4.93536783730094,
43.9399661337855));
#52458=CARTESIAN_POINT('Ctrl Pts',(-2.01265447190855,4.80921413483915,43.9928863878675));
#52459=CARTESIAN_POINT('Ctrl Pts',(-3.57482984815219,3.79472135667302,44.0458066419495));
#52460=CARTESIAN_POINT('Ctrl Pts',(-4.35341454219008,2.35613689213404,44.0987268960314));
#52461=CARTESIAN_POINT('Ctrl Pts',(-4.74060923336151,1.6407204811301,44.125044445802));
#52462=CARTESIAN_POINT('Ctrl Pts',(-4.93401170909488,0.820420654182907,
44.1513619955726));
#52463=CARTESIAN_POINT('Ctrl Pts',(-4.93390371744476,7.29331094537614E-5,
44.1776795453432));
#52464=CARTESIAN_POINT('Origin',(0.,0.,16.));
#52465=CARTESIAN_POINT('',(-4.94264971735337,-0.00447858357024544,45.3223204546569));
#52466=CARTESIAN_POINT('',(-4.94345166054126,-0.00439535110808767,45.1776795453432));
#52467=CARTESIAN_POINT('',(-4.942,-6.05220448138622E-16,16.));
#52468=CARTESIAN_POINT('Ctrl Pts',(-4.94264971735337,-0.00447858357024544,
45.3223204546569));
#52469=CARTESIAN_POINT('Ctrl Pts',(-4.93082575729553,1.27648252745284,45.2810416707067));
#52470=CARTESIAN_POINT('Ctrl Pts',(-4.42134998955586,2.56578412734584,45.2397628867565));
#52471=CARTESIAN_POINT('Ctrl Pts',(-3.52575508348954,3.47457186233093,45.1984841028063));
#52472=CARTESIAN_POINT('Ctrl Pts',(-2.37758390575486,4.63965651937944,45.1455638487244));
#52473=CARTESIAN_POINT('Ctrl Pts',(-0.594796197848898,5.17933734465609,
45.0926435946425));
#52474=CARTESIAN_POINT('Ctrl Pts',(1.00677715711088,4.84664815013159,45.0397233405605));
#52475=CARTESIAN_POINT('Ctrl Pts',(2.60835051207067,4.51395895560708,44.9868030864785));
#52476=CARTESIAN_POINT('Ctrl Pts',(4.02870951408424,3.30889974128137,44.9338828323965));
#52477=CARTESIAN_POINT('Ctrl Pts',(4.61787619111481,1.78292400813641,44.8809625783145));
#52478=CARTESIAN_POINT('Ctrl Pts',(5.20704286814536,0.25694827499149,44.8280423242326));
#52479=CARTESIAN_POINT('Ctrl Pts',(4.96501722019298,-1.58994397697268,44.7751220701506));
#52480=CARTESIAN_POINT('Ctrl Pts',(4.00255388014552,-2.91258664622809,44.7222018160687));
#52481=CARTESIAN_POINT('Ctrl Pts',(3.04009054009802,-4.23522931548356,44.6692815619867));
#52482=CARTESIAN_POINT('Ctrl Pts',(1.35718950795542,-5.03362240203022,44.6163613079047));
#52483=CARTESIAN_POINT('Ctrl Pts',(-0.276028001533181,-4.94240903584718,
44.5634410538228));
#52484=CARTESIAN_POINT('Ctrl Pts',(-1.90924551102172,-4.85119566966413,
44.5105207997408));
#52485=CARTESIAN_POINT('Ctrl Pts',(-3.49277949785625,-3.8703758507514,44.4576005456588));
#52486=CARTESIAN_POINT('Ctrl Pts',(-4.30198062482356,-2.4487877080092,44.4046802915769));
#52487=CARTESIAN_POINT('Ctrl Pts',(-4.72176742799645,-1.71131475847591,
44.3772270126036));
#52488=CARTESIAN_POINT('Ctrl Pts',(-4.93316642875337,-0.85522261151742,
44.3497737336302));
#52489=CARTESIAN_POINT('Ctrl Pts',(-4.93394997286128,0.000507016503537849,
44.3223204546569));
#52490=CARTESIAN_POINT('Ctrl Pts',(-4.93390371744476,7.29331094537614E-5,
44.1776795453432));
#52491=CARTESIAN_POINT('Ctrl Pts',(-4.93379455568915,-0.829163376745596,
44.2042822496546));
#52492=CARTESIAN_POINT('Ctrl Pts',(-4.73595877931974,-1.65844862422957,
44.2308849539659));
#52493=CARTESIAN_POINT('Ctrl Pts',(-4.34068739432695,-2.37950250585247,
44.2574876582773));
#52494=CARTESIAN_POINT('Ctrl Pts',(-3.55438154059382,-3.813881288388,44.3104079123592));
#52495=CARTESIAN_POINT('Ctrl Pts',(-1.98677582129545,-4.81996270254719,
44.3633281664412));
#52496=CARTESIAN_POINT('Ctrl Pts',(-0.355230555152893,-4.9373485276323,
44.4162484205232));
#52497=CARTESIAN_POINT('Ctrl Pts',(1.27631471098969,-5.05473435271742,44.4691686746052));
#52498=CARTESIAN_POINT('Ctrl Pts',(2.97179952397649,-4.28342458872844,44.5220889286871));
#52499=CARTESIAN_POINT('Ctrl Pts',(3.95534413875573,-2.9763823636485,44.5750091827691));
#52500=CARTESIAN_POINT('Ctrl Pts',(4.93888875353493,-1.66934013856861,44.627929436851));
#52501=CARTESIAN_POINT('Ctrl Pts',(5.21049317010665,0.173434547602146,44.680849690933));
#52502=CARTESIAN_POINT('Ctrl Pts',(4.64586705931524,1.70865985432931,44.733769945015));
#52503=CARTESIAN_POINT('Ctrl Pts',(4.08124094852381,3.24388516105654,44.7866901990969));
#52504=CARTESIAN_POINT('Ctrl Pts',(2.68038431036912,4.47156108834011,44.8396104531789));
#52505=CARTESIAN_POINT('Ctrl Pts',(1.08435053733238,4.82988438193028,44.8925307072609));
#52506=CARTESIAN_POINT('Ctrl Pts',(-0.511683235704347,5.18820767552046,
44.9454509613428));
#52507=CARTESIAN_POINT('Ctrl Pts',(-2.30289414362315,4.67717833541725,44.9983712154248));
#52508=CARTESIAN_POINT('Ctrl Pts',(-3.46959671833554,3.53065119244912,45.0512914695067));
#52509=CARTESIAN_POINT('Ctrl Pts',(-4.39839859233384,2.61791080594467,45.0934208281189));
#52510=CARTESIAN_POINT('Ctrl Pts',(-4.93141112790613,1.30241637823199,45.1355501867311));
#52511=CARTESIAN_POINT('Ctrl Pts',(-4.94345166054126,-0.00439535110808767,
45.1776795453432));
#52512=CARTESIAN_POINT('Origin',(0.,0.,16.));
#52513=CARTESIAN_POINT('',(-4.94881445934699,0.00227942523971326,46.3223204546569));
#52514=CARTESIAN_POINT('',(-4.94828946219151,0.00267981890309541,46.1776795453432));
#52515=CARTESIAN_POINT('',(-4.942,-6.05220448138622E-16,16.));
#52516=CARTESIAN_POINT('Ctrl Pts',(-4.94881445934699,0.00227942523971326,
46.3223204546569));
#52517=CARTESIAN_POINT('Ctrl Pts',(-4.94955378308614,0.131274482234953,
46.3181501159471));
#52518=CARTESIAN_POINT('Ctrl Pts',(-4.94494719039334,0.260215895992481,
46.3139797772374));
#52519=CARTESIAN_POINT('Ctrl Pts',(-4.93482452766902,0.388722801454193,
46.3098094385276));
#52520=CARTESIAN_POINT('Ctrl Pts',(-4.80637120034064,2.01943401260374,46.2568891844456));
#52521=CARTESIAN_POINT('Ctrl Pts',(-3.78967659005442,3.58017725671765,46.2039689303636));
#52522=CARTESIAN_POINT('Ctrl Pts',(-2.34999567814797,4.35673258852779,46.1510486762817));
#52523=CARTESIAN_POINT('Ctrl Pts',(-0.910314766241556,5.13328792033792,
46.0981284221997));
#52524=CARTESIAN_POINT('Ctrl Pts',(0.952352447285067,5.12565533984434,46.0452081681177));
#52525=CARTESIAN_POINT('Ctrl Pts',(2.38562099756669,4.33732763245101,45.9922879140358));
#52526=CARTESIAN_POINT('Ctrl Pts',(3.81888954784836,3.54899992505766,45.9393676599538));
#52527=CARTESIAN_POINT('Ctrl Pts',(4.82275943488501,1.97997709076453,45.8864474058719));
#52528=CARTESIAN_POINT('Ctrl Pts',(4.93784446656618,0.348267941757418,45.8335271517899));
#52529=CARTESIAN_POINT('Ctrl Pts',(5.05292949824735,-1.28344120724965,45.7806068977079));
#52530=CARTESIAN_POINT('Ctrl Pts',(4.27922967457309,-2.97783667097068,45.727686643626));
#52531=CARTESIAN_POINT('Ctrl Pts',(2.97080185134115,-3.95953720721528,45.674766389544));
#52532=CARTESIAN_POINT('Ctrl Pts',(1.66237402810921,-4.94123774345989,45.621846135462));
#52533=CARTESIAN_POINT('Ctrl Pts',(-0.18078179468041,-5.21024335222807,
45.5689258813801));
#52534=CARTESIAN_POINT('Ctrl Pts',(-1.71520936255536,-4.64345295850584,
45.5160056272981));
#52535=CARTESIAN_POINT('Ctrl Pts',(-3.24963693043034,-4.0766625647836,45.4630853732162));
#52536=CARTESIAN_POINT('Ctrl Pts',(-4.47533624339064,-2.67407616857091,
45.4101651191342));
#52537=CARTESIAN_POINT('Ctrl Pts',(-4.8314085760891,-1.07753872605438,45.3572448650522));
#52538=CARTESIAN_POINT('Ctrl Pts',(-4.90973785658425,-0.726330228027688,
45.3456033949204));
#52539=CARTESIAN_POINT('Ctrl Pts',(-4.94598431844091,-0.365736088925451,
45.3339619247887));
#52540=CARTESIAN_POINT('Ctrl Pts',(-4.94264971735337,-0.00447858357024544,
45.3223204546569));
#52541=CARTESIAN_POINT('Ctrl Pts',(-4.94345166054126,-0.00439535110808767,
45.1776795453432));
#52542=CARTESIAN_POINT('Ctrl Pts',(-4.94653568871891,-0.339118433408757,
45.188470440813));
#52543=CARTESIAN_POINT('Ctrl Pts',(-4.91544069255685,-0.673271876348126,
45.1992613362828));
#52544=CARTESIAN_POINT('Ctrl Pts',(-4.848063077171,-0.999941813506336,45.2100522317526));
#52545=CARTESIAN_POINT('Ctrl Pts',(-4.51763261978812,-2.60198273066066,
45.2629724858346));
#52546=CARTESIAN_POINT('Ctrl Pts',(-3.31457746351644,-4.02403961913634,
45.3158927399166));
#52547=CARTESIAN_POINT('Ctrl Pts',(-1.78943402176491,-4.61535752812037,
45.3688129939985));
#52548=CARTESIAN_POINT('Ctrl Pts',(-0.264290580013278,-5.20667543710444,
45.4217332480805));
#52549=CARTESIAN_POINT('Ctrl Pts',(1.58294114721826,-4.96725436659668,45.4746535021624));
#52550=CARTESIAN_POINT('Ctrl Pts',(2.90693970933454,-4.00665705506737,45.5275737562444));
#52551=CARTESIAN_POINT('Ctrl Pts',(4.23093827145077,-3.0460597435381,45.5804940103263));
#52552=CARTESIAN_POINT('Ctrl Pts',(5.0317036684518,-1.36428619098739,45.6334142644083));
#52553=CARTESIAN_POINT('Ctrl Pts',(4.94279342482124,0.2690583397166,45.6863345184903));
#52554=CARTESIAN_POINT('Ctrl Pts',(4.85388318119067,1.90240287042061,45.7392547725723));
#52555=CARTESIAN_POINT('Ctrl Pts',(3.87529729692844,3.4873183792779,45.7921750266543));
#52556=CARTESIAN_POINT('Ctrl Pts',(2.45485161832049,4.29852332349801,45.8450952807362));
#52557=CARTESIAN_POINT('Ctrl Pts',(1.03440593971258,5.1097282677181,45.8980155348182));
#52558=CARTESIAN_POINT('Ctrl Pts',(-0.827899533241065,5.1472226473011,45.9509357889001));
#52559=CARTESIAN_POINT('Ctrl Pts',(-2.27984537368615,4.39384846150945,46.0038560429821));
#52560=CARTESIAN_POINT('Ctrl Pts',(-3.73179121413126,3.64047427571779,46.056776297064));
#52561=CARTESIAN_POINT('Ctrl Pts',(-4.77337742206781,2.0962315245515,46.109696551146));
#52562=CARTESIAN_POINT('Ctrl Pts',(-4.92795824091158,0.46778927569873,46.162616805228));
#52563=CARTESIAN_POINT('Ctrl Pts',(-4.94262440066108,0.31328760891278,46.1676377185997));
#52564=CARTESIAN_POINT('Ctrl Pts',(-4.94930605767903,0.158028008604056,
46.1726586319715));
#52565=CARTESIAN_POINT('Ctrl Pts',(-4.94828946219151,0.00267981890309541,
46.1776795453432));
#52566=CARTESIAN_POINT('Origin',(0.,0.,16.));
#52567=CARTESIAN_POINT('',(-4.9358501160701,0.00303175399314515,47.3223204546569));
#52568=CARTESIAN_POINT('',(-4.93538463697233,0.00269292579073279,47.1776795453432));
#52569=CARTESIAN_POINT('',(-4.942,-6.05220448138622E-16,16.));
#52570=CARTESIAN_POINT('Ctrl Pts',(-4.9358501160701,0.00303175399314515,
47.3223204546569));
#52571=CARTESIAN_POINT('Ctrl Pts',(-4.93933793021421,0.625283723714611,
47.3023383071056));
#52572=CARTESIAN_POINT('Ctrl Pts',(-4.83028758168748,1.24635811395051,47.2823561595543));
#52573=CARTESIAN_POINT('Ctrl Pts',(-4.60310972348256,1.82070849089976,47.2623740120029));
#52574=CARTESIAN_POINT('Ctrl Pts',(-4.00145717602152,3.34180464946569,47.2094537579209));
#52575=CARTESIAN_POINT('Ctrl Pts',(-2.57127018656423,4.53518329005682,47.156533503839));
#52576=CARTESIAN_POINT('Ctrl Pts',(-0.967024164301558,4.85473612062603,
47.103613249757));
#52577=CARTESIAN_POINT('Ctrl Pts',(0.637221857961163,5.17428895119525,47.050692995675));
#52578=CARTESIAN_POINT('Ctrl Pts',(2.41552691302929,4.62001597174252,46.9977727415931));
#52579=CARTESIAN_POINT('Ctrl Pts',(3.55411144818602,3.44556096290971,46.9448524875111));
#52580=CARTESIAN_POINT('Ctrl Pts',(4.69269598334273,2.27110595407693,46.8919322334292));
#52581=CARTESIAN_POINT('Ctrl Pts',(5.19155999858808,0.476468915864107,46.8390119793472));
#52582=CARTESIAN_POINT('Ctrl Pts',(4.82241570154595,-1.11709683409153,46.7860917252652));
#52583=CARTESIAN_POINT('Ctrl Pts',(4.45327140450381,-2.71066258404717,46.7331714711833));
#52584=CARTESIAN_POINT('Ctrl Pts',(3.21611879517418,-4.10315704574563,46.6802512171013));
#52585=CARTESIAN_POINT('Ctrl Pts',(1.67709780224552,-4.65735348636513,46.6273309630194));
#52586=CARTESIAN_POINT('Ctrl Pts',(0.138076809316829,-5.21154992698464,
46.5744107089374));
#52587=CARTESIAN_POINT('Ctrl Pts',(-1.7028125672109,-4.92744834652514,46.5214904548554));
#52588=CARTESIAN_POINT('Ctrl Pts',(-3.00315123328947,-3.93505796720279,
46.4685702007734));
#52589=CARTESIAN_POINT('Ctrl Pts',(-4.2010177406636,-3.02087212574391,46.4198202854013));
#52590=CARTESIAN_POINT('Ctrl Pts',(-4.94017200312835,-1.50563121453851,
46.3710703700291));
#52591=CARTESIAN_POINT('Ctrl Pts',(-4.94881445934699,0.00227942523971326,
46.3223204546569));
#52592=CARTESIAN_POINT('Ctrl Pts',(-4.94828946219151,0.00267981890309541,
46.1776795453432));
#52593=CARTESIAN_POINT('Ctrl Pts',(-4.93859117623925,-1.47933656262951,
46.2255788860534));
#52594=CARTESIAN_POINT('Ctrl Pts',(-4.22826766932132,-2.96941554830109,
46.2734782267636));
#52595=CARTESIAN_POINT('Ctrl Pts',(-3.06585319961028,-3.88640494404102,
46.3213775674738));
#52596=CARTESIAN_POINT('Ctrl Pts',(-1.78159190971431,-4.89951516838867,
46.3742978215558));
#52597=CARTESIAN_POINT('Ctrl Pts',(0.0545060998286173,-5.21309387054478,
46.4272180756378));
#52598=CARTESIAN_POINT('Ctrl Pts',(1.60221433767964,-4.68364264720964,46.4801383297198));
#52599=CARTESIAN_POINT('Ctrl Pts',(3.14992257553069,-4.15419142387448,46.5330585838017));
#52600=CARTESIAN_POINT('Ctrl Pts',(4.40924104168984,-2.78171027504809,46.5859788378836));
#52601=CARTESIAN_POINT('Ctrl Pts',(4.80388637285101,-1.19426753592463,46.6388990919656));
#52602=CARTESIAN_POINT('Ctrl Pts',(5.19853170401218,0.393175203198827,46.6918193460476));
#52603=CARTESIAN_POINT('Ctrl Pts',(4.72850390017529,2.19557953261941,46.7447396001296));
#52604=CARTESIAN_POINT('Ctrl Pts',(3.60889486296925,3.38813770361555,46.7976598542115));
#52605=CARTESIAN_POINT('Ctrl Pts',(2.48928582576321,4.58069587461169,46.8505801082935));
#52606=CARTESIAN_POINT('Ctrl Pts',(0.720095555188062,5.16340788718348,46.9035003623755));
#52607=CARTESIAN_POINT('Ctrl Pts',(-0.889067460630859,4.86961582479301,
46.9564206164574));
#52608=CARTESIAN_POINT('Ctrl Pts',(-2.49823047644978,4.57582376240254,47.0093408705394));
#52609=CARTESIAN_POINT('Ctrl Pts',(-3.9473662375124,3.40552762504981,47.0622611246213));
#52610=CARTESIAN_POINT('Ctrl Pts',(-4.57332808734244,1.89427279876787,47.1151813787033));
#52611=CARTESIAN_POINT('Ctrl Pts',(-4.81974582587867,1.29934836887573,47.1360141009166));
#52612=CARTESIAN_POINT('Ctrl Pts',(-4.93859613551441,0.651585501425685,
47.1568468231299));
#52613=CARTESIAN_POINT('Ctrl Pts',(-4.93538463697233,0.00269292579073279,
47.1776795453432));
#52614=CARTESIAN_POINT('Origin',(0.,0.,16.));
#52615=CARTESIAN_POINT('',(-4.93779824682792,-0.00394849367342132,48.3223204546569));
#52616=CARTESIAN_POINT('',(-4.93847649956811,-0.00414486738929824,48.1776795453433));
#52617=CARTESIAN_POINT('',(-4.942,-6.05220448138622E-16,16.));
#52618=CARTESIAN_POINT('Ctrl Pts',(-4.93779824682792,-0.00394849367342132,
48.3223204546569));
#52619=CARTESIAN_POINT('Ctrl Pts',(-4.92945107906705,1.10958389040538,48.286526498264));
#52620=CARTESIAN_POINT('Ctrl Pts',(-4.55663414200584,2.22817899674935,48.2507325418711));
#52621=CARTESIAN_POINT('Ctrl Pts',(-3.86551329136296,3.09215224876629,48.2149385854782));
#52622=CARTESIAN_POINT('Ctrl Pts',(-2.8437125545035,4.36950989861378,48.1620183313963));
#52623=CARTESIAN_POINT('Ctrl Pts',(-1.12614067807074,5.09029714456033,48.1090980773143));
#52624=CARTESIAN_POINT('Ctrl Pts',(0.50121521532169,4.92467073449426,48.0561778232323));
#52625=CARTESIAN_POINT('Ctrl Pts',(2.12857110871417,4.75904432442819,48.0032575691504));
#52626=CARTESIAN_POINT('Ctrl Pts',(3.66571101906626,3.70700425834946,47.9503373150684));
#52627=CARTESIAN_POINT('Ctrl Pts',(4.40921624712591,2.2499801379868,47.8974170609865));
#52628=CARTESIAN_POINT('Ctrl Pts',(5.15272147518552,0.792956017624232,47.8444968069045));
#52629=CARTESIAN_POINT('Ctrl Pts',(5.10259202095273,-1.06905215702231,47.7915765528226));
#52630=CARTESIAN_POINT('Ctrl Pts',(4.28176788829653,-2.4839610073443,47.7386562987406));
#52631=CARTESIAN_POINT('Ctrl Pts',(3.46094375564028,-3.89886985766637,47.6857360446586));
#52632=CARTESIAN_POINT('Ctrl Pts',(1.86942494456057,-4.86667938366393,47.6328157905766));
#52633=CARTESIAN_POINT('Ctrl Pts',(0.235514769794999,-4.94450516517706,
47.5798955364947));
#52634=CARTESIAN_POINT('Ctrl Pts',(-1.39839540497048,-5.02233094669018,
47.5269752824127));
#52635=CARTESIAN_POINT('Ctrl Pts',(-3.07469694342178,-4.21017298371899,
47.4740550283308));
#52636=CARTESIAN_POINT('Ctrl Pts',(-4.02628865991507,-2.87968716396305,
47.4211347742488));
#52637=CARTESIAN_POINT('Ctrl Pts',(-4.61856906134665,-2.05157920362054,
47.3881966677182));
#52638=CARTESIAN_POINT('Ctrl Pts',(-4.93010088448512,-1.0226738972605,47.3552585611876));
#52639=CARTESIAN_POINT('Ctrl Pts',(-4.9358501160701,0.00303175399314515,
47.3223204546569));
#52640=CARTESIAN_POINT('Ctrl Pts',(-4.93538463697233,0.00269292579073279,
47.1776795453432));
#52641=CARTESIAN_POINT('Ctrl Pts',(-4.93043813690577,-0.996761729574154,
47.2097670772119));
#52642=CARTESIAN_POINT('Ctrl Pts',(-4.63591709407219,-1.99889645937005,
47.2418546090805));
#52643=CARTESIAN_POINT('Ctrl Pts',(-4.07193915439288,-2.81476655400573,
47.2739421409492));
#52644=CARTESIAN_POINT('Ctrl Pts',(-3.1418004330159,-4.16033756528617,47.3268623950311));
#52645=CARTESIAN_POINT('Ctrl Pts',(-1.47873505166457,-4.99926607263594,
47.3797826491131));
#52646=CARTESIAN_POINT('Ctrl Pts',(0.156212871657996,-4.94764557838933,
47.4327029031951));
#52647=CARTESIAN_POINT('Ctrl Pts',(1.79116079498061,-4.89602508414272,47.4856231572771));
#52648=CARTESIAN_POINT('Ctrl Pts',(3.39799126027446,-3.95385558829969,47.538543411359));
#52649=CARTESIAN_POINT('Ctrl Pts',(4.24139410598325,-2.552288241629,47.591463665441));
#52650=CARTESIAN_POINT('Ctrl Pts',(5.08479695169201,-1.15072089495835,47.6443839195229));
#52651=CARTESIAN_POINT('Ctrl Pts',(5.16477217781576,0.710244302539926,47.6973041736049));
#52652=CARTESIAN_POINT('Ctrl Pts',(4.44472189944271,2.17900125452958,47.7502244276869));
#52653=CARTESIAN_POINT('Ctrl Pts',(3.72467162106964,3.64775820651928,47.8031446817689));
#52654=CARTESIAN_POINT('Ctrl Pts',(2.20459583819974,4.72430691300034,47.8560649358508));
#52655=CARTESIAN_POINT('Ctrl Pts',(0.580104444733958,4.91600224408279,47.9089851899327));
#52656=CARTESIAN_POINT('Ctrl Pts',(-1.04438694873177,5.10769757516524,47.9619054440147));
#52657=CARTESIAN_POINT('Ctrl Pts',(-2.77329395279337,4.41453953084916,48.0148256980967));
#52658=CARTESIAN_POINT('Ctrl Pts',(-3.81544231731622,3.15372781860764,48.0677459521787));
#52659=CARTESIAN_POINT('Ctrl Pts',(-4.53707600502276,2.28068110435693,48.1043904832335));
#52660=CARTESIAN_POINT('Ctrl Pts',(-4.92941962837742,1.13545330336185,48.1410350142884));
#52661=CARTESIAN_POINT('Ctrl Pts',(-4.93847649956811,-0.00414486738929824,
48.1776795453433));
#52662=CARTESIAN_POINT('Origin',(0.,0.,16.));
#52663=CARTESIAN_POINT('',(-4.94996872029631,-0.000754789231165454,49.3223204546569));
#52664=CARTESIAN_POINT('',(-4.95009281286112,-0.000267728824007536,49.1776795453432));
#52665=CARTESIAN_POINT('',(-4.942,-6.05220448138622E-16,16.));
#52666=CARTESIAN_POINT('Ctrl Pts',(-4.94996872029631,-0.000754789231165454,
49.3223204546569));
#52667=CARTESIAN_POINT('Ctrl Pts',(-4.94657205241788,1.59450047399929,49.2707146894224));
#52668=CARTESIAN_POINT('Ctrl Pts',(-4.10534559557285,3.19283284813315,49.219108924188));
#52669=CARTESIAN_POINT('Ctrl Pts',(-2.78707318578254,4.09094385103807,49.1675031589536));
#52670=CARTESIAN_POINT('Ctrl Pts',(-1.4352220784804,5.01193130760659,49.1145829048716));
#52671=CARTESIAN_POINT('Ctrl Pts',(0.418286878732396,5.19657136329379,49.0616626507896));
#52672=CARTESIAN_POINT('Ctrl Pts',(1.92525967895112,4.56036990866522,49.0087423967077));
#52673=CARTESIAN_POINT('Ctrl Pts',(3.4322324791698,3.92416845403667,48.9558221426257));
#52674=CARTESIAN_POINT('Ctrl Pts',(4.59266912239443,2.4671254890924,48.9029018885438));
#52675=CARTESIAN_POINT('Ctrl Pts',(4.87553607768602,0.856006127569342,48.8499816344618));
#52676=CARTESIAN_POINT('Ctrl Pts',(5.15840303297761,-0.755113233953766,
48.7970613803799));
#52677=CARTESIAN_POINT('Ctrl Pts',(4.56370030033613,-2.52030899205568,48.7441411262979));
#52678=CARTESIAN_POINT('Ctrl Pts',(3.36357293293406,-3.63180060852569,48.6912208722159));
#52679=CARTESIAN_POINT('Ctrl Pts',(2.16344556553202,-4.74329222499568,48.6383006181339));
#52680=CARTESIAN_POINT('Ctrl Pts',(0.357893563369426,-5.20107969983381,
48.585380364052));
#52681=CARTESIAN_POINT('Ctrl Pts',(-1.22683490171212,-4.79567249290391,
48.53246010997));
#52682=CARTESIAN_POINT('Ctrl Pts',(-2.81156336679367,-4.39026528597401,
48.4795398558881));
#52683=CARTESIAN_POINT('Ctrl Pts',(-4.17546829479417,-3.12166339727609,
48.4266196018061));
#52684=CARTESIAN_POINT('Ctrl Pts',(-4.69440596015137,-1.57039842605291,
48.3736993477241));
#52685=CARTESIAN_POINT('Ctrl Pts',(-4.86234697051046,-1.0683708724689,48.356573050035));
#52686=CARTESIAN_POINT('Ctrl Pts',(-4.94179210764521,-0.536739194059861,
48.339446752346));
#52687=CARTESIAN_POINT('Ctrl Pts',(-4.93779824682792,-0.00394849367342132,
48.3223204546569));
#52688=CARTESIAN_POINT('Ctrl Pts',(-4.93847649956811,-0.00414486738929824,
48.1776795453433));
#52689=CARTESIAN_POINT('Ctrl Pts',(-4.942499122392,-0.510299091646249,48.1939552683704));
#52690=CARTESIAN_POINT('Ctrl Pts',(-4.87091055869885,-1.01534275567644,
48.2102309913974));
#52691=CARTESIAN_POINT('Ctrl Pts',(-4.7189797263556,-1.49493463832769,48.2265067144245));
#52692=CARTESIAN_POINT('Ctrl Pts',(-4.224979045888,-3.05432000285457,48.2794269685065));
#52693=CARTESIAN_POINT('Ctrl Pts',(-2.88158795996869,-4.34462535174135,
48.3323472225885));
#52694=CARTESIAN_POINT('Ctrl Pts',(-1.30356274672183,-4.77538725089245,
48.3852674766704));
#52695=CARTESIAN_POINT('Ctrl Pts',(0.274462466525034,-5.20614915004355,
48.4381877307524));
#52696=CARTESIAN_POINT('Ctrl Pts',(2.08712180709941,-4.77736759945896,48.4911079848343));
#52697=CARTESIAN_POINT('Ctrl Pts',(3.30491467655429,-3.68525958533767,48.5440282389163));
#52698=CARTESIAN_POINT('Ctrl Pts',(4.5227075460092,-2.59315157121635,48.5969484929983));
#52699=CARTESIAN_POINT('Ctrl Pts',(5.14563394434455,-0.837717093558183,
48.6498687470803));
#52700=CARTESIAN_POINT('Ctrl Pts',(4.88863323791471,0.7777302204381,48.7027890011622));
#52701=CARTESIAN_POINT('Ctrl Pts',(4.63163253148487,2.39317753443434,48.7557092552442));
#52702=CARTESIAN_POINT('Ctrl Pts',(3.49470472029,3.86863768476876,48.8086295093261));
#52703=CARTESIAN_POINT('Ctrl Pts',(1.99812533468889,4.52891757238984,48.8615497634081));
#52704=CARTESIAN_POINT('Ctrl Pts',(0.501545949087793,5.18919746001092,48.91447001749));
#52705=CARTESIAN_POINT('Ctrl Pts',(-1.35468501091949,5.03429708491863,48.967390271572));
#52706=CARTESIAN_POINT('Ctrl Pts',(-2.7211279083772,4.13510122450199,49.020310525654));
#52707=CARTESIAN_POINT('Ctrl Pts',(-4.07559217393182,3.24378797391906,49.0727668655504));
#52708=CARTESIAN_POINT('Ctrl Pts',(-4.94881798417885,1.62117145762289,49.1252232054468));
#52709=CARTESIAN_POINT('Ctrl Pts',(-4.95009281286112,-0.000267728824007536,
49.1776795453432));
#52710=CARTESIAN_POINT('Origin',(0.,0.,16.));
#52711=CARTESIAN_POINT('',(-4.94000433004934,0.00442567287284368,50.3223204546569));
#52712=CARTESIAN_POINT('',(-4.93925722597112,0.00431400617654748,50.1776795453432));
#52713=CARTESIAN_POINT('',(-4.942,-6.05220448138622E-16,16.));
#52714=CARTESIAN_POINT('Ctrl Pts',(-4.94000433004934,0.00442567287284368,
50.3223204546569));
#52715=CARTESIAN_POINT('Ctrl Pts',(-4.94391985550658,0.454920647205931,
50.3078231346629));
#52716=CARTESIAN_POINT('Ctrl Pts',(-4.88736862134446,0.904450331901516,
50.2933258146688));
#52717=CARTESIAN_POINT('Ctrl Pts',(-4.76643244788693,1.33593422554585,50.2788284946748));
#52718=CARTESIAN_POINT('Ctrl Pts',(-4.3249734037525,2.91100032695947,50.2259082405929));
#52719=CARTESIAN_POINT('Ctrl Pts',(-3.02558272518919,4.24560561283798,50.1729879865109));
#52720=CARTESIAN_POINT('Ctrl Pts',(-1.46288143191014,4.72901432133872,50.120067732429));
#52721=CARTESIAN_POINT('Ctrl Pts',(0.0998198613689605,5.21242302983948,
50.067147478347));
#52722=CARTESIAN_POINT('Ctrl Pts',(1.92583176936386,4.84463516096244,50.014227224265));
#52723=CARTESIAN_POINT('Ctrl Pts',(3.17954335484605,3.79395606061911,49.961306970183));
#52724=CARTESIAN_POINT('Ctrl Pts',(4.43325494032821,2.74327696027582,49.9083867161011));
#52725=CARTESIAN_POINT('Ctrl Pts',(5.11466620329769,1.00970662846638,49.8554664620191));
#52726=CARTESIAN_POINT('Ctrl Pts',(4.91195294283073,-0.613446674675755,
49.8025462079371));
#52727=CARTESIAN_POINT('Ctrl Pts',(4.70923968236377,-2.23659997781789,49.7496259538552));
#52728=CARTESIAN_POINT('Ctrl Pts',(3.62240189846027,-3.74933625229266,49.6967056997732));
#52729=CARTESIAN_POINT('Ctrl Pts',(2.14879315998069,-4.45940427533482,49.6437854456913));
#52730=CARTESIAN_POINT('Ctrl Pts',(0.675184421501018,-5.16947229837701,
49.5908651916093));
#52731=CARTESIAN_POINT('Ctrl Pts',(-1.18519527155483,-5.0768720699865,49.5379449375273));
#52732=CARTESIAN_POINT('Ctrl Pts',(-2.58100775862557,-4.22397886893019,
49.4850246834454));
#52733=CARTESIAN_POINT('Ctrl Pts',(-3.97682024569624,-3.37108566787394,
49.4321044293634));
#52734=CARTESIAN_POINT('Ctrl Pts',(-4.9080655267819,-1.75789949415196,49.3791841752814));
#52735=CARTESIAN_POINT('Ctrl Pts',(-4.94859153862899,-0.12263897856609,
49.3262639211994));
#52736=CARTESIAN_POINT('Ctrl Pts',(-4.94959816627151,-0.0820206605359307,
49.3249494323519));
#52737=CARTESIAN_POINT('Ctrl Pts',(-4.9500552393514,-0.0413887231133244,
49.3236349435044));
#52738=CARTESIAN_POINT('Ctrl Pts',(-4.94996872029631,-0.000754789231165454,
49.3223204546569));
#52739=CARTESIAN_POINT('Ctrl Pts',(-4.95009281286112,-0.000267728824007536,
49.1776795453432));
#52740=CARTESIAN_POINT('Ctrl Pts',(-4.95010408721063,-0.0146074376385199,
49.1781434595288));
#52741=CARTESIAN_POINT('Ctrl Pts',(-4.95004716359657,-0.02894705437045,
49.1786073737143));
#52742=CARTESIAN_POINT('Ctrl Pts',(-4.94992177176232,-0.0432860723615371,
49.1790712878999));
#52743=CARTESIAN_POINT('Ctrl Pts',(-4.93561790278161,-1.6789861630675,49.2319915419818));
#52744=CARTESIAN_POINT('Ctrl Pts',(-4.03035532991194,-3.30689499873837,
49.2849117960638));
#52745=CARTESIAN_POINT('Ctrl Pts',(-2.6483960323012,-4.18205663360964,49.3378320501458));
#52746=CARTESIAN_POINT('Ctrl Pts',(-1.26643673469055,-5.05721826848085,
49.3907523042277));
#52747=CARTESIAN_POINT('Ctrl Pts',(0.592219287661027,-5.17963270255261,
49.4436725583097));
#52748=CARTESIAN_POINT('Ctrl Pts',(2.07702265223193,-4.49328122119488,49.4965928123917));
#52749=CARTESIAN_POINT('Ctrl Pts',(3.56182601680279,-3.80692973983718,49.5495130664736));
#52750=CARTESIAN_POINT('Ctrl Pts',(4.67277672359291,-2.31181234304998,49.6024333205556));
#52751=CARTESIAN_POINT('Ctrl Pts',(4.90148676195955,-0.692117586080884,
49.6553535746375));
#52752=CARTESIAN_POINT('Ctrl Pts',(5.13019680032621,0.927577170888348,49.7082738287195));
#52753=CARTESIAN_POINT('Ctrl Pts',(4.47666617026921,2.67184928803957,49.7611940828015));
#52754=CARTESIAN_POINT('Ctrl Pts',(3.23996046927922,3.7424932048215,49.8141143368834));
#52755=CARTESIAN_POINT('Ctrl Pts',(2.00325476828929,4.81313712160337,49.8670345909654));
#52756=CARTESIAN_POINT('Ctrl Pts',(0.183373996366374,5.21015283801606,49.9199548450474));
#52757=CARTESIAN_POINT('Ctrl Pts',(-1.38687661076657,4.75185989872763,49.9728750991293));
#52758=CARTESIAN_POINT('Ctrl Pts',(-2.95712721789961,4.29356695943917,50.0257953532113));
#52759=CARTESIAN_POINT('Ctrl Pts',(-4.27774766024261,2.97996536444961,50.0787156072932));
#52760=CARTESIAN_POINT('Ctrl Pts',(-4.74440185394119,1.41217926586765,50.1316358613752));
#52761=CARTESIAN_POINT('Ctrl Pts',(-4.87974057311241,0.957491050521679,
50.1469837560312));
#52762=CARTESIAN_POINT('Ctrl Pts',(-4.94325117479429,0.481423074070403,
50.1623316506872));
#52763=CARTESIAN_POINT('Ctrl Pts',(-4.93925722597112,0.00431400617654748,
50.1776795453432));
#52764=CARTESIAN_POINT('Origin',(0.,0.,16.));
#52765=CARTESIAN_POINT('',(-4.9346053643787,-0.00190906406864477,51.3223204546569));
#52766=CARTESIAN_POINT('',(-4.93494424898874,-0.00229539766483815,51.1776795453432));
#52767=CARTESIAN_POINT('',(-4.942,-6.05220448138622E-16,16.));
#52768=CARTESIAN_POINT('Ctrl Pts',(-4.9346053643787,-0.00190906406864477,
51.3223204546569));
#52769=CARTESIAN_POINT('Ctrl Pts',(-4.93132359046474,0.942525285964724,
51.2920113258213));
#52770=CARTESIAN_POINT('Ctrl Pts',(-4.67058264693544,1.88863740917005,51.2617021969857));
#52771=CARTESIAN_POINT('Ctrl Pts',(-4.16399066183724,2.67671072463696,51.2313930681501));
#52772=CARTESIAN_POINT('Ctrl Pts',(-3.27947244580022,4.05270012756452,51.1784728140682));
#52773=CARTESIAN_POINT('Ctrl Pts',(-1.64545880455478,4.94689631680689,51.1255525599862));
#52774=CARTESIAN_POINT('Ctrl Pts',(-0.00969933613304136,4.95010145937766,
51.0726323059043));
#52775=CARTESIAN_POINT('Ctrl Pts',(1.62606013228874,4.95330660194842,51.0197120518223));
#52776=CARTESIAN_POINT('Ctrl Pts',(3.26356542788682,4.06552069784751,50.9667917977403));
#52777=CARTESIAN_POINT('Ctrl Pts',(4.15346911827026,2.69300813567829,50.9138715436584));
#52778=CARTESIAN_POINT('Ctrl Pts',(5.04337280865373,1.32049557350902,50.8609512895764));
#52779=CARTESIAN_POINT('Ctrl Pts',(5.18567489382252,-0.536743646728604,
50.8080310354945));
#52780=CARTESIAN_POINT('Ctrl Pts',(4.5152557662665,-2.0288084927985,50.7551107814125));
#52781=CARTESIAN_POINT('Ctrl Pts',(3.8448366387105,-3.52087333886836,50.7021905273305));
#52782=CARTESIAN_POINT('Ctrl Pts',(2.36169629842972,-4.64776381077051,50.6492702732485));
#52783=CARTESIAN_POINT('Ctrl Pts',(0.74454241669244,-4.89379761790371,50.5963500191666));
#52784=CARTESIAN_POINT('Ctrl Pts',(-0.872611465044887,-5.13983142503691,
50.5434297650846));
#52785=CARTESIAN_POINT('Ctrl Pts',(-2.62377888823873,-4.50500856740112,
50.4905095110027));
#52786=CARTESIAN_POINT('Ctrl Pts',(-3.70759889498285,-3.27983368010881,
50.4375892569207));
#52787=CARTESIAN_POINT('Ctrl Pts',(-4.49451017129344,-2.39029120233235,
50.3991663228328));
#52788=CARTESIAN_POINT('Ctrl Pts',(-4.92962682740573,-1.18954250282331,
50.3607433887448));
#52789=CARTESIAN_POINT('Ctrl Pts',(-4.94000433004934,0.00442567287284368,
50.3223204546569));
#52790=CARTESIAN_POINT('Ctrl Pts',(-4.93925722597112,0.00431400617654748,
50.1776795453432));
#52791=CARTESIAN_POINT('Ctrl Pts',(-4.92947985362941,-1.16367116612706,
50.2152519047692));
#52792=CARTESIAN_POINT('Ctrl Pts',(-4.51515233090316,-2.33789552818176,
50.2528242641951));
#52793=CARTESIAN_POINT('Ctrl Pts',(-3.75970560074729,-3.21997096669155,
50.2903966236211));
#52794=CARTESIAN_POINT('Ctrl Pts',(-2.69566720880064,-4.46236449849485,
50.3433168777031));
#52795=CARTESIAN_POINT('Ctrl Pts',(-0.95490247985317,-5.12518095992721,
50.396237131785));
#52796=CARTESIAN_POINT('Ctrl Pts',(0.665988059953313,-4.90510541524102,
50.449157385867));
#52797=CARTESIAN_POINT('Ctrl Pts',(2.28687859975984,-4.68502987055481,50.5020776399489));
#52798=CARTESIAN_POINT('Ctrl Pts',(3.78789495042532,-3.58206231974999,50.5549978940309));
#52799=CARTESIAN_POINT('Ctrl Pts',(4.48214910531455,-2.10093755936608,50.6079181481129));
#52800=CARTESIAN_POINT('Ctrl Pts',(5.17640326020376,-0.619812798982218,
50.6608384021949));
#52801=CARTESIAN_POINT('Ctrl Pts',(5.06389521931669,1.2394691709808,50.7137586562768));
#52802=CARTESIAN_POINT('Ctrl Pts',(4.19611038046471,2.62607252481409,50.7666789103588));
#52803=CARTESIAN_POINT('Ctrl Pts',(3.32832554161272,4.01267587864738,50.8195991644407));
#52804=CARTESIAN_POINT('Ctrl Pts',(1.70526390479588,4.92660061635104,50.8725194185227));
#52805=CARTESIAN_POINT('Ctrl Pts',(0.0696632635531223,4.94962081985461,
50.9254396726047));
#52806=CARTESIAN_POINT('Ctrl Pts',(-1.56593737768968,4.97264102335818,50.9783599266866));
#52807=CARTESIAN_POINT('Ctrl Pts',(-3.21407702335836,4.1047566926616,51.0312801807686));
#52808=CARTESIAN_POINT('Ctrl Pts',(-4.12054180005445,2.74312495242765,51.0842004348505));
#52809=CARTESIAN_POINT('Ctrl Pts',(-4.65427267801061,1.94138954819395,51.1153601383481));
#52810=CARTESIAN_POINT('Ctrl Pts',(-4.93087142137606,0.968476272531438,
51.1465198418457));
#52811=CARTESIAN_POINT('Ctrl Pts',(-4.93494424898874,-0.00229539766483815,
51.1776795453432));
#52812=CARTESIAN_POINT('Origin',(0.,0.,16.));
#52813=CARTESIAN_POINT('',(-4.94698954266231,-0.00340802453188072,52.3223204546568));
#52814=CARTESIAN_POINT('',(-4.94764183754834,-0.00307943510729547,52.1776795453432));
#52815=CARTESIAN_POINT('',(-4.942,-6.05220448138622E-16,16.));
#52816=CARTESIAN_POINT('Ctrl Pts',(-4.94698954266231,-0.00340802453188072,
52.3223204546568));
#52817=CARTESIAN_POINT('Ctrl Pts',(-4.93574079437759,1.42456851634609,52.2761995169797));
#52818=CARTESIAN_POINT('Ctrl Pts',(-4.28342182577614,2.86150661417242,52.2300785793026));
#52819=CARTESIAN_POINT('Ctrl Pts',(-3.19438680274345,3.78146684366169,52.1839576416255));
#52820=CARTESIAN_POINT('Ctrl Pts',(-1.94480227507184,4.83705095668842,52.1310373875436));
#52821=CARTESIAN_POINT('Ctrl Pts',(-0.120245685876333,5.21199182863453,
52.0781171334615));
#52822=CARTESIAN_POINT('Ctrl Pts',(1.44433800372382,4.73471079013843,52.0251968793796));
#52823=CARTESIAN_POINT('Ctrl Pts',(3.00892169332389,4.25742975164236,51.9722766252976));
#52824=CARTESIAN_POINT('Ctrl Pts',(4.31353248332859,2.92792680270421,51.9193563712157));
#52825=CARTESIAN_POINT('Ctrl Pts',(4.7611605513041,1.3546027978562,51.8664361171337));
#52826=CARTESIAN_POINT('Ctrl Pts',(5.20878861927959,-0.218721206991761,
51.8135158630518));
#52827=CARTESIAN_POINT('Ctrl Pts',(4.79943396522586,-2.03586626774964,51.7605956089698));
#52828=CARTESIAN_POINT('Ctrl Pts',(3.72042353078829,-3.26527905190521,51.7076753548878));
#52829=CARTESIAN_POINT('Ctrl Pts',(2.64141309635066,-4.49469183606084,51.6547551008059));
#52830=CARTESIAN_POINT('Ctrl Pts',(0.892746881529132,-5.1363723436142,51.6018348467239));
#52831=CARTESIAN_POINT('Ctrl Pts',(-0.725358746921474,-4.8966777741157,
51.5489145926419));
#52832=CARTESIAN_POINT('Ctrl Pts',(-2.34346437537199,-4.65698320461722,
51.49599433856));
#52833=CARTESIAN_POINT('Ctrl Pts',(-3.83100941745154,-3.535913558067,51.443074084478));
#52834=CARTESIAN_POINT('Ctrl Pts',(-4.50727054307715,-2.04648742648548,
51.3901538303961));
#52835=CARTESIAN_POINT('Ctrl Pts',(-4.79621520662888,-1.41010346743882,
51.3675427051497));
#52836=CARTESIAN_POINT('Ctrl Pts',(-4.93705362349566,-0.70647314083382,
51.3449315799033));
#52837=CARTESIAN_POINT('Ctrl Pts',(-4.9346053643787,-0.00190906406864477,
51.3223204546569));
#52838=CARTESIAN_POINT('Ctrl Pts',(-4.93494424898874,-0.00229539766483815,
51.1776795453432));
#52839=CARTESIAN_POINT('Ctrl Pts',(-4.9377885305877,-0.680239141156077,
51.1994400959276));
#52840=CARTESIAN_POINT('Ctrl Pts',(-4.80772180958983,-1.35713842276963,
51.221200646512));
#52841=CARTESIAN_POINT('Ctrl Pts',(-4.53950114466406,-1.9739626613036,51.2429611970964));
#52842=CARTESIAN_POINT('Ctrl Pts',(-3.88720580485411,-3.47403938502989,
51.2958814511784));
#52843=CARTESIAN_POINT('Ctrl Pts',(-2.41782521751062,-4.61881368271118,
51.3488017052603));
#52844=CARTESIAN_POINT('Ctrl Pts',(-0.803770380809228,-4.88441935193539,
51.4017219593423));
#52845=CARTESIAN_POINT('Ctrl Pts',(0.810284455892164,-5.1500250211596,51.4546422134243));
#52846=CARTESIAN_POINT('Ctrl Pts',(2.56901354195146,-4.53646206192671,51.5075624675063));
#52847=CARTESIAN_POINT('Ctrl Pts',(3.6675955870482,-3.32450625514402,51.5604827215882));
#52848=CARTESIAN_POINT('Ctrl Pts',(4.7661776321449,-2.11255044836137,51.6134029756702));
#52849=CARTESIAN_POINT('Ctrl Pts',(5.20461263627908,-0.302201794028944,
51.6663232297521));
#52850=CARTESIAN_POINT('Ctrl Pts',(4.78226604547315,1.27809651472091,51.7192434838341));
#52851=CARTESIAN_POINT('Ctrl Pts',(4.3599194546672,2.85839482347081,51.7721637379161));
#52852=CARTESIAN_POINT('Ctrl Pts',(3.07679126892111,4.20864278663813,51.825083991998));
#52853=CARTESIAN_POINT('Ctrl Pts',(1.52006054286266,4.71094631434696,51.87800424608));
#52854=CARTESIAN_POINT('Ctrl Pts',(-0.0366701831957017,5.21324984205576,
51.930924500162));
#52855=CARTESIAN_POINT('Ctrl Pts',(-1.86700344956638,4.86760893430616,51.9838447542439));
#52856=CARTESIAN_POINT('Ctrl Pts',(-3.13335079942941,3.83219414935389,52.0367650083259));
#52857=CARTESIAN_POINT('Ctrl Pts',(-4.25734861844162,2.9131698704424,52.083736520665));
#52858=CARTESIAN_POINT('Ctrl Pts',(-4.93702884968978,1.45073013335928,52.1307080330041));
#52859=CARTESIAN_POINT('Ctrl Pts',(-4.94764183754834,-0.00307943510729547,
52.1776795453432));
#52860=CARTESIAN_POINT('Origin',(0.,0.,16.));
#52861=CARTESIAN_POINT('',(-4.94509673752737,0.0040742516207555,53.3223204546569));
#52862=CARTESIAN_POINT('',(-4.94431829400652,0.00425244366110885,53.1776795453432));
#52863=CARTESIAN_POINT('',(-4.942,-6.05220448138622E-16,16.));
#52864=CARTESIAN_POINT('Ctrl Pts',(-4.94509673752737,0.0040742516207555,
53.3223204546569));
#52865=CARTESIAN_POINT('Ctrl Pts',(-4.94757864022345,0.283393084706415,
53.3133079622201));
#52866=CARTESIAN_POINT('Ctrl Pts',(-4.92595073565188,0.562327591030859,
53.3042954697834));
#52867=CARTESIAN_POINT('Ctrl Pts',(-4.87885318126865,0.836893165749963,
53.2952829773467));
#52868=CARTESIAN_POINT('Ctrl Pts',(-4.60230209819144,2.44910866310731,53.2423627232647));
#52869=CARTESIAN_POINT('Ctrl Pts',(-3.44758426677398,3.91068799192893,53.1894424691828));
#52870=CARTESIAN_POINT('Ctrl Pts',(-1.94311620233063,4.55279012908506,53.1365222151008));
#52871=CARTESIAN_POINT('Ctrl Pts',(-0.438648137887247,5.19489226624121,
53.0836019610189));
#52872=CARTESIAN_POINT('Ctrl Pts',(1.4155701595821,5.01751721173186,53.0306817069369));
#52873=CARTESIAN_POINT('Ctrl Pts',(2.77102007823768,4.10183449949628,52.9777614528549));
#52874=CARTESIAN_POINT('Ctrl Pts',(4.12646999689325,3.1861517872607,52.924841198773));
#52875=CARTESIAN_POINT('Ctrl Pts',(4.98315153673507,1.53216141729899,52.871920944691));
#52876=CARTESIAN_POINT('Ctrl Pts',(4.9490341412924,-0.10324535619766,52.8190006906091));
#52877=CARTESIAN_POINT('Ctrl Pts',(4.91491674584974,-1.73865212969422,52.7660804365271));
#52878=CARTESIAN_POINT('Ctrl Pts',(3.99000041512261,-3.35547530672568,52.7131601824451));
#52879=CARTESIAN_POINT('Ctrl Pts',(2.59754098802034,-4.21383190822896,52.6602399283632));
#52880=CARTESIAN_POINT('Ctrl Pts',(1.205081560918,-5.07218850973229,52.6073196742812));
#52881=CARTESIAN_POINT('Ctrl Pts',(-0.654920962559591,-5.17207853570735,
52.5543994201993));
#52882=CARTESIAN_POINT('Ctrl Pts',(-2.13130102041059,-4.4677907846777,52.5014791661173));
#52883=CARTESIAN_POINT('Ctrl Pts',(-3.6076810782616,-3.76350303364805,52.4485589120353));
#52884=CARTESIAN_POINT('Ctrl Pts',(-4.70043867048604,-2.25503750561363,
52.3956386579533));
#52885=CARTESIAN_POINT('Ctrl Pts',(-4.90951123352436,-0.632691064542821,
52.3427184038713));
#52886=CARTESIAN_POINT('Ctrl Pts',(-4.93637335904372,-0.424248248792036,
52.3359190874665));
#52887=CARTESIAN_POINT('Ctrl Pts',(-4.94864787405361,-0.213925520686765,
52.3291197710617));
#52888=CARTESIAN_POINT('Ctrl Pts',(-4.94698954266231,-0.00340802453188072,
52.3223204546568));
#52889=CARTESIAN_POINT('Ctrl Pts',(-4.94764183754834,-0.00307943510729547,
52.1776795453432));
#52890=CARTESIAN_POINT('Ctrl Pts',(-4.94898592720496,-0.187198217650565,
52.1836282870861));
#52891=CARTESIAN_POINT('Ctrl Pts',(-4.93959875206843,-0.371178579690442,
52.1895770288289));
#52892=CARTESIAN_POINT('Ctrl Pts',(-4.91902378063747,-0.553899157022463,
52.1955257705718));
#52893=CARTESIAN_POINT('Ctrl Pts',(-4.73598797862701,-2.17938901629118,
52.2484460246538));
#52894=CARTESIAN_POINT('Ctrl Pts',(-3.66755494125079,-3.70518007267354,
52.3013662787357));
#52895=CARTESIAN_POINT('Ctrl Pts',(-2.2026559442682,-4.43304703582165,52.3542865328177));
#52896=CARTESIAN_POINT('Ctrl Pts',(-0.737756947285612,-5.16091399896976,
52.4072067868996));
#52897=CARTESIAN_POINT('Ctrl Pts',(1.12360800930335,-5.09085686888362,52.4601270409816));
#52898=CARTESIAN_POINT('Ctrl Pts',(2.52964989329714,-4.2549348582521,52.5130472950635));
#52899=CARTESIAN_POINT('Ctrl Pts',(3.93569177729098,-3.41901284762056,52.5659675491455));
#52900=CARTESIAN_POINT('Ctrl Pts',(4.88641058868961,-1.81722595644361,52.6188878032275));
#52901=CARTESIAN_POINT('Ctrl Pts',(4.94674287935491,-0.182576329732651,
52.6718080573094));
#52902=CARTESIAN_POINT('Ctrl Pts',(5.0070751700202,1.45207329697826,52.7247283113914));
#52903=CARTESIAN_POINT('Ctrl Pts',(4.17702093995222,3.11958565922317,52.7776485654734));
#52904=CARTESIAN_POINT('Ctrl Pts',(2.83642568199835,4.05688163262466,52.8305688195553));
#52905=CARTESIAN_POINT('Ctrl Pts',(1.49583042404448,4.99417760602615,52.8834890736373));
#52906=CARTESIAN_POINT('Ctrl Pts',(-0.355305861795278,5.20125719058422,
52.9364093277193));
#52907=CARTESIAN_POINT('Ctrl Pts',(-1.86987493927361,4.58335760574097,52.9893295818012));
#52908=CARTESIAN_POINT('Ctrl Pts',(-3.384444016752,3.9654580208977,53.0422498358832));
#52909=CARTESIAN_POINT('Ctrl Pts',(-4.56244588586893,2.52257926665306,53.0951700899651));
#52910=CARTESIAN_POINT('Ctrl Pts',(-4.86480890004871,0.915004697602124,
53.1480903440471));
#52911=CARTESIAN_POINT('Ctrl Pts',(-4.92116211960056,0.615391324314909,
53.1579534111458));
#52912=CARTESIAN_POINT('Ctrl Pts',(-4.94709912492537,0.310057072885753,
53.1678164782445));
#52913=CARTESIAN_POINT('Ctrl Pts',(-4.94431829400652,0.00425244366110885,
53.1776795453432));
#52914=CARTESIAN_POINT('Origin',(0.,0.,16.));
#52915=CARTESIAN_POINT('',(-4.93403082595878,0.000832190755156725,54.3223204546569));
#52916=CARTESIAN_POINT('',(-4.93393232083006,0.000401187422265207,54.1776795453432));
#52917=CARTESIAN_POINT('',(-4.942,-6.05220448138622E-16,16.));
#52918=CARTESIAN_POINT('Ctrl Pts',(-4.93403082595878,0.000832190755156725,
54.3223204546569));
#52919=CARTESIAN_POINT('Ctrl Pts',(-4.93519480376781,0.77458390453562,54.2974961533786));
#52920=CARTESIAN_POINT('Ctrl Pts',(-4.76408859627892,1.54784860488958,54.2726718521003));
#52921=CARTESIAN_POINT('Ctrl Pts',(-4.41799967623941,2.23268389970517,54.2478475508221));
#52922=CARTESIAN_POINT('Ctrl Pts',(-3.6802099846732,3.69261050145239,54.1949272967401));
#52923=CARTESIAN_POINT('Ctrl Pts',(-2.14720464186602,4.75066627671043,54.1420070426582));
#52924=CARTESIAN_POINT('Ctrl Pts',(-0.52051030581542,4.92266874335397,54.0890867885762));
#52925=CARTESIAN_POINT('Ctrl Pts',(1.10618403023518,5.0946712099975,54.0361665344942));
#52926=CARTESIAN_POINT('Ctrl Pts',(2.82656735952921,4.38062036802653,53.9832462804122));
#52927=CARTESIAN_POINT('Ctrl Pts',(3.85336599568517,3.10727678821045,53.9303260263302));
#52928=CARTESIAN_POINT('Ctrl Pts',(4.8801646318411,1.83393320839441,53.8774057722483));
#52929=CARTESIAN_POINT('Ctrl Pts',(5.21337857485901,0.00129689073330608,
53.8244855181664));
#52930=CARTESIAN_POINT('Ctrl Pts',(4.70052403533771,-1.55198979650856,53.7715652640844));
#52931=CARTESIAN_POINT('Ctrl Pts',(4.18766949581641,-3.10527648375042,53.7186450100024));
#52932=CARTESIAN_POINT('Ctrl Pts',(2.82874647375599,-4.37921354057296,53.6657247559204));
#52933=CARTESIAN_POINT('Ctrl Pts',(1.24561889847324,-4.79082791331733,53.6128045018385));
#52934=CARTESIAN_POINT('Ctrl Pts',(-0.337508676809509,-5.2024422860617,
53.5598842477565));
#52935=CARTESIAN_POINT('Ctrl Pts',(-2.14484080531469,-4.75173397472772,
53.5069639936746));
#52936=CARTESIAN_POINT('Ctrl Pts',(-3.34931470219873,-3.64495398611418,
53.4540437395926));
#52937=CARTESIAN_POINT('Ctrl Pts',(-4.34866275314335,-2.72666225118592,
53.4101359779474));
#52938=CARTESIAN_POINT('Ctrl Pts',(-4.93300521093011,-1.35673296483636,
53.3662282163021));
#52939=CARTESIAN_POINT('Ctrl Pts',(-4.94509673752737,0.0040742516207555,
53.3223204546569));
#52940=CARTESIAN_POINT('Ctrl Pts',(-4.94431829400652,0.00425244366110885,
53.1776795453432));
#52941=CARTESIAN_POINT('Ctrl Pts',(-4.93217858577541,-1.33073665953657,
53.2207367323265));
#52942=CARTESIAN_POINT('Ctrl Pts',(-4.37274694612505,-2.67469001651735,
53.2637939193098));
#52943=CARTESIAN_POINT('Ctrl Pts',(-3.4073211579765,-3.59078845896452,53.306851106293));
#52944=CARTESIAN_POINT('Ctrl Pts',(-2.22074624248181,-4.71673666262315,
53.359771360375));
#52945=CARTESIAN_POINT('Ctrl Pts',(-0.42087225224974,-5.19636268608309,
53.4126916144569));
#52946=CARTESIAN_POINT('Ctrl Pts',(1.16865098585596,-4.81018233582522,53.4656118685389));
#52947=CARTESIAN_POINT('Ctrl Pts',(2.75817422396157,-4.42400198556738,53.5185321226208));
#52948=CARTESIAN_POINT('Ctrl Pts',(4.13734670994089,-3.17201526159183,53.5714523767028));
#52949=CARTESIAN_POINT('Ctrl Pts',(4.6750380505237,-1.62715041000601,53.6243726307848));
#52950=CARTESIAN_POINT('Ctrl Pts',(5.2127293911065,-0.0822855584201898,
53.6772928848668));
#52951=CARTESIAN_POINT('Ctrl Pts',(4.90893958629287,1.75545742077581,53.7302131389487));
#52952=CARTESIAN_POINT('Ctrl Pts',(3.9026874904557,3.045099273007,53.7831333930307));
#52953=CARTESIAN_POINT('Ctrl Pts',(2.89643539461849,4.33474112523822,53.8360536471126));
#52954=CARTESIAN_POINT('Ctrl Pts',(1.18772100775765,5.0762818505045,53.8889739011946));
#52955=CARTESIAN_POINT('Ctrl Pts',(-0.441521870018959,4.93038108759577,
53.9418941552766));
#52956=CARTESIAN_POINT('Ctrl Pts',(-2.07076474779552,4.78448032468705,53.9948144093585));
#52957=CARTESIAN_POINT('Ctrl Pts',(-3.62053611648792,3.75113807360336,54.0477346634405));
#52958=CARTESIAN_POINT('Ctrl Pts',(-4.38163692859106,2.30322753036564,54.1006549175225));
#52959=CARTESIAN_POINT('Ctrl Pts',(-4.75089382782116,1.60075691273335,54.1263297934627));
#52960=CARTESIAN_POINT('Ctrl Pts',(-4.9345120375631,0.800704467282281,54.152004669403));
#52961=CARTESIAN_POINT('Ctrl Pts',(-4.93393232083006,0.000401187422265207,
54.1776795453432));
#52962=CARTESIAN_POINT('Origin',(0.,0.,16.));
#52963=CARTESIAN_POINT('',(-4.94204396072975,-0.00451108372972908,55.3223204546568));
#52964=CARTESIAN_POINT('',(-4.94284599866247,-0.00446247280752122,55.1776795453432));
#52965=CARTESIAN_POINT('',(-4.942,-6.05220448138622E-16,16.));
#52966=CARTESIAN_POINT('Ctrl Pts',(-4.94204396072975,-0.00451108372972908,
55.3223204546568));
#52967=CARTESIAN_POINT('Ctrl Pts',(-4.93045565886636,1.25690241555476,55.281684344537));
#52968=CARTESIAN_POINT('Ctrl Pts',(-4.43833582829864,2.52635331123123,55.2410482344173));
#52969=CARTESIAN_POINT('Ctrl Pts',(-3.56758671933519,3.43160655309978,55.2004121242975));
#52970=CARTESIAN_POINT('Ctrl Pts',(-2.43361341450575,4.61051446104039,55.1474918702155));
#52971=CARTESIAN_POINT('Ctrl Pts',(-0.65749411504605,5.17175205664432,55.0945716161334));
#52972=CARTESIAN_POINT('Ctrl Pts',(0.947991861475882,4.85848844455039,55.0416513620514));
#52973=CARTESIAN_POINT('Ctrl Pts',(2.55347783799768,4.54522483245649,54.9887311079695));
#52974=CARTESIAN_POINT('Ctrl Pts',(3.98833049158174,3.35746001266491,54.9358108538876));
#52975=CARTESIAN_POINT('Ctrl Pts',(4.59593933387555,1.83873330708663,54.8828905998056));
#52976=CARTESIAN_POINT('Ctrl Pts',(5.2035481761694,0.320006601508274,54.8299703457237));
#52977=CARTESIAN_POINT('Ctrl Pts',(4.98391320717291,-1.52968198985681,54.7770500916417));
#52978=CARTESIAN_POINT('Ctrl Pts',(4.0375427431176,-2.86388671786309,54.7241298375597));
#52979=CARTESIAN_POINT('Ctrl Pts',(3.09117227906232,-4.19809144586933,54.6712095834777));
#52980=CARTESIAN_POINT('Ctrl Pts',(1.41806631994828,-5.0168123105168,54.6182893293958));
#52981=CARTESIAN_POINT('Ctrl Pts',(-0.216136294490469,-4.94539014006561,
54.5653690753138));
#52982=CARTESIAN_POINT('Ctrl Pts',(-1.85033890892918,-4.87396796961441,
54.5124488212319));
#52983=CARTESIAN_POINT('Ctrl Pts',(-3.4456381786926,-3.91240276406461,54.4595285671499));
#52984=CARTESIAN_POINT('Ctrl Pts',(-4.27200079341172,-2.50072144717157,
54.4066083130679));
#52985=CARTESIAN_POINT('Ctrl Pts',(-4.7107259171786,-1.75124409976784,54.3785123602642));
#52986=CARTESIAN_POINT('Ctrl Pts',(-4.93271344484821,-0.874894033659396,
54.3504164074605));
#52987=CARTESIAN_POINT('Ctrl Pts',(-4.93403082595878,0.000832190755156725,
54.3223204546569));
#52988=CARTESIAN_POINT('Ctrl Pts',(-4.93393232083006,0.000401187422265207,
54.1776795453432));
#52989=CARTESIAN_POINT('Ctrl Pts',(-4.93331714350093,-0.848855710199169,
54.2049249234849));
#52990=CARTESIAN_POINT('Ctrl Pts',(-4.72528049547278,-1.69839506725433,
54.2321703016266));
#52991=CARTESIAN_POINT('Ctrl Pts',(-4.31154403127411,-2.43191021565593,
54.2594156797684));
#52992=CARTESIAN_POINT('Ctrl Pts',(-3.50792006634005,-3.85665858304818,
54.3123359338503));
#52993=CARTESIAN_POINT('Ctrl Pts',(-1.92824188095795,-4.8436764824408,54.3652561879323));
#52994=CARTESIAN_POINT('Ctrl Pts',(-0.295394338707872,-4.9412894486446,
54.4181764420142));
#52995=CARTESIAN_POINT('Ctrl Pts',(1.33745320354216,-5.0389024148484,54.4710966960962));
#52996=CARTESIAN_POINT('Ctrl Pts',(3.02347010266025,-4.24711044786332,54.5240169501782));
#52997=CARTESIAN_POINT('Ctrl Pts',(3.99110927558139,-2.92824964458212,54.5769372042601));
#52998=CARTESIAN_POINT('Ctrl Pts',(4.95874844850256,-1.60938884130088,54.6298574583421));
#52999=CARTESIAN_POINT('Ctrl Pts',(5.20800989522687,0.236540798276539,54.6827777124241));
#53000=CARTESIAN_POINT('Ctrl Pts',(4.62482777083827,1.76481367875202,54.735697966506));
#53001=CARTESIAN_POINT('Ctrl Pts',(4.04164564644968,3.29308655922746,54.788618220588));
#53002=CARTESIAN_POINT('Ctrl Pts',(2.62601995094824,4.50370268060093,54.8415384746699));
#53003=CARTESIAN_POINT('Ctrl Pts',(1.02576262302031,4.84266561635652,54.8944587287519));
#53004=CARTESIAN_POINT('Ctrl Pts',(-0.574494704907621,5.1816285521121,54.9473789828339));
#53005=CARTESIAN_POINT('Ctrl Pts',(-2.35938366526199,4.64893830224978,55.0002992369159));
#53006=CARTESIAN_POINT('Ctrl Pts',(-3.51211180971311,3.48836206072432,55.0532194909978));
#53007=CARTESIAN_POINT('Ctrl Pts',(-4.4157898059278,2.57853157081683,55.0947061757796));
#53008=CARTESIAN_POINT('Ctrl Pts',(-4.93095870305679,1.2828191742603,55.1361928605614));
#53009=CARTESIAN_POINT('Ctrl Pts',(-4.94284599866247,-0.00446247280752122,
55.1776795453432));
#53010=CARTESIAN_POINT('Origin',(0.,0.,16.));
#53011=CARTESIAN_POINT('',(-4.94916162572937,0.00195780085970945,56.3223204546569));
#53012=CARTESIAN_POINT('',(-4.9486927940556,0.00238008058365034,56.1776795453432));
#53013=CARTESIAN_POINT('',(-4.942,-6.05220448138622E-16,16.));
#53014=CARTESIAN_POINT('Ctrl Pts',(-4.94916162572937,0.00195780085970945,
56.3223204546569));
#53015=CARTESIAN_POINT('Ctrl Pts',(-4.94971144692239,0.111053665337975,
56.3187927897774));
#53016=CARTESIAN_POINT('Ctrl Pts',(-4.94641661384693,0.220115719674017,
56.315265124898));
#53017=CARTESIAN_POINT('Ctrl Pts',(-4.93917135292333,0.328914702796541,
56.3117374600186));
#53018=CARTESIAN_POINT('Ctrl Pts',(-4.83048159296228,1.96106232098248,56.2588172059367));
#53019=CARTESIAN_POINT('Ctrl Pts',(-3.83276814539685,3.53400710106189,56.2058969518547));
#53020=CARTESIAN_POINT('Ctrl Pts',(-2.40259992160997,4.32794548855851,56.1529766977728));
#53021=CARTESIAN_POINT('Ctrl Pts',(-0.972431697823093,5.12188387605513,
56.1000564436908));
#53022=CARTESIAN_POINT('Ctrl Pts',(0.890191302185183,5.13681587096895,56.0471361896088));
#53023=CARTESIAN_POINT('Ctrl Pts',(2.33290434633096,4.36590836437554,55.9942159355269));
#53024=CARTESIAN_POINT('Ctrl Pts',(3.77561739047674,3.59500085778213,55.9412956814449));
#53025=CARTESIAN_POINT('Ctrl Pts',(4.79842047875997,2.03825384968152,55.8883754273629));
#53026=CARTESIAN_POINT('Ctrl Pts',(4.93326329701873,0.408058546708748,55.8354551732809));
#53027=CARTESIAN_POINT('Ctrl Pts',(5.0681061152775,-1.22213675626403,55.782534919199));
#53028=CARTESIAN_POINT('Ctrl Pts',(4.31498866351168,-2.92578035410902,55.729614665117));
#53029=CARTESIAN_POINT('Ctrl Pts',(3.01854898978546,-3.92325891721657,55.6766944110351));
#53030=CARTESIAN_POINT('Ctrl Pts',(1.72210931605921,-4.92073748032415,55.6237741569531));
#53031=CARTESIAN_POINT('Ctrl Pts',(-0.117652579627481,-5.21205100869435,
55.5708539028712));
#53032=CARTESIAN_POINT('Ctrl Pts',(-1.65883355567899,-4.66388998260118,
55.5179336487892));
#53033=CARTESIAN_POINT('Ctrl Pts',(-3.20001453173045,-4.11572895650802,
55.4650133947072));
#53034=CARTESIAN_POINT('Ctrl Pts',(-4.4426145881467,-2.72809337595155,55.4120931406252));
#53035=CARTESIAN_POINT('Ctrl Pts',(-4.81800096125524,-1.13598647553473,
55.3591728865432));
#53036=CARTESIAN_POINT('Ctrl Pts',(-4.90513773579808,-0.766417759225417,
55.3468887425811));
#53037=CARTESIAN_POINT('Ctrl Pts',(-4.94554706100059,-0.385831662281748,
55.334604598619));
#53038=CARTESIAN_POINT('Ctrl Pts',(-4.94204396072975,-0.00451108372972908,
55.3223204546568));
#53039=CARTESIAN_POINT('Ctrl Pts',(-4.94284599866247,-0.00446247280752122,
55.1776795453432));
#53040=CARTESIAN_POINT('Ctrl Pts',(-4.94612209119225,-0.359232298306442,
55.1891131146434));
#53041=CARTESIAN_POINT('Ctrl Pts',(-4.91117232521921,-0.713361781229651,
55.2005466839435));
#53042=CARTESIAN_POINT('Ctrl Pts',(-4.83559423534505,-1.05859700628939,
55.2119802532437));
#53043=CARTESIAN_POINT('Ctrl Pts',(-4.48578118797803,-2.6565175985889,55.2649005073256));
#53044=CARTESIAN_POINT('Ctrl Pts',(-3.26558776469621,-4.06389654999934,
55.3178207614076));
#53045=CARTESIAN_POINT('Ctrl Pts',(-1.73339311164005,-4.63669575788038,
55.3707410154896));
#53046=CARTESIAN_POINT('Ctrl Pts',(-0.201198458583838,-5.20949496576144,
55.4236612695715));
#53047=CARTESIAN_POINT('Ctrl Pts',(1.64299742424673,-4.94771443011306,55.4765815236535));
#53048=CARTESIAN_POINT('Ctrl Pts',(2.95526233502001,-3.97114892214321,55.5295017777355));
#53049=CARTESIAN_POINT('Ctrl Pts',(4.26752724579325,-2.9945834141734,55.5824220318174));
#53050=CARTESIAN_POINT('Ctrl Pts',(5.04786118450924,-1.30323293388218,55.6353422858994));
#53051=CARTESIAN_POINT('Ctrl Pts',(4.93917142300628,0.328914707462642,55.6882625399813));
#53052=CARTESIAN_POINT('Ctrl Pts',(4.83048166150332,1.96106234880747,55.7411827940633));
#53053=CARTESIAN_POINT('Ctrl Pts',(3.83276819978142,3.5340071512059,55.7941030481453));
#53054=CARTESIAN_POINT('Ctrl Pts',(2.40259995570176,4.32794554996814,55.8470233022272));
#53055=CARTESIAN_POINT('Ctrl Pts',(0.972431711622098,5.12188394873038,55.8999435563092));
#53056=CARTESIAN_POINT('Ctrl Pts',(-0.890191314815322,5.13681594385641,
55.9528638103912));
#53057=CARTESIAN_POINT('Ctrl Pts',(-2.33290437943218,4.36590842632473,56.0057840644731));
#53058=CARTESIAN_POINT('Ctrl Pts',(-3.77561744404904,3.59500090879304,56.0587043185551));
#53059=CARTESIAN_POINT('Ctrl Pts',(-4.79842054684533,2.03825387860361,56.1116245726371));
#53060=CARTESIAN_POINT('Ctrl Pts',(-4.93326336701772,0.408058552499706,
56.164544826719));
#53061=CARTESIAN_POINT('Ctrl Pts',(-4.94441928789138,0.273187967299986,
56.1689230662604));
#53062=CARTESIAN_POINT('Ctrl Pts',(-4.94949737612309,0.137814649647994,
56.1733013058018));
#53063=CARTESIAN_POINT('Ctrl Pts',(-4.9486927940556,0.00238008058365034,
56.1776795453432));
#53064=CARTESIAN_POINT('Origin',(0.,0.,16.));
#53065=CARTESIAN_POINT('',(-4.93623902664834,0.00326946414225537,57.3223204546569));
#53066=CARTESIAN_POINT('',(-4.93573111423024,0.00295138605979709,57.1776795453432));
#53067=CARTESIAN_POINT('',(-4.942,-6.05220448138622E-16,16.));
#53068=CARTESIAN_POINT('Ctrl Pts',(-4.93623902664834,0.00326946414225537,
57.3223204546569));
#53069=CARTESIAN_POINT('Ctrl Pts',(-4.93989713650663,0.605389273547052,
57.3029809809359));
#53070=CARTESIAN_POINT('Ctrl Pts',(-4.83794904041642,1.20631307007342,57.2836415072149));
#53071=CARTESIAN_POINT('Ctrl Pts',(-4.62482770521538,1.76481365371148,57.2643020334939));
#53072=CARTESIAN_POINT('Ctrl Pts',(-4.04164558910142,3.29308651250188,57.211381779412));
#53073=CARTESIAN_POINT('Ctrl Pts',(-2.6260199136863,4.50370261669748,57.15846152533));
#53074=CARTESIAN_POINT('Ctrl Pts',(-1.02576260846464,4.84266554764316,57.1055412712481));
#53075=CARTESIAN_POINT('Ctrl Pts',(0.574494696756969,5.18162847858883,57.0526210171661));
#53076=CARTESIAN_POINT('Ctrl Pts',(2.35938363178511,4.64893823628462,56.9997007630841));
#53077=CARTESIAN_POINT('Ctrl Pts',(3.51211175987971,3.48836201122659,56.9467805090022));
#53078=CARTESIAN_POINT('Ctrl Pts',(4.66483988797431,2.32778578616857,56.8938602549202));
#53079=CARTESIAN_POINT('Ctrl Pts',(5.18540720913538,0.539323578356728,56.8409400008383));
#53080=CARTESIAN_POINT('Ctrl Pts',(4.83559416673167,-1.05859699126952,56.7880197467563));
#53081=CARTESIAN_POINT('Ctrl Pts',(4.48578112432795,-2.65651756089581,56.7350994926743));
#53082=CARTESIAN_POINT('Ctrl Pts',(3.26558771835941,-4.0638964923365,56.6821792385924));
#53083=CARTESIAN_POINT('Ctrl Pts',(1.73339308704371,-4.63669569208971,56.6292589845104));
#53084=CARTESIAN_POINT('Ctrl Pts',(0.201198455728012,-5.20949489184292,
56.5763387304284));
#53085=CARTESIAN_POINT('Ctrl Pts',(-1.64299740093485,-4.94771435990864,
56.5234184763465));
#53086=CARTESIAN_POINT('Ctrl Pts',(-2.95526229308795,-3.97114886579523,
56.4704982222645));
#53087=CARTESIAN_POINT('Ctrl Pts',(-4.18005158912286,-3.0596812412178,56.4211056330619));
#53088=CARTESIAN_POINT('Ctrl Pts',(-4.94146330594845,-1.52554761761349,
56.3717130438594));
#53089=CARTESIAN_POINT('Ctrl Pts',(-4.94916162572937,0.00195780085970945,
56.3223204546569));
#53090=CARTESIAN_POINT('Ctrl Pts',(-4.9486927940556,0.00238008058365034,
56.1776795453432));
#53091=CARTESIAN_POINT('Ctrl Pts',(-4.93977230579782,-1.49919761032442,
56.2262215598838));
#53092=CARTESIAN_POINT('Ctrl Pts',(-4.20773066973569,-3.00830456759471,
56.2747635744243));
#53093=CARTESIAN_POINT('Ctrl Pts',(-3.018549032617,-3.92325897288391,56.3233055889649));
#53094=CARTESIAN_POINT('Ctrl Pts',(-1.72210934049551,-4.92073755014514,
56.3762258430469));
#53095=CARTESIAN_POINT('Ctrl Pts',(0.117652581295909,-5.2120510826492,56.4291460971289));
#53096=CARTESIAN_POINT('Ctrl Pts',(1.65883357921563,-4.66389004877836,56.4820663512108));
#53097=CARTESIAN_POINT('Ctrl Pts',(3.2000145771353,-4.11572901490753,56.5349866052928));
#53098=CARTESIAN_POINT('Ctrl Pts',(4.44261465118334,-2.72809341466183,56.5879068593747));
#53099=CARTESIAN_POINT('Ctrl Pts',(4.8180010296186,-1.13598649165438,56.6408271134567));
#53100=CARTESIAN_POINT('Ctrl Pts',(5.19338740805387,0.456120431353115,56.6937473675386));
#53101=CARTESIAN_POINT('Ctrl Pts',(4.70156009087639,2.25269867712231,56.7466676216206));
#53102=CARTESIAN_POINT('Ctrl Pts',(3.56758676995704,3.43160660179086,56.7995878757026));
#53103=CARTESIAN_POINT('Ctrl Pts',(2.43361344903769,4.61051452645941,56.8525081297845));
#53104=CARTESIAN_POINT('Ctrl Pts',(0.65749412437644,5.17175213002719,56.9054283838665));
#53105=CARTESIAN_POINT('Ctrl Pts',(-0.94799187492607,4.85848851348866,56.9583486379485));
#53106=CARTESIAN_POINT('Ctrl Pts',(-2.55347787422853,4.54522489695015,57.0112688920304));
#53107=CARTESIAN_POINT('Ctrl Pts',(-3.98833054817231,3.35746006030537,57.0641891461124));
#53108=CARTESIAN_POINT('Ctrl Pts',(-4.59593939908791,1.83873333317766,57.1171094001944));
#53109=CARTESIAN_POINT('Ctrl Pts',(-4.82775332951413,1.25931120769625,57.1372994485773));
#53110=CARTESIAN_POINT('Ctrl Pts',(-4.93915674573565,0.631715508347176,
57.1574894969603));
#53111=CARTESIAN_POINT('Ctrl Pts',(-4.93573111423024,0.00295138605979709,
57.1776795453432));
#53112=CARTESIAN_POINT('Origin',(0.,0.,16.));
#53113=CARTESIAN_POINT('',(-4.9373129524182,-0.00377529733612325,58.3223204546568));
#53114=CARTESIAN_POINT('',(-4.93796046055574,-0.00400002009900308,58.1776795453432));
#53115=CARTESIAN_POINT('',(-4.942,-6.05220448138622E-16,16.));
#53116=CARTESIAN_POINT('Ctrl Pts',(-4.9373129524182,-0.00377529733612325,
58.3223204546568));
#53117=CARTESIAN_POINT('Ctrl Pts',(-4.92952693668152,1.09003472006405,58.2871691720943));
#53118=CARTESIAN_POINT('Ctrl Pts',(-4.57107143779465,2.18847891881712,58.2520178895318));
#53119=CARTESIAN_POINT('Ctrl Pts',(-3.90268743507911,3.04509922980021,58.2168666069693));
#53120=CARTESIAN_POINT('Ctrl Pts',(-2.89643535351957,4.33474106373227,58.1639463528874));
#53121=CARTESIAN_POINT('Ctrl Pts',(-1.18772099090388,5.07628177847635,58.1110260988054));
#53122=CARTESIAN_POINT('Ctrl Pts',(0.441521863755048,4.93038101763753,58.0581058447234));
#53123=CARTESIAN_POINT('Ctrl Pts',(2.07076471841393,4.78448025679871,58.0051855906414));
#53124=CARTESIAN_POINT('Ctrl Pts',(3.62053606511612,3.75113802037702,57.9522653365595));
#53125=CARTESIAN_POINT('Ctrl Pts',(4.38163686641958,2.30322749768385,57.8993450824775));
#53126=CARTESIAN_POINT('Ctrl Pts',(5.14273766772306,0.855316974990642,57.8464248283956));
#53127=CARTESIAN_POINT('Ctrl Pts',(5.11516792362781,-1.00716183397399,57.7935045743136));
#53128=CARTESIAN_POINT('Ctrl Pts',(4.31154397009623,-2.43191018115001,57.7405843202316));
#53129=CARTESIAN_POINT('Ctrl Pts',(3.50792001656464,-3.85665852832602,57.6876640661497));
#53130=CARTESIAN_POINT('Ctrl Pts',(1.92824185359667,-4.84367641371333,57.6347438120677));
#53131=CARTESIAN_POINT('Ctrl Pts',(0.295394334515388,-4.94128937853172,
57.5818235579858));
#53132=CARTESIAN_POINT('Ctrl Pts',(-1.33745318456585,-5.03890234335011,
57.5289033039038));
#53133=CARTESIAN_POINT('Ctrl Pts',(-3.02347005976055,-4.24711038759957,
57.4759830498218));
#53134=CARTESIAN_POINT('Ctrl Pts',(-3.99110921895138,-2.92824960303174,
57.4230627957398));
#53135=CARTESIAN_POINT('Ctrl Pts',(-4.60512891022411,-2.09136068211493,
57.3894820153788));
#53136=CARTESIAN_POINT('Ctrl Pts',(-4.9298871379951,-1.04224259902719,57.3559012350179));
#53137=CARTESIAN_POINT('Ctrl Pts',(-4.93623902664834,0.00326946414225537,
57.3223204546569));
#53138=CARTESIAN_POINT('Ctrl Pts',(-4.93573111423024,0.00295138605979709,
57.1776795453432));
#53139=CARTESIAN_POINT('Ctrl Pts',(-4.93017780293081,-1.01634181563486,
57.2104097510422));
#53140=CARTESIAN_POINT('Ctrl Pts',(-4.62285556832308,-2.03870561435216,
57.2431399567412));
#53141=CARTESIAN_POINT('Ctrl Pts',(-4.03754280040764,-2.86388675849859,
57.2758701624402));
#53142=CARTESIAN_POINT('Ctrl Pts',(-3.09117232292437,-4.19809150543631,
57.3287904165222));
#53143=CARTESIAN_POINT('Ctrl Pts',(-1.41806634007047,-5.01681238170109,
57.3817106706042));
#53144=CARTESIAN_POINT('Ctrl Pts',(0.216136297556334,-4.94539021023678,
57.4346309246861));
#53145=CARTESIAN_POINT('Ctrl Pts',(1.85033893518309,-4.87396803877247,57.4875511787681));
#53146=CARTESIAN_POINT('Ctrl Pts',(3.4456382275827,-3.91240281957913,57.5404714328501));
#53147=CARTESIAN_POINT('Ctrl Pts',(4.27200085402752,-2.50072148265561,57.593391686932));
#53148=CARTESIAN_POINT('Ctrl Pts',(5.0983634804724,-1.08904014573198,57.646311941014));
#53149=CARTESIAN_POINT('Ctrl Pts',(5.15578944096228,0.772757308922017,57.699232195096));
#53150=CARTESIAN_POINT('Ctrl Pts',(4.41799973892759,2.23268393138458,57.7521524491779));
#53151=CARTESIAN_POINT('Ctrl Pts',(3.68021003689295,3.69261055384702,57.8050727032599));
#53152=CARTESIAN_POINT('Ctrl Pts',(2.14720467233395,4.75066634411819,57.8579929573418));
#53153=CARTESIAN_POINT('Ctrl Pts',(0.520510313201973,4.9226688132026,57.9109132114238));
#53154=CARTESIAN_POINT('Ctrl Pts',(-1.1061840459301,5.09467128228702,57.9638334655058));
#53155=CARTESIAN_POINT('Ctrl Pts',(-2.8265673996351,4.38062043018456,58.0167537195877));
#53156=CARTESIAN_POINT('Ctrl Pts',(-3.85336605036076,3.10727683230095,58.0696739736697));
#53157=CARTESIAN_POINT('Ctrl Pts',(-4.5519012154505,2.2410161688934,58.1056758308942));
#53158=CARTESIAN_POINT('Ctrl Pts',(-4.92943605312281,1.11590730173118,58.1416776881187));
#53159=CARTESIAN_POINT('Ctrl Pts',(-4.93796046055574,-0.00400002009900308,
58.1776795453432));
#53160=CARTESIAN_POINT('Origin',(0.,0.,16.));
#53161=CARTESIAN_POINT('',(-4.94980236868244,-0.00111614563719775,59.3223204546569));
#53162=CARTESIAN_POINT('',(-4.95000952859661,-0.000636468299896517,59.1776795453432));
#53163=CARTESIAN_POINT('',(-4.942,-6.05220448138622E-16,16.));
#53164=CARTESIAN_POINT('Ctrl Pts',(-4.94980236868244,-0.00111614563719775,
59.3223204546569));
#53165=CARTESIAN_POINT('Ctrl Pts',(-4.94498060556177,1.57441454729254,59.2713573632528));
#53166=CARTESIAN_POINT('Ctrl Pts',(-4.12744131963774,3.15424986030506,59.2203942718487));
#53167=CARTESIAN_POINT('Ctrl Pts',(-2.83642564175097,4.05688157506129,59.1694311804446));
#53168=CARTESIAN_POINT('Ctrl Pts',(-1.49583040281886,4.99417753516308,59.1165109263627));
#53169=CARTESIAN_POINT('Ctrl Pts',(0.355305856754859,5.20125711678249,59.0635906722807));
#53170=CARTESIAN_POINT('Ctrl Pts',(1.86987491274258,4.58335754070639,59.0106704181987));
#53171=CARTESIAN_POINT('Ctrl Pts',(3.38444396873026,3.96545796463031,58.9577501641168));
#53172=CARTESIAN_POINT('Ctrl Pts',(4.56244582113197,2.52257923085877,58.9048299100348));
#53173=CARTESIAN_POINT('Ctrl Pts',(4.86480883102114,0.915004684618019,58.8519096559529));
#53174=CARTESIAN_POINT('Ctrl Pts',(5.16717184091031,-0.692569861622737,
58.7989894018709));
#53175=CARTESIAN_POINT('Ctrl Pts',(4.59389600828695,-2.46484022033272,58.7460691477889));
#53176=CARTESIAN_POINT('Ctrl Pts',(3.40732110962866,-3.59078840801476,58.6931488937069));
#53177=CARTESIAN_POINT('Ctrl Pts',(2.22074621097036,-4.7167365956968,58.640228639625));
#53178=CARTESIAN_POINT('Ctrl Pts',(0.42087224627713,-5.1963626123509,58.5873083855431));
#53179=CARTESIAN_POINT('Ctrl Pts',(-1.16865096927437,-4.81018226757243,
58.5343881314611));
#53180=CARTESIAN_POINT('Ctrl Pts',(-2.75817418482588,-4.42400192279397,
58.4814678773791));
#53181=CARTESIAN_POINT('Ctrl Pts',(-4.13734665123566,-3.17201521658293,
58.4285476232971));
#53182=CARTESIAN_POINT('Ctrl Pts',(-4.67503798418886,-1.62715038691743,
58.3756273692152));
#53183=CARTESIAN_POINT('Ctrl Pts',(-4.85557797114165,-1.10843293863767,
58.3578583976957));
#53184=CARTESIAN_POINT('Ctrl Pts',(-4.94124878297087,-0.556696204625704,
58.3400894261763));
#53185=CARTESIAN_POINT('Ctrl Pts',(-4.9373129524182,-0.00377529733612325,
58.3223204546568));
#53186=CARTESIAN_POINT('Ctrl Pts',(-4.93796046055574,-0.00400002009900308,
58.1776795453432));
#53187=CARTESIAN_POINT('Ctrl Pts',(-4.94196634578065,-0.530279439411995,
58.1945979422007));
#53188=CARTESIAN_POINT('Ctrl Pts',(-4.86448168129051,-1.05541017361004,
58.2115163390581));
#53189=CARTESIAN_POINT('Ctrl Pts',(-4.70052410203468,-1.55198981852916,
58.2284347359156));
#53190=CARTESIAN_POINT('Ctrl Pts',(-4.18766955523667,-3.10527652781102,
58.2813549899975));
#53191=CARTESIAN_POINT('Ctrl Pts',(-2.82874651389436,-4.37921360271005,
58.3342752440795));
#53192=CARTESIAN_POINT('Ctrl Pts',(-1.24561891614835,-4.79082798129515,
58.3871954981615));
#53193=CARTESIAN_POINT('Ctrl Pts',(0.337508681597706,-5.20244235988026,
58.4401157522434));
#53194=CARTESIAN_POINT('Ctrl Pts',(2.14484083574746,-4.75173404215139,58.4930360063254));
#53195=CARTESIAN_POINT('Ctrl Pts',(3.34931474972224,-3.6449540378337,58.5459562604074));
#53196=CARTESIAN_POINT('Ctrl Pts',(4.55378866369698,-2.53817403351603,58.5988765144893));
#53197=CARTESIAN_POINT('Ctrl Pts',(5.15540433749678,-0.775322342609574,
58.6517967685713));
#53198=CARTESIAN_POINT('Ctrl Pts',(4.87885325049583,0.836893177623885,58.7047170226533));
#53199=CARTESIAN_POINT('Ctrl Pts',(4.60230216349487,2.44910869785739,58.7576372767352));
#53200=CARTESIAN_POINT('Ctrl Pts',(3.44758431569312,3.91068804741789,58.8105575308172));
#53201=CARTESIAN_POINT('Ctrl Pts',(1.94311622990263,4.5527901936852,58.8634777848992));
#53202=CARTESIAN_POINT('Ctrl Pts',(0.438648144112182,5.19489233995249,58.9163980389811));
#53203=CARTESIAN_POINT('Ctrl Pts',(-1.41557017966698,5.01751728292666,58.969318293063));
#53204=CARTESIAN_POINT('Ctrl Pts',(-2.77102011755545,4.10183455769855,59.022238547145));
#53205=CARTESIAN_POINT('Ctrl Pts',(-4.09812694403132,3.205299199536,59.0740522132111));
#53206=CARTESIAN_POINT('Ctrl Pts',(-4.94710627363632,1.60101008771938,59.1258658792772));
#53207=CARTESIAN_POINT('Ctrl Pts',(-4.95000952859661,-0.000636468299896517,
59.1776795453432));
#53208=CARTESIAN_POINT('Origin',(0.,0.,16.));
#53209=CARTESIAN_POINT('',(-4.9405850371911,0.0044815032353801,60.3223204546569));
#53210=CARTESIAN_POINT('',(-4.93981933179839,0.00440230787564107,60.1776795453432));
#53211=CARTESIAN_POINT('',(-4.942,-6.05220448138622E-16,16.));
#53212=CARTESIAN_POINT('Ctrl Pts',(-4.9405850371911,0.0044815032353801,
60.3223204546569));
#53213=CARTESIAN_POINT('Ctrl Pts',(-4.94441025446321,0.434877172261215,
60.3084658084932));
#53214=CARTESIAN_POINT('Ctrl Pts',(-4.89283730030809,0.864370712953886,
60.2946111623296));
#53215=CARTESIAN_POINT('Ctrl Pts',(-4.78226597761638,1.27809649658665,60.2807565161659));
#53216=CARTESIAN_POINT('Ctrl Pts',(-4.3599193928029,2.85839478291331,60.2278362620839));
#53217=CARTESIAN_POINT('Ctrl Pts',(-3.07679122526311,4.20864272692144,60.1749160080019));
#53218=CARTESIAN_POINT('Ctrl Pts',(-1.52006052129332,4.71094624750269,60.12199575392));
#53219=CARTESIAN_POINT('Ctrl Pts',(0.0366701826763779,5.21324976808391,
60.069075499838));
#53220=CARTESIAN_POINT('Ctrl Pts',(1.867003423076,4.86760886523835,60.016155245756));
#53221=CARTESIAN_POINT('Ctrl Pts',(3.1333507549704,3.83219409497753,59.9632349916741));
#53222=CARTESIAN_POINT('Ctrl Pts',(4.39969808686486,2.79677932471666,59.9103147375921));
#53223=CARTESIAN_POINT('Ctrl Pts',(5.102059510254,1.07159068704033,59.8573944835102));
#53224=CARTESIAN_POINT('Ctrl Pts',(4.91902371084035,-0.55389914916401,59.8044742294282));
#53225=CARTESIAN_POINT('Ctrl Pts',(4.73598791142671,-2.1793889853683,59.7515539753462));
#53226=CARTESIAN_POINT('Ctrl Pts',(3.66755488921043,-3.70518002010068,59.6986337212642));
#53227=CARTESIAN_POINT('Ctrl Pts',(2.20265591301344,-4.43304697292067,59.6457134671823));
#53228=CARTESIAN_POINT('Ctrl Pts',(0.737756936816448,-5.16091392574066,
59.5927932131003));
#53229=CARTESIAN_POINT('Ctrl Pts',(-1.12360799336121,-5.09085679664823,
59.5398729590184));
#53230=CARTESIAN_POINT('Ctrl Pts',(-2.52964985740424,-4.25493479787751,
59.4869527049364));
#53231=CARTESIAN_POINT('Ctrl Pts',(-3.93569172144728,-3.41901279910679,
59.4340324508545));
#53232=CARTESIAN_POINT('Ctrl Pts',(-4.88641051935565,-1.8172259306578,59.3811121967725));
#53233=CARTESIAN_POINT('Ctrl Pts',(-4.94674280916461,-0.182576327141242,
59.3281919426905));
#53234=CARTESIAN_POINT('Ctrl Pts',(-4.94897409296954,-0.122121681733242,
59.3262347800127));
#53235=CARTESIAN_POINT('Ctrl Pts',(-4.94998754141356,-0.0616220879792628,
59.3242776173348));
#53236=CARTESIAN_POINT('Ctrl Pts',(-4.94980236868244,-0.00111614563719775,
59.3223204546569));
#53237=CARTESIAN_POINT('Ctrl Pts',(-4.95000952859661,-0.000636468299896517,
59.1776795453432));
#53238=CARTESIAN_POINT('Ctrl Pts',(-4.95007153361169,-0.0348429435249772,
59.1787861333591));
#53239=CARTESIAN_POINT('Ctrl Pts',(-4.94974762270576,-0.0690482134159459,
59.179892721375));
#53240=CARTESIAN_POINT('Ctrl Pts',(-4.94903421151526,-0.103245357661693,
59.1809993093909));
#53241=CARTESIAN_POINT('Ctrl Pts',(-4.9149168155888,-1.73865215436347,59.2339195634729));
#53242=CARTESIAN_POINT('Ctrl Pts',(-3.99000047173805,-3.35547535433661,
59.2868398175548));
#53243=CARTESIAN_POINT('Ctrl Pts',(-2.59754102487793,-4.21383196801951,
59.3397600716368));
#53244=CARTESIAN_POINT('Ctrl Pts',(-1.20508157801781,-5.07218858170242,
59.3926803257188));
#53245=CARTESIAN_POINT('Ctrl Pts',(0.654920971851715,-5.17207860909511,
59.4456005798008));
#53246=CARTESIAN_POINT('Ctrl Pts',(2.13130105065146,-4.46779084807236,59.4985208338827));
#53247=CARTESIAN_POINT('Ctrl Pts',(3.60768112945116,-3.76350308704963,59.5514410879647));
#53248=CARTESIAN_POINT('Ctrl Pts',(4.70043873718116,-2.25503753761151,59.6043613420466));
#53249=CARTESIAN_POINT('Ctrl Pts',(4.90951130318629,-0.632691073520989,
59.6572815961286));
#53250=CARTESIAN_POINT('Ctrl Pts',(5.11858386919144,0.98965539056958,59.7102018502105));
#53251=CARTESIAN_POINT('Ctrl Pts',(4.44397139347178,2.7258827693125,59.7631221042925));
#53252=CARTESIAN_POINT('Ctrl Pts',(3.19438684806975,3.78146689731725,59.8160423583745));
#53253=CARTESIAN_POINT('Ctrl Pts',(1.94480230266778,4.83705102532194,59.8689626124565));
#53254=CARTESIAN_POINT('Ctrl Pts',(0.120245687583507,5.21199190258845,59.9218828665384));
#53255=CARTESIAN_POINT('Ctrl Pts',(-1.44433802421679,4.7347108573205,59.9748031206203));
#53256=CARTESIAN_POINT('Ctrl Pts',(-3.00892173601718,4.25742981205253,60.0277233747023));
#53257=CARTESIAN_POINT('Ctrl Pts',(-4.31353254453361,2.92792684424999,60.0806436287843));
#53258=CARTESIAN_POINT('Ctrl Pts',(-4.7611606188609,1.35460281707783,60.1335638828663));
#53259=CARTESIAN_POINT('Ctrl Pts',(-4.88554531419032,0.917415247758462,
60.1482691036919));
#53260=CARTESIAN_POINT('Ctrl Pts',(-4.94375845579816,0.461401140068047,
60.1629743245176));
#53261=CARTESIAN_POINT('Ctrl Pts',(-4.93981933179839,0.00440230787564107,
60.1776795453432));
#53262=CARTESIAN_POINT('Origin',(0.,0.,16.));
#53263=CARTESIAN_POINT('',(-4.93439206002794,-0.00160550854955477,61.3223204546568));
#53264=CARTESIAN_POINT('',(-4.93468237204831,-0.00200522711461992,61.1776795453432));
#53265=CARTESIAN_POINT('',(-4.942,-6.05220448138622E-16,16.));
#53266=CARTESIAN_POINT('Ctrl Pts',(-4.93439206002794,-0.00160550854955477,
61.3223204546568));
#53267=CARTESIAN_POINT('Ctrl Pts',(-4.93169731118072,0.922902919227787,
61.2926539996516));
#53268=CARTESIAN_POINT('Ctrl Pts',(-4.68258000927622,1.84875941269167,61.2629875446464));
#53269=CARTESIAN_POINT('Ctrl Pts',(-4.19611032092476,2.62607248755302,61.2333210896412));
#53270=CARTESIAN_POINT('Ctrl Pts',(-3.3283254943857,4.01267582171134,61.1804008355592));
#53271=CARTESIAN_POINT('Ctrl Pts',(-1.7052638805986,4.92660054644685,61.1274805814773));
#53272=CARTESIAN_POINT('Ctrl Pts',(-0.0696632625637214,4.94962074962347,
61.0745603273953));
#53273=CARTESIAN_POINT('Ctrl Pts',(1.56593735547125,4.97264095280009,61.0216400733134));
#53274=CARTESIAN_POINT('Ctrl Pts',(3.21407697775393,4.10475663441781,60.9687198192314));
#53275=CARTESIAN_POINT('Ctrl Pts',(4.12054174158777,2.74312491350412,60.9157995651494));
#53276=CARTESIAN_POINT('Ctrl Pts',(5.02700650542156,1.3814931925905,60.8628793110674));
#53277=CARTESIAN_POINT('Ctrl Pts',(5.19179641080646,-0.473885930854428,
60.8099590569854));
#53278=CARTESIAN_POINT('Ctrl Pts',(4.53950108025175,-1.97396263329564,60.7570388029035));
#53279=CARTESIAN_POINT('Ctrl Pts',(3.88720574969703,-3.47403933573684,60.7041185488216));
#53280=CARTESIAN_POINT('Ctrl Pts',(2.41782518320256,-4.61881361717445,60.6511982947396));
#53281=CARTESIAN_POINT('Ctrl Pts',(0.803770369403307,-4.88441928262956,
60.5982780406577));
#53282=CARTESIAN_POINT('Ctrl Pts',(-0.810284444395997,-5.15002494808468,
60.5453577865757));
#53283=CARTESIAN_POINT('Ctrl Pts',(-2.56901350550008,-4.53646199755745,
60.4924375324937));
#53284=CARTESIAN_POINT('Ctrl Pts',(-3.66759553500858,-3.32450620797124,
60.4395172784117));
#53285=CARTESIAN_POINT('Ctrl Pts',(-4.47856622242051,-2.42984327576097,
60.4004516704934));
#53286=CARTESIAN_POINT('Ctrl Pts',(-4.92979916533343,-1.20909466877745,
60.3613860625752));
#53287=CARTESIAN_POINT('Ctrl Pts',(-4.9405850371911,0.0044815032353801,
60.3223204546569));
#53288=CARTESIAN_POINT('Ctrl Pts',(-4.93981933179839,0.00440230787564107,
60.1776795453432));
#53289=CARTESIAN_POINT('Ctrl Pts',(-4.9295825759933,-1.18321845466868,60.2158945785995));
#53290=CARTESIAN_POINT('Ctrl Pts',(-4.49960389811683,-2.3774895002097,60.2541096118559));
#53291=CARTESIAN_POINT('Ctrl Pts',(-3.72042358357856,-3.26527909823641,
60.2923246451122));
#53292=CARTESIAN_POINT('Ctrl Pts',(-2.64141313383085,-4.49469189983651,
60.3452448991941));
#53293=CARTESIAN_POINT('Ctrl Pts',(-0.892746894197383,-5.13637241649503,
60.3981651532761));
#53294=CARTESIAN_POINT('Ctrl Pts',(0.72535875721281,-4.89667784359578,60.451085407358));
#53295=CARTESIAN_POINT('Ctrl Pts',(2.34346440862305,-4.65698327069652,60.50400566144));
#53296=CARTESIAN_POINT('Ctrl Pts',(3.83100947181002,-3.53591360823934,60.556925915522));
#53297=CARTESIAN_POINT('Ctrl Pts',(4.50727060703144,-2.0464874555241,60.6098461696039));
#53298=CARTESIAN_POINT('Ctrl Pts',(5.18353174225287,-0.557061302808867,
60.6627664236859));
#53299=CARTESIAN_POINT('Ctrl Pts',(5.04850894950886,1.30072134016443,60.7156866777678));
#53300=CARTESIAN_POINT('Ctrl Pts',(4.16399072092151,2.67671076261644,60.7686069318498));
#53301=CARTESIAN_POINT('Ctrl Pts',(3.27947249233419,4.0527001850684,60.8215271859318));
#53302=CARTESIAN_POINT('Ctrl Pts',(1.64545882790348,4.94689638699909,60.8744474400138));
#53303=CARTESIAN_POINT('Ctrl Pts',(0.00969933627160482,4.95010152961563,
60.9273676940957));
#53304=CARTESIAN_POINT('Ctrl Pts',(-1.62606015536036,4.95330667223218,60.9802879481777));
#53305=CARTESIAN_POINT('Ctrl Pts',(-3.26356547419351,4.06552075553457,61.0332082022597));
#53306=CARTESIAN_POINT('Ctrl Pts',(-4.15346917720423,2.69300817389058,61.0861284563416));
#53307=CARTESIAN_POINT('Ctrl Pts',(-4.66664165108668,1.90153413622322,61.1166454860088));
#53308=CARTESIAN_POINT('Ctrl Pts',(-4.93120852346023,0.948870286286938,
61.147162515676));
#53309=CARTESIAN_POINT('Ctrl Pts',(-4.93468237204831,-0.00200522711461992,
61.1776795453432));
#53310=CARTESIAN_POINT('Origin',(0.,0.,16.));
#53311=CARTESIAN_POINT('',(-4.94646539259968,-0.00363051697945815,62.3223204546568));
#53312=CARTESIAN_POINT('',(-4.94715367607242,-0.003331217148393,62.1776795453432));
#53313=CARTESIAN_POINT('',(-4.942,-6.05220448138622E-16,16.));
#53314=CARTESIAN_POINT('Ctrl Pts',(-4.94646539259968,-0.00363051697945815,
62.3223204546568));
#53315=CARTESIAN_POINT('Ctrl Pts',(-4.93485651568824,1.40483737949782,62.2768421908101));
#53316=CARTESIAN_POINT('Ctrl Pts',(-4.3027525120455,2.82241015727549,62.2313639269634));
#53317=CARTESIAN_POINT('Ctrl Pts',(-3.23996042330606,3.74249315171913,62.1858856631166));
#53318=CARTESIAN_POINT('Ctrl Pts',(-2.00325473986379,4.81313705330919,62.1329654090346));
#53319=CARTESIAN_POINT('Ctrl Pts',(-0.183373993763468,5.2101527640882,62.0800451549526));
#53320=CARTESIAN_POINT('Ctrl Pts',(1.3868765910888,4.75185983130228,62.0271249008706));
#53321=CARTESIAN_POINT('Ctrl Pts',(2.95712717594107,4.29356689851636,61.9742046467886));
#53322=CARTESIAN_POINT('Ctrl Pts',(4.2777475995453,2.97996532216552,61.9212843927068));
#53323=CARTESIAN_POINT('Ctrl Pts',(4.74440178662215,1.4121792458292,61.8683641386248));
#53324=CARTESIAN_POINT('Ctrl Pts',(5.21105597369902,-0.155606830507172,
61.8154438845429));
#53325=CARTESIAN_POINT('Ctrl Pts',(4.82374392424848,-1.97757740682905,61.7625236304608));
#53326=CARTESIAN_POINT('Ctrl Pts',(3.75970554739938,-3.21997092100356,61.7096033763788));
#53327=CARTESIAN_POINT('Ctrl Pts',(2.69566717055032,-4.46236443517805,61.6566831222968));
#53328=CARTESIAN_POINT('Ctrl Pts',(0.954902466302742,-5.12518088720521,
61.603762868215));
#53329=CARTESIAN_POINT('Ctrl Pts',(-0.665988050504544,-4.90510534564135,
61.550842614133));
#53330=CARTESIAN_POINT('Ctrl Pts',(-2.28687856731188,-4.68502980407749,
61.4979223600511));
#53331=CARTESIAN_POINT('Ctrl Pts',(-3.78789489667891,-3.58206226892256,
61.4450021059691));
#53332=CARTESIAN_POINT('Ctrl Pts',(-4.4821490417169,-2.10093752955449,61.3920818518871));
#53333=CARTESIAN_POINT('Ctrl Pts',(-4.78721270168923,-1.45011342271034,
61.3688280528103));
#53334=CARTESIAN_POINT('Ctrl Pts',(-4.9365043160506,-0.726273596479458,
61.3455742537336));
#53335=CARTESIAN_POINT('Ctrl Pts',(-4.93439206002794,-0.00160550854955477,
61.3223204546568));
#53336=CARTESIAN_POINT('Ctrl Pts',(-4.93468237204831,-0.00200522711461992,
61.1776795453432));
#53337=CARTESIAN_POINT('Ctrl Pts',(-4.93723260089922,-0.700063909415997,
61.200082769758));
#53338=CARTESIAN_POINT('Ctrl Pts',(-4.79907061241107,-1.39715879423438,
61.2224859941727));
#53339=CARTESIAN_POINT('Ctrl Pts',(-4.51525583033475,-2.02880852158482,
61.2448892185875));
#53340=CARTESIAN_POINT('Ctrl Pts',(-3.84483669326632,-3.520873388826,61.2978094726695));
#53341=CARTESIAN_POINT('Ctrl Pts',(-2.36169633194117,-4.64776387671811,
61.3507297267514));
#53342=CARTESIAN_POINT('Ctrl Pts',(-0.744542427257826,-4.89379768734264,
61.4036499808334));
#53343=CARTESIAN_POINT('Ctrl Pts',(0.872611477425563,-5.13983149796717,
61.4565702349153));
#53344=CARTESIAN_POINT('Ctrl Pts',(2.62377892546721,-4.50500863132408,61.5094904889973));
#53345=CARTESIAN_POINT('Ctrl Pts',(3.7075989475901,-3.27983372664773,61.5624107430792));
#53346=CARTESIAN_POINT('Ctrl Pts',(4.79141896971299,-2.05465882197138,61.6153309971612));
#53347=CARTESIAN_POINT('Ctrl Pts',(5.20789156591715,-0.23913187926188,61.6682512512432));
#53348=CARTESIAN_POINT('Ctrl Pts',(4.76643251551905,1.33593424450079,61.7211715053252));
#53349=CARTESIAN_POINT('Ctrl Pts',(4.32497346512095,2.91100036826346,61.7740917594072));
#53350=CARTESIAN_POINT('Ctrl Pts',(3.02558276812051,4.24560567307922,61.8270120134891));
#53351=CARTESIAN_POINT('Ctrl Pts',(1.46288145266801,4.72901438843942,61.879932267571));
#53352=CARTESIAN_POINT('Ctrl Pts',(-0.099819862784441,5.2124231037996,61.932852521653));
#53353=CARTESIAN_POINT('Ctrl Pts',(-1.92583179668899,4.84463522970427,61.985772775735));
#53354=CARTESIAN_POINT('Ctrl Pts',(-3.17954339996051,3.79395611445292,62.038693029817));
#53355=CARTESIAN_POINT('Ctrl Pts',(-4.27710053403159,2.87414301265627,62.0850218683257));
#53356=CARTESIAN_POINT('Ctrl Pts',(-4.93604317278978,1.43095786114934,62.1313507068344));
#53357=CARTESIAN_POINT('Ctrl Pts',(-4.94715367607242,-0.003331217148393,
62.1776795453432));
#53358=CARTESIAN_POINT('Origin',(0.,0.,16.));
#53359=CARTESIAN_POINT('',(-4.94566965389892,0.00391030538274315,63.3223204546568));
#53360=CARTESIAN_POINT('',(-4.94490839420487,0.00412192395711707,63.1776795453432));
#53361=CARTESIAN_POINT('',(-4.942,-6.05220448138622E-16,16.));
#53362=CARTESIAN_POINT('Ctrl Pts',(-4.94566965389892,0.00391030538274314,
63.3223204546568));
#53363=CARTESIAN_POINT('Ctrl Pts',(-4.94791640205867,0.263233220344943,
63.3139506360505));
#53364=CARTESIAN_POINT('Ctrl Pts',(-4.92928016281063,0.522232554885722,
63.3055808174441));
#53365=CARTESIAN_POINT('Ctrl Pts',(-4.88863316854879,0.777730209403516,
63.2972109988377));
#53366=CARTESIAN_POINT('Ctrl Pts',(-4.63163246576532,2.39317750047789,63.2442907447558));
#53367=CARTESIAN_POINT('Ctrl Pts',(-3.49470467070217,3.86863762987662,63.1913704906738));
#53368=CARTESIAN_POINT('Ctrl Pts',(-1.99812530633611,4.52891750812856,63.1384502365919));
#53369=CARTESIAN_POINT('Ctrl Pts',(-0.501545941970182,5.18919738638045,
63.0855299825099));
#53370=CARTESIAN_POINT('Ctrl Pts',(1.35468499169859,5.0342970134857,63.0326097284279));
#53371=CARTESIAN_POINT('Ctrl Pts',(2.72112786976736,4.1351011658277,62.979689474346));
#53372=CARTESIAN_POINT('Ctrl Pts',(4.08757074783617,3.23590531816966,62.926769220264));
#53373=CARTESIAN_POINT('Ctrl Pts',(4.96422557030495,1.59241399574832,62.8738489661821));
#53374=CARTESIAN_POINT('Ctrl Pts',(4.94992170152689,-0.0432860717482803,
62.8209287121001));
#53375=CARTESIAN_POINT('Ctrl Pts',(4.93561783274882,-1.67898613924493,62.7680084580182));
#53376=CARTESIAN_POINT('Ctrl Pts',(4.03035527272386,-3.30689495181684,62.7150882039362));
#53377=CARTESIAN_POINT('Ctrl Pts',(2.64839599472191,-4.18205657427003,62.6621679498542));
#53378=CARTESIAN_POINT('Ctrl Pts',(1.26643671671996,-5.05721819672321,62.6092476957723));
#53379=CARTESIAN_POINT('Ctrl Pts',(-0.592219279258987,-5.17963262905766,
62.5563274416903));
#53380=CARTESIAN_POINT('Ctrl Pts',(-2.07702262276162,-4.49328115743837,
62.5034071876083));
#53381=CARTESIAN_POINT('Ctrl Pts',(-3.56182596626416,-3.80692968581911,
62.4504869335263));
#53382=CARTESIAN_POINT('Ctrl Pts',(-4.67277665729038,-2.31181231024634,
62.3975666794443));
#53383=CARTESIAN_POINT('Ctrl Pts',(-4.9014866924115,-0.692117576259364,
62.3446464253624));
#53384=CARTESIAN_POINT('Ctrl Pts',(-4.93364938470368,-0.464345570938786,
62.3372044351272));
#53385=CARTESIAN_POINT('Ctrl Pts',(-4.94836505061889,-0.234109947053592,
62.329762444892));
#53386=CARTESIAN_POINT('Ctrl Pts',(-4.94646539259968,-0.00363051697945815,
62.3223204546568));
#53387=CARTESIAN_POINT('Ctrl Pts',(-4.94715367607242,-0.003331217148393,
62.1776795453432));
#53388=CARTESIAN_POINT('Ctrl Pts',(-4.94873441814843,-0.207394078888273,
62.1842709609164));
#53389=CARTESIAN_POINT('Ctrl Pts',(-4.93720170764577,-0.4112768658406,62.1908623764896));
#53390=CARTESIAN_POINT('Ctrl Pts',(-4.91195301252751,-0.613446683379284,
62.1974537920628));
#53391=CARTESIAN_POINT('Ctrl Pts',(-4.70923974918446,-2.23660000955276,
62.2503740461448));
#53392=CARTESIAN_POINT('Ctrl Pts',(-3.6224019498598,-3.74933630549224,62.3032943002267));
#53393=CARTESIAN_POINT('Ctrl Pts',(-2.14879319047093,-4.45940433860991,
62.3562145543087));
#53394=CARTESIAN_POINT('Ctrl Pts',(-0.675184431082104,-5.16947237172755,
62.4091348083907));
#53395=CARTESIAN_POINT('Ctrl Pts',(1.18519528837092,-5.07687214202343,62.4620550624727));
#53396=CARTESIAN_POINT('Ctrl Pts',(2.58100779524721,-4.22397892886556,62.5149753165546));
#53397=CARTESIAN_POINT('Ctrl Pts',(3.97682030212355,-3.37108571570767,62.5678955706366));
#53398=CARTESIAN_POINT('Ctrl Pts',(4.90806559642314,-1.75789951909599,62.6208158247185));
#53399=CARTESIAN_POINT('Ctrl Pts',(4.94859160884553,-0.122638980307035,
62.6737360788005));
#53400=CARTESIAN_POINT('Ctrl Pts',(4.98911762126792,1.51262155848192,62.7266563328825));
#53401=CARTESIAN_POINT('Ctrl Pts',(4.13892435181312,3.16995643944814,62.7795765869645));
#53402=CARTESIAN_POINT('Ctrl Pts',(2.78707322532942,4.09094390908492,62.8324968410464));
#53403=CARTESIAN_POINT('Ctrl Pts',(1.43522209884579,5.01193137872164,62.8854170951284));
#53404=CARTESIAN_POINT('Ctrl Pts',(-0.418286884666658,5.19657143702902,
62.9383373492103));
#53405=CARTESIAN_POINT('Ctrl Pts',(-1.92525970626815,4.56036997337358,62.9912576032922));
#53406=CARTESIAN_POINT('Ctrl Pts',(-3.43223252786973,3.92416850971811,63.0441778573742));
#53407=CARTESIAN_POINT('Ctrl Pts',(-4.59266918756032,2.46712552409973,63.0970981114562));
#53408=CARTESIAN_POINT('Ctrl Pts',(-4.87553614686583,0.856006139716171,
63.1500183655382));
#53409=CARTESIAN_POINT('Ctrl Pts',(-4.9248205778018,0.57529784411246,63.1592387588066));
#53410=CARTESIAN_POINT('Ctrl Pts',(-4.94746485856309,0.289912292218248,
63.1684591520749));
#53411=CARTESIAN_POINT('Ctrl Pts',(-4.94490839420487,0.00412192395711708,
63.1776795453432));
#53412=CARTESIAN_POINT('Origin',(0.,0.,16.));
#53413=CARTESIAN_POINT('',(-4.93415080838549,0.00115309545102804,64.3223204546568));
#53414=CARTESIAN_POINT('',(-4.9340004404197,0.000727385793248169,64.1776795453432));
#53415=CARTESIAN_POINT('',(-4.942,-6.05220448138622E-16,16.));
#53416=CARTESIAN_POINT('Ctrl Pts',(-4.93415080838549,0.00115309545102804,
64.3223204546568));
#53417=CARTESIAN_POINT('Ctrl Pts',(-4.93572402472308,0.754827492624239,
64.2981388272089));
#53418=CARTESIAN_POINT('Ctrl Pts',(-4.77374496051519,1.5078605887699,64.273957199761));
#53419=CARTESIAN_POINT('Ctrl Pts',(-4.44472183637519,2.17900122361227,64.2497755723131));
#53420=CARTESIAN_POINT('Ctrl Pts',(-3.72467156821878,3.64775815476123,64.1968553182311));
#53421=CARTESIAN_POINT('Ctrl Pts',(-2.20459580691742,4.72430684596657,64.1439350641492));
#53422=CARTESIAN_POINT('Ctrl Pts',(-0.580104436501948,4.91600217432875,
64.0910148100672));
#53423=CARTESIAN_POINT('Ctrl Pts',(1.04438693391362,5.10769750269094,64.0380945559853));
#53424=CARTESIAN_POINT('Ctrl Pts',(2.77329391344336,4.41453946820987,63.9851743019033));
#53425=CARTESIAN_POINT('Ctrl Pts',(3.81544226317875,3.15372777385805,63.9322540478213));
#53426=CARTESIAN_POINT('Ctrl Pts',(4.85759061291414,1.89291607950622,63.8793337937393));
#53427=CARTESIAN_POINT('Ctrl Pts',(5.2129803328552,0.0644507252837223,63.8264135396574));
#53428=CARTESIAN_POINT('Ctrl Pts',(4.71897965939677,-1.49493461711666,63.7734932855754));
#53429=CARTESIAN_POINT('Ctrl Pts',(4.22497898593836,-3.05431995951699,63.7205730314935));
#53430=CARTESIAN_POINT('Ctrl Pts',(2.88158791908043,-4.34462529009514,63.6676527774115));
#53431=CARTESIAN_POINT('Ctrl Pts',(1.30356272822442,-4.77538718313377,63.6147325233296));
#53432=CARTESIAN_POINT('Ctrl Pts',(-0.274462462631595,-5.2061490761724,
63.5618122692476));
#53433=CARTESIAN_POINT('Ctrl Pts',(-2.08712177748574,-4.77736753167153,
63.5088920151656));
#53434=CARTESIAN_POINT('Ctrl Pts',(-3.30491462966089,-3.68525953304616,
63.4559717610837));
#53435=CARTESIAN_POINT('Ctrl Pts',(-4.33010248683659,-2.76587832883282,
63.4114213256081));
#53436=CARTESIAN_POINT('Ctrl Pts',(-4.93371077956384,-1.37640022865803,
63.3668708901324));
#53437=CARTESIAN_POINT('Ctrl Pts',(-4.94566965389892,0.00391030538274314,
63.3223204546568));
#53438=CARTESIAN_POINT('Ctrl Pts',(-4.94490839420487,0.00412192395711708,
63.1776795453432));
#53439=CARTESIAN_POINT('Ctrl Pts',(-4.9327920849133,-1.35037554176026,63.2213794061568));
#53440=CARTESIAN_POINT('Ctrl Pts',(-4.35459996207,-2.71396626059995,63.2650792669704));
#53441=CARTESIAN_POINT('Ctrl Pts',(-3.36357298066115,-3.6318006600574,63.308779127784));
#53442=CARTESIAN_POINT('Ctrl Pts',(-2.16344559623047,-4.74329229229879,
63.361699381866));
#53443=CARTESIAN_POINT('Ctrl Pts',(-0.35789356844863,-5.2010797736329,63.4146196359481));
#53444=CARTESIAN_POINT('Ctrl Pts',(1.22683491911902,-4.7956725609509,63.46753989003));
#53445=CARTESIAN_POINT('Ctrl Pts',(2.81156340668672,-4.39026534826889,63.520460144112));
#53446=CARTESIAN_POINT('Ctrl Pts',(4.17546835404021,-3.12166344157071,63.5733803981938));
#53447=CARTESIAN_POINT('Ctrl Pts',(4.69440602676098,-1.57039844833637,63.6263006522758));
#53448=CARTESIAN_POINT('Ctrl Pts',(5.21334369948175,-0.0191334551020692,
63.6792209063577));
#53449=CARTESIAN_POINT('Ctrl Pts',(4.88731409756984,1.81479462466838,63.7321411604398));
#53450=CARTESIAN_POINT('Ctrl Pts',(3.86551334621209,3.09215229264073,63.7850614145218));
#53451=CARTESIAN_POINT('Ctrl Pts',(2.84371259485431,4.36950996061312,63.8379816686038));
#53452=CARTESIAN_POINT('Ctrl Pts',(1.12614069405063,5.09029721678739,63.8909019226856));
#53453=CARTESIAN_POINT('Ctrl Pts',(-0.501215222432739,4.92467080437148,
63.9438221767676));
#53454=CARTESIAN_POINT('Ctrl Pts',(-2.12857113891606,4.75904439195557,63.9967424308495));
#53455=CARTESIAN_POINT('Ctrl Pts',(-3.66571107107909,3.70700431094953,64.0496626849316));
#53456=CARTESIAN_POINT('Ctrl Pts',(-4.40921630968873,2.24998016991306,64.1025829390136));
#53457=CARTESIAN_POINT('Ctrl Pts',(-4.76090724023141,1.56078236823718,64.1276151411235));
#53458=CARTESIAN_POINT('Ctrl Pts',(-4.93502599479208,0.780971213387874,
64.1526473432333));
#53459=CARTESIAN_POINT('Ctrl Pts',(-4.9340004404197,0.000727385793248169,
64.1776795453432));
#53460=CARTESIAN_POINT('Origin',(0.,0.,16.));
#53461=CARTESIAN_POINT('',(-4.94144181990917,-0.00451754960951789,65.3223204546568));
#53462=CARTESIAN_POINT('',(-4.94223974397651,-0.00450342756324047,65.1776795453432));
#53463=CARTESIAN_POINT('',(-4.942,-6.05220448138622E-16,16.));
#53464=CARTESIAN_POINT('Ctrl Pts',(-4.94144181990917,-0.00451754960951789,
65.3223204546568));
#53465=CARTESIAN_POINT('Ctrl Pts',(-4.93014544737618,1.2373328062097,65.2823270183674));
#53466=CARTESIAN_POINT('Ctrl Pts',(-4.45501720554112,2.48688539619672,65.2423335820779));
#53467=CARTESIAN_POINT('Ctrl Pts',(-3.60889481176119,3.38813765554137,65.2023401457884));
#53468=CARTESIAN_POINT('Ctrl Pts',(-2.48928579044125,4.58069580961582,65.1494198917065));
#53469=CARTESIAN_POINT('Ctrl Pts',(-0.720095544969354,5.16340781391902,
65.0964996376245));
#53470=CARTESIAN_POINT('Ctrl Pts',(0.889067448016765,4.86961575569687,65.0435793835425));
#53471=CARTESIAN_POINT('Ctrl Pts',(2.49823044100288,4.57582369747472,64.9906591294606));
#53472=CARTESIAN_POINT('Ctrl Pts',(3.94736618150317,3.40552757672724,64.9377388753786));
#53473=CARTESIAN_POINT('Ctrl Pts',(4.57332802245098,1.89427277188866,64.8848186212967));
#53474=CARTESIAN_POINT('Ctrl Pts',(5.19928986339881,0.383017967050043,64.8318983672147));
#53475=CARTESIAN_POINT('Ctrl Pts',(5.00207780479406,-1.46919552187978,64.7789781131327));
#53476=CARTESIAN_POINT('Ctrl Pts',(4.07193909661463,-2.81476651406745,64.7260578590508));
#53477=CARTESIAN_POINT('Ctrl Pts',(3.14180038843529,-4.16033750625501,64.6731376049688));
#53478=CARTESIAN_POINT('Ctrl Pts',(1.47873503068148,-4.99926600170063,64.6202173508868));
#53479=CARTESIAN_POINT('Ctrl Pts',(-0.156212869442396,-4.94764550818617,
64.5672970968049));
#53480=CARTESIAN_POINT('Ctrl Pts',(-1.79116076956636,-4.8960250146717,64.5143768427229));
#53481=CARTESIAN_POINT('Ctrl Pts',(-3.39799121206035,-3.95385553219706,
64.461456588641));
#53482=CARTESIAN_POINT('Ctrl Pts',(-4.24139404580168,-2.55228820541339,
64.408536334559));
#53483=CARTESIAN_POINT('Ctrl Pts',(-4.69940845940318,-1.7911595826268,64.379797707925));
#53484=CARTESIAN_POINT('Ctrl Pts',(-4.93228112128365,-0.89455035340317,
64.3510590812909));
#53485=CARTESIAN_POINT('Ctrl Pts',(-4.93415080838549,0.00115309545102804,
64.3223204546568));
#53486=CARTESIAN_POINT('Ctrl Pts',(-4.9340004404197,0.000727385793248169,
64.1776795453432));
#53487=CARTESIAN_POINT('Ctrl Pts',(-4.93285788358386,-0.868532151155221,
64.2055675973153));
#53488=CARTESIAN_POINT('Ctrl Pts',(-4.71432797343864,-1.73832871715993,
64.2334556492873));
#53489=CARTESIAN_POINT('Ctrl Pts',(-4.28176794905193,-2.48396104258879,
64.2613437012593));
#53490=CARTESIAN_POINT('Ctrl Pts',(-3.46094380474913,-3.89886991298749,
64.3142639553413));
#53491=CARTESIAN_POINT('Ctrl Pts',(-1.86942497108703,-4.86667945271791,
64.3671842094234));
#53492=CARTESIAN_POINT('Ctrl Pts',(-0.23551477313756,-4.94450523533559,
64.4201044635053));
#53493=CARTESIAN_POINT('Ctrl Pts',(1.39839542481181,-5.02233101795326,64.4730247175873));
#53494=CARTESIAN_POINT('Ctrl Pts',(3.0746969870487,-4.21017304345841,64.5259449716692));
#53495=CARTESIAN_POINT('Ctrl Pts',(4.0262887170445,-2.87968720482404,64.5788652257512));
#53496=CARTESIAN_POINT('Ctrl Pts',(4.97788044704027,-1.5492013661897,64.6317854798331));
#53497=CARTESIAN_POINT('Ctrl Pts',(5.20476234479506,0.299612336584008,64.6847057339151));
#53498=CARTESIAN_POINT('Ctrl Pts',(4.6031097887974,1.82070851673316,64.7376259879971));
#53499=CARTESIAN_POINT('Ctrl Pts',(4.00145723279969,3.34180469688243,64.790546242079));
#53500=CARTESIAN_POINT('Ctrl Pts',(2.57127022304931,4.535183354407,64.843466496161));
#53501=CARTESIAN_POINT('Ctrl Pts',(0.967024178023638,4.85473618951069,64.896386750243));
#53502=CARTESIAN_POINT('Ctrl Pts',(-0.637221867001943,5.17428902461436,
64.9493070043249));
#53503=CARTESIAN_POINT('Ctrl Pts',(-2.41552694730285,4.62001603729727,65.0022272584069));
#53504=CARTESIAN_POINT('Ctrl Pts',(-3.55411149861537,3.44556101180013,65.0551475124888));
#53505=CARTESIAN_POINT('Ctrl Pts',(-4.43287447301319,2.53911309775405,65.0959915234403));
#53506=CARTESIAN_POINT('Ctrl Pts',(-4.93056880366583,1.26323522569467,65.1368355343917));
#53507=CARTESIAN_POINT('Ctrl Pts',(-4.94223974397651,-0.00450342756324047,
65.1776795453432));
#53508=CARTESIAN_POINT('Origin',(0.,0.,16.));
#53509=CARTESIAN_POINT('',(-4.94946148968121,0.00162189178913478,66.3223204546568));
#53510=CARTESIAN_POINT('',(-4.94905436241693,0.00206350582114702,66.1776795453432));
#53511=CARTESIAN_POINT('',(-4.942,-6.05220448138622E-16,16.));
#53512=CARTESIAN_POINT('Ctrl Pts',(-4.94946148968121,0.00162189178913478,
66.3223204546568));
#53513=CARTESIAN_POINT('Ctrl Pts',(-4.94984329083445,0.0908281755408331,
66.3194354636078));
#53514=CARTESIAN_POINT('Ctrl Pts',(-4.94764036946139,0.180015220631608,
66.3165504725587));
#53515=CARTESIAN_POINT('Ctrl Pts',(-4.9427933546869,0.26905833589981,66.3136654815097));
#53516=CARTESIAN_POINT('Ctrl Pts',(-4.8538831123176,1.90240284342791,66.2607452274277));
#53517=CARTESIAN_POINT('Ctrl Pts',(-3.87529724194047,3.48731832979629,66.2078249733457));
#53518=CARTESIAN_POINT('Ctrl Pts',(-2.45485158348742,4.2985232625058,66.1549047192638));
#53519=CARTESIAN_POINT('Ctrl Pts',(-1.03440592503428,5.10972819521536,66.1019844651818));
#53520=CARTESIAN_POINT('Ctrl Pts',(0.827899521494876,5.14722257426599,66.0490642110999));
#53521=CARTESIAN_POINT('Ctrl Pts',(2.27984534133793,4.39384839916376,65.9961439570179));
#53522=CARTESIAN_POINT('Ctrl Pts',(3.7317911611809,3.64047422406158,65.9432237029359));
#53523=CARTESIAN_POINT('Ctrl Pts',(4.77337735433786,2.09623149480659,65.8903034488539));
#53524=CARTESIAN_POINT('Ctrl Pts',(4.9279581709879,0.467789269060101,65.8373831947719));
#53525=CARTESIAN_POINT('Ctrl Pts',(5.08253898763794,-1.16065295668643,65.78446294069));
#53526=CARTESIAN_POINT('Ctrl Pts',(4.35011442778111,-2.87329467892442,65.7315426866081));
#53527=CARTESIAN_POINT('Ctrl Pts',(3.06585315610755,-3.88640488889663,65.6786224325261));
#53528=CARTESIAN_POINT('Ctrl Pts',(1.78159188443402,-4.89951509886881,65.6257021784442));
#53529=CARTESIAN_POINT('Ctrl Pts',(-0.0545060990562027,-5.21309379657515,
65.5727819243622));
#53530=CARTESIAN_POINT('Ctrl Pts',(-1.60221431494639,-4.6836425807522,65.5198616702802));
#53531=CARTESIAN_POINT('Ctrl Pts',(-3.14992253083658,-4.15419136492924,
65.4669414161983));
#53532=CARTESIAN_POINT('Ctrl Pts',(-4.40924097912677,-2.78171023557699,
65.4140211621163));
#53533=CARTESIAN_POINT('Ctrl Pts',(-4.80388630468793,-1.19426751897802,
65.3611009080343));
#53534=CARTESIAN_POINT('Ctrl Pts',(-4.90028622386234,-0.806503266718003,
65.3481740902418));
#53535=CARTESIAN_POINT('Ctrl Pts',(-4.9450930727896,-0.405912747537303,
65.3352472724493));
#53536=CARTESIAN_POINT('Ctrl Pts',(-4.94144181990917,-0.00451754960951789,
65.3223204546568));
#53537=CARTESIAN_POINT('Ctrl Pts',(-4.94223974397651,-0.00450342756324047,
65.1776795453432));
#53538=CARTESIAN_POINT('Ctrl Pts',(-4.94569046072715,-0.379332437889885,
65.1897557884737));
#53539=CARTESIAN_POINT('Ctrl Pts',(-4.90665339169033,-0.753449924055778,
65.2018320316042));
#53540=CARTESIAN_POINT('Ctrl Pts',(-4.82241576997234,-1.11709684994147,
65.2139082747347));
#53541=CARTESIAN_POINT('Ctrl Pts',(-4.45327146769261,-2.71066262250856,
65.2668285288167));
#53542=CARTESIAN_POINT('Ctrl Pts',(-3.21611884080908,-4.10315710396555,
65.3197487828986));
#53543=CARTESIAN_POINT('Ctrl Pts',(-1.67709782604308,-4.65735355244893,
65.3726690369806));
#53544=CARTESIAN_POINT('Ctrl Pts',(-0.138076811276997,-5.21155000093235,
65.4255892910626));
#53545=CARTESIAN_POINT('Ctrl Pts',(1.70281259137165,-4.92744841644198,65.4785095451446));
#53546=CARTESIAN_POINT('Ctrl Pts',(3.00315127590115,-3.9350580230386,65.5314297992265));
#53547=CARTESIAN_POINT('Ctrl Pts',(4.30348996043062,-2.94266762963524,65.5843500533085));
#53548=CARTESIAN_POINT('Ctrl Pts',(5.06327792684106,-1.24198842731896,65.6372703073904));
#53549=CARTESIAN_POINT('Ctrl Pts',(4.93482459769029,0.388722806969066,65.6901905614724));
#53550=CARTESIAN_POINT('Ctrl Pts',(4.80637126853953,2.019434041257,65.7431108155543));
#53551=CARTESIAN_POINT('Ctrl Pts',(3.78967664382766,3.58017730751661,65.7960310696363));
#53552=CARTESIAN_POINT('Ctrl Pts',(2.34999571149359,4.35673265034576,65.8489513237183));
#53553=CARTESIAN_POINT('Ctrl Pts',(0.910314779159406,5.13328799317498,65.9018715778003));
#53554=CARTESIAN_POINT('Ctrl Pts',(-0.952352460797159,5.1256554125735,65.9547918318822));
#53555=CARTESIAN_POINT('Ctrl Pts',(-2.38562103141592,4.33732769399468,66.0077120859641));
#53556=CARTESIAN_POINT('Ctrl Pts',(-3.81888960203473,3.54899997541583,66.0606323400461));
#53557=CARTESIAN_POINT('Ctrl Pts',(-4.82275950331579,1.97997711885965,66.1135525941282));
#53558=CARTESIAN_POINT('Ctrl Pts',(-4.93784453663019,0.348267946699855,
66.1664728482101));
#53559=CARTESIAN_POINT('Ctrl Pts',(-4.94596822597675,0.233087909497783,
66.1702084139211));
#53560=CARTESIAN_POINT('Ctrl Pts',(-4.94966332434242,0.117595522185004,
66.1739439796322));
#53561=CARTESIAN_POINT('Ctrl Pts',(-4.94905436241693,0.00206350582114702,
66.1776795453432));
#53562=CARTESIAN_POINT('Origin',(0.,0.,16.));
#53563=CARTESIAN_POINT('',(-4.93665814957204,0.00348993981812262,67.3223204546568));
#53564=CARTESIAN_POINT('',(-4.93610990017314,0.00319438934087567,67.1776795453432));
#53565=CARTESIAN_POINT('',(-4.942,-6.05220448138622E-16,16.));
#53566=CARTESIAN_POINT('Ctrl Pts',(-4.93665814957204,0.00348993981812262,
67.3223204546568));
#53567=CARTESIAN_POINT('Ctrl Pts',(-4.94045351450443,0.585476451976408,
67.3036236547662));
#53568=CARTESIAN_POINT('Ctrl Pts',(-4.84535018635696,1.16626258658175,67.2849268548756));
#53569=CARTESIAN_POINT('Ctrl Pts',(-4.64586699339373,1.70865983008581,67.266230054985));
#53570=CARTESIAN_POINT('Ctrl Pts',(-4.08124089061357,3.24388511502926,67.213309800903));
#53571=CARTESIAN_POINT('Ctrl Pts',(-2.68038427233572,4.47156102489275,67.1603895468211));
#53572=CARTESIAN_POINT('Ctrl Pts',(-1.08435052194541,4.82988431339829,67.1074692927391));
#53573=CARTESIAN_POINT('Ctrl Pts',(0.511683228444911,5.18820760190384,67.0545490386571));
#53574=CARTESIAN_POINT('Ctrl Pts',(2.3028941109477,4.67717826905144,67.0016287845752));
#53575=CARTESIAN_POINT('Ctrl Pts',(3.4695966691053,3.53065114235145,66.9487085304932));
#53576=CARTESIAN_POINT('Ctrl Pts',(4.6362992272629,2.38412401565146,66.8957882764113));
#53577=CARTESIAN_POINT('Ctrl Pts',(5.17849346107531,0.602099095103884,66.8428680223293));
#53578=CARTESIAN_POINT('Ctrl Pts',(4.84806300838071,-0.999941799318743,
66.7899477682473));
#53579=CARTESIAN_POINT('Ctrl Pts',(4.51763255568609,-2.60198269374146,66.7370275141654));
#53580=CARTESIAN_POINT('Ctrl Pts',(3.31457741648437,-4.02403956203921,66.6841072600834));
#53581=CARTESIAN_POINT('Ctrl Pts',(1.78943399637315,-4.61535746263258,66.6311870060014));
#53582=CARTESIAN_POINT('Ctrl Pts',(0.264290576262007,-5.20667536322592,
66.5782667519194));
#53583=CARTESIAN_POINT('Ctrl Pts',(-1.5829411247586,-4.96725429611497,66.5253464978375));
#53584=CARTESIAN_POINT('Ctrl Pts',(-2.90693966808815,-4.00665699821556,
66.4724262437555));
#53585=CARTESIAN_POINT('Ctrl Pts',(-4.15875934507,-3.09842744975845,66.4223909807226));
#53586=CARTESIAN_POINT('Ctrl Pts',(-4.94283979803511,-1.54550938030458,
66.3723557176897));
#53587=CARTESIAN_POINT('Ctrl Pts',(-4.94946148968121,0.00162189178913478,
66.3223204546568));
#53588=CARTESIAN_POINT('Ctrl Pts',(-4.94905436241693,0.00206350582114702,
66.1776795453432));
#53589=CARTESIAN_POINT('Ctrl Pts',(-4.94103640614155,-1.51909999692026,
66.2268642337141));
#53590=CARTESIAN_POINT('Ctrl Pts',(-4.18686966888732,-3.04713356331113,
66.276048922085));
#53591=CARTESIAN_POINT('Ctrl Pts',(-2.97080189349508,-3.95953726339747,
66.3252336104559));
#53592=CARTESIAN_POINT('Ctrl Pts',(-1.66237405169773,-4.94123781357185,
66.3781538645379));
#53593=CARTESIAN_POINT('Ctrl Pts',(0.180781797244686,-5.21024342615729,
66.4310741186199));
#53594=CARTESIAN_POINT('Ctrl Pts',(1.71520938689206,-4.643453024393,66.4839943727019));
#53595=CARTESIAN_POINT('Ctrl Pts',(3.24963697653938,-4.07666262262872,66.5369146267838));
#53596=CARTESIAN_POINT('Ctrl Pts',(4.47533630689159,-2.6740762065147,66.5898348808657));
#53597=CARTESIAN_POINT('Ctrl Pts',(4.83140864464272,-1.0775387413447,66.6427551349477));
#53598=CARTESIAN_POINT('Ctrl Pts',(5.18748098239386,0.518998723825342,66.6956753890297));
#53599=CARTESIAN_POINT('Ctrl Pts',(4.67392632754393,2.30948723805131,66.7485956431117));
#53600=CARTESIAN_POINT('Ctrl Pts',(3.52575513351784,3.47457191163166,66.8015158971936));
#53601=CARTESIAN_POINT('Ctrl Pts',(2.37758393949173,4.63965658521205,66.8544361512756));
#53602=CARTESIAN_POINT('Ctrl Pts',(0.59479620628932,5.17933741814667,66.9073564053575));
#53603=CARTESIAN_POINT('Ctrl Pts',(-1.0067771713956,4.84664821890178,66.9602766594395));
#53604=CARTESIAN_POINT('Ctrl Pts',(-2.60835054908043,4.5139590196569,67.0131969135215));
#53605=CARTESIAN_POINT('Ctrl Pts',(-4.02870957124789,3.3088997882326,67.0661171676034));
#53606=CARTESIAN_POINT('Ctrl Pts',(-4.61787625663849,1.78292403343541,67.1190374216854));
#53607=CARTESIAN_POINT('Ctrl Pts',(-4.83549920786993,1.2192680163841,67.138584796238));
#53608=CARTESIAN_POINT('Ctrl Pts',(-4.93971654397597,0.611827024271365,
67.1581321707906));
#53609=CARTESIAN_POINT('Ctrl Pts',(-4.93610990017314,0.00319438934087567,
67.1776795453432));
#53610=CARTESIAN_POINT('Origin',(0.,0.,16.));
#53611=CARTESIAN_POINT('',(-4.93685333923596,-0.0035819126635156,68.3223204546569));
#53612=CARTESIAN_POINT('',(-4.9374673003319,-0.00383358773467055,68.1776795453432));
#53613=CARTESIAN_POINT('',(-4.942,-6.05220448138622E-16,16.));
#53614=CARTESIAN_POINT('Ctrl Pts',(-4.93685333923596,-0.0035819126635156,
68.3223204546569));
#53615=CARTESIAN_POINT('Ctrl Pts',(-4.92964532583484,1.0704814894781,68.2878118459247));
#53616=CARTESIAN_POINT('Ctrl Pts',(-4.585217373837,2.14875374624117,68.2533032371925));
#53617=CARTESIAN_POINT('Ctrl Pts',(-3.93928885933925,2.99759934246388,68.2187946284603));
#53618=CARTESIAN_POINT('Ctrl Pts',(-2.94873310059188,4.29933610551658,68.1658743743783));
#53619=CARTESIAN_POINT('Ctrl Pts',(-1.24912700565894,5.06152146794402,68.1129541202964));
#53620=CARTESIAN_POINT('Ctrl Pts',(0.3817637188463,4.93536776727194,68.0600338662144));
#53621=CARTESIAN_POINT('Ctrl Pts',(2.01265444335154,4.80921406659986,68.0071136121325));
#53622=CARTESIAN_POINT('Ctrl Pts',(3.57482979742896,3.79472130282827,67.9541933580505));
#53623=CARTESIAN_POINT('Ctrl Pts',(4.35341448041909,2.35613685870146,67.9012731039685));
#53624=CARTESIAN_POINT('Ctrl Pts',(5.13199916340922,0.91755241457464,67.8483528498866));
#53625=CARTESIAN_POINT('Ctrl Pts',(5.12699317531198,-0.945123709907305,
67.7954325958046));
#53626=CARTESIAN_POINT('Ctrl Pts',(4.34068733273566,-2.37950247209,67.7425123417227));
#53627=CARTESIAN_POINT('Ctrl Pts',(3.55438149015938,-3.81388123427261,67.6895920876407));
#53628=CARTESIAN_POINT('Ctrl Pts',(1.98677579310383,-4.81996263415611,67.6366718335588));
#53629=CARTESIAN_POINT('Ctrl Pts',(0.355230550111662,-4.93734845757534,
67.5837515794768));
#53630=CARTESIAN_POINT('Ctrl Pts',(-1.27631469288069,-5.05473428099459,
67.5308313253949));
#53631=CARTESIAN_POINT('Ctrl Pts',(-2.9717994818098,-4.28342452794957,67.4779110713129));
#53632=CARTESIAN_POINT('Ctrl Pts',(-3.95534408263313,-2.97638232141527,
67.4249908172309));
#53633=CARTESIAN_POINT('Ctrl Pts',(-4.59140099837083,-2.13111995717548,
67.3907673630395));
#53634=CARTESIAN_POINT('Ctrl Pts',(-4.92971094477425,-1.06180405997696,
67.3565439088482));
#53635=CARTESIAN_POINT('Ctrl Pts',(-4.93665814957204,0.00348993981812262,
67.3223204546568));
#53636=CARTESIAN_POINT('Ctrl Pts',(-4.93610990017314,0.00319438934087567,
67.1776795453432));
#53637=CARTESIAN_POINT('Ctrl Pts',(-4.929952342348,-1.03591311578948,67.2110524248726));
#53638=CARTESIAN_POINT('Ctrl Pts',(-4.60950819503561,-2.07849403525122,
67.2444253044019));
#53639=CARTESIAN_POINT('Ctrl Pts',(-4.00255393693903,-2.91258668755472,
67.2777981839313));
#53640=CARTESIAN_POINT('Ctrl Pts',(-3.0400905832352,-4.23522937557753,67.3307184380133));
#53641=CARTESIAN_POINT('Ctrl Pts',(-1.35718952721374,-5.03362247345304,
67.3836386920952));
#53642=CARTESIAN_POINT('Ctrl Pts',(0.276028005448868,-4.94240910597606,
67.4365589461772));
#53643=CARTESIAN_POINT('Ctrl Pts',(1.90924553811157,-4.85119573849907,67.4894792002592));
#53644=CARTESIAN_POINT('Ctrl Pts',(3.49277954741543,-3.87037590566948,67.5423994543411));
#53645=CARTESIAN_POINT('Ctrl Pts',(4.30198068586489,-2.4487877427561,67.5953197084231));
#53646=CARTESIAN_POINT('Ctrl Pts',(5.11118182431431,-1.0271995798428,67.6482399625051));
#53647=CARTESIAN_POINT('Ctrl Pts',(5.14605009190941,0.835156913154248,67.7011602165871));
#53648=CARTESIAN_POINT('Ctrl Pts',(4.39062923686613,2.28603896182972,67.754080470669));
#53649=CARTESIAN_POINT('Ctrl Pts',(3.63520838182284,3.73692101050519,67.8070007247509));
#53650=CARTESIAN_POINT('Ctrl Pts',(2.08949840414118,4.77632861485907,67.8599209788329));
#53651=CARTESIAN_POINT('Ctrl Pts',(0.460839796771268,4.92861298057972,67.9128412329148));
#53652=CARTESIAN_POINT('Ctrl Pts',(-1.16781881059865,5.08089734630037,67.9657614869968));
#53653=CARTESIAN_POINT('Ctrl Pts',(-2.87942604765681,4.34605847338777,68.0186817410788));
#53654=CARTESIAN_POINT('Ctrl Pts',(-3.89072430186352,3.06036985305955,68.0716019951608));
#53655=CARTESIAN_POINT('Ctrl Pts',(-4.56643308401115,2.20132447426127,68.1069611785549));
#53656=CARTESIAN_POINT('Ctrl Pts',(-4.92949771464715,1.09635914283018,68.142320361949));
#53657=CARTESIAN_POINT('Ctrl Pts',(-4.9374673003319,-0.00383358773467055,
68.1776795453432));
#53658=CARTESIAN_POINT('Origin',(0.,0.,16.));
#53659=CARTESIAN_POINT('',(-4.94957828458471,-0.00146882823891858,69.3223204546568));
#53660=CARTESIAN_POINT('',(-4.94986277816997,-0.00100007488610477,69.1776795453432));
#53661=CARTESIAN_POINT('',(-4.942,-6.05220448138622E-16,16.));
#53662=CARTESIAN_POINT('Ctrl Pts',(-4.94957828458471,-0.00146882823891858,
69.3223204546568));
#53663=CARTESIAN_POINT('Ctrl Pts',(-4.94347825971363,1.5543817607618,69.2720000370831));
#53664=CARTESIAN_POINT('Ctrl Pts',(-4.14920711766337,3.115598423098,69.2216796195094));
#53665=CARTESIAN_POINT('Ctrl Pts',(-2.8853618522021,4.0222239516356,69.1713592019357));
#53666=CARTESIAN_POINT('Ctrl Pts',(-1.55621921401708,4.97569086707049,69.1184389478537));
#53667=CARTESIAN_POINT('Ctrl Pts',(0.292272693635941,5.20517958568956,69.0655186937718));
#53668=CARTESIAN_POINT('Ctrl Pts',(1.81421574235462,4.60567256494064,69.0125984396898));
#53669=CARTESIAN_POINT('Ctrl Pts',(3.3361587910733,4.00616554419172,68.9596781856078));
#53670=CARTESIAN_POINT('Ctrl Pts',(4.53155298085772,2.57766278407475,68.9067579315258));
#53671=CARTESIAN_POINT('Ctrl Pts',(4.85336767356702,0.973868964711821,68.8538376774439));
#53672=CARTESIAN_POINT('Ctrl Pts',(5.17518236627633,-0.629924854651203,
68.8009174233619));
#53673=CARTESIAN_POINT('Ctrl Pts',(4.62341756191056,-2.40900973326008,68.74799716928));
#53674=CARTESIAN_POINT('Ctrl Pts',(3.45056926188509,-3.5492492592361,68.695076915198));
#53675=CARTESIAN_POINT('Ctrl Pts',(2.27772096185968,-4.68948878521204,68.6421566611161));
#53676=CARTESIAN_POINT('Ctrl Pts',(0.483789166174606,-5.19088295855499,
68.5892364070341));
#53677=CARTESIAN_POINT('Ctrl Pts',(-1.11029553728448,-4.82398614790096,
68.5363161529521));
#53678=CARTESIAN_POINT('Ctrl Pts',(-2.70438024074366,-4.45708933724691,
68.4833958988701));
#53679=CARTESIAN_POINT('Ctrl Pts',(-4.09861785197692,-3.22190154259576,
68.4304756447882));
#53680=CARTESIAN_POINT('Ctrl Pts',(-4.65498394631264,-1.6836635634312,68.3775553907063));
#53681=CARTESIAN_POINT('Ctrl Pts',(-4.84855095371391,-1.14849054456963,
68.3591437453565));
#53682=CARTESIAN_POINT('Ctrl Pts',(-4.94069908646524,-0.576635280213381,
68.3407321000067));
#53683=CARTESIAN_POINT('Ctrl Pts',(-4.93685333923596,-0.0035819126635156,
68.3223204546569));
#53684=CARTESIAN_POINT('Ctrl Pts',(-4.9374673003319,-0.00383358773467055,
68.1776795453432));
#53685=CARTESIAN_POINT('Ctrl Pts',(-4.94142537979325,-0.550242199503817,
68.195240616031));
#53686=CARTESIAN_POINT('Ctrl Pts',(-4.85779595713247,-1.09547360479138,
68.2128016867188));
#53687=CARTESIAN_POINT('Ctrl Pts',(-4.68137867571166,-1.60881724419501,
68.2303627574066));
#53688=CARTESIAN_POINT('Ctrl Pts',(-4.14974552399779,-3.15577735337756,
68.2832830114886));
#53689=CARTESIAN_POINT('Ctrl Pts',(-2.77548994921469,-4.41315920399872,
68.3362032655706));
#53690=CARTESIAN_POINT('Ctrl Pts',(-1.18749229097476,-4.8055656575998,68.3891235196525));
#53691=CARTESIAN_POINT('Ctrl Pts',(0.400505367265077,-5.19797211120086,
68.4420437737345));
#53692=CARTESIAN_POINT('Ctrl Pts',(2.20224510896182,-4.72540316778197,68.4949640278164));
#53693=CARTESIAN_POINT('Ctrl Pts',(3.39322331088645,-3.60411359325479,68.5478842818984));
#53694=CARTESIAN_POINT('Ctrl Pts',(4.58420151281108,-2.48282401872761,68.6008045359804));
#53695=CARTESIAN_POINT('Ctrl Pts',(5.16441817496363,-0.71281381309235,68.6537247900624));
#53696=CARTESIAN_POINT('Ctrl Pts',(4.8683572912689,0.895933320719813,68.7066450441443));
#53697=CARTESIAN_POINT('Ctrl Pts',(4.57229640757415,2.50468045453207,68.7595652982263));
#53698=CARTESIAN_POINT('Ctrl Pts',(3.39995797803181,3.95216451652107,68.8124855523082));
#53699=CARTESIAN_POINT('Ctrl Pts',(1.88782197277238,4.57599469293234,68.8654058063902));
#53700=CARTESIAN_POINT('Ctrl Pts',(0.375685967513026,5.19982486934357,68.9183260604721));
#53701=CARTESIAN_POINT('Ctrl Pts',(-1.47624761346349,5.00000116017722,68.9712463145541));
#53702=CARTESIAN_POINT('Ctrl Pts',(-2.82050567947833,4.06796594659513,69.0241665686361));
#53703=CARTESIAN_POINT('Ctrl Pts',(-4.1203297308193,3.16673885490861,69.0753375608718));
#53704=CARTESIAN_POINT('Ctrl Pts',(-4.94548567424374,1.58090626393571,69.1265085531075));
#53705=CARTESIAN_POINT('Ctrl Pts',(-4.94986277816997,-0.00100007488610477,
69.1776795453432));
#53706=CARTESIAN_POINT('Origin',(0.,0.,16.));
#53707=CARTESIAN_POINT('',(-4.94117660785543,0.00451214175946527,70.3223204546568));
#53708=CARTESIAN_POINT('',(-4.94039592783718,0.00446617472429873,70.1776795453432));
#53709=CARTESIAN_POINT('',(-4.942,-6.05220448138622E-16,16.));
#53710=CARTESIAN_POINT('Ctrl Pts',(-4.94117660785543,0.00451214175946527,
70.3223204546568));
#53711=CARTESIAN_POINT('Ctrl Pts',(-4.94488654917412,0.414817947726635,
70.3091084823236));
#53712=CARTESIAN_POINT('Ctrl Pts',(-4.8980529188199,0.824288512579107,70.2958965099902));
#53713=CARTESIAN_POINT('Ctrl Pts',(-4.79739770972192,1.22007120694207,70.2826845376569));
#53714=CARTESIAN_POINT('Ctrl Pts',(-4.39422556359881,2.80536976937794,70.229764283575));
#53715=CARTESIAN_POINT('Ctrl Pts',(-3.12754820616573,4.17106222260404,70.176844029493));
#53716=CARTESIAN_POINT('Ctrl Pts',(-1.57701654176587,4.69218684221452,70.123923775411));
#53717=CARTESIAN_POINT('Ctrl Pts',(-0.0264848773660925,5.21331146182497,
70.071003521329));
#53718=CARTESIAN_POINT('Ctrl Pts',(1.80790109400033,4.88986824781988,70.0180832672471));
#53719=CARTESIAN_POINT('Ctrl Pts',(3.0866983358117,3.86986975477877,69.9651630131651));
#53720=CARTESIAN_POINT('Ctrl Pts',(4.36549557762306,2.84987126173766,69.9122427590831));
#53721=CARTESIAN_POINT('Ctrl Pts',(5.08870408987935,1.13331748966031,69.8593225050012));
#53722=CARTESIAN_POINT('Ctrl Pts',(4.9253726120261,-0.494270338941504,69.8064022509192));
#53723=CARTESIAN_POINT('Ctrl Pts',(4.76204113417285,-2.12185816754332,69.7534819968373));
#53724=CARTESIAN_POINT('Ctrl Pts',(3.71216966621028,-3.66048005266973,69.7005617427553));
#53725=CARTESIAN_POINT('Ctrl Pts',(2.25619542624873,-4.40603912077827,69.6476414886733));
#53726=CARTESIAN_POINT('Ctrl Pts',(0.80022118628726,-5.15159818888676,69.5947212345913));
#53727=CARTESIAN_POINT('Ctrl Pts',(-1.06185582567303,-5.10409443997744,
69.5418009805094));
#53728=CARTESIAN_POINT('Ctrl Pts',(-2.47792073001783,-4.28526631506165,
69.4888807264275));
#53729=CARTESIAN_POINT('Ctrl Pts',(-3.89398563436272,-3.46643819014582,
69.4359604723455));
#53730=CARTESIAN_POINT('Ctrl Pts',(-4.864038431092,-1.87628568922347,69.3830402182635));
#53731=CARTESIAN_POINT('Ctrl Pts',(-4.94416814509815,-0.242486882636884,
69.3301199641816));
#53732=CARTESIAN_POINT('Ctrl Pts',(-4.94810471266539,-0.162222532848887,
69.3275201276733));
#53733=CARTESIAN_POINT('Ctrl Pts',(-4.94989344626512,-0.081852842476203,
69.3249202911651));
#53734=CARTESIAN_POINT('Ctrl Pts',(-4.94957828458471,-0.00146882823891858,
69.3223204546568));
#53735=CARTESIAN_POINT('Ctrl Pts',(-4.94986277816997,-0.00100007488610477,
69.1776795453432));
#53736=CARTESIAN_POINT('Ctrl Pts',(-4.95001240788323,-0.0550769704471047,
69.1794288071895));
#53737=CARTESIAN_POINT('Ctrl Pts',(-4.94920288408253,-0.10914927783116,
69.1811780690357));
#53738=CARTESIAN_POINT('Ctrl Pts',(-4.94742038040276,-0.163189491703912,
69.182927330882));
#53739=CARTESIAN_POINT('Ctrl Pts',(-4.89349446425897,-1.79806299842275,
69.2358475849639));
#53740=CARTESIAN_POINT('Ctrl Pts',(-3.94906008091826,-3.40356329386249,
69.2887678390458));
#53741=CARTESIAN_POINT('Ctrl Pts',(-2.54630482825922,-4.24498892250744,
69.3416880931278));
#53742=CARTESIAN_POINT('Ctrl Pts',(-1.14354957560017,-5.0864145511524,69.3946083472098));
#53743=CARTESIAN_POINT('Ctrl Pts',(0.717526546377131,-5.16376551300254,
69.4475286012918));
#53744=CARTESIAN_POINT('Ctrl Pts',(2.18526668060081,-4.44164482655728,69.5004488553738));
#53745=CARTESIAN_POINT('Ctrl Pts',(3.65300681482441,-3.71952414011206,69.5533691094558));
#53746=CARTESIAN_POINT('Ctrl Pts',(4.72741096129446,-2.19793180537131,69.6062893635377));
#53747=CARTESIAN_POINT('Ctrl Pts',(4.91681537353513,-0.573171713534203,
69.6592096176196));
#53748=CARTESIAN_POINT('Ctrl Pts',(5.1062197857758,1.05158837830299,69.7121298717016));
#53749=CARTESIAN_POINT('Ctrl Pts',(4.41062446378718,2.77951622723674,69.7650501257836));
#53750=CARTESIAN_POINT('Ctrl Pts',(3.14834445052908,3.81988565947332,69.8179703798655));
#53751=CARTESIAN_POINT('Ctrl Pts',(1.88606443727098,4.8602550917099,69.8708906339475));
#53752=CARTESIAN_POINT('Ctrl Pts',(0.0570997327434936,5.21306610724925,
69.9238108880295));
#53753=CARTESIAN_POINT('Ctrl Pts',(-1.50158748103454,4.71686699700421,69.9767311421114));
#53754=CARTESIAN_POINT('Ctrl Pts',(-3.06027469481266,4.22066788675913,70.0296513961934));
#53755=CARTESIAN_POINT('Ctrl Pts',(-4.34868441784121,2.87545865072958,70.0825716502754));
#53756=CARTESIAN_POINT('Ctrl Pts',(-4.77722068336862,1.29682758029823,70.1354919043573));
#53757=CARTESIAN_POINT('Ctrl Pts',(-4.8910960129131,0.877336517731382,70.1495544513526));
#53758=CARTESIAN_POINT('Ctrl Pts',(-4.9442531721895,0.441362859310636,70.1636169983479));
#53759=CARTESIAN_POINT('Ctrl Pts',(-4.94039592783718,0.00446617472429873,
70.1776795453432));
#53760=CARTESIAN_POINT('Origin',(0.,0.,16.));
#53761=CARTESIAN_POINT('',(-4.93421645959303,-0.00129368103133631,71.3223204546568));
#53762=CARTESIAN_POINT('',(-4.93445704478049,-0.00170468936910681,71.1776795453431));
#53763=CARTESIAN_POINT('',(-4.942,-6.05220448138622E-16,16.));
#53764=CARTESIAN_POINT('Ctrl Pts',(-4.93421645959303,-0.00129368103133631,
71.3223204546568));
#53765=CARTESIAN_POINT('Ctrl Pts',(-4.93209641645617,0.903267203006942,
71.293296673482));
#53766=CARTESIAN_POINT('Ctrl Pts',(-4.69429817649842,1.80886543486343,71.2642728923071));
#53767=CARTESIAN_POINT('Ctrl Pts',(-4.22761420074216,2.5750488742813,71.2352491111322));
#53768=CARTESIAN_POINT('Ctrl Pts',(-3.37669011114097,3.97206265560444,71.1823288570503));
#53769=CARTESIAN_POINT('Ctrl Pts',(-1.76481870913523,4.90558179736215,71.1294086029683));
#53770=CARTESIAN_POINT('Ctrl Pts',(-0.129616965909283,4.94841368292938,
71.0764883488863));
#53771=CARTESIAN_POINT('Ctrl Pts',(1.50558477731675,4.9912455684966,71.0235680948044));
#53772=CARTESIAN_POINT('Ctrl Pts',(3.164116861763,4.14339019787323,70.9706478407224));
#53773=CARTESIAN_POINT('Ctrl Pts',(4.08700967532571,2.79283913769631,70.9177275866405));
#53774=CARTESIAN_POINT('Ctrl Pts',(5.00990248888837,1.44228807751946,70.8648073325585));
#53775=CARTESIAN_POINT('Ctrl Pts',(5.19715603156758,-0.410958672210887,
70.8118870784765));
#53776=CARTESIAN_POINT('Ctrl Pts',(4.56308022236637,-1.91882709473861,70.7589668243946));
#53777=CARTESIAN_POINT('Ctrl Pts',(3.92900441316517,-3.42669551726634,70.7060465703126));
#53778=CARTESIAN_POINT('Ctrl Pts',(2.47359925208355,-4.58918561259145,70.6531263162307));
#53779=CARTESIAN_POINT('Ctrl Pts',(0.86288036879719,-4.87432415873202,70.6002060621487));
#53780=CARTESIAN_POINT('Ctrl Pts',(-0.747838514489167,-5.1594627048726,
70.5472858080667));
#53781=CARTESIAN_POINT('Ctrl Pts',(-2.51387111998026,-4.56724970182864,
70.4943655539847));
#53782=CARTESIAN_POINT('Ctrl Pts',(-3.62705395531922,-3.36869086448392,
70.4414452999028));
#53783=CARTESIAN_POINT('Ctrl Pts',(-4.46232163175454,-2.46936200011537,
70.4017370181541));
#53784=CARTESIAN_POINT('Ctrl Pts',(-4.93002646377116,-1.22865260726002,
70.3620287364055));
#53785=CARTESIAN_POINT('Ctrl Pts',(-4.94117660785543,0.00451214175946527,
70.3223204546568));
#53786=CARTESIAN_POINT('Ctrl Pts',(-4.94039592783718,0.00446617472429873,
70.1776795453432));
#53787=CARTESIAN_POINT('Ctrl Pts',(-4.92973756905946,-1.20276914349332,
70.2165372524299));
#53788=CARTESIAN_POINT('Ctrl Pts',(-4.48375687255021,-2.4170520476298,70.2553949595166));
#53789=CARTESIAN_POINT('Ctrl Pts',(-3.68059559417778,-3.31010805001079,
70.2942526666032));
#53790=CARTESIAN_POINT('Ctrl Pts',(-2.58677143143322,-4.52635970505561,
70.3471729206852));
#53791=CARTESIAN_POINT('Ctrl Pts',(-0.83046029791784,-5.14681011031225,
70.4000931747671));
#53792=CARTESIAN_POINT('Ctrl Pts',(0.784623008060776,-4.88753168438311,
70.453013428849));
#53793=CARTESIAN_POINT('Ctrl Pts',(2.3997063140393,-4.62825325845398,70.505933682931));
#53794=CARTESIAN_POINT('Ctrl Pts',(3.87356179248119,-3.48924600133894,70.558853937013));
#53795=CARTESIAN_POINT('Ctrl Pts',(4.53173066670028,-1.99173702960891,70.611774191095));
#53796=CARTESIAN_POINT('Ctrl Pts',(5.18989954091941,-0.494228057878804,
70.664694445177));
#53797=CARTESIAN_POINT('Ctrl Pts',(5.0323818109159,1.36178262846646,70.7176146992589));
#53798=CARTESIAN_POINT('Ctrl Pts',(4.13125999566019,2.72695619306305,70.7705349533408));
#53799=CARTESIAN_POINT('Ctrl Pts',(3.23013818040442,4.09212975765972,70.8234552074228));
#53800=CARTESIAN_POINT('Ctrl Pts',(1.58541227989642,4.96646620050757,70.8763754615048));
#53801=CARTESIAN_POINT('Ctrl Pts',(-0.0502660143879759,4.94985581188227,
70.9292957155868));
#53802=CARTESIAN_POINT('Ctrl Pts',(-1.68594430867228,4.93324542325696,70.9822159696687));
#53803=CARTESIAN_POINT('Ctrl Pts',(-3.3125749967329,4.02568820315859,71.0351362237507));
#53804=CARTESIAN_POINT('Ctrl Pts',(-4.18578703267271,2.64249619635225,71.0880564778327));
#53805=CARTESIAN_POINT('Ctrl Pts',(-4.67872962214464,1.86166150614078,71.1179308336695));
#53806=CARTESIAN_POINT('Ctrl Pts',(-4.93157361279594,0.929252063276933,
71.1478051895063));
#53807=CARTESIAN_POINT('Ctrl Pts',(-4.93445704478049,-0.00170468936910681,
71.1776795453431));
#53808=CARTESIAN_POINT('Origin',(0.,0.,16.));
#53809=CARTESIAN_POINT('',(-4.9459185577707,-0.00382965742011687,72.3223204546568));
#53810=CARTESIAN_POINT('',(-4.9466376895248,-0.00356105100536129,72.1776795453432));
#53811=CARTESIAN_POINT('',(-4.942,-6.05220448138622E-16,16.));
#53812=CARTESIAN_POINT('Ctrl Pts',(-4.9459185577707,-0.00382965742011687,
72.3223204546568));
#53813=CARTESIAN_POINT('Ctrl Pts',(-4.93404671791329,1.38513423103216,72.2774848646404));
#53814=CARTESIAN_POINT('Ctrl Pts',(-4.32176677967432,2.78326338156107,72.232649274624));
#53815=CARTESIAN_POINT('Ctrl Pts',(-3.28505857961465,3.70297024883463,72.1878136846076));
#53816=CARTESIAN_POINT('Ctrl Pts',(-2.06141322698447,4.78851682197505,72.1348934305256));
#53817=CARTESIAN_POINT('Ctrl Pts',(-0.246475391513582,5.20754910952386,
72.0819731764437));
#53818=CARTESIAN_POINT('Ctrl Pts',(1.32921165428745,4.76831153694478,72.0290529223617));
#53819=CARTESIAN_POINT('Ctrl Pts',(2.90489870008848,4.32907396436569,71.9761326682797));
#53820=CARTESIAN_POINT('Ctrl Pts',(4.24133495621976,3.03156653165866,71.9232124141978));
#53821=CARTESIAN_POINT('Ctrl Pts',(4.72694678088706,1.46954845647079,71.8702921601158));
#53822=CARTESIAN_POINT('Ctrl Pts',(5.21255860555439,-0.09246961871717,71.8173719060338));
#53823=CARTESIAN_POINT('Ctrl Pts',(4.84734599875778,-1.91899833638585,71.7644516519519));
#53824=CARTESIAN_POINT('Ctrl Pts',(3.79843582714949,-3.17419025930731,71.7115313978699));
#53825=CARTESIAN_POINT('Ctrl Pts',(2.74952565554119,-4.42938218222877,71.658611143788));
#53826=CARTESIAN_POINT('Ctrl Pts',(1.0169179191211,-5.1132373104028,71.605690889706));
#53827=CARTESIAN_POINT('Ctrl Pts',(-0.60651962032857,-4.91281309286346,
71.552770635624));
#53828=CARTESIAN_POINT('Ctrl Pts',(-2.22995715977815,-4.71238887532414,
71.4998503815421));
#53829=CARTESIAN_POINT('Ctrl Pts',(-3.74422450225742,-3.62768531207155,
71.4469301274601));
#53830=CARTESIAN_POINT('Ctrl Pts',(-4.45636978489872,-2.15507932000099,
71.3940098733781));
#53831=CARTESIAN_POINT('Ctrl Pts',(-4.77794345735694,-1.49011484084619,
71.370113400471));
#53832=CARTESIAN_POINT('Ctrl Pts',(-4.93596197831358,-0.746055865118146,
71.3462169275639));
#53833=CARTESIAN_POINT('Ctrl Pts',(-4.93421645959303,-0.00129368103133631,
71.3223204546568));
#53834=CARTESIAN_POINT('Ctrl Pts',(-4.93445704478049,-0.00170468936910681,
71.1776795453431));
#53835=CARTESIAN_POINT('Ctrl Pts',(-4.93668140337337,-0.71987028628676,
71.2007254435883));
#53836=CARTESIAN_POINT('Ctrl Pts',(-4.79015415455198,-1.43717138679696,
71.2237713418334));
#53837=CARTESIAN_POINT('Ctrl Pts',(-4.49034790212576,-2.08335665417659,
71.2468172400785));
#53838=CARTESIAN_POINT('Ctrl Pts',(-3.80190335182005,-3.56719070438483,
71.2997374941605));
#53839=CARTESIAN_POINT('Ctrl Pts',(-2.30522086738965,-4.67603201128707,
71.3526577482425));
#53840=CARTESIAN_POINT('Ctrl Pts',(-0.685205212090817,-4.90245785784546,
71.4055780023244));
#53841=CARTESIAN_POINT('Ctrl Pts',(0.934810443208014,-5.12888370440385,
71.4584982564064));
#53842=CARTESIAN_POINT('Ctrl Pts',(2.67815926937537,-4.47289409061839,71.5114185104883));
#53843=CARTESIAN_POINT('Ctrl Pts',(3.74705821791536,-3.23467988248916,71.5643387645703));
#53844=CARTESIAN_POINT('Ctrl Pts',(4.8159571664554,-1.99646567435987,71.6172590186523));
#53845=CARTESIAN_POINT('Ctrl Pts',(5.21040623736806,-0.176026871886955,
71.6701792727342));
#53846=CARTESIAN_POINT('Ctrl Pts',(4.74989951150191,1.39357592590467,71.7230995268162));
#53847=CARTESIAN_POINT('Ctrl Pts',(4.28939278563578,2.96317872369621,71.7760197808982));
#53848=CARTESIAN_POINT('Ctrl Pts',(2.97393026299076,4.28194551680631,71.8289400349801));
#53849=CARTESIAN_POINT('Ctrl Pts',(1.40548768459228,4.74638847957966,71.8818602890621));
#53850=CARTESIAN_POINT('Ctrl Pts',(-0.162954893806299,5.21083144235304,
71.934780543144));
#53851=CARTESIAN_POINT('Ctrl Pts',(-1.98437752795848,4.82095057478956,71.987700797226));
#53852=CARTESIAN_POINT('Ctrl Pts',(-3.22526940243671,3.7551613164194,72.040621051308));
#53853=CARTESIAN_POINT('Ctrl Pts',(-4.29653392126676,2.83506324782479,72.0863072159864));
#53854=CARTESIAN_POINT('Ctrl Pts',(-4.93513440489649,1.41121710573191,72.1319933806648));
#53855=CARTESIAN_POINT('Ctrl Pts',(-4.9466376895248,-0.00356105100536129,
72.1776795453432));
#53856=CARTESIAN_POINT('Origin',(0.,0.,16.));
#53857=CARTESIAN_POINT('',(-4.94622533435752,0.00372181280100414,73.3223204546568));
#53858=CARTESIAN_POINT('',(-4.94548609638219,0.00396606047658106,73.1776795453432));
#53859=CARTESIAN_POINT('',(-4.942,-6.05220448138622E-16,16.));
#53860=CARTESIAN_POINT('Ctrl Pts',(-4.94622533435752,0.00372181280100414,
73.3223204546568));
#53861=CARTESIAN_POINT('Ctrl Pts',(-4.94823216917571,0.243062776937041,
73.3145933098808));
#53862=CARTESIAN_POINT('Ctrl Pts',(-4.93236152324834,0.482136497176127,
73.3068661651048));
#53863=CARTESIAN_POINT('Ctrl Pts',(-4.89769574881769,0.718453121134063,
73.2991390203288));
#53864=CARTESIAN_POINT('Ctrl Pts',(-4.66028314118601,2.33689513900433,73.2462187662469));
#53865=CARTESIAN_POINT('Ctrl Pts',(-3.5413122266531,3.82601954517773,73.1932985121649));
#53866=CARTESIAN_POINT('Ctrl Pts',(-2.05284118541496,4.50438026844074,73.1403782580829));
#53867=CARTESIAN_POINT('Ctrl Pts',(-0.564370144176819,5.18274099170376,
73.087458004001));
#53868=CARTESIAN_POINT('Ctrl Pts',(1.29360102376645,5.05033803205637,73.034537749919));
#53869=CARTESIAN_POINT('Ctrl Pts',(2.67083633572998,4.16776100598374,72.9816174958371));
#53870=CARTESIAN_POINT('Ctrl Pts',(4.04807164769343,3.28518397991116,72.9286972417551));
#53871=CARTESIAN_POINT('Ctrl Pts',(4.9445711036771,1.6524328874135,72.8757769876731));
#53872=CARTESIAN_POINT('Ctrl Pts',(4.95008286065676,0.0166795649332413,
72.8228567335911));
#53873=CARTESIAN_POINT('Ctrl Pts',(4.95559461763642,-1.61907375754711,72.7699364795092));
#53874=CARTESIAN_POINT('Ctrl Pts',(4.07011867561174,-3.25782931001015,72.7170162254272));
#53875=CARTESIAN_POINT('Ctrl Pts',(2.69886234926083,-4.14966752342842,72.6640959713453));
#53876=CARTESIAN_POINT('Ctrl Pts',(1.32760602290984,-5.04150573684673,72.6111757172633));
#53877=CARTESIAN_POINT('Ctrl Pts',(-0.529430687767451,-5.18642661122039,
72.5582554631813));
#53878=CARTESIAN_POINT('Ctrl Pts',(-2.02243942200268,-4.51811214110315,
72.5053352090994));
#53879=CARTESIAN_POINT('Ctrl Pts',(-3.51544815623782,-3.84979767098594,
72.4524149550174));
#53880=CARTESIAN_POINT('Ctrl Pts',(-4.64442891403086,-2.36824785637795,
72.3994947009354));
#53881=CARTESIAN_POINT('Ctrl Pts',(-4.89274285803262,-0.751442519707904,
72.3465744468535));
#53882=CARTESIAN_POINT('Ctrl Pts',(-4.93067795216383,-0.50444204261031,
72.3384897827879));
#53883=CARTESIAN_POINT('Ctrl Pts',(-4.9480592642285,-0.254284852349217,
72.3304051187224));
#53884=CARTESIAN_POINT('Ctrl Pts',(-4.9459185577707,-0.00382965742011687,
72.3223204546568));
#53885=CARTESIAN_POINT('Ctrl Pts',(-4.9466376895248,-0.00356105100536129,
72.1776795453432));
#53886=CARTESIAN_POINT('Ctrl Pts',(-4.94845915538918,-0.227581424440414,
72.1849136347467));
#53887=CARTESIAN_POINT('Ctrl Pts',(-4.93455770132463,-0.451374440445247,
72.1921477241503));
#53888=CARTESIAN_POINT('Ctrl Pts',(-4.90416141521875,-0.672904186423828,
72.1993818135539));
#53889=CARTESIAN_POINT('Ctrl Pts',(-4.68180043871832,-2.29348278172022,
72.2523020676359));
#53890=CARTESIAN_POINT('Ctrl Pts',(-3.57671737091314,-3.79294232313627,
72.3052223217178));
#53891=CARTESIAN_POINT('Ctrl Pts',(-2.09461510123176,-4.48510722372598,
72.3581425757998));
#53892=CARTESIAN_POINT('Ctrl Pts',(-0.612512831550301,-5.17727212431573,
72.4110628298817));
#53893=CARTESIAN_POINT('Ctrl Pts',(1.24660864000739,-5.06214238407903,72.4639830839637));
#53894=CARTESIAN_POINT('Ctrl Pts',(2.63198693425408,-4.19240313049007,72.5169033380457));
#53895=CARTESIAN_POINT('Ctrl Pts',(4.01736522850069,-3.32266387690115,72.5698235921276));
#53896=CARTESIAN_POINT('Ctrl Pts',(4.92900034543634,-1.69831510996005,72.6227438462096));
#53897=CARTESIAN_POINT('Ctrl Pts',(4.94971413242267,-0.0626836336085702,
72.6756641002916));
#53898=CARTESIAN_POINT('Ctrl Pts',(4.97042791940901,1.57294784274291,72.7285843543735));
#53899=CARTESIAN_POINT('Ctrl Pts',(4.10022037644603,3.21986202850478,72.7815046084555));
#53900=CARTESIAN_POINT('Ctrl Pts',(2.73731176561134,4.12440583944801,72.8344248625374));
#53901=CARTESIAN_POINT('Ctrl Pts',(1.37440315477665,5.02894965039124,72.8873451166194));
#53902=CARTESIAN_POINT('Ctrl Pts',(-0.481206523929751,5.19112308651582,
72.9402653707013));
#53903=CARTESIAN_POINT('Ctrl Pts',(-1.98036194136401,4.53671310662511,72.9931856247833));
#53904=CARTESIAN_POINT('Ctrl Pts',(-3.47951735879827,3.8823031267344,73.0461058788653));
#53905=CARTESIAN_POINT('Ctrl Pts',(-4.62221851496038,2.41130973082838,73.0990261329473));
#53906=CARTESIAN_POINT('Ctrl Pts',(-4.88554790865992,0.796881962912803,
73.1519463870292));
#53907=CARTESIAN_POINT('Ctrl Pts',(-4.92823035034716,0.535203165516849,
73.1605241064672));
#53908=CARTESIAN_POINT('Ctrl Pts',(-4.94780958080646,0.269756002185876,
73.1691018259052));
#53909=CARTESIAN_POINT('Ctrl Pts',(-4.94548609638219,0.00396606047658106,
73.1776795453432));
#53910=CARTESIAN_POINT('Origin',(0.,0.,16.));
#53911=CARTESIAN_POINT('',(-4.93430944804537,0.00146807591443893,74.3223204546568));
#53912=CARTESIAN_POINT('',(-4.93410780896188,0.00104985362950368,74.1776795453432));
#53913=CARTESIAN_POINT('',(-4.942,-6.05220448138622E-16,16.));
#53914=CARTESIAN_POINT('Ctrl Pts',(-4.93430944804537,0.00146807591443893,
74.3223204546568));
#53915=CARTESIAN_POINT('Ctrl Pts',(-4.93626271862051,0.735053226945857,
74.2987815010393));
#53916=CARTESIAN_POINT('Ctrl Pts',(-4.78313292282981,1.46786315098495,74.2752425474217));
#53917=CARTESIAN_POINT('Ctrl Pts',(-4.47079173349639,2.12499877904777,74.2517035938041));
#53918=CARTESIAN_POINT('Ctrl Pts',(-3.76858655614047,3.60237049949084,74.1987833397222));
#53919=CARTESIAN_POINT('Ctrl Pts',(-2.2616634474919,4.69725412310252,74.1458630856402));
#53920=CARTESIAN_POINT('Ctrl Pts',(-0.639613436851163,4.9086141818902,74.0929428315583));
#53921=CARTESIAN_POINT('Ctrl Pts',(0.982436573789575,5.11997424067789,74.0400225774763));
#53922=CARTESIAN_POINT('Ctrl Pts',(2.71961348642258,4.44781073464159,73.9871023233943));
#53923=CARTESIAN_POINT('Ctrl Pts',(3.77695861444706,3.19971594989436,73.9341820693124));
#53924=CARTESIAN_POINT('Ctrl Pts',(4.83430374247159,1.95162116514706,73.8812618152304));
#53925=CARTESIAN_POINT('Ctrl Pts',(5.21181708588759,0.127595101688968,73.8283415611484));
#53926=CARTESIAN_POINT('Ctrl Pts',(4.73674277310034,-1.43766005604103,73.7754213070665));
#53927=CARTESIAN_POINT('Ctrl Pts',(4.26166846031312,-3.00291521377094,73.7225010529845));
#53928=CARTESIAN_POINT('Ctrl Pts',(2.9340064913226,-4.30939946577263,73.6695807989026));
#53929=CARTESIAN_POINT('Ctrl Pts',(1.36131526012037,-4.7592456647895,73.6166605448206));
#53930=CARTESIAN_POINT('Ctrl Pts',(-0.211375971081961,-5.2090918638064,
73.5637402907386));
#53931=CARTESIAN_POINT('Ctrl Pts',(-2.02909646449615,-4.80230000983842,
73.5108200366566));
#53932=CARTESIAN_POINT('Ctrl Pts',(-3.260029560838,-3.72502426807083,73.4578997825747));
#53933=CARTESIAN_POINT('Ctrl Pts',(-4.31122810355742,-2.80504681907828,
73.4127066732687));
#53934=CARTESIAN_POINT('Ctrl Pts',(-4.9344881263814,-1.3960917881023,73.3675135639628));
#53935=CARTESIAN_POINT('Ctrl Pts',(-4.94622533435752,0.00372181280100414,
73.3223204546568));
#53936=CARTESIAN_POINT('Ctrl Pts',(-4.94548609638219,0.00396606047658106,
73.1776795453432));
#53937=CARTESIAN_POINT('Ctrl Pts',(-4.9334748398561,-1.37003547728531,73.2220220799872));
#53938=CARTESIAN_POINT('Ctrl Pts',(-4.33614096919029,-2.75319733775313,
73.2663646146311));
#53939=CARTESIAN_POINT('Ctrl Pts',(-3.3193311989464,-3.67227989433378,73.3107071492751));
#53940=CARTESIAN_POINT('Ctrl Pts',(-2.10582746429627,-4.76915184373973,
73.3636274033571));
#53941=CARTESIAN_POINT('Ctrl Pts',(-0.29486236375909,-5.2050336026263,73.416547657439));
#53942=CARTESIAN_POINT('Ctrl Pts',(1.28483881433472,-4.78045902103617,73.469467911521));
#53943=CARTESIAN_POINT('Ctrl Pts',(2.86453999242835,-4.35588443944609,73.522388165603));
#53944=CARTESIAN_POINT('Ctrl Pts',(4.21297724807857,-3.07085351737952,73.5753084196849));
#53945=CARTESIAN_POINT('Ctrl Pts',(4.71308509882384,-1.51341603066432,73.6282286737669));
#53946=CARTESIAN_POINT('Ctrl Pts',(5.21319294956918,0.0440214560510618,
73.6811489278489));
#53947=CARTESIAN_POINT('Ctrl Pts',(4.8649713954092,1.87386550741532,73.7340691819308));
#53948=CARTESIAN_POINT('Ctrl Pts',(3.82777193781054,3.13875153886656,73.7869894360128));
#53949=CARTESIAN_POINT('Ctrl Pts',(2.790572480212,4.40363757031766,73.8399096900947));
#53950=CARTESIAN_POINT('Ctrl Pts',(1.06439511917504,5.10356558185611,73.8928299441767));
#53951=CARTESIAN_POINT('Ctrl Pts',(-0.560835021503018,4.91823782561222,
73.9457501982587));
#53952=CARTESIAN_POINT('Ctrl Pts',(-2.18606516218117,4.73291006936832,73.9986704523406));
#53953=CARTESIAN_POINT('Ctrl Pts',(-3.71034808250029,3.662326545342,74.0515907064226));
#53954=CARTESIAN_POINT('Ctrl Pts',(-4.43614863820842,2.1964026248274,74.1045109605045));
#53955=CARTESIAN_POINT('Ctrl Pts',(-4.77065068257367,1.52079753684611,74.1289004887841));
#53956=CARTESIAN_POINT('Ctrl Pts',(-4.9355517737741,0.761220515306077,74.1532900170636));
#53957=CARTESIAN_POINT('Ctrl Pts',(-4.93410780896188,0.00104985362950368,
74.1776795453432));
#53958=CARTESIAN_POINT('Origin',(0.,0.,16.));
#53959=CARTESIAN_POINT('',(-4.94084634488987,-0.00449823523784309,75.3223204546568));
#53960=CARTESIAN_POINT('',(-4.94163609422309,-0.00451829382380276,75.1776795453432));
#53961=CARTESIAN_POINT('',(-4.942,-6.05220448138622E-16,16.));
#53962=CARTESIAN_POINT('Ctrl Pts',(-4.94084634488987,-0.00449823523784309,
75.3223204546568));
#53963=CARTESIAN_POINT('Ctrl Pts',(-4.92989311437387,1.21777170867941,75.2829696921977));
#53964=CARTESIAN_POINT('Ctrl Pts',(-4.47139568953686,2.44738194782565,75.2436189297386));
#53965=CARTESIAN_POINT('Ctrl Pts',(-3.64967329880456,3.34417154871685,75.2042681672795));
#53966=CARTESIAN_POINT('Ctrl Pts',(-2.54459286363954,4.55020494099322,75.1513479131975));
#53967=CARTESIAN_POINT('Ctrl Pts',(-0.782591300857919,5.15430584099797,
75.0984276591155));
#53968=CARTESIAN_POINT('Ctrl Pts',(0.83001256389233,4.88002845063787,75.0455074050336));
#53969=CARTESIAN_POINT('Ctrl Pts',(2.44261642864267,4.60575106027776,74.9925871509516));
#53970=CARTESIAN_POINT('Ctrl Pts',(3.90582259536151,3.45309537955268,74.9396668968697));
#53971=CARTESIAN_POINT('Ctrl Pts',(4.55004557505128,1.94953425212549,74.8867466427877));
#53972=CARTESIAN_POINT('Ctrl Pts',(5.19426855474108,0.445973124698207,74.8338263887057));
#53973=CARTESIAN_POINT('Ctrl Pts',(5.01950834740155,-1.40849344943142,74.7809061346238));
#53974=CARTESIAN_POINT('Ctrl Pts',(4.10573789297132,-2.76523324323168,74.7279858805418));
#53975=CARTESIAN_POINT('Ctrl Pts',(3.19196743854115,-4.12197303703186,74.6750656264599));
#53976=CARTESIAN_POINT('Ctrl Pts',(1.53918673702048,-4.98098605050295,74.6221453723779));
#53977=CARTESIAN_POINT('Ctrl Pts',(-0.0962665201530125,-4.94917480923354,
74.5692251182959));
#53978=CARTESIAN_POINT('Ctrl Pts',(-1.73171977732641,-4.91736356796412,
74.516304864214));
#53979=CARTESIAN_POINT('Ctrl Pts',(-3.34984559015253,-3.99472807195434,
74.463384610132));
#53980=CARTESIAN_POINT('Ctrl Pts',(-4.21016487353403,-2.60348041531225,
74.4104643560501));
#53981=CARTESIAN_POINT('Ctrl Pts',(-4.68781373971693,-1.8310603631163,74.3810830555857));
#53982=CARTESIAN_POINT('Ctrl Pts',(-4.93187137749265,-0.914192241399431,
74.3517017551212));
#53983=CARTESIAN_POINT('Ctrl Pts',(-4.93430944804537,0.00146807591443893,
74.3223204546568));
#53984=CARTESIAN_POINT('Ctrl Pts',(-4.93410780896188,0.00104985362950368,
74.1776795453432));
#53985=CARTESIAN_POINT('Ctrl Pts',(-4.93241866747241,-0.888193286408816,
74.2062102711456));
#53986=CARTESIAN_POINT('Ctrl Pts',(-4.70309992547236,-1.77824877440845,
74.234740996948));
#53987=CARTESIAN_POINT('Ctrl Pts',(-4.25136351730091,-2.53564734819139,
74.2632717227504));
#53988=CARTESIAN_POINT('Ctrl Pts',(-3.41345964958825,-3.94050908369249,
74.3161919768324));
#53989=CARTESIAN_POINT('Ctrl Pts',(-1.8103337230659,-4.88896823769192,74.3691122309144));
#53990=CARTESIAN_POINT('Ctrl Pts',(-0.175600645770052,-4.94699541578848,
74.4220324849964));
#53991=CARTESIAN_POINT('Ctrl Pts',(1.45913243152579,-5.00502259388504,74.4749527390783));
#53992=CARTESIAN_POINT('Ctrl Pts',(3.12547265959522,-4.17261779607872,74.5278729931603));
#53993=CARTESIAN_POINT('Ctrl Pts',(4.06087730056111,-2.83070217091354,74.5807932472422));
#53994=CARTESIAN_POINT('Ctrl Pts',(4.99628194152704,-1.48878654574829,74.6337135013242));
#53995=CARTESIAN_POINT('Ctrl Pts',(5.20075099538943,0.36263990677569,74.6866337554061));
#53996=CARTESIAN_POINT('Ctrl Pts',(4.58071630030657,1.87633616570506,74.7395540094881));
#53997=CARTESIAN_POINT('Ctrl Pts',(3.96068160522376,3.39003242463435,74.7924742635701));
#53998=CARTESIAN_POINT('Ctrl Pts',(2.51614316119567,4.56599848996891,74.8453945176521));
#53999=CARTESIAN_POINT('Ctrl Pts',(0.908143822210297,4.86609433003599,74.898314771734));
#54000=CARTESIAN_POINT('Ctrl Pts',(-0.699855516775171,5.16619017010308,
74.951235025816));
#54001=CARTESIAN_POINT('Ctrl Pts',(-2.47131575071806,4.59041578490263,75.0041552798979));
#54002=CARTESIAN_POINT('Ctrl Pts',(-3.59558962158726,3.4022543267312,75.0570755339799));
#54003=CARTESIAN_POINT('Ctrl Pts',(-4.44965416990239,2.49965701001681,75.097276871101));
#54004=CARTESIAN_POINT('Ctrl Pts',(-4.93023943833446,1.2436624400959,75.1374782082221));
#54005=CARTESIAN_POINT('Ctrl Pts',(-4.94163609422309,-0.00451829382380276,
75.1776795453432));
#54006=CARTESIAN_POINT('Origin',(0.,0.,16.));
#54007=CARTESIAN_POINT('',(-4.949709811623,0.00127385101247733,76.3223204546568));
#54008=CARTESIAN_POINT('',(-4.94936999019276,0.00173199160742904,76.1776795453431));
#54009=CARTESIAN_POINT('',(-4.942,-6.05220448138622E-16,16.));
#54010=CARTESIAN_POINT('Ctrl Pts',(-4.949709811623,0.00127385101247733,
76.3223204546568));
#54011=CARTESIAN_POINT('Ctrl Pts',(-4.94994903879905,0.0705988515890139,
76.3200781374381));
#54012=CARTESIAN_POINT('Ctrl Pts',(-4.94861862980554,0.139914463982202,
76.3178358202194));
#54013=CARTESIAN_POINT('Ctrl Pts',(-4.94569000143091,0.209162484687126,
76.3155935030007));
#54014=CARTESIAN_POINT('Ctrl Pts',(-4.87657232423312,1.84346418821971,76.2626732489188));
#54015=CARTESIAN_POINT('Ctrl Pts',(-3.91725763853945,3.44011779449909,76.2097529948368));
#54016=CARTESIAN_POINT('Ctrl Pts',(-2.50674299584768,4.26847022808205,76.1568327407548));
#54017=CARTESIAN_POINT('Ctrl Pts',(-1.09622835315598,5.09682266166495,76.1039124866729));
#54018=CARTESIAN_POINT('Ctrl Pts',(0.765486246533761,5.15687392255156,76.0509922325909));
#54019=CARTESIAN_POINT('Ctrl Pts',(2.22645176899709,4.4211436366153,75.9980719785089));
#54020=CARTESIAN_POINT('Ctrl Pts',(3.68741729146043,3.68541335067904,75.9451517244269));
#54021=CARTESIAN_POINT('Ctrl Pts',(4.74763373669735,2.15390151791992,75.892231470345));
#54022=CARTESIAN_POINT('Ctrl Pts',(4.92192986700097,0.527451343327534,75.8393112162631));
#54023=CARTESIAN_POINT('Ctrl Pts',(5.09622599730458,-1.09899883126485,75.7863909621811));
#54024=CARTESIAN_POINT('Ctrl Pts',(4.38460181267489,-2.8203873476905,75.7334707080991));
#54025=CARTESIAN_POINT('Ctrl Pts',(3.1127074084203,-3.84898053058463,75.6805504540171));
#54026=CARTESIAN_POINT('Ctrl Pts',(1.84081300416571,-4.87757371347876,75.6276301999351));
#54027=CARTESIAN_POINT('Ctrl Pts',(0.00864838028622472,-5.21337156284137,
75.5747099458532));
#54028=CARTESIAN_POINT('Ctrl Pts',(-1.54535994923236,-4.70270785426469,
75.5217896917713));
#54029=CARTESIAN_POINT('Ctrl Pts',(-3.09936827875094,-4.19204414568801,
75.4688694376893));
#54030=CARTESIAN_POINT('Ctrl Pts',(-4.37522031390861,-2.83491887917204,
75.4159491836074));
#54031=CARTESIAN_POINT('Ctrl Pts',(-4.78906667771331,-1.25237330364,75.3630289295254));
#54032=CARTESIAN_POINT('Ctrl Pts',(-4.89518266041626,-0.846586534424758,
75.3494594379025));
#54033=CARTESIAN_POINT('Ctrl Pts',(-4.94462339418807,-0.425978804568305,
75.3358899462797));
#54034=CARTESIAN_POINT('Ctrl Pts',(-4.94084634488987,-0.00449823523784309,
75.3223204546568));
#54035=CARTESIAN_POINT('Ctrl Pts',(-4.94163609422309,-0.00451829382380276,
75.1776795453432));
#54036=CARTESIAN_POINT('Ctrl Pts',(-4.94524177329398,-0.3994182708838,75.1903984623041));
#54037=CARTESIAN_POINT('Ctrl Pts',(-4.90188327382623,-0.793536109632625,
75.2031173792649));
#54038=CARTESIAN_POINT('Ctrl Pts',(-4.80852961499291,-1.17543275960954,
75.2158362962258));
#54039=CARTESIAN_POINT('Ctrl Pts',(-4.42010822973382,-2.76440985663659,
75.2687565503078));
#54040=CARTESIAN_POINT('Ctrl Pts',(-3.16617795142011,-4.14181551954833,
75.3216768043897));
#54041=CARTESIAN_POINT('Ctrl Pts',(-1.62055642630759,-4.6773278802945,75.3745970584716));
#54042=CARTESIAN_POINT('Ctrl Pts',(-0.0749349011951517,-5.21284024104065,
75.4275173125536));
#54043=CARTESIAN_POINT('Ctrl Pts',(1.76237787071597,-4.90645929962131,75.4804375666356));
#54044=CARTESIAN_POINT('Ctrl Pts',(3.05059950427476,-3.89838965409382,75.5333578207175));
#54045=CARTESIAN_POINT('Ctrl Pts',(4.3388211378337,-2.8903200085662,75.5862780747995));
#54046=CARTESIAN_POINT('Ctrl Pts',(5.07795163304007,-1.18056165893029,75.6391983288815));
#54047=CARTESIAN_POINT('Ctrl Pts',(4.92975358676999,0.448473861396107,75.6921185829634));
#54048=CARTESIAN_POINT('Ctrl Pts',(4.78155554049993,2.07750938172241,75.7450388370454));
#54049=CARTESIAN_POINT('Ctrl Pts',(3.74602895275332,3.62582207273939,75.7979590911274));
#54050=CARTESIAN_POINT('Ctrl Pts',(2.29704660536897,4.38488040012382,75.8508793452094));
#54051=CARTESIAN_POINT('Ctrl Pts',(0.848064257984615,5.14393872750825,75.9037995992913));
#54052=CARTESIAN_POINT('Ctrl Pts',(-1.0143738490375,5.11374269126039,75.9567198533733));
#54053=CARTESIAN_POINT('Ctrl Pts',(-2.43798759346781,4.30811045874223,76.0096401074552));
#54054=CARTESIAN_POINT('Ctrl Pts',(-3.86160133789813,3.50247822622406,76.0625603615372));
#54055=CARTESIAN_POINT('Ctrl Pts',(-4.84639071973656,1.92140979743563,76.1154806156192));
#54056=CARTESIAN_POINT('Ctrl Pts',(-4.94170107746221,0.28842623257243,76.1684008697011));
#54057=CARTESIAN_POINT('Ctrl Pts',(-4.94727143302206,0.192987506953041,
76.1714937615818));
#54058=CARTESIAN_POINT('Ctrl Pts',(-4.94980355369306,0.0973714523878282,
76.1745866534625));
#54059=CARTESIAN_POINT('Ctrl Pts',(-4.94936999019276,0.00173199160742904,
76.1776795453431));
#54060=CARTESIAN_POINT('Origin',(0.,0.,16.));
#54061=CARTESIAN_POINT('',(-4.93710573305067,0.00369191742993435,77.3223204546568));
#54062=CARTESIAN_POINT('',(-4.93651943436554,0.00342058198068374,77.1776795453431));
#54063=CARTESIAN_POINT('',(-4.942,-6.05220448138622E-16,16.));
#54064=CARTESIAN_POINT('Ctrl Pts',(-4.93710573305067,0.00369191742993435,
77.3223204546568));
#54065=CARTESIAN_POINT('Ctrl Pts',(-4.94100558540341,0.565545404544723,
77.3042663285965));
#54066=CARTESIAN_POINT('Ctrl Pts',(-4.85249197896959,1.12620708123838,77.2862122025363));
#54067=CARTESIAN_POINT('Ctrl Pts',(-4.66622450050179,1.65225526059718,77.2681580764761));
#54068=CARTESIAN_POINT('Ctrl Pts',(-4.12023726994686,3.19420767735372,77.2152378223941));
#54069=CARTESIAN_POINT('Ctrl Pts',(-2.73435528454182,4.43876323142188,77.1623175683121));
#54070=CARTESIAN_POINT('Ctrl Pts',(-1.14277930696628,4.81639429353784,77.1093973142302));
#54071=CARTESIAN_POINT('Ctrl Pts',(0.448796670609252,5.1940253556538,77.0564770601482));
#54072=CARTESIAN_POINT('Ctrl Pts',(2.24606664035538,4.70473192581759,77.0035568060662));
#54073=CARTESIAN_POINT('Ctrl Pts',(3.42657241495318,3.57242215035347,76.9506365519843));
#54074=CARTESIAN_POINT('Ctrl Pts',(4.60707818955111,2.44011237488923,76.8977162979023));
#54075=CARTESIAN_POINT('Ctrl Pts',(5.1708197690006,0.664786253797156,76.8447960438203));
#54076=CARTESIAN_POINT('Ctrl Pts',(4.85982039669027,-0.941139865890017,
76.7918757897384));
#54077=CARTESIAN_POINT('Ctrl Pts',(4.54882102437996,-2.54706598557701,76.7389555356564));
#54078=CARTESIAN_POINT('Ctrl Pts',(3.36308070030987,-3.983592103859,76.6860352815744));
#54079=CARTESIAN_POINT('Ctrl Pts',(1.84521230622943,-4.59334192937927,76.6331150274925));
#54080=CARTESIAN_POINT('Ctrl Pts',(0.327343912148982,-5.20309175489953,
76.5801947734105));
#54081=CARTESIAN_POINT('Ctrl Pts',(-1.52265255194192,-4.98606528765813,
76.5272745193286));
#54082=CARTESIAN_POINT('Ctrl Pts',(-2.85819044963632,-4.04157715364459,
76.4743542652466));
#54083=CARTESIAN_POINT('Ctrl Pts',(-4.13713943489684,-3.13710851769457,
76.4236763283833));
#54084=CARTESIAN_POINT('Ctrl Pts',(-4.94430311018814,-1.56551963073416,
76.3729983915201));
#54085=CARTESIAN_POINT('Ctrl Pts',(-4.949709811623,0.00127385101247733,
76.3223204546568));
#54086=CARTESIAN_POINT('Ctrl Pts',(-4.94936999019276,0.00173199160742904,
76.1776795453431));
#54087=CARTESIAN_POINT('Ctrl Pts',(-4.9423851596845,-1.5390467478049,76.2275069075444));
#54088=CARTESIAN_POINT('Ctrl Pts',(-4.16568308583621,-3.08590036450939,
76.2773342697457));
#54089=CARTESIAN_POINT('Ctrl Pts',(-2.92261878913845,-3.99523449174163,
76.327161631947));
#54090=CARTESIAN_POINT('Ctrl Pts',(-1.60239480947616,-4.96101295025462,
76.380081886029));
#54091=CARTESIAN_POINT('Ctrl Pts',(0.243884483461281,-5.20767116634268,
76.4330021401109));
#54092=CARTESIAN_POINT('Ctrl Pts',(1.77133348755807,-4.62233457318728,76.4859223941929));
#54093=CARTESIAN_POINT('Ctrl Pts',(3.29878249165486,-4.03699798003188,76.5388426482749));
#54094=CARTESIAN_POINT('Ctrl Pts',(4.507401206911,-2.61966657763301,76.5917629023568));
#54095=CARTESIAN_POINT('Ctrl Pts',(4.84410725035561,-1.01893286220407,76.6446831564388));
#54096=CARTESIAN_POINT('Ctrl Pts',(5.18081329380023,0.581800853224953,76.6976034105207));
#54097=CARTESIAN_POINT('Ctrl Pts',(4.64560666543322,2.36593688168406,76.7505236646027));
#54098=CARTESIAN_POINT('Ctrl Pts',(3.483406092445,3.51702732797801,76.8034439186847));
#54099=CARTESIAN_POINT('Ctrl Pts',(2.32120551945685,4.6681177742719,76.8563641727667));
#54100=CARTESIAN_POINT('Ctrl Pts',(0.532011001847567,5.1861626384007,76.9092844268486));
#54101=CARTESIAN_POINT('Ctrl Pts',(-1.06541472329578,4.83409667859588,76.9622046809306));
#54102=CARTESIAN_POINT('Ctrl Pts',(-2.66284044843913,4.48203071879105,77.0151249350126));
#54103=CARTESIAN_POINT('Ctrl Pts',(-4.06849738111654,3.2598539350526,77.0680451890945));
#54104=CARTESIAN_POINT('Ctrl Pts',(-4.63913544075982,1.72685308955721,77.1209654431764));
#54105=CARTESIAN_POINT('Ctrl Pts',(-4.84298445708464,1.17921924512925,77.1398701438987));
#54106=CARTESIAN_POINT('Ctrl Pts',(-4.94027400061573,0.591920131780996,
77.1587748446209));
#54107=CARTESIAN_POINT('Ctrl Pts',(-4.93651943436554,0.00342058198068374,
77.1776795453431));
#54108=CARTESIAN_POINT('Origin',(0.,0.,16.));
#54109=CARTESIAN_POINT('',(-4.93642136366389,-0.0033694929564293,78.3223204546568));
#54110=CARTESIAN_POINT('',(-4.93699915860479,-0.00364661157755484,78.1776795453431));
#54111=CARTESIAN_POINT('',(-4.942,-6.05220448138622E-16,16.));
#54112=CARTESIAN_POINT('Ctrl Pts',(-4.93642136366389,-0.0033694929564293,
78.3223204546568));
#54113=CARTESIAN_POINT('Ctrl Pts',(-4.92980420575396,1.05092284524382,78.288454519755));
#54114=CARTESIAN_POINT('Ctrl Pts',(-4.59907343284897,2.10900469043804,78.2545885848532));
#54115=CARTESIAN_POINT('Ctrl Pts',(-3.975312192884,2.94965955736624,78.2207226499514));
#54116=CARTESIAN_POINT('Ctrl Pts',(-3.00059812102546,4.26330021964482,78.1678023958694));
#54117=CARTESIAN_POINT('Ctrl Pts',(-1.31034971100207,5.04601837903923,78.1148821417875));
#54118=CARTESIAN_POINT('Ctrl Pts',(0.321949550104491,4.93963025159188,78.0619618877055));
#54119=CARTESIAN_POINT('Ctrl Pts',(1.95424881121096,4.83324212414454,78.0090416336236));
#54120=CARTESIAN_POINT('Ctrl Pts',(3.52859892340051,3.83774770985554,77.9561213795416));
#54121=CARTESIAN_POINT('Ctrl Pts',(4.32455323076013,2.40870045658987,77.9032011254596));
#54122=CARTESIAN_POINT('Ctrl Pts',(5.12050753811972,0.979653203324283,77.8502808713777));
#54123=CARTESIAN_POINT('Ctrl Pts',(5.13806604064937,-0.882946888918111,
77.7973606172957));
#54124=CARTESIAN_POINT('Ctrl Pts',(4.36919369942578,-2.32674557099659,77.7444403632137));
#54125=CARTESIAN_POINT('Ctrl Pts',(3.60032135820212,-3.77054425307524,77.6915201091318));
#54126=CARTESIAN_POINT('Ctrl Pts',(2.04501817322514,-4.79554152499005,77.6385998550498));
#54127=CARTESIAN_POINT('Ctrl Pts',(0.415014635617477,-4.93268298063817,
77.5856796009678));
#54128=CARTESIAN_POINT('Ctrl Pts',(-1.21498890199009,-5.06982443628629,
77.5327593468859));
#54129=CARTESIAN_POINT('Ctrl Pts',(-2.91969279222824,-4.3191100756678,77.4798390928039));
#54130=CARTESIAN_POINT('Ctrl Pts',(-3.91899849949491,-3.02407825563606,
77.4269188387219));
#54131=CARTESIAN_POINT('Ctrl Pts',(-4.57738386303512,-2.17085587390878,
77.3920527107002));
#54132=CARTESIAN_POINT('Ctrl Pts',(-4.92957433823582,-1.08135952985832,
77.3571865826785));
#54133=CARTESIAN_POINT('Ctrl Pts',(-4.93710573305067,0.00369191742993435,
77.3223204546568));
#54134=CARTESIAN_POINT('Ctrl Pts',(-4.93651943436554,0.00342058198068374,
77.1776795453431));
#54135=CARTESIAN_POINT('Ctrl Pts',(-4.92976377869543,-1.05547678606275,
77.2116950987028));
#54136=CARTESIAN_POINT('Ctrl Pts',(-4.59587353108828,-2.11826061804498,
77.2457106520626));
#54137=CARTESIAN_POINT('Ctrl Pts',(-3.96697769860343,-2.96085919445861,
77.2797262054223));
#54138=CARTESIAN_POINT('Ctrl Pts',(-2.98856271019464,-4.27174572572668,
77.3326464595043));
#54139=CARTESIAN_POINT('Ctrl Pts',(-1.29611354676788,-5.0496938810105,77.3855667135863));
#54140=CARTESIAN_POINT('Ctrl Pts',(0.335879206226305,-4.93870270308427,
77.4384869676682));
#54141=CARTESIAN_POINT('Ctrl Pts',(1.96787195922058,-4.82771152515804,77.4914072217502));
#54142=CARTESIAN_POINT('Ctrl Pts',(3.53940830178236,-3.82778101402163,77.5443274758322));
#54143=CARTESIAN_POINT('Ctrl Pts',(4.33132920195393,-2.39649464320875,77.5972477299141));
#54144=CARTESIAN_POINT('Ctrl Pts',(5.12325010212551,-0.96520827239587,77.6501679839961));
#54145=CARTESIAN_POINT('Ctrl Pts',(5.13555555990697,0.897433958093309,77.7030882380781));
#54146=CARTESIAN_POINT('Ctrl Pts',(4.36261440987998,2.33905851601337,77.75600849216));
#54147=CARTESIAN_POINT('Ctrl Pts',(3.58967325985303,3.78068307393336,77.808928746242));
#54148=CARTESIAN_POINT('Ctrl Pts',(2.03148550201762,4.8012899592841,77.8618490003239));
#54149=CARTESIAN_POINT('Ctrl Pts',(0.40110165209169,4.93383387390743,77.9147692544059));
#54150=CARTESIAN_POINT('Ctrl Pts',(-1.22928219783424,5.06637778853077,77.9676895084879));
#54151=CARTESIAN_POINT('Ctrl Pts',(-2.93186213985079,4.31085873242671,78.0206097625698));
#54152=CARTESIAN_POINT('Ctrl Pts',(-3.92751158950039,3.01301376448353,78.0735300166518));
#54153=CARTESIAN_POINT('Ctrl Pts',(-4.58067311036902,2.16160728461073,78.1082465262156));
#54154=CARTESIAN_POINT('Ctrl Pts',(-4.92960256861,1.07680737701515,78.1429630357793));
#54155=CARTESIAN_POINT('Ctrl Pts',(-4.93699915860479,-0.00364661157755484,
78.1776795453431));
#54156=CARTESIAN_POINT('Origin',(0.,0.,16.));
#54157=CARTESIAN_POINT('',(-4.94930076406873,-0.0018103975202266,79.3223204546568));
#54158=CARTESIAN_POINT('',(-4.94965689841004,-0.00135584006909748,79.1776795453431));
#54159=CARTESIAN_POINT('',(-4.942,-6.05220448138622E-16,16.));
#54160=CARTESIAN_POINT('Ctrl Pts',(-4.94930076406873,-0.0018103975202266,
79.3223204546568));
#54161=CARTESIAN_POINT('Ctrl Pts',(-4.94206344439878,1.53439887470602,79.2726427109135));
#54162=CARTESIAN_POINT('Ctrl Pts',(-4.17064455342085,3.07688083896746,79.2229649671701));
#54163=CARTESIAN_POINT('Ctrl Pts',(-2.93387463574621,3.9869760667678,79.1732872234267));
#54164=CARTESIAN_POINT('Ctrl Pts',(-1.61637965001588,4.95647401624775,79.1203669693448));
#54165=CARTESIAN_POINT('Ctrl Pts',(0.229196639493549,5.20833819439267,79.0674467152628));
#54166=CARTESIAN_POINT('Ctrl Pts',(1.75829033577168,4.62731170663768,79.0145264611808));
#54167=CARTESIAN_POINT('Ctrl Pts',(3.28738403204981,4.04628521888269,78.9616062070989));
#54168=CARTESIAN_POINT('Ctrl Pts',(4.49999513509664,2.6323680652278,78.9086859530169));
#54169=CARTESIAN_POINT('Ctrl Pts',(4.84121428431374,1.03259032951638,78.8557656989349));
#54170=CARTESIAN_POINT('Ctrl Pts',(5.18243343353085,-0.567187406195048,
78.802845444853));
#54171=CARTESIAN_POINT('Ctrl Pts',(4.65226062891823,-2.35282572396301,78.749925190771));
#54172=CARTESIAN_POINT('Ctrl Pts',(3.49331104303619,-3.50718925806059,78.6970049366891));
#54173=CARTESIAN_POINT('Ctrl Pts',(2.33436145715409,-4.66155279215825,78.6440846826071));
#54174=CARTESIAN_POINT('Ctrl Pts',(0.546635090002505,-5.18464154258545,
78.5911644285251));
#54175=CARTESIAN_POINT('Ctrl Pts',(-1.05177716940348,-4.83708210816974,
78.5382441744432));
#54176=CARTESIAN_POINT('Ctrl Pts',(-2.65018942880937,-4.48952267375405,
78.4853239203612));
#54177=CARTESIAN_POINT('Ctrl Pts',(-4.05928758046969,-3.27131505449554,
78.4324036662792));
#54178=CARTESIAN_POINT('Ctrl Pts',(-4.63424678945294,-1.73992966228502,
78.3794834121973));
#54179=CARTESIAN_POINT('Ctrl Pts',(-4.84126499965602,-1.18854330639521,
78.3604290930171));
#54180=CARTESIAN_POINT('Ctrl Pts',(-4.94014443935181,-0.596556209328453,
78.3413747738369));
#54181=CARTESIAN_POINT('Ctrl Pts',(-4.93642136366389,-0.0033694929564293,
78.3223204546568));
#54182=CARTESIAN_POINT('Ctrl Pts',(-4.93699915860479,-0.00364661157755484,
78.1776795453431));
#54183=CARTESIAN_POINT('Ctrl Pts',(-4.94087759097782,-0.57018710251793,
78.1958832898613));
#54184=CARTESIAN_POINT('Ctrl Pts',(-4.85085250590991,-1.13553269504931,
78.2140870343795));
#54185=CARTESIAN_POINT('Ctrl Pts',(-4.66154625697823,-1.66540857589943,
78.2322907788976));
#54186=CARTESIAN_POINT('Ctrl Pts',(-4.11121251752373,-3.20581506855694,
78.2852110329796));
#54187=CARTESIAN_POINT('Ctrl Pts',(-2.72182608133198,-4.44645717408944,
78.3381312870616));
#54188=CARTESIAN_POINT('Ctrl Pts',(-1.12919140128498,-4.819598117052,78.3910515411436));
#54189=CARTESIAN_POINT('Ctrl Pts',(0.463443278761841,-5.19273906001451,
78.4439717952256));
#54190=CARTESIAN_POINT('Ctrl Pts',(2.25932620266378,-4.69837884040726,78.4968920493075));
#54191=CARTESIAN_POINT('Ctrl Pts',(3.43663391646442,-3.56274424493725,78.5498123033895));
#54192=CARTESIAN_POINT('Ctrl Pts',(4.6139416302652,-2.42710964946711,78.6027325574714));
#54193=CARTESIAN_POINT('Ctrl Pts',(5.17267413396446,-0.65020067813383,78.6556528115534));
#54194=CARTESIAN_POINT('Ctrl Pts',(4.85714690051601,0.954841985584431,78.7085730656353));
#54195=CARTESIAN_POINT('Ctrl Pts',(4.54161966706758,2.5598846493026,78.7614933197173));
#54196=CARTESIAN_POINT('Ctrl Pts',(3.35183269647175,3.99306100540591,78.8144135737993));
#54197=CARTESIAN_POINT('Ctrl Pts',(1.83225067773116,4.59852766487066,78.8673338278812));
#54198=CARTESIAN_POINT('Ctrl Pts',(0.312668658990661,5.20399432433538,78.9202540819632));
#54199=CARTESIAN_POINT('Ctrl Pts',(-1.53670840789443,4.98175128716162,78.9731743360452));
#54200=CARTESIAN_POINT('Ctrl Pts',(-2.86957733213866,4.03350036141105,79.0260945901271));
#54201=CARTESIAN_POINT('Ctrl Pts',(-4.14220208735026,3.12810930583763,79.0766229085325));
#54202=CARTESIAN_POINT('Ctrl Pts',(-4.94395467452422,1.56085664483311,79.1271512269378));
#54203=CARTESIAN_POINT('Ctrl Pts',(-4.94965689841004,-0.00135584006909748,
79.1776795453431));
#54204=CARTESIAN_POINT('Origin',(0.,0.,16.));
#54205=CARTESIAN_POINT('',(-4.94177616066966,0.00451715357047341,80.3223204546568));
#54206=CARTESIAN_POINT('',(-4.94098429374081,0.00450501606805162,80.1776795453432));
#54207=CARTESIAN_POINT('',(-4.942,-6.05220448138622E-16,16.));
#54208=CARTESIAN_POINT('Ctrl Pts',(-4.94177616066966,0.00451715357047341,
80.3223204546568));
#54209=CARTESIAN_POINT('Ctrl Pts',(-4.94534763047119,0.394743465756727,
80.3097511561539));
#54210=CARTESIAN_POINT('Ctrl Pts',(-4.90301618269456,0.784203971238864,
80.2971818576509));
#54211=CARTESIAN_POINT('Ctrl Pts',(-4.81182542362119,1.16186687182505,80.284612559148));
#54212=CARTESIAN_POINT('Ctrl Pts',(-4.42788688170829,2.75193306777578,80.231692305066));
#54213=CARTESIAN_POINT('Ctrl Pts',(-3.17784621930909,4.13286961482545,80.178772050984));
#54214=CARTESIAN_POINT('Ctrl Pts',(-1.63374113503097,4.67273885841708,80.125851796902));
#54215=CARTESIAN_POINT('Ctrl Pts',(-0.0896360507527699,5.21260810200875,
80.07293154282));
#54216=CARTESIAN_POINT('Ctrl Pts',(1.74853345540447,4.91141004214231,80.0200112887381));
#54217=CARTESIAN_POINT('Ctrl Pts',(3.03959294361313,3.90697751111939,79.9670910346562));
#54218=CARTESIAN_POINT('Ctrl Pts',(4.33065243182171,2.90254498009653,79.9141707805742));
#54219=CARTESIAN_POINT('Ctrl Pts',(5.0746019020818,1.1948779779175,79.8612505264923));
#54220=CARTESIAN_POINT('Ctrl Pts',(4.93099871468662,-0.43456899453677,79.8083302724103));
#54221=CARTESIAN_POINT('Ctrl Pts',(4.78739552729143,-2.06401596699104,79.7554100183283));
#54222=CARTESIAN_POINT('Ctrl Pts',(3.7562396822408,-3.61524290972046,79.7024897642464));
#54223=CARTESIAN_POINT('Ctrl Pts',(2.30940384276248,-4.37838468231013,79.6495695101644));
#54224=CARTESIAN_POINT('Ctrl Pts',(0.86256800328416,-5.14152645489981,79.5966492560824));
#54225=CARTESIAN_POINT('Ctrl Pts',(-0.999947830621951,-5.1165830573498,
79.5437290020005));
#54226=CARTESIAN_POINT('Ctrl Pts',(-2.4258279677168,-4.31496896933192,79.4908087479185));
#54227=CARTESIAN_POINT('Ctrl Pts',(-3.85170810481173,-3.51335488131399,
79.4378884938365));
#54228=CARTESIAN_POINT('Ctrl Pts',(-4.84095254509543,-1.93507010282805,
79.3849682397546));
#54229=CARTESIAN_POINT('Ctrl Pts',(-4.9408679242616,-0.302361853177563,
79.3320479856726));
#54230=CARTESIAN_POINT('Ctrl Pts',(-4.94698990261473,-0.202323153982769,
79.328805475334));
#54231=CARTESIAN_POINT('Ctrl Pts',(-4.94977315033439,-0.10208013749047,
79.3255629649954));
#54232=CARTESIAN_POINT('Ctrl Pts',(-4.94930076406873,-0.0018103975202266,
79.3223204546568));
#54233=CARTESIAN_POINT('Ctrl Pts',(-4.94965689841004,-0.00135584006909748,
79.1776795453431));
#54234=CARTESIAN_POINT('Ctrl Pts',(-4.9499268332343,-0.0753086628631314,
79.1800714810198));
#54235=CARTESIAN_POINT('Ctrl Pts',(-4.94841287075996,-0.149250190949008,
79.1824634166964));
#54236=CARTESIAN_POINT('Ctrl Pts',(-4.94508051525459,-0.223109677684533,
79.184855352373));
#54237=CARTESIAN_POINT('Ctrl Pts',(-4.87135399252289,-1.85720997670206,
79.237775606455));
#54238=CARTESIAN_POINT('Ctrl Pts',(-3.90754016545605,-3.45115176040958,
79.290695860537));
#54239=CARTESIAN_POINT('Ctrl Pts',(-2.49469496135826,-4.27552292478954,
79.3436161146189));
#54240=CARTESIAN_POINT('Ctrl Pts',(-1.08184975726055,-5.09989408916944,
79.3965363687009));
#54241=CARTESIAN_POINT('Ctrl Pts',(0.780026823868144,-5.15469463422192,
79.4494566227829));
#54242=CARTESIAN_POINT('Ctrl Pts',(2.23891162262289,-4.41484699357874,79.5023768768648));
#54243=CARTESIAN_POINT('Ctrl Pts',(3.69779642137764,-3.67499935293556,79.5552971309468));
#54244=CARTESIAN_POINT('Ctrl Pts',(4.75368943775855,-2.14050352659667,79.6082173850287));
#54245=CARTESIAN_POINT('Ctrl Pts',(4.92339790113362,-0.51356824058747,79.6611376391107));
#54246=CARTESIAN_POINT('Ctrl Pts',(5.0931063645087,1.11336704542182,79.7140578931926));
#54247=CARTESIAN_POINT('Ctrl Pts',(4.37663027487802,2.83274179110132,79.7669781472746));
#54248=CARTESIAN_POINT('Ctrl Pts',(3.10184003337994,3.85774385333563,79.8198984013566));
#54249=CARTESIAN_POINT('Ctrl Pts',(1.82704979188194,4.88274591556987,79.8728186554386));
#54250=CARTESIAN_POINT('Ctrl Pts',(-0.00605460148340203,5.21337529435879,
79.9257389095204));
#54251=CARTESIAN_POINT('Ctrl Pts',(-1.55861657986055,4.69833093636568,79.9786591636024));
#54252=CARTESIAN_POINT('Ctrl Pts',(-3.11117855823778,4.18328657837255,80.0315794176844));
#54253=CARTESIAN_POINT('Ctrl Pts',(-4.38319812162688,2.82256848359726,80.0844996717665));
#54254=CARTESIAN_POINT('Ctrl Pts',(-4.79257969064933,1.23886203404666,80.1374199258484));
#54255=CARTESIAN_POINT('Ctrl Pts',(-4.89639341618109,0.837255124705079,
80.1508397990133));
#54256=CARTESIAN_POINT('Ctrl Pts',(-4.94473415317796,0.421308677192607,
80.1642596721782));
#54257=CARTESIAN_POINT('Ctrl Pts',(-4.94098429374081,0.00450501606805162,
80.1776795453432));
#54258=CARTESIAN_POINT('Origin',(0.,0.,16.));
#54259=CARTESIAN_POINT('',(-4.93407925753408,-0.000975201913082646,81.3223204546568));
#54260=CARTESIAN_POINT('',(-4.93426916398102,-0.00139536187133696,81.1776795453431));
#54261=CARTESIAN_POINT('',(-4.942,-6.05220448138622E-16,16.));
#54262=CARTESIAN_POINT('Ctrl Pts',(-4.93407925753408,-0.000975201913082646,
81.3223204546568));
#54263=CARTESIAN_POINT('Ctrl Pts',(-4.93251895945243,0.883617373199263,
81.2939393473123));
#54264=CARTESIAN_POINT('Ctrl Pts',(-4.70573849196771,1.76895636928203,81.2655582399678));
#54265=CARTESIAN_POINT('Ctrl Pts',(-4.25849767807825,2.52364737255269,81.2371771326233));
#54266=CARTESIAN_POINT('Ctrl Pts',(-3.42455919852679,3.93086658925474,81.1842568785413));
#54267=CARTESIAN_POINT('Ctrl Pts',(-1.8241145504932,4.88384315405391,81.1313366244594));
#54268=CARTESIAN_POINT('Ctrl Pts',(-0.189551647970844,4.94648043642473,
81.0784163703775));
#54269=CARTESIAN_POINT('Ctrl Pts',(1.44501125455142,5.00911771879556,81.0254961162955));
#54270=CARTESIAN_POINT('Ctrl Pts',(3.11369241156233,4.18141571873815,80.9725758622135));
#54271=CARTESIAN_POINT('Ctrl Pts',(4.05287784031979,2.84214351269564,80.9196556081315));
#54272=CARTESIAN_POINT('Ctrl Pts',(4.99206326907725,1.50287130665312,80.8667353540495));
#54273=CARTESIAN_POINT('Ctrl Pts',(5.20175296958118,-0.347971105374417,
80.8138150999676));
#54274=CARTESIAN_POINT('Ctrl Pts',(4.58598973236862,-1.86340996827063,80.7608948458856));
#54275=CARTESIAN_POINT('Ctrl Pts',(3.97022649515609,-3.37884883116675,80.7079745918037));
#54276=CARTESIAN_POINT('Ctrl Pts',(2.52901032022692,-4.5588841449317,80.6550543377218));
#54277=CARTESIAN_POINT('Ctrl Pts',(0.92186374048162,-4.86351372766964,80.6021340836398));
#54278=CARTESIAN_POINT('Ctrl Pts',(-0.685282839263774,-5.16814331040758,
80.5492138295578));
#54279=CARTESIAN_POINT('Ctrl Pts',(-2.45835982382543,-4.59736716211862,
80.4962935754758));
#54280=CARTESIAN_POINT('Ctrl Pts',(-3.58598010539301,-3.41238116554821,
80.4433733213938));
#54281=CARTESIAN_POINT('Ctrl Pts',(-4.44577484147009,-2.5088458719475,80.4030223658148));
#54282=CARTESIAN_POINT('Ctrl Pts',(-4.93031074601031,-1.24821819877227,
80.3626714102358));
#54283=CARTESIAN_POINT('Ctrl Pts',(-4.94177616066966,0.00451715357047341,
80.3223204546568));
#54284=CARTESIAN_POINT('Ctrl Pts',(-4.94098429374081,0.00450501606805162,
80.1776795453432));
#54285=CARTESIAN_POINT('Ctrl Pts',(-4.92994686631264,-1.22232501277905,
80.2171799262602));
#54286=CARTESIAN_POINT('Ctrl Pts',(-4.46760970741441,-2.45658172320469,
80.2566803071772));
#54287=CARTESIAN_POINT('Ctrl Pts',(-3.64022747730309,-3.35445124336543,
80.2961806880942));
#54288=CARTESIAN_POINT('Ctrl Pts',(-2.53175012027843,-4.55736326690124,
80.3491009421762));
#54289=CARTESIAN_POINT('Ctrl Pts',(-0.768051831573162,-5.1564925096469,
80.4020211962582));
#54290=CARTESIAN_POINT('Ctrl Pts',(0.843772115467599,-4.87766827980189,
80.4549414503402));
#54291=CARTESIAN_POINT('Ctrl Pts',(2.45559606250818,-4.59884404995691,80.5078617044222));
#54292=CARTESIAN_POINT('Ctrl Pts',(3.91554566788429,-3.4420663475215,80.5607819585041));
#54293=CARTESIAN_POINT('Ctrl Pts',(4.55552569480652,-1.93669431624669,80.613702212586));
#54294=CARTESIAN_POINT('Ctrl Pts',(5.19550572172878,-0.431322284971791,
80.666622466668));
#54295=CARTESIAN_POINT('Ctrl Pts',(5.01551617019705,1.42264407514254,80.71954272075));
#54296=CARTESIAN_POINT('Ctrl Pts',(4.09792300791601,2.7768014426365,80.7724629748319));
#54297=CARTESIAN_POINT('Ctrl Pts',(3.18032984563491,4.13095881013054,80.8253832289139));
#54298=CARTESIAN_POINT('Ctrl Pts',(1.52513307260442,4.98530718500416,80.8783034829959));
#54299=CARTESIAN_POINT('Ctrl Pts',(-0.110223988510079,4.94888370271273,
80.9312237370779));
#54300=CARTESIAN_POINT('Ctrl Pts',(-1.74558104962448,4.9124602204213,80.9841439911598));
#54301=CARTESIAN_POINT('Ctrl Pts',(-3.36109839882289,3.98526488096493,81.0370642452417));
#54302=CARTESIAN_POINT('Ctrl Pts',(-4.21749062381118,2.59159643244825,81.0899844993237));
#54303=CARTESIAN_POINT('Ctrl Pts',(-4.69053795942863,1.82177259814856,81.1192161813301));
#54304=CARTESIAN_POINT('Ctrl Pts',(-4.93196472022524,0.909620752018895,
81.1484478633366));
#54305=CARTESIAN_POINT('Ctrl Pts',(-4.93426916398102,-0.00139536187133696,
81.1776795453431));
#54306=CARTESIAN_POINT('Origin',(0.,0.,16.));
#54307=CARTESIAN_POINT('',(-4.94535283272668,-0.00400458364991862,82.3223204546568));
#54308=CARTESIAN_POINT('',(-4.94609777444767,-0.00376784846301249,82.1776795453432));
#54309=CARTESIAN_POINT('',(-4.942,-6.05220448138622E-16,16.));
#54310=CARTESIAN_POINT('Ctrl Pts',(-4.94535283272668,-0.00400458364991862,
82.3223204546568));
#54311=CARTESIAN_POINT('Ctrl Pts',(-4.93330953662462,1.36545649397123,82.2781275384708));
#54312=CARTESIAN_POINT('Ctrl Pts',(-4.34046622285376,2.74406818932791,82.2339346222847));
#54313=CARTESIAN_POINT('Ctrl Pts',(-3.32967465270896,3.66290393572493,82.1897417060986));
#54314=CARTESIAN_POINT('Ctrl Pts',(-2.11926920015238,4.76319387708596,82.1368214520167));
#54315=CARTESIAN_POINT('Ctrl Pts',(-0.309540619040862,5.20418124698654,
82.0839011979348));
#54316=CARTESIAN_POINT('Ctrl Pts',(1.27135165523017,4.78406349239674,82.0309809438528));
#54317=CARTESIAN_POINT('Ctrl Pts',(2.85224392950138,4.3639457378069,81.9780606897708));
#54318=CARTESIAN_POINT('Ctrl Pts',(4.20429989693216,3.08272285872646,81.9251404356888));
#54319=CARTESIAN_POINT('Ctrl Pts',(4.7087980958408,1.52670201104665,81.8722201816068));
#54320=CARTESIAN_POINT('Ctrl Pts',(5.21329629474935,-0.0293188366329011,
81.8192999275248));
#54321=CARTESIAN_POINT('Ctrl Pts',(4.87023672513615,-1.86013765291182,81.7663796734429));
#54322=CARTESIAN_POINT('Ctrl Pts',(3.83660868625431,-3.12794378523385,81.713459419361));
#54323=CARTESIAN_POINT('Ctrl Pts',(2.80298064737236,-4.39574991755603,81.660539165279));
#54324=CARTESIAN_POINT('Ctrl Pts',(1.07878413922189,-5.10054336592114,81.607618911197));
#54325=CARTESIAN_POINT('Ctrl Pts',(-0.546962183326737,-4.91979988461579,
81.554698657115));
#54326=CARTESIAN_POINT('Ctrl Pts',(-2.17270850587518,-4.73905640331046,
81.5017784030331));
#54327=CARTESIAN_POINT('Ctrl Pts',(-3.70000464282163,-3.6727759923347,81.4488581489512));
#54328=CARTESIAN_POINT('Ctrl Pts',(-4.42993655576027,-2.20890485254455,
81.3959378948692));
#54329=CARTESIAN_POINT('Ctrl Pts',(-4.7684063275082,-1.53010711570026,81.3713987481318));
#54330=CARTESIAN_POINT('Ctrl Pts',(-4.93542833750884,-0.765820165151225,
81.3468596013943));
#54331=CARTESIAN_POINT('Ctrl Pts',(-4.93407925753408,-0.000975201913082646,
81.3223204546568));
#54332=CARTESIAN_POINT('Ctrl Pts',(-4.93426916398102,-0.00139536187133696,
81.1776795453431));
#54333=CARTESIAN_POINT('Ctrl Pts',(-4.93613662347209,-0.739658417382295,
81.2013681174186));
#54334=CARTESIAN_POINT('Ctrl Pts',(-4.78097132279663,-1.47717563214288,
81.2250566894941));
#54335=CARTESIAN_POINT('Ctrl Pts',(-4.46478101528126,-2.13759905414229,
81.2487452615696));
#54336=CARTESIAN_POINT('Ctrl Pts',(-3.75841208098482,-3.61298453463955,
81.3016655156515));
#54337=CARTESIAN_POINT('Ctrl Pts',(-2.24840711161364,-4.7036139380569,81.3545857697334));
#54338=CARTESIAN_POINT('Ctrl Pts',(-0.625767443036273,-4.91039859255742,
81.4075060238154));
#54339=CARTESIAN_POINT('Ctrl Pts',(0.996872225541001,-5.11718324705793,
81.4604262778974));
#54340=CARTESIAN_POINT('Ctrl Pts',(2.73214659332435,-4.44012315264172,81.5133465319795));
#54341=CARTESIAN_POINT('Ctrl Pts',(3.7859676073568,-3.18905134900772,81.5662667860614));
#54342=CARTESIAN_POINT('Ctrl Pts',(4.83978862138919,-1.9379795453738,81.6191870401434));
#54343=CARTESIAN_POINT('Ctrl Pts',(5.21215628167071,-0.112896032521955,
81.6721072942252));
#54344=CARTESIAN_POINT('Ctrl Pts',(4.7326694596758,1.45101310003748,81.7250275483072));
#54345=CARTESIAN_POINT('Ctrl Pts',(4.25318263768082,3.01492223259719,81.7779478023891));
#54346=CARTESIAN_POINT('Ctrl Pts',(2.92184133340926,4.31765698486456,81.8308680564712));
#54347=CARTESIAN_POINT('Ctrl Pts',(1.34788766110338,4.7630660380761,81.8837883105532));
#54348=CARTESIAN_POINT('Ctrl Pts',(-0.226066011202234,5.20847509128757,
81.9367085646351));
#54349=CARTESIAN_POINT('Ctrl Pts',(-2.04263205154196,4.79655844544351,81.989628818717));
#54350=CARTESIAN_POINT('Ctrl Pts',(-3.27052209643622,3.71581544847434,82.042549072799));
#54351=CARTESIAN_POINT('Ctrl Pts',(-4.31565037405029,2.79593253903751,82.087592563647));
#54352=CARTESIAN_POINT('Ctrl Pts',(-4.93430071630666,1.39150518826543,82.1326360544951));
#54353=CARTESIAN_POINT('Ctrl Pts',(-4.94609777444767,-0.00376784846301249,
82.1776795453432));
#54354=CARTESIAN_POINT('Origin',(0.,0.,16.));
#54355=CARTESIAN_POINT('',(-4.94676006163664,0.00350952918951444,83.3223204546568));
#54356=CARTESIAN_POINT('',(-4.94604776483535,0.00378542647206983,83.1776795453431));
#54357=CARTESIAN_POINT('',(-4.942,-6.05220448138622E-16,16.));
#54358=CARTESIAN_POINT('Ctrl Pts',(-4.94676006163664,0.00350952918951444,
83.3223204546568));
#54359=CARTESIAN_POINT('Ctrl Pts',(-4.94852531327494,0.222882433779423,
83.3152359837111));
#54360=CARTESIAN_POINT('Ctrl Pts',(-4.93519531289187,0.442039477932862,
83.3081515127655));
#54361=CARTESIAN_POINT('Ctrl Pts',(-4.90603966821321,0.659070530865341,
83.3010670418199));
#54362=CARTESIAN_POINT('Ctrl Pts',(-4.68825006385762,2.28026970762846,83.2481467877379));
#54363=CARTESIAN_POINT('Ctrl Pts',(-3.58740009065817,3.78283999594482,83.1952265336559));
#54364=CARTESIAN_POINT('Ctrl Pts',(-2.10725577029135,4.47918204688364,83.1423062795739));
#54365=CARTESIAN_POINT('Ctrl Pts',(-0.627111449924431,5.1755240978225,83.089386025492));
#54366=CARTESIAN_POINT('Ctrl Pts',(1.23232721760991,5.06563791138373,83.0364657714101));
#54367=CARTESIAN_POINT('Ctrl Pts',(2.62015283567102,4.19980920832437,82.9835455173281));
#54368=CARTESIAN_POINT('Ctrl Pts',(4.00797845373196,3.33398050526512,82.9306252632462));
#54369=CARTESIAN_POINT('Ctrl Pts',(4.9241910223198,1.71220928558549,82.8777050091641));
#54370=CARTESIAN_POINT('Ctrl Pts',(4.94951760585997,0.0766427637077434,
82.8247847550821));
#54371=CARTESIAN_POINT('Ctrl Pts',(4.97484418940015,-1.55892375817019,82.7718645010002));
#54372=CARTESIAN_POINT('Ctrl Pts',(4.10928478789245,-3.20828558224624,82.7189442469183));
#54373=CARTESIAN_POINT('Ctrl Pts',(2.74893264004429,-4.11666951392571,82.6660239928363));
#54374=CARTESIAN_POINT('Ctrl Pts',(1.38858049219621,-5.02505344560512,82.6131037387543));
#54375=CARTESIAN_POINT('Ctrl Pts',(-0.466564401992278,-5.19245948488802,
82.5601834846723));
#54376=CARTESIAN_POINT('Ctrl Pts',(-1.96755942526789,-4.5422800890475,82.5072632305904));
#54377=CARTESIAN_POINT('Ctrl Pts',(-3.4685544485435,-3.89210069320699,82.4543429765084));
#54378=CARTESIAN_POINT('Ctrl Pts',(-4.61539960090623,-2.42433586224305,
82.4014227224265));
#54379=CARTESIAN_POINT('Ctrl Pts',(-4.88328101508674,-0.810657190350331,
82.3485024683445));
#54380=CARTESIAN_POINT('Ctrl Pts',(-4.92745864911638,-0.544537549215846,
82.3397751304486));
#54381=CARTESIAN_POINT('Ctrl Pts',(-4.94773117576294,-0.274449500871191,
82.3310477925527));
#54382=CARTESIAN_POINT('Ctrl Pts',(-4.94535283272668,-0.00400458364991862,
82.3223204546568));
#54383=CARTESIAN_POINT('Ctrl Pts',(-4.94609777444767,-0.00376784846301249,
82.1776795453432));
#54384=CARTESIAN_POINT('Ctrl Pts',(-4.94816072809722,-0.247759491874606,
82.1855563085771));
#54385=CARTESIAN_POINT('Ctrl Pts',(-4.93166636384428,-0.49147120021732,
82.193433071811));
#54386=CARTESIAN_POINT('Ctrl Pts',(-4.89565013237716,-0.732262940926013,
82.201309835045));
#54387=CARTESIAN_POINT('Ctrl Pts',(-4.65367407397507,-2.35002898526266,
82.2542300891269));
#54388=CARTESIAN_POINT('Ctrl Pts',(-3.53050790772224,-3.83599172584166,
82.3071503432088));
#54389=CARTESIAN_POINT('Ctrl Pts',(-2.04012962670993,-4.51015191896435,
82.3600705972908));
#54390=CARTESIAN_POINT('Ctrl Pts',(-0.549751345697456,-5.18431211208712,
82.4129908513727));
#54391=CARTESIAN_POINT('Ctrl Pts',(1.3078390500746,-5.04666975775335,82.4659111054547));
#54392=CARTESIAN_POINT('Ctrl Pts',(2.68257982821446,-4.16021209746218,82.5188313595367));
#54393=CARTESIAN_POINT('Ctrl Pts',(4.05732060635432,-3.273754437171,82.5717516136187));
#54394=CARTESIAN_POINT('Ctrl Pts',(4.94921176686199,-1.63848147092241,82.6246718677007));
#54395=CARTESIAN_POINT('Ctrl Pts',(4.95011028710458,-0.00271908696136483,
82.6775921217826));
#54396=CARTESIAN_POINT('Ctrl Pts',(4.95100880734717,1.63304329699958,82.7305123758646));
#54397=CARTESIAN_POINT('Ctrl Pts',(4.06091468732478,3.26929509867298,82.7834326299465));
#54398=CARTESIAN_POINT('Ctrl Pts',(2.68714860199004,4.15726251102139,82.8363528840285));
#54399=CARTESIAN_POINT('Ctrl Pts',(1.31338251665521,5.04522992336985,82.8892731381104));
#54400=CARTESIAN_POINT('Ctrl Pts',(-0.544055533992037,5.18491294639323,
82.9421933921924));
#54401=CARTESIAN_POINT('Ctrl Pts',(-2.0351735518924,4.51239048126625,82.9951136462744));
#54402=CARTESIAN_POINT('Ctrl Pts',(-3.52629156979259,3.83986801613934,83.0480339003563));
#54403=CARTESIAN_POINT('Ctrl Pts',(-4.651089554946,2.35514006286229,83.1009541544383));
#54404=CARTESIAN_POINT('Ctrl Pts',(-4.8948427284911,0.737640835765265,83.1538744085202));
#54405=CARTESIAN_POINT('Ctrl Pts',(-4.9313919209059,0.495107417134616,83.1618094541278));
#54406=CARTESIAN_POINT('Ctrl Pts',(-4.94813254848979,0.249588896780995,
83.1697444997355));
#54407=CARTESIAN_POINT('Ctrl Pts',(-4.94604776483535,0.00378542647206983,
83.1776795453431));
#54408=CARTESIAN_POINT('Origin',(0.,0.,16.));
#54409=CARTESIAN_POINT('',(-4.93450205841395,0.0017791821159216,84.3223204546568));
#54410=CARTESIAN_POINT('',(-4.93425329604086,0.00136738585504144,84.1776795453431));
#54411=CARTESIAN_POINT('',(-4.942,-6.05220448138622E-16,16.));
#54412=CARTESIAN_POINT('Ctrl Pts',(-4.93450205841395,0.0017791821159216,
84.3223204546568));
#54413=CARTESIAN_POINT('Ctrl Pts',(-4.9368080070955,0.715261896051447,84.2994241748696));
#54414=CARTESIAN_POINT('Ctrl Pts',(-4.79225594661696,1.42785481900567,84.2765278950824));
#54415=CARTESIAN_POINT('Ctrl Pts',(-4.49620929648531,2.07068108576527,84.2536316152951));
#54416=CARTESIAN_POINT('Ctrl Pts',(-3.81195560589931,3.55644775544483,84.2007113612132));
#54417=CARTESIAN_POINT('Ctrl Pts',(-2.31839897625278,4.66951227096791,84.1477911071313));
#54418=CARTESIAN_POINT('Ctrl Pts',(-0.699026613519106,4.90050762812279,
84.0948708530493));
#54419=CARTESIAN_POINT('Ctrl Pts',(0.92034574921447,5.13150298527765,84.0419505989674));
#54420=CARTESIAN_POINT('Ctrl Pts',(2.66553384503535,4.48042918406423,83.9890303448854));
#54421=CARTESIAN_POINT('Ctrl Pts',(3.73791967339092,3.24523363926685,83.9361100908034));
#54422=CARTESIAN_POINT('Ctrl Pts',(4.81030550174656,2.01003809446939,83.8831898367214));
#54423=CARTESIAN_POINT('Ctrl Pts',(5.20988906263709,0.190720806087873,83.8302695826395));
#54424=CARTESIAN_POINT('Ctrl Pts',(4.75381130414694,-1.38017403364147,83.7773493285575));
#54425=CARTESIAN_POINT('Ctrl Pts',(4.29773354565674,-2.951068873371,83.7244290744756));
#54426=CARTESIAN_POINT('Ctrl Pts',(2.9859944677857,-4.27354126444818,83.6715088203937));
#54427=CARTESIAN_POINT('Ctrl Pts',(1.41886773993217,-4.74240598011873,83.6185885663117));
#54428=CARTESIAN_POINT('Ctrl Pts',(-0.148258987921171,-5.21127069578923,
83.5656683122296));
#54429=CARTESIAN_POINT('Ctrl Pts',(-1.97077336575683,-4.82652773605328,
83.5127480581476));
#54430=CARTESIAN_POINT('Ctrl Pts',(-3.21466593691877,-3.76424222358033,
83.4598278040656));
#54431=CARTESIAN_POINT('Ctrl Pts',(-4.29203775090064,-2.84416560597453,
83.4139920209293));
#54432=CARTESIAN_POINT('Ctrl Pts',(-4.93533906889132,-1.41581012896607,
83.3681562377931));
#54433=CARTESIAN_POINT('Ctrl Pts',(-4.94676006163664,0.00350952918951444,
83.3223204546568));
#54434=CARTESIAN_POINT('Ctrl Pts',(-4.94604776483535,0.00378542647206983,
83.1776795453431));
#54435=CARTESIAN_POINT('Ctrl Pts',(-4.93422874929891,-1.38971889629444,
83.2226647538174));
#54436=CARTESIAN_POINT('Ctrl Pts',(-4.31736833349613,-2.79238139987207,
83.2676499622918));
#54437=CARTESIAN_POINT('Ctrl Pts',(-3.27460228178232,-3.71222020633235,
83.3126351707661));
#54438=CARTESIAN_POINT('Ctrl Pts',(-2.04790029959144,-4.7943115204161,83.3655554248481));
#54439=CARTESIAN_POINT('Ctrl Pts',(-0.231787973272793,-5.20822364766616,
83.4184756789301));
#54440=CARTESIAN_POINT('Ctrl Pts',(1.34265411435701,-4.76454397765274,83.4713959330121));
#54441=CARTESIAN_POINT('Ctrl Pts',(2.91709620198673,-4.32086430763936,83.524316187094));
#54442=CARTESIAN_POINT('Ctrl Pts',(4.24986805092773,-3.01959284036256,83.577236441176));
#54443=CARTESIAN_POINT('Ctrl Pts',(4.73107261188716,-1.45621146364564,83.630156695258));
#54444=CARTESIAN_POINT('Ctrl Pts',(5.21227717284655,0.107169913071196,83.6830769493399));
#54445=CARTESIAN_POINT('Ctrl Pts',(4.84191444582465,1.93266119922796,83.7359972034218));
#54446=CARTESIAN_POINT('Ctrl Pts',(3.78946863845564,3.18489006691465,83.7889174575038));
#54447=CARTESIAN_POINT('Ctrl Pts',(2.73702283108663,4.43711893460135,83.8418377115857));
#54448=CARTESIAN_POINT('Ctrl Pts',(1.00249394337044,5.11608538381779,83.8947579656677));
#54449=CARTESIAN_POINT('Ctrl Pts',(-0.620372201325573,4.91108329901265,
83.9476782197497));
#54450=CARTESIAN_POINT('Ctrl Pts',(-2.24323834602159,4.70608121420751,84.0005984738317));
#54451=CARTESIAN_POINT('Ctrl Pts',(-3.75444174769753,3.6171105953808,84.0535187279136));
#54452=CARTESIAN_POINT('Ctrl Pts',(-4.4624305684118,2.14250236754745,84.1064389819956));
#54453=CARTESIAN_POINT('Ctrl Pts',(-4.78012570742429,1.48080284317098,84.1301858364447));
#54454=CARTESIAN_POINT('Ctrl Pts',(-4.93608736949663,0.741452199377731,
84.1539326908939));
#54455=CARTESIAN_POINT('Ctrl Pts',(-4.93425329604086,0.00136738585504144,
84.1776795453431));
#54456=CARTESIAN_POINT('Origin',(0.,0.,16.));
#54457=CARTESIAN_POINT('',(-4.93983901057914,-0.00407131671605609,85.3223204546568));
#54458=CARTESIAN_POINT('',(-4.94096920053978,-0.0044629540342261,85.1776795453431));
#54459=CARTESIAN_POINT('',(-4.942,-6.05220448138622E-16,16.));
#54460=CARTESIAN_POINT('Ctrl Pts',(-4.93983901057914,-0.00407131671605609,
85.3223204546568));
#54461=CARTESIAN_POINT('Ctrl Pts',(-4.92935782359351,1.19852489561668,85.283612366028));
#54462=CARTESIAN_POINT('Ctrl Pts',(-4.48753687762877,2.40778661262928,85.2449042773993));
#54463=CARTESIAN_POINT('Ctrl Pts',(-3.69010132050912,3.2995468819145,85.2061961887705));
#54464=CARTESIAN_POINT('Ctrl Pts',(-2.59987718928131,4.51872823916,85.1532759346885));
#54465=CARTESIAN_POINT('Ctrl Pts',(-0.844961773498813,5.14445691330988,
85.1003556806066));
#54466=CARTESIAN_POINT('Ctrl Pts',(0.770932612771407,4.88981272332166,85.0474354265247));
#54467=CARTESIAN_POINT('Ctrl Pts',(2.38682699904172,4.63516853333343,84.9945151724427));
#54468=CARTESIAN_POINT('Ctrl Pts',(3.86370035579973,3.500151479207,84.9415949183607));
#54469=CARTESIAN_POINT('Ctrl Pts',(4.52604489048226,2.00446382425534,84.8886746642787));
#54470=CARTESIAN_POINT('Ctrl Pts',(5.18838942516471,0.508776169303851,84.8357544101967));
#54471=CARTESIAN_POINT('Ctrl Pts',(5.0362051377719,-1.34758208647277,84.7828341561149));
#54472=CARTESIAN_POINT('Ctrl Pts',(4.13896054991356,-2.7152702523835,84.7299139020329));
#54473=CARTESIAN_POINT('Ctrl Pts',(3.24171596205511,-4.08295841829439,84.6769936479509));
#54474=CARTESIAN_POINT('Ctrl Pts',(1.59941107373096,-4.96197649433929,84.6240733938688));
#54475=CARTESIAN_POINT('Ctrl Pts',(-0.0363198163526684,-4.94999030922869,
84.5711531397869));
#54476=CARTESIAN_POINT('Ctrl Pts',(-1.67205070643629,-4.93800412411811,
84.518232885705));
#54477=CARTESIAN_POINT('Ctrl Pts',(-3.30120759827939,-4.03501367785208,
84.4653126316231));
#54478=CARTESIAN_POINT('Ctrl Pts',(-4.17831066843813,-2.65428404280099,
84.4123923775412));
#54479=CARTESIAN_POINT('Ctrl Pts',(-4.67592959505013,-1.87093574279885,
84.3823684032464));
#54480=CARTESIAN_POINT('Ctrl Pts',(-4.93147825958796,-0.9338132749143,84.3523444289516));
#54481=CARTESIAN_POINT('Ctrl Pts',(-4.93450205841395,0.0017791821159216,
84.3223204546568));
#54482=CARTESIAN_POINT('Ctrl Pts',(-4.93425329604086,0.00136738585504144,
84.1776795453431));
#54483=CARTESIAN_POINT('Ctrl Pts',(-4.93200010676076,-0.907838929165127,
84.2068529449759));
#54484=CARTESIAN_POINT('Ctrl Pts',(-4.6915933103023,-1.81815329167953,84.2360263446087));
#54485=CARTESIAN_POINT('Ctrl Pts',(-4.22033403606684,-2.58696080038834,
84.2651997442415));
#54486=CARTESIAN_POINT('Ctrl Pts',(-3.36547444325506,-3.98156990365044,
84.3181199983235));
#54487=CARTESIAN_POINT('Ctrl Pts',(-1.75098101787896,-4.91054227333463,
84.3710402524054));
#54488=CARTESIAN_POINT('Ctrl Pts',(-0.115662974249316,-4.94876105553069,
84.4239605064874));
#54489=CARTESIAN_POINT('Ctrl Pts',(1.51965506938033,-4.98697983772675,84.4768807605693));
#54490=CARTESIAN_POINT('Ctrl Pts',(3.17579773126353,-4.1344450324347,84.5298010146513));
#54491=CARTESIAN_POINT('Ctrl Pts',(4.09487421234139,-2.78129899063739,84.5827212687333));
#54492=CARTESIAN_POINT('Ctrl Pts',(5.01395069341925,-1.42815294884008,84.6356415228152));
#54493=CARTESIAN_POINT('Ctrl Pts',(5.19596099369178,0.425604329462498,84.6885617768972));
#54494=CARTESIAN_POINT('Ctrl Pts',(4.55764242829978,1.93168321282745,84.7414820309791));
#54495=CARTESIAN_POINT('Ctrl Pts',(3.91932386290774,3.43776209619249,84.7944022850611));
#54496=CARTESIAN_POINT('Ctrl Pts',(2.46067643185109,4.59616258461988,84.8473225391431));
#54497=CARTESIAN_POINT('Ctrl Pts',(0.849145831707845,4.87674842560418,84.9002427932251));
#54498=CARTESIAN_POINT('Ctrl Pts',(-0.762384768435213,5.15733426658845,
84.9531630473071));
#54499=CARTESIAN_POINT('Ctrl Pts',(-2.52679853766482,4.5601054601299,85.006083301389));
#54500=CARTESIAN_POINT('Ctrl Pts',(-3.63657003853315,3.35842910333814,85.059003555471));
#54501=CARTESIAN_POINT('Ctrl Pts',(-4.46614045337841,2.46015846561364,85.0985622187617));
#54502=CARTESIAN_POINT('Ctrl Pts',(-4.92991110676884,1.22413577549367,85.1381208820524));
#54503=CARTESIAN_POINT('Ctrl Pts',(-4.94096920053978,-0.0044629540342261,
85.1776795453431));
#54504=CARTESIAN_POINT('Origin',(0.,0.,24.1514101080949));
#54505=CARTESIAN_POINT('',(-4.37008825460381,-0.00360173951420115,85.6514101080948));
#54506=CARTESIAN_POINT('',(-4.37741404908174,0.00054794132368214,85.8485898919049));
#54507=CARTESIAN_POINT('',(-4.372,3.82579154166093E-12,24.1514101080949));
#54508=CARTESIAN_POINT('',(2.54472701347433,-3.56250531650779,85.9999999999999));
#54509=CARTESIAN_POINT('Ctrl Pts',(-4.37008825460381,-0.00360173951420056,
85.6514101080948));
#54510=CARTESIAN_POINT('Ctrl Pts',(-4.37349270028371,-0.394222905349127,
85.665622273548));
#54511=CARTESIAN_POINT('Ctrl Pts',(-4.14658524106498,-2.2356015936124,85.7327546930832));
#54512=CARTESIAN_POINT('Ctrl Pts',(-1.63914477126166,-4.84388062782939,
85.8489513237184));
#54513=CARTESIAN_POINT('Ctrl Pts',(1.44818750565376,-4.33531680853971,85.9509357889001));
#54514=CARTESIAN_POINT('Ctrl Pts',(2.54472701347433,-3.56250531650779,85.9999999999999));
#54515=CARTESIAN_POINT('',(-2.53835875722777,-3.5596515025498,86.));
#54516=CARTESIAN_POINT('Origin',(0.,0.,86.));
#54517=CARTESIAN_POINT('Ctrl Pts',(-4.37741404908174,0.000547941323682409,
85.8485898919049));
#54518=CARTESIAN_POINT('Ctrl Pts',(-4.37702756934774,-0.658293262144059,
85.8725998008956));
#54519=CARTESIAN_POINT('Ctrl Pts',(-4.04502790407186,-2.04740376323306,
85.9230698369273));
#54520=CARTESIAN_POINT('Ctrl Pts',(-3.130164636136,-3.13763950664809,85.973539872959));
#54521=CARTESIAN_POINT('Ctrl Pts',(-2.53835875722777,-3.5596515025498,86.));
#54522=CARTESIAN_POINT('Origin',(0.,0.,24.1514101080949));
#54523=CARTESIAN_POINT('',(-4.3653668553998,0.00157397495328755,84.6514101080948));
#54524=CARTESIAN_POINT('',(-4.37108809080528,-0.00394820619502134,84.8485898919049));
#54525=CARTESIAN_POINT('',(-4.372,3.82579154166093E-12,24.1514101080949));
#54526=CARTESIAN_POINT('Ctrl Pts',(-4.3653668553998,0.00157397495328733,
84.6514101080948));
#54527=CARTESIAN_POINT('Ctrl Pts',(-4.36269181524081,-0.826109194237039,
84.6814340823896));
#54528=CARTESIAN_POINT('Ctrl Pts',(-3.73813921667308,-3.11640593107392,
84.7643783107663));
#54529=CARTESIAN_POINT('Ctrl Pts',(-0.0379465312430282,-5.16730640666113,
84.9002427932251));
#54530=CARTESIAN_POINT('Ctrl Pts',(4.32070804489202,-2.83440452778566,85.059003555471));
#54531=CARTESIAN_POINT('Ctrl Pts',(4.72460304963626,2.09234474027741,85.2177643177169));
#54532=CARTESIAN_POINT('Ctrl Pts',(0.805001482004623,5.10466438453535,85.3765250799626));
#54533=CARTESIAN_POINT('Ctrl Pts',(-3.43558144629758,3.5926517202867,85.5210736767555));
#54534=CARTESIAN_POINT('Ctrl Pts',(-4.3608159459227,1.06028952724385,85.6127020194661));
#54535=CARTESIAN_POINT('Ctrl Pts',(-4.37008825460381,-0.00360173951420056,
85.6514101080948));
#54536=CARTESIAN_POINT('Ctrl Pts',(-4.37108809080528,-0.00394820619502242,
84.8485898919049));
#54537=CARTESIAN_POINT('Ctrl Pts',(-4.37439235100703,-0.371064815037356,
84.8619514826962));
#54538=CARTESIAN_POINT('Ctrl Pts',(-4.16412636077677,-2.18847582560682,
84.9282333275694));
#54539=CARTESIAN_POINT('Ctrl Pts',(-1.63279460579437,-4.90302030367583,
85.0474354265246));
#54540=CARTESIAN_POINT('Ctrl Pts',(3.23428855022947,-4.03017982392474,85.2061961887705));
#54541=CARTESIAN_POINT('Ctrl Pts',(5.13873193725801,0.529582954402255,85.3649569510164));
#54542=CARTESIAN_POINT('Ctrl Pts',(2.34489518331184,4.6077777382683,85.5237177132623));
#54543=CARTESIAN_POINT('Ctrl Pts',(-2.60449736313211,4.46265913321349,85.6824784755082));
#54544=CARTESIAN_POINT('Ctrl Pts',(-4.34126539015093,1.58670061603872,85.7907692017224));
#54545=CARTESIAN_POINT('Ctrl Pts',(-4.37745348944865,0.0677828737684449,
85.8461396738546));
#54546=CARTESIAN_POINT('Ctrl Pts',(-4.37741404908174,0.000547941323682409,
85.8485898919049));
#54547=CARTESIAN_POINT('Origin',(0.,0.,24.1514101080949));
#54548=CARTESIAN_POINT('',(-4.37621104602901,0.00310474739351271,83.6514101080948));
#54549=CARTESIAN_POINT('',(-4.36514678476137,0.00120967441979231,83.8485898919049));
#54550=CARTESIAN_POINT('',(-4.372,3.82579154166093E-12,24.1514101080949));
#54551=CARTESIAN_POINT('Ctrl Pts',(-4.37621104602901,0.00310474739351276,
83.6514101080948));
#54552=CARTESIAN_POINT('Ctrl Pts',(-4.36610732682993,-1.25251353375917,
83.6972458912311));
#54553=CARTESIAN_POINT('Ctrl Pts',(-3.13993685867563,-3.97504379283746,
83.7960019284495));
#54554=CARTESIAN_POINT('Ctrl Pts',(1.4811502559097,-4.9505810809301,83.9476782197498));
#54555=CARTESIAN_POINT('Ctrl Pts',(4.96248771955931,-1.44075755171813,84.1064389819956));
#54556=CARTESIAN_POINT('Ctrl Pts',(3.90199844707087,3.38768549854763,84.2651997442416));
#54557=CARTESIAN_POINT('Ctrl Pts',(-0.729706746127024,5.11562640844579,
84.4239605064874));
#54558=CARTESIAN_POINT('Ctrl Pts',(-3.94395824097378,2.72022390956171,84.5526972944385));
#54559=CARTESIAN_POINT('Ctrl Pts',(-4.36740684075686,0.63276507679951,84.6285138283076));
#54560=CARTESIAN_POINT('Ctrl Pts',(-4.3653668553998,0.00157397495328733,
84.6514101080948));
#54561=CARTESIAN_POINT('Ctrl Pts',(-4.36514678476137,0.00120967441979238,
83.8485898919049));
#54562=CARTESIAN_POINT('Ctrl Pts',(-4.36315347364677,-0.803130675494322,
83.8777632915377));
#54563=CARTESIAN_POINT('Ctrl Pts',(-3.76467753114223,-3.06929475283447,
83.9598569452526));
#54564=CARTESIAN_POINT('Ctrl Pts',(-0.120745397495975,-5.1659971710397,
84.0948708530492));
#54565=CARTESIAN_POINT('Ctrl Pts',(4.27463443926266,-2.90338152834273,84.2536316152952));
#54566=CARTESIAN_POINT('Ctrl Pts',(4.75768727179541,2.01646478129229,84.412392377541));
#54567=CARTESIAN_POINT('Ctrl Pts',(0.886457060193665,5.09084373843816,84.571153139787));
#54568=CARTESIAN_POINT('Ctrl Pts',(-3.40216585276062,3.63920626636618,84.7165523112416));
#54569=CARTESIAN_POINT('Ctrl Pts',(-4.36130541456655,1.08294650151228,84.8090312286142));
#54570=CARTESIAN_POINT('Ctrl Pts',(-4.37108809080528,-0.00394820619502242,
84.8485898919049));
#54571=CARTESIAN_POINT('Origin',(0.,0.,24.1514101080949));
#54572=CARTESIAN_POINT('',(-4.37496612397431,-0.00354270330085218,82.6514101080948));
#54573=CARTESIAN_POINT('',(-4.37558090405915,0.00334882326136696,82.8485898919049));
#54574=CARTESIAN_POINT('',(-4.372,3.82579154166093E-12,24.1514101080949));
#54575=CARTESIAN_POINT('Ctrl Pts',(-4.37496612397431,-0.00354270330085171,
82.6514101080948));
#54576=CARTESIAN_POINT('Ctrl Pts',(-4.37707015387208,-0.242795066330439,
82.6601374459907));
#54577=CARTESIAN_POINT('Ctrl Pts',(-4.25038678075279,-1.93057999813071,
82.7217850379685));
#54578=CARTESIAN_POINT('Ctrl Pts',(-2.05392817541576,-4.74166978382725,
82.8363528840287));
#54579=CARTESIAN_POINT('Ctrl Pts',(2.86960084768762,-4.29737645901297,82.9951136462743));
#54580=CARTESIAN_POINT('Ctrl Pts',(5.16678358952832,0.0800071275065655,
83.1538744085204));
#54581=CARTESIAN_POINT('Ctrl Pts',(2.73516803922529,4.38416562959496,83.312635170766));
#54582=CARTESIAN_POINT('Ctrl Pts',(-2.19975659925683,4.67580205641259,83.4713959330121));
#54583=CARTESIAN_POINT('Ctrl Pts',(-4.27789107195956,1.83931825768632,83.5843209121216));
#54584=CARTESIAN_POINT('Ctrl Pts',(-4.37777269721528,0.197175637492073,
83.6443256371492));
#54585=CARTESIAN_POINT('Ctrl Pts',(-4.37621104602901,0.00310474739351276,
83.6514101080948));
#54586=CARTESIAN_POINT('Ctrl Pts',(-4.37558090405915,0.0033488232613671,
82.8485898919049));
#54587=CARTESIAN_POINT('Ctrl Pts',(-4.36512506919086,-1.22943160958811,
82.8935751003793));
#54588=CARTESIAN_POINT('Ctrl Pts',(-3.17743944272853,-3.93007838737006,
82.9914805629356));
#54589=CARTESIAN_POINT('Ctrl Pts',(1.40159167776471,-4.9736903294079,83.142306279574));
#54590=CARTESIAN_POINT('Ctrl Pts',(4.93874982643145,-1.52013376024582,83.3010670418199));
#54591=CARTESIAN_POINT('Ctrl Pts',(3.95581224496304,3.32469499516411,83.4598278040656));
#54592=CARTESIAN_POINT('Ctrl Pts',(-0.647603556591826,5.12666260907039,
83.6185885663118));
#54593=CARTESIAN_POINT('Ctrl Pts',(-3.92132004033239,2.76762804019117,83.7481759289246));
#54594=CARTESIAN_POINT('Ctrl Pts',(-4.36676931999915,0.655934645021535,
83.8248430374557));
#54595=CARTESIAN_POINT('Ctrl Pts',(-4.36514678476137,0.00120967441979238,
83.8485898919049));
#54596=CARTESIAN_POINT('Origin',(0.,0.,24.1514101080949));
#54597=CARTESIAN_POINT('',(-4.36499281949393,-0.000862724152283187,81.6514101080949));
#54598=CARTESIAN_POINT('',(-4.37562514566675,-0.00333327265474082,81.8485898919049));
#54599=CARTESIAN_POINT('',(-4.372,3.82579154166093E-12,24.1514101080949));
#54600=CARTESIAN_POINT('Ctrl Pts',(-4.36499281949393,-0.000862724152282945,
81.6514101080949));
#54601=CARTESIAN_POINT('Ctrl Pts',(-4.36618629939077,-0.677492060307118,
81.6759492548323));
#54602=CARTESIAN_POINT('Ctrl Pts',(-3.8997785113075,-2.81175799367349,81.7534086556517));
#54603=CARTESIAN_POINT('Ctrl Pts',(-0.57097184883837,-5.13576134197884,
81.8837883105532));
#54604=CARTESIAN_POINT('Ctrl Pts',(4.00502195951943,-3.26524922770216,82.0425490727989));
#54605=CARTESIAN_POINT('Ctrl Pts',(4.91549733690694,1.59371871934676,82.2013098350451));
#54606=CARTESIAN_POINT('Ctrl Pts',(1.32715940311121,4.99406661129702,82.3600705972907));
#54607=CARTESIAN_POINT('Ctrl Pts',(-3.21180689907642,3.88802958864094,82.510104021641));
#54608=CARTESIAN_POINT('Ctrl Pts',(-4.36431187659278,1.20796758228371,82.6072171919088));
#54609=CARTESIAN_POINT('Ctrl Pts',(-4.37496612397431,-0.00354270330085171,
82.6514101080948));
#54610=CARTESIAN_POINT('Ctrl Pts',(-4.37562514566675,-0.00333327265474043,
81.8485898919049));
#54611=CARTESIAN_POINT('Ctrl Pts',(-4.37745016253379,-0.219183427450699,
81.8564666551388));
#54612=CARTESIAN_POINT('Ctrl Pts',(-4.26482187642182,-1.88331740650866,
81.9172636724547));
#54613=CARTESIAN_POINT('Ctrl Pts',(-2.12968395259116,-4.7081313086182,82.0309809438528));
#54614=CARTESIAN_POINT('Ctrl Pts',(2.80033539806548,-4.3428303941221,82.1897417060986));
#54615=CARTESIAN_POINT('Ctrl Pts',(5.16740226597732,-0.00283844241944707,
82.3485024683445));
#54616=CARTESIAN_POINT('Ctrl Pts',(2.80510471878759,4.33975132503298,82.5072632305904));
#54617=CARTESIAN_POINT('Ctrl Pts',(-2.12451031000386,4.71046814615349,82.6660239928362));
#54618=CARTESIAN_POINT('Ctrl Pts',(-4.26384621089875,1.88655500314254,82.7797995466078));
#54619=CARTESIAN_POINT('Ctrl Pts',(-4.37742523310327,0.220801832606586,
82.8406548462974));
#54620=CARTESIAN_POINT('Ctrl Pts',(-4.37558090405915,0.0033488232613671,
82.8485898919049));
#54621=CARTESIAN_POINT('Origin',(0.,0.,24.1514101080949));
#54622=CARTESIAN_POINT('',(-4.37180197783241,0.00399615447510604,80.6514101080948));
#54623=CARTESIAN_POINT('',(-4.3651608225263,-0.00123442373144794,80.8485898919049));
#54624=CARTESIAN_POINT('',(-4.372,3.82579154166093E-12,24.1514101080949));
#54625=CARTESIAN_POINT('Ctrl Pts',(-4.37180197783241,0.00399615447510625,
80.6514101080948));
#54626=CARTESIAN_POINT('Ctrl Pts',(-4.36165896025063,-1.10425130818043,
80.6917610636739));
#54627=CARTESIAN_POINT('Ctrl Pts',(-3.37083349090091,-3.68210362881494,
80.7850322733349));
#54628=CARTESIAN_POINT('Ctrl Pts',(0.962330231331446,-5.07700442602626,
80.9312237370778));
#54629=CARTESIAN_POINT('Ctrl Pts',(4.78729812901886,-1.94520694012218,81.0899844993237));
#54630=CARTESIAN_POINT('Ctrl Pts',(4.2307845491307,2.96690335452649,81.2487452615696));
#54631=CARTESIAN_POINT('Ctrl Pts',(-0.19787228117179,5.16361307382143,81.4075060238155));
#54632=CARTESIAN_POINT('Ctrl Pts',(-3.78889879581372,3.02535473653369,81.541727639324));
#54633=CARTESIAN_POINT('Ctrl Pts',(-4.36361248294727,0.781702783413628,
81.6230290007504));
#54634=CARTESIAN_POINT('Ctrl Pts',(-4.36499281949393,-0.000862724152282945,
81.6514101080949));
#54635=CARTESIAN_POINT('Ctrl Pts',(-4.3651608225263,-0.00123442373144732,
80.8485898919049));
#54636=CARTESIAN_POINT('Ctrl Pts',(-4.36681289312482,-0.654347754103861,
80.8722784639804));
#54637=CARTESIAN_POINT('Ctrl Pts',(-3.92288549979199,-2.76438197736347,
80.9488872901379));
#54638=CARTESIAN_POINT('Ctrl Pts',(-0.653236375128765,-5.12594736724498,
81.0784163703773));
#54639=CARTESIAN_POINT('Ctrl Pts',(3.95215792026738,-3.32903919274863,81.2371771326234));
#54640=CARTESIAN_POINT('Ctrl Pts',(4.94041656702063,1.51470733791976,81.3959378948691));
#54641=CARTESIAN_POINT('Ctrl Pts',(1.40705506422376,4.97214744531344,81.5546986571151));
#54642=CARTESIAN_POINT('Ctrl Pts',(-3.17488990257063,3.9331654538798,81.7055826561271));
#54643=CARTESIAN_POINT('Ctrl Pts',(-4.36518873567112,1.23101187436481,81.8035464010569));
#54644=CARTESIAN_POINT('Ctrl Pts',(-4.37562514566675,-0.00333327265474043,
81.8485898919049));
#54645=CARTESIAN_POINT('Origin',(0.,0.,24.1514101080949));
#54646=CARTESIAN_POINT('',(-4.37845870912757,-0.00160159003492085,79.6514101080949));
#54647=CARTESIAN_POINT('',(-4.37110144318797,0.00398541688994905,79.8485898919049));
#54648=CARTESIAN_POINT('',(-4.372,3.82579154166093E-12,24.1514101080949));
#54649=CARTESIAN_POINT('Ctrl Pts',(-4.37845870912757,-0.00160159003492056,
79.6514101080949));
#54650=CARTESIAN_POINT('Ctrl Pts',(-4.37887661134401,-0.0903064267712891,
79.6546526184335));
#54651=CARTESIAN_POINT('Ctrl Pts',(-4.3362288360819,-1.62633270599671,79.7108153828541));
#54652=CARTESIAN_POINT('Ctrl Pts',(-2.53231305975701,-4.50438053270811,
79.8198984013567));
#54653=CARTESIAN_POINT('Ctrl Pts',(2.41077833593552,-4.57057996659486,79.9786591636024));
#54654=CARTESIAN_POINT('Ctrl Pts',(5.14745176039643,-0.453645004871452,
80.1374199258484));
#54655=CARTESIAN_POINT('Ctrl Pts',(3.1730201027819,4.07847972207792,80.2961806880942));
#54656=CARTESIAN_POINT('Ctrl Pts',(-1.70545647406065,4.87785522859546,80.4549414503402));
#54657=CARTESIAN_POINT('Ctrl Pts',(-4.17984164299754,2.14436901967187,80.573351257007));
#54658=CARTESIAN_POINT('Ctrl Pts',(-4.37496152173606,0.349214575534816,
80.6388408095919));
#54659=CARTESIAN_POINT('Ctrl Pts',(-4.37180197783241,0.00399615447510625,
80.6514101080948));
#54660=CARTESIAN_POINT('Ctrl Pts',(-4.37110144318797,0.00398541688994905,
79.8485898919049));
#54661=CARTESIAN_POINT('Ctrl Pts',(-4.36133704968111,-1.0813445883965,79.888090272822));
#54662=CARTESIAN_POINT('Ctrl Pts',(-3.40435481309659,-3.63610732924809,
79.980510907821));
#54663=CARTESIAN_POINT('Ctrl Pts',(0.880810665839244,-5.09178031191025,
80.125851796902));
#54664=CARTESIAN_POINT('Ctrl Pts',(4.75549683016874,-2.02170820645871,80.2846125591479));
#54665=CARTESIAN_POINT('Ctrl Pts',(4.27780703699033,2.89869300342805,80.4433733213939));
#54666=CARTESIAN_POINT('Ctrl Pts',(-0.11506242376767,5.16612183484124,80.6021340836397));
#54667=CARTESIAN_POINT('Ctrl Pts',(-3.76287956508864,3.07252682993506,80.7372062738101));
#54668=CARTESIAN_POINT('Ctrl Pts',(-4.36312216851904,0.804706986612936,
80.8193582098985));
#54669=CARTESIAN_POINT('Ctrl Pts',(-4.3651608225263,-0.00123442373144732,
80.8485898919049));
#54670=CARTESIAN_POINT('Origin',(0.,0.,24.1514101080949));
#54671=CARTESIAN_POINT('',(-4.36706479197461,-0.00298086264687759,78.6514101080949));
#54672=CARTESIAN_POINT('',(-4.37877376767475,-0.00119946029119966,78.8485898919049));
#54673=CARTESIAN_POINT('',(-4.372,3.82579154166093E-12,24.1514101080949));
#54674=CARTESIAN_POINT('Ctrl Pts',(-4.36706479197461,-0.00298086264687698,
78.6514101080949));
#54675=CARTESIAN_POINT('Ctrl Pts',(-4.37035845585727,-0.527750657057906,
78.670464427275));
#54676=CARTESIAN_POINT('Ctrl Pts',(-4.03993636744864,-2.50597397148776,
78.7424390005372));
#54677=CARTESIAN_POINT('Ctrl Pts',(-1.0979463908737,-5.04941255383462,78.8673338278812));
#54678=CARTESIAN_POINT('Ctrl Pts',(3.64665478912629,-3.66114220769932,79.0260945901272));
#54679=CARTESIAN_POINT('Ctrl Pts',(5.05372611759689,1.07791731796727,79.184855352373));
#54680=CARTESIAN_POINT('Ctrl Pts',(1.83547293516864,4.83043398881696,79.3436161146189));
#54681=CARTESIAN_POINT('Ctrl Pts',(-2.96262225304742,4.17564214514766,79.4991343665262));
#54682=CARTESIAN_POINT('Ctrl Pts',(-4.37205612685341,1.35742450024673,79.6017323643515));
#54683=CARTESIAN_POINT('Ctrl Pts',(-4.37845870912757,-0.00160159003492056,
79.6514101080949));
#54684=CARTESIAN_POINT('Ctrl Pts',(-4.37877376767475,-0.00119946029119964,
78.8485898919049));
#54685=CARTESIAN_POINT('Ctrl Pts',(-4.37901256877795,-0.0666227183370213,
78.8509818275816));
#54686=CARTESIAN_POINT('Ctrl Pts',(-4.34804095188971,-1.57926832145057,
78.9062940173403));
#54687=CARTESIAN_POINT('Ctrl Pts',(-2.60420306585193,-4.46320294918618,
79.0145264611808));
#54688=CARTESIAN_POINT('Ctrl Pts',(2.33719176176521,-4.60864284172174,79.1732872234268));
#54689=CARTESIAN_POINT('Ctrl Pts',(5.13951729856278,-0.536112032685121,
79.3320479856725));
#54690=CARTESIAN_POINT('Ctrl Pts',(3.23799961511593,4.02708488442023,79.4908087479186));
#54691=CARTESIAN_POINT('Ctrl Pts',(-1.62703422207133,4.90457070639472,79.6495695101643));
#54692=CARTESIAN_POINT('Ctrl Pts',(-4.16301218854004,2.19175778571074,79.7688298914932));
#54693=CARTESIAN_POINT('Ctrl Pts',(-4.37441880163748,0.372715810744746,
79.83517001874));
#54694=CARTESIAN_POINT('Ctrl Pts',(-4.37110144318797,0.00398541688994905,
79.8485898919049));
#54695=CARTESIAN_POINT('Origin',(0.,0.,24.1514101080949));
#54696=CARTESIAN_POINT('',(-4.36767022761989,0.00326609935392151,77.6514101080949));
#54697=CARTESIAN_POINT('',(-4.36757594524889,-0.00322601897944697,77.8485898919049));
#54698=CARTESIAN_POINT('',(-4.372,3.82579154166093E-12,24.1514101080949));
#54699=CARTESIAN_POINT('Ctrl Pts',(-4.36767022761989,0.00326609935392137,
77.6514101080949));
#54700=CARTESIAN_POINT('Ctrl Pts',(-4.36100748821687,-0.956637771051708,
77.6862762361166));
#54701=CARTESIAN_POINT('Ctrl Pts',(-3.57653367776381,-3.38339660944801,
77.7740626182202));
#54702=CARTESIAN_POINT('Ctrl Pts',(0.433232280173729,-5.14920995954434,
77.9147692544059));
#54703=CARTESIAN_POINT('Ctrl Pts',(4.56098553273524,-2.42888130344712,78.0735300166518));
#54704=CARTESIAN_POINT('Ctrl Pts',(4.51438550862023,2.51443371271033,78.2322907788977));
#54705=CARTESIAN_POINT('Ctrl Pts',(0.336081973315249,5.15646219061744,78.3910515411436));
#54706=CARTESIAN_POINT('Ctrl Pts',(-3.61142097688492,3.32845736892325,78.5307579842093));
#54707=CARTESIAN_POINT('Ctrl Pts',(-4.36121084329327,0.929711590329863,
78.6175441731931));
#54708=CARTESIAN_POINT('Ctrl Pts',(-4.36706479197461,-0.00298086264687698,
78.6514101080949));
#54709=CARTESIAN_POINT('Ctrl Pts',(-4.36757594524889,-0.00322601897944683,
77.8485898919049));
#54710=CARTESIAN_POINT('Ctrl Pts',(-4.37100704730013,-0.504422908173594,
77.8667936364231));
#54711=CARTESIAN_POINT('Ctrl Pts',(-4.05983800326864,-2.45852322858237,
77.9379176350233));
#54712=CARTESIAN_POINT('Ctrl Pts',(-1.17875882811733,-5.03116107861318,
78.0619618877055));
#54713=CARTESIAN_POINT('Ctrl Pts',(3.58748974126774,-3.71913585798031,78.2207226499514));
#54714=CARTESIAN_POINT('Ctrl Pts',(5.07035811814355,0.996756102360001,78.3794834121972));
#54715=CARTESIAN_POINT('Ctrl Pts',(1.91267986918918,4.80038643150889,78.5382441744432));
#54716=CARTESIAN_POINT('Ctrl Pts',(-2.92159273453857,4.2194430180671,78.6946130010123));
#54717=CARTESIAN_POINT('Ctrl Pts',(-4.37372922642899,1.38083068620526,78.7980615734996));
#54718=CARTESIAN_POINT('Ctrl Pts',(-4.37877376767475,-0.00119946029119964,
78.8485898919049));
#54719=CARTESIAN_POINT('Origin',(0.,0.,24.1514101080949));
#54720=CARTESIAN_POINT('',(-4.37882057798781,0.00112692768741051,76.6514101080949));
#54721=CARTESIAN_POINT('',(-4.36715155140556,0.00302605917446269,76.8485898919049));
#54722=CARTESIAN_POINT('',(-4.372,3.82579154166093E-12,24.1514101080949));
#54723=CARTESIAN_POINT('Ctrl Pts',(-4.37882057798781,0.00112692768741048,
76.6514101080949));
#54724=CARTESIAN_POINT('Ctrl Pts',(-4.37403747425012,-1.38495585300809,
76.7020880449581));
#54725=CARTESIAN_POINT('Ctrl Pts',(-2.91430837048911,-4.22712294708155,
76.8056862359034));
#54726=CARTESIAN_POINT('Ctrl Pts',(1.92621046639379,-4.79497306094723,76.9622046809306));
#54727=CARTESIAN_POINT('Ctrl Pts',(5.07314897115,-0.982452509068445,77.1209654431764));
#54728=CARTESIAN_POINT('Ctrl Pts',(3.5769865761566,3.7292385885125,77.2797262054224));
#54729=CARTESIAN_POINT('Ctrl Pts',(-1.19294319381297,5.02781661881079,77.4384869676682));
#54730=CARTESIAN_POINT('Ctrl Pts',(-4.06328911396928,2.45017653498889,77.5623816018925));
#54731=CARTESIAN_POINT('Ctrl Pts',(-4.37112027911439,0.500316573992826,
77.6333559820347));
#54732=CARTESIAN_POINT('Ctrl Pts',(-4.36767022761989,0.00326609935392137,
77.6514101080949));
#54733=CARTESIAN_POINT('Ctrl Pts',(-4.36715155140556,0.00302605917446276,
76.8485898919049));
#54734=CARTESIAN_POINT('Ctrl Pts',(-4.36117507900865,-0.933740289083742,
76.8826054452647));
#54735=CARTESIAN_POINT('Ctrl Pts',(-3.60625270295825,-3.33668347601213,
76.9695412527065));
#54736=CARTESIAN_POINT('Ctrl Pts',(0.350623091062388,-5.15549392607834,
77.1093973142301));
#54737=CARTESIAN_POINT('Ctrl Pts',(4.52145892049186,-2.50169210817825,77.268158076476));
#54738=CARTESIAN_POINT('Ctrl Pts',(4.55411743612604,2.44173474230699,77.4269188387219));
#54739=CARTESIAN_POINT('Ctrl Pts',(0.4187085668894,5.15041137287398,77.5856796009678));
#54740=CARTESIAN_POINT('Ctrl Pts',(-3.58180307113106,3.37518619718569,77.7262366186955));
#54741=CARTESIAN_POINT('Ctrl Pts',(-4.36103246255736,0.952610654051967,
77.8138733823412));
#54742=CARTESIAN_POINT('Ctrl Pts',(-4.36757594524889,-0.00322601897944683,
77.8485898919049));
#54743=CARTESIAN_POINT('Origin',(0.,0.,24.1514101080949));
#54744=CARTESIAN_POINT('',(-4.37097940507052,-0.00397941814148454,75.6514101080949));
#54745=CARTESIAN_POINT('',(-4.37851995085447,0.0015322273023494,75.8485898919049));
#54746=CARTESIAN_POINT('',(-4.372,3.82579154166093E-12,24.1514101080949));
#54747=CARTESIAN_POINT('Ctrl Pts',(-4.37097940507052,-0.00397941814148494,
75.6514101080949));
#54748=CARTESIAN_POINT('Ctrl Pts',(-4.3743208173595,-0.376847295339705,
75.6649795997177));
#54749=CARTESIAN_POINT('Ctrl Pts',(-4.16000539985281,-2.20009534110889,
75.7314693454226));
#54750=CARTESIAN_POINT('Ctrl Pts',(-1.61319567320764,-4.90913975519121,
75.8508793452094));
#54751=CARTESIAN_POINT('Ctrl Pts',(3.24934402869518,-4.01793688343129,76.0096401074552));
#54752=CARTESIAN_POINT('Ctrl Pts',(5.13798482303055,0.550604553524979,76.1684008697012));
#54753=CARTESIAN_POINT('Ctrl Pts',(2.32418496553848,4.61521588466023,76.3271616319469));
#54754=CARTESIAN_POINT('Ctrl Pts',(-2.61677996556865,4.45584066454958,76.485922394193));
#54755=CARTESIAN_POINT('Ctrl Pts',(-4.35007811558771,1.57099298812344,76.5940052195755));
#54756=CARTESIAN_POINT('Ctrl Pts',(-4.37903221319898,0.0624561269022633,
76.6491677908762));
#54757=CARTESIAN_POINT('Ctrl Pts',(-4.37882057798781,0.00112692768741048,
76.6514101080949));
#54758=CARTESIAN_POINT('Ctrl Pts',(-4.37851995085447,0.00153222730234961,
75.8485898919049));
#54759=CARTESIAN_POINT('Ctrl Pts',(-4.37234073616906,-1.36153629732671,
75.8984172541062));
#54760=CARTESIAN_POINT('Ctrl Pts',(-2.9554520406374,-4.18336396709743,76.0011648703895));
#54761=CARTESIAN_POINT('Ctrl Pts',(1.84908863423975,-4.82523837717284,76.1568327407549));
#54762=CARTESIAN_POINT('Ctrl Pts',(5.05674607440601,-1.06366033713594,76.3155935030006));
#54763=CARTESIAN_POINT('Ctrl Pts',(3.63631504695578,3.6714121333759,76.4743542652466));
#54764=CARTESIAN_POINT('Ctrl Pts',(-1.11218258415778,5.04629607467818,76.6331150274925));
#54765=CARTESIAN_POINT('Ctrl Pts',(-4.04347203458464,2.49762731386996,76.7578602363785));
#54766=CARTESIAN_POINT('Ctrl Pts',(-4.37047307379395,0.523649295054832,
76.8296851911827));
#54767=CARTESIAN_POINT('Ctrl Pts',(-4.36715155140556,0.00302605917446276,
76.8485898919049));
#54768=CARTESIAN_POINT('Origin',(0.,0.,24.1514101080949));
#54769=CARTESIAN_POINT('',(-4.36519646031047,0.00129875109319553,74.6514101080949));
#54770=CARTESIAN_POINT('',(-4.37167806635839,-0.00399716320838295,74.8485898919049));
#54771=CARTESIAN_POINT('',(-4.372,3.82579154166093E-12,24.1514101080949));
#54772=CARTESIAN_POINT('Ctrl Pts',(-4.36519646031047,0.00129875109319548,
74.6514101080949));
#54773=CARTESIAN_POINT('Ctrl Pts',(-4.36303959174397,-0.808751209913892,
74.6807914085593));
#54774=CARTESIAN_POINT('Ctrl Pts',(-3.75824647517972,-3.08081912741743,
74.7630929631056));
#54775=CARTESIAN_POINT('Ctrl Pts',(-0.100492272925181,-5.16642571988962,
74.898314771734));
#54776=CARTESIAN_POINT('Ctrl Pts',(4.28596496729055,-2.88661700182285,75.0570755339799));
#54777=CARTESIAN_POINT('Ctrl Pts',(4.74977615293751,2.03511176917654,75.2158362962258));
#54778=CARTESIAN_POINT('Ctrl Pts',(0.866447119614458,5.09424408572719,75.3745970584717));
#54779=CARTESIAN_POINT('Ctrl Pts',(-3.41018887347201,3.62800267766814,75.5197883290947));
#54780=CARTESIAN_POINT('Ctrl Pts',(-4.36128949737787,1.07731645292395,75.6120593456358));
#54781=CARTESIAN_POINT('Ctrl Pts',(-4.37097940507052,-0.00397941814148494,
75.6514101080949));
#54782=CARTESIAN_POINT('Ctrl Pts',(-4.37167806635839,-0.00399716320838302,
74.8485898919049));
#54783=CARTESIAN_POINT('Ctrl Pts',(-4.37486787390589,-0.3533501983587,74.8613088088659));
#54784=CARTESIAN_POINT('Ctrl Pts',(-4.1769137234544,-2.15270356402942,74.9269479799088));
#54785=CARTESIAN_POINT('Ctrl Pts',(-1.69169300421356,-4.88264569196979,
75.0455074050335));
#54786=CARTESIAN_POINT('Ctrl Pts',(3.18450981172911,-4.06951488912588,75.2042681672795));
#54787=CARTESIAN_POINT('Ctrl Pts',(5.14615197585861,0.468160245196775,75.3630289295254));
#54788=CARTESIAN_POINT('Ctrl Pts',(2.39787866042351,4.57736082297456,75.5217896917712));
#54789=CARTESIAN_POINT('Ctrl Pts',(-2.54500644918866,4.49722095825909,75.6805504540172));
#54790=CARTESIAN_POINT('Ctrl Pts',(-4.33833518668749,1.61805156266242,75.7894838540617));
#54791=CARTESIAN_POINT('Ctrl Pts',(-4.37890350804243,0.0861408316175627,
75.8454970000243));
#54792=CARTESIAN_POINT('Ctrl Pts',(-4.37851995085447,0.00153222730234961,
75.8485898919049));
#54793=CARTESIAN_POINT('Origin',(0.,0.,24.1514101080949));
#54794=CARTESIAN_POINT('',(-4.37573799308197,0.00329254665532695,73.6514101080949));
#54795=CARTESIAN_POINT('',(-4.36501807785945,0.000928765700389245,73.8485898919049));
#54796=CARTESIAN_POINT('',(-4.372,3.82579154166093E-12,24.1514101080949));
#54797=CARTESIAN_POINT('Ctrl Pts',(-4.37573799308197,0.00329254665532727,
73.6514101080949));
#54798=CARTESIAN_POINT('Ctrl Pts',(-4.36535453025917,-1.23506946531353,
73.6966032174009));
#54799=CARTESIAN_POINT('Ctrl Pts',(-3.16833117156948,-3.94108625070045,
73.7947165807888));
#54800=CARTESIAN_POINT('Ctrl Pts',(1.42107208653042,-4.9681593715318,73.9457501982587));
#54801=CARTESIAN_POINT('Ctrl Pts',(4.94466868411869,-1.50076814343543,74.1045109605046));
#54802=CARTESIAN_POINT('Ctrl Pts',(3.94275346512999,3.34017193109278,74.2632717227505));
#54803=CARTESIAN_POINT('Ctrl Pts',(-0.667690158118302,5.12408462740484,
74.4220324849963));
#54804=CARTESIAN_POINT('Ctrl Pts',(-3.9268970087966,2.75604594892831,74.5514119467779));
#54805=CARTESIAN_POINT('Ctrl Pts',(-4.3669244447204,0.650273716756605,74.6278711544774));
#54806=CARTESIAN_POINT('Ctrl Pts',(-4.36519646031047,0.00129875109319548,
74.6514101080949));
#54807=CARTESIAN_POINT('Ctrl Pts',(-4.36501807785945,0.000928765700389245,
73.8485898919049));
#54808=CARTESIAN_POINT('Ctrl Pts',(-4.36352375843653,-0.785750920308218,
73.8771206177074));
#54809=CARTESIAN_POINT('Ctrl Pts',(-3.78436122884701,-3.0336560998423,73.9585715975918));
#54810=CARTESIAN_POINT('Ctrl Pts',(-0.183308880309829,-5.16415065893858,
74.0929428315583));
#54811=CARTESIAN_POINT('Ctrl Pts',(4.23913515679244,-2.95495977912772,74.2517035938041));
#54812=CARTESIAN_POINT('Ctrl Pts',(4.78179321232898,1.95870055096247,74.4104643560501));
#54813=CARTESIAN_POINT('Ctrl Pts',(0.948008058166557,5.07969830752458,74.5692251182959));
#54814=CARTESIAN_POINT('Ctrl Pts',(-3.37677384390662,3.67402258696438,74.7152669635808));
#54815=CARTESIAN_POINT('Ctrl Pts',(-4.36159587705234,1.10022100123729,74.8083885547839));
#54816=CARTESIAN_POINT('Ctrl Pts',(-4.37167806635839,-0.00399716320838302,
74.8485898919049));
#54817=CARTESIAN_POINT('Origin',(0.,0.,24.1514101080949));
#54818=CARTESIAN_POINT('',(-4.37546659946853,-0.00338795269852561,72.6514101080949));
#54819=CARTESIAN_POINT('',(-4.37508401727703,0.00350862331529297,72.848589891905));
#54820=CARTESIAN_POINT('',(-4.372,3.82579154166093E-12,24.1514101080949));
#54821=CARTESIAN_POINT('Ctrl Pts',(-4.37546659946853,-0.00338795269852542,
72.6514101080949));
#54822=CARTESIAN_POINT('Ctrl Pts',(-4.37736040129649,-0.224956166423907,
72.6594947721605));
#54823=CARTESIAN_POINT('Ctrl Pts',(-4.26133239251396,-1.89486696261105,
72.720499690308));
#54824=CARTESIAN_POINT('Ctrl Pts',(-2.1112172128698,-4.71644095649861,72.8344248625374));
#54825=CARTESIAN_POINT('Ctrl Pts',(2.81733266516402,-4.33182294996633,72.9931856247833));
#54826=CARTESIAN_POINT('Ctrl Pts',(5.16737363149282,0.0174117376300544,
73.1519463870293));
#54827=CARTESIAN_POINT('Ctrl Pts',(2.78807641079671,4.35071067109887,73.3107071492751));
#54828=CARTESIAN_POINT('Ctrl Pts',(-2.14295350396336,4.70210630419026,73.469467911521));
#54829=CARTESIAN_POINT('Ctrl Pts',(-4.26731753777204,1.87500660994908,73.5830355644609));
#54830=CARTESIAN_POINT('Ctrl Pts',(-4.37751336374666,0.215028421847947,
73.6436829633189));
#54831=CARTESIAN_POINT('Ctrl Pts',(-4.37573799308197,0.00329254665532727,
73.6514101080949));
#54832=CARTESIAN_POINT('Ctrl Pts',(-4.37508401727703,0.00350862331529318,
72.848589891905));
#54833=CARTESIAN_POINT('Ctrl Pts',(-4.36445811409486,-1.21201843518349,
72.892932426549));
#54834=CARTESIAN_POINT('Ctrl Pts',(-3.20535851125622,-3.89598203052578,
72.9901952152748));
#54835=CARTESIAN_POINT('Ctrl Pts',(1.34123860080759,-4.99030391755056,73.140378258083));
#54836=CARTESIAN_POINT('Ctrl Pts',(4.91997252333115,-1.57984953191204,73.2991390203287));
#54837=CARTESIAN_POINT('Ctrl Pts',(3.99579730998455,3.27653140246455,73.4578997825747));
#54838=CARTESIAN_POINT('Ctrl Pts',(-0.585453654677876,5.13413071435083,
73.6166605448206));
#54839=CARTESIAN_POINT('Ctrl Pts',(-3.90388041542688,2.80342624447369,73.746890581264));
#54840=CARTESIAN_POINT('Ctrl Pts',(-4.36629549877317,0.673422924511184,
73.8242003636254));
#54841=CARTESIAN_POINT('Ctrl Pts',(-4.36501807785945,0.000928765700389245,
73.8485898919049));
#54842=CARTESIAN_POINT('Origin',(0.,0.,24.1514101080949));
#54843=CARTESIAN_POINT('',(-4.3651141969528,-0.00114447055126671,71.6514101080949));
#54844=CARTESIAN_POINT('',(-4.37610278806197,-0.00315032678594118,71.8485898919049));
#54845=CARTESIAN_POINT('',(-4.372,3.82579154166093E-12,24.1514101080949));
#54846=CARTESIAN_POINT('Ctrl Pts',(-4.3651141969528,-0.00114447055126629,
71.6514101080949));
#54847=CARTESIAN_POINT('Ctrl Pts',(-4.36665839117516,-0.660007333527467,
71.675306581002));
#54848=CARTESIAN_POINT('Ctrl Pts',(-3.91728495207162,-2.77596398718315,
71.7521233079911));
#54849=CARTESIAN_POINT('Ctrl Pts',(-0.63314364249968,-5.12846785541421,
71.8818602890621));
#54850=CARTESIAN_POINT('Ctrl Pts',(3.9651734499498,-3.31352575482195,72.040621051308));
#54851=CARTESIAN_POINT('Ctrl Pts',(4.93444268320512,1.53405632954553,72.1993818135539));
#54852=CARTESIAN_POINT('Ctrl Pts',(1.38755924827672,4.97762320275213,72.3581425757998));
#54853=CARTESIAN_POINT('Ctrl Pts',(-3.18397114357576,3.92214967618973,72.50881867398));
#54854=CARTESIAN_POINT('Ctrl Pts',(-4.36496403292504,1.22537573008428,72.6065745180785));
#54855=CARTESIAN_POINT('Ctrl Pts',(-4.37546659946853,-0.00338795269852542,
72.6514101080949));
#54856=CARTESIAN_POINT('Ctrl Pts',(-4.37610278806197,-0.00315032678594042,
71.8485898919049));
#54857=CARTESIAN_POINT('Ctrl Pts',(-4.37771416984263,-0.201332656341541,
71.8558239813086));
#54858=CARTESIAN_POINT('Ctrl Pts',(-4.27545064435103,-1.84762538881353,
71.9159783247941));
#54859=CARTESIAN_POINT('Ctrl Pts',(-2.18656114390733,-4.68198724237597,
72.0290529223616));
#54860=CARTESIAN_POINT('Ctrl Pts',(2.74752166081747,-4.3764344959288,72.1878136846077));
#54861=CARTESIAN_POINT('Ctrl Pts',(5.16698871742013,-0.0654352188752399,
72.3465744468534));
#54862=CARTESIAN_POINT('Ctrl Pts',(2.85746987211454,4.30545236923763,72.5053352090995));
#54863=CARTESIAN_POINT('Ctrl Pts',(-2.06729268270395,4.73585843726931,72.6640959713451));
#54864=CARTESIAN_POINT('Ctrl Pts',(-4.2529565583671,1.92226442851864,72.7785141989471));
#54865=CARTESIAN_POINT('Ctrl Pts',(-4.37713951584072,0.238642906024094,
72.840012172467));
#54866=CARTESIAN_POINT('Ctrl Pts',(-4.37508401727703,0.00350862331529318,
72.848589891905));
#54867=CARTESIAN_POINT('Origin',(0.,0.,24.1514101080949));
#54868=CARTESIAN_POINT('',(-4.37127157619262,0.00399172071570709,70.6514101080949));
#54869=CARTESIAN_POINT('',(-4.36532703354517,-0.00150807403881736,70.8485898919049));
#54870=CARTESIAN_POINT('',(-4.372,3.82579154166093E-12,24.1514101080949));
#54871=CARTESIAN_POINT('Ctrl Pts',(-4.37127157619262,0.00399172071570714,
70.6514101080949));
#54872=CARTESIAN_POINT('Ctrl Pts',(-4.36140746653353,-1.08694237129441,
70.6911183898435));
#54873=CARTESIAN_POINT('Ctrl Pts',(-3.39621711134158,-3.64736222930015,
70.7837469256742));
#54874=CARTESIAN_POINT('Ctrl Pts',(0.900757702520816,-5.08828939599587,
70.9292957155868));
#54875=CARTESIAN_POINT('Ctrl Pts',(4.76338297422217,-2.00305667841551,71.0880564778326));
#54876=CARTESIAN_POINT('Ctrl Pts',(4.26641464848803,2.9154346954137,71.2468172400786));
#54877=CARTESIAN_POINT('Ctrl Pts',(-0.135306682874774,5.16563118288797,
71.4055780023244));
#54878=CARTESIAN_POINT('Ctrl Pts',(-3.76928933575608,3.06100151884775,71.5404422916632));
#54879=CARTESIAN_POINT('Ctrl Pts',(-4.36323867518121,0.799086242725653,
71.62238632692));
#54880=CARTESIAN_POINT('Ctrl Pts',(-4.3651141969528,-0.00114447055126629,
71.6514101080949));
#54881=CARTESIAN_POINT('Ctrl Pts',(-4.36532703354517,-0.00150807403881757,
70.8485898919049));
#54882=CARTESIAN_POINT('Ctrl Pts',(-4.36729483924552,-0.636841944886774,
70.8716357901501));
#54883=CARTESIAN_POINT('Ctrl Pts',(-3.94000526365074,-2.72857085726927,
70.9476019424773));
#54884=CARTESIAN_POINT('Ctrl Pts',(-0.715283247733823,-5.11765806295492,
71.0764883488864));
#54885=CARTESIAN_POINT('Ctrl Pts',(3.91154054911197,-3.37667065413102,71.2352491111322));
#54886=CARTESIAN_POINT('Ctrl Pts',(4.95840295584866,1.45474887910182,71.3940098733782));
#54887=CARTESIAN_POINT('Ctrl Pts',(1.46718352100222,4.95473780229749,71.552770635624));
#54888=CARTESIAN_POINT('Ctrl Pts',(-3.14657975547223,3.96714821422749,71.7042973084663));
#54889=CARTESIAN_POINT('Ctrl Pts',(-4.36592626835323,1.24845026027391,71.8029037272266));
#54890=CARTESIAN_POINT('Ctrl Pts',(-4.37610278806197,-0.00315032678594042,
71.8485898919049));
#54891=CARTESIAN_POINT('Origin',(0.,0.,24.1514101080949));
#54892=CARTESIAN_POINT('',(-4.37870422100453,-0.0012994166445059,69.6514101080949));
#54893=CARTESIAN_POINT('',(-4.3705809381838,0.00395105542623939,69.848589891905));
#54894=CARTESIAN_POINT('',(-4.372,3.82579154166093E-12,24.1514101080949));
#54895=CARTESIAN_POINT('Ctrl Pts',(-4.37870422100453,-0.00129941664450634,
69.6514101080949));
#54896=CARTESIAN_POINT('Ctrl Pts',(-4.3789830325923,-0.0724121058889038,
69.6540099446031));
#54897=CARTESIAN_POINT('Ctrl Pts',(-4.34518999704772,-1.59076889411841,
69.7095300351934));
#54898=CARTESIAN_POINT('Ctrl Pts',(-2.58669250630018,-4.47337403912361,
69.8179703798655));
#54899=CARTESIAN_POINT('Ctrl Pts',(2.35523426198658,-4.5994483350962,69.9767311421114));
#54900=CARTESIAN_POINT('Ctrl Pts',(5.14157869213602,-0.51596702281012,70.1354919043573));
#54901=CARTESIAN_POINT('Ctrl Pts',(3.22219325167658,4.03974306916968,70.2942526666032));
#54902=CARTESIAN_POINT('Ctrl Pts',(-1.6462418758917,4.89815690868675,70.4530134288491));
#54903=CARTESIAN_POINT('Ctrl Pts',(-4.16716700492617,2.18017319825989,70.5720659093463));
#54904=CARTESIAN_POINT('Ctrl Pts',(-4.3745536205967,0.366973708511667,70.6381981357616));
#54905=CARTESIAN_POINT('Ctrl Pts',(-4.37127157619262,0.00399172071570714,
70.6514101080949));
#54906=CARTESIAN_POINT('Ctrl Pts',(-4.3705809381838,0.00395105542623928,
69.848589891905));
#54907=CARTESIAN_POINT('Ctrl Pts',(-4.36115189233779,-1.06404425239527,
69.8874475989916));
#54908=CARTESIAN_POINT('Ctrl Pts',(-3.42928322572819,-3.60126660220352,
69.9792255601602));
#54909=CARTESIAN_POINT('Ctrl Pts',(0.819065126108891,-5.102076684352,70.1239237754111));
#54910=CARTESIAN_POINT('Ctrl Pts',(4.73065728621489,-2.07916709626671,70.2826845376568));
#54911=CARTESIAN_POINT('Ctrl Pts',(4.31260739816882,2.84665972730784,70.4414452999028));
#54912=CARTESIAN_POINT('Ctrl Pts',(-0.0524725109896868,5.16713661609669,
70.6002060621488));
#54913=CARTESIAN_POINT('Ctrl Pts',(-3.74285914641375,3.1081338808624,70.7359209261493));
#54914=CARTESIAN_POINT('Ctrl Pts',(-4.36277617060702,0.822074063266301,
70.8187155360681));
#54915=CARTESIAN_POINT('Ctrl Pts',(-4.36532703354517,-0.00150807403881757,
70.8485898919049));
#54916=CARTESIAN_POINT('Origin',(0.,0.,24.1514101080949));
#54917=CARTESIAN_POINT('',(-4.36744694438276,-0.00316878230680772,68.6514101080949));
#54918=CARTESIAN_POINT('',(-4.37895590169143,-0.000884728325120654,68.848589891905));
#54919=CARTESIAN_POINT('',(-4.372,3.82579154166093E-12,24.1514101080949));
#54920=CARTESIAN_POINT('Ctrl Pts',(-4.36744694438276,-0.0031687823068071,
68.6514101080949));
#54921=CARTESIAN_POINT('Ctrl Pts',(-4.37084913112638,-0.510127366468858,
68.6698217534447));
#54922=CARTESIAN_POINT('Ctrl Pts',(-4.05501785193817,-2.47012128343436,
68.7411536528764));
#54923=CARTESIAN_POINT('Ctrl Pts',(-1.15903350388962,-5.03574172817834,
68.8654058063903));
#54924=CARTESIAN_POINT('Ctrl Pts',(3.60203679805415,-3.70504849111566,69.0241665686361));
#54925=CARTESIAN_POINT('Ctrl Pts',(5.06641299677213,1.01661829719571,69.182927330882));
#54926=CARTESIAN_POINT('Ctrl Pts',(1.89385326524434,4.80784496690336,69.3416880931279));
#54927=CARTESIAN_POINT('Ctrl Pts',(-2.93168118063718,4.20875891624129,69.4978490188655));
#54928=CARTESIAN_POINT('Ctrl Pts',(-4.37330776031301,1.37510260179151,69.6010896905212));
#54929=CARTESIAN_POINT('Ctrl Pts',(-4.37870422100453,-0.00129941664450634,
69.6514101080949));
#54930=CARTESIAN_POINT('Ctrl Pts',(-4.37895590169143,-0.00088472832512114,
68.848589891905));
#54931=CARTESIAN_POINT('Ctrl Pts',(-4.37908827342486,-0.0487245072402155,
68.8503391537513));
#54932=CARTESIAN_POINT('Ctrl Pts',(-4.35670634828455,-1.54372976222875,
68.9050086696796));
#54933=CARTESIAN_POINT('Ctrl Pts',(-2.65807841962993,-4.43132861441282,
69.0125984396897));
#54934=CARTESIAN_POINT('Ctrl Pts',(2.2811920004135,-4.63661700284439,69.1713592019357));
#54935=CARTESIAN_POINT('Ctrl Pts',(5.1326458217616,-0.598331882962418,69.3301199641815));
#54936=CARTESIAN_POINT('Ctrl Pts',(3.28654540832559,3.98756485249208,69.4888807264275));
#54937=CARTESIAN_POINT('Ctrl Pts',(-1.56750175164667,4.92392043319156,69.6476414886732));
#54938=CARTESIAN_POINT('Ctrl Pts',(-4.14999820818835,2.2275746797718,69.7675445438326));
#54939=CARTESIAN_POINT('Ctrl Pts',(-4.37399329599569,0.390456985212737,
69.8345273449097));
#54940=CARTESIAN_POINT('Ctrl Pts',(-4.3705809381838,0.00395105542623928,
69.848589891905));
#54941=CARTESIAN_POINT('Origin',(0.,0.,24.1514101080949));
#54942=CARTESIAN_POINT('',(-4.36727426748866,0.00308741741996557,67.6514101080949));
#54943=CARTESIAN_POINT('',(-4.36799009248299,-0.00339142969553563,67.8485898919049));
#54944=CARTESIAN_POINT('',(-4.372,3.82579154166093E-12,24.1514101080949));
#54945=CARTESIAN_POINT('Ctrl Pts',(-4.36727426748866,0.0030874174199657,
67.6514101080949));
#54946=CARTESIAN_POINT('Ctrl Pts',(-4.36112833884136,-0.939337788388386,
67.6856335622863));
#54947=CARTESIAN_POINT('Ctrl Pts',(-3.59904165290846,-3.34810943987296,
67.7727772705596));
#54948=CARTESIAN_POINT('Ctrl Pts',(0.370823889097725,-5.15408023407956,
67.9128412329148));
#54949=CARTESIAN_POINT('Ctrl Pts',(4.53122783943781,-2.48395404207855,68.0716019951608));
#54950=CARTESIAN_POINT('Ctrl Pts',(4.5445136629679,2.45956276259679,68.2303627574067));
#54951=CARTESIAN_POINT('Ctrl Pts',(0.398521768172548,5.15201259862078,68.3891235196525));
#54952=CARTESIAN_POINT('Ctrl Pts',(-3.58909538685354,3.36377270257325,68.5294726365487));
#54953=CARTESIAN_POINT('Ctrl Pts',(-4.36107028825353,0.947014381222592,
68.6169014993627));
#54954=CARTESIAN_POINT('Ctrl Pts',(-4.36744694438276,-0.0031687823068071,
68.6514101080949));
#54955=CARTESIAN_POINT('Ctrl Pts',(-4.36799009248299,-0.00339142969553514,
67.8485898919049));
#54956=CARTESIAN_POINT('Ctrl Pts',(-4.37149165529305,-0.486778408785156,
67.8661509625928));
#54957=CARTESIAN_POINT('Ctrl Pts',(-4.07455789488293,-2.42267137940883,
67.9366322873626));
#54958=CARTESIAN_POINT('Ctrl Pts',(-1.23961891643423,-5.01651264483955,
68.0600338662145));
#54959=CARTESIAN_POINT('Ctrl Pts',(3.54217356679019,-3.76232117137135,68.2187946284603));
#54960=CARTESIAN_POINT('Ctrl Pts',(5.08206060458778,0.935261559732356,68.3775553907062));
#54961=CARTESIAN_POINT('Ctrl Pts',(1.97069054350433,4.77686434343271,68.5363161529522));
#54962=CARTESIAN_POINT('Ctrl Pts',(-2.89016105242335,4.25237825733215,68.6933276533517));
#54963=CARTESIAN_POINT('Ctrl Pts',(-4.37508364382578,1.39856782394589,68.7974188996693));
#54964=CARTESIAN_POINT('Ctrl Pts',(-4.37895590169143,-0.00088472832512114,
68.848589891905));
#54965=CARTESIAN_POINT('Origin',(0.,0.,24.1514101080949));
#54966=CARTESIAN_POINT('',(-4.37860089698225,0.00143482616460942,66.6514101080949));
#54967=CARTESIAN_POINT('',(-4.36678925203502,0.00282595512297229,66.8485898919049));
#54968=CARTESIAN_POINT('',(-4.372,3.82579154166093E-12,24.1514101080949));
#54969=CARTESIAN_POINT('Ctrl Pts',(-4.37860089698225,0.00143482616460969,
66.6514101080949));
#54970=CARTESIAN_POINT('Ctrl Pts',(-4.37274293747686,-1.3672535432393,66.7014453711278));
#54971=CARTESIAN_POINT('Ctrl Pts',(-2.94545539126712,-4.19408159696058,
66.8044008882426));
#54972=CARTESIAN_POINT('Ctrl Pts',(1.86798369006022,-4.81795499664787,66.9602766594396));
#54973=CARTESIAN_POINT('Ctrl Pts',(5.06087547593053,-1.04383563513614,67.1190374216854));
#54974=CARTESIAN_POINT('Ctrl Pts',(3.62189943977487,3.68563398402679,67.2777981839313));
#54975=CARTESIAN_POINT('Ctrl Pts',(-1.13194959602156,5.04189880185246,67.4365589461772));
#54976=CARTESIAN_POINT('Ctrl Pts',(-4.04836008668961,2.48602916041319,67.5610962542317));
#54977=CARTESIAN_POINT('Ctrl Pts',(-4.37063188292449,0.517948815873062,
67.6327133082043));
#54978=CARTESIAN_POINT('Ctrl Pts',(-4.36727426748866,0.0030874174199657,
67.6514101080949));
#54979=CARTESIAN_POINT('Ctrl Pts',(-4.36678925203502,0.00282595512297222,
66.8485898919049));
#54980=CARTESIAN_POINT('Ctrl Pts',(-4.36134189412171,-0.916433051844979,
66.8819627714344));
#54981=CARTESIAN_POINT('Ctrl Pts',(-3.62832781641238,-3.30133069322053,
66.9682559050458));
#54982=CARTESIAN_POINT('Ctrl Pts',(0.288144638596748,-5.15936302667923,
67.1074692927391));
#54983=CARTESIAN_POINT('Ctrl Pts',(4.49082211047655,-2.55628068604989,67.266230054985));
#54984=CARTESIAN_POINT('Ctrl Pts',(4.58336201290063,2.38638782106256,67.4249908172308));
#54985=CARTESIAN_POINT('Ctrl Pts',(0.481069000502546,5.14496130117338,67.5837515794768));
#54986=CARTESIAN_POINT('Ctrl Pts',(-3.55904252406398,3.41043311335412,67.7249512710348));
#54987=CARTESIAN_POINT('Ctrl Pts',(-4.36093970223245,0.969907359868089,
67.8132307085108));
#54988=CARTESIAN_POINT('Ctrl Pts',(-4.36799009248299,-0.00339142969553514,
67.8485898919049));
#54989=CARTESIAN_POINT('Origin',(0.,0.,24.1514101080949));
#54990=CARTESIAN_POINT('',(-4.37150619923976,-0.00399650483370713,65.6514101080949));
#54991=CARTESIAN_POINT('',(-4.37824072692977,0.00182550535674644,65.8485898919049));
#54992=CARTESIAN_POINT('',(-4.372,3.82579154166093E-12,24.1514101080949));
#54993=CARTESIAN_POINT('Ctrl Pts',(-4.37150619923976,-0.00399650483370689,
65.6514101080949));
#54994=CARTESIAN_POINT('Ctrl Pts',(-4.37473632420811,-0.359095615586663,
65.6643369258874));
#54995=CARTESIAN_POINT('Ctrl Pts',(-4.17282222069464,-2.16428561428065,
65.7301839977619));
#54996=CARTESIAN_POINT('Ctrl Pts',(-1.67254574036732,-4.88923758498539,
65.8489513237183));
#54997=CARTESIAN_POINT('Ctrl Pts',(3.20043304382085,-4.05700403599433,66.0077120859643));
#54998=CARTESIAN_POINT('Ctrl Pts',(5.14427774780404,0.488323529540513,66.16647284821));
#54999=CARTESIAN_POINT('Ctrl Pts',(2.3799223229872,4.58672248480354,66.3252336104561));
#55000=CARTESIAN_POINT('Ctrl Pts',(-2.56261070750152,4.48721291871176,66.4839943727018));
#55001=CARTESIAN_POINT('Ctrl Pts',(-4.34124164729195,1.60654622778481,66.5927198719149));
#55002=CARTESIAN_POINT('Ctrl Pts',(-4.37893866198466,0.0803522427089276,
66.6485251170459));
#55003=CARTESIAN_POINT('Ctrl Pts',(-4.37860089698225,0.00143482616460969,
66.6514101080949));
#55004=CARTESIAN_POINT('Ctrl Pts',(-4.37824072692977,0.00182550535674642,
65.8485898919049));
#55005=CARTESIAN_POINT('Ctrl Pts',(-4.37114754505431,-1.34389016319695,
65.8977745802759));
#55006=CARTESIAN_POINT('Ctrl Pts',(-2.98610974303986,-4.15014526257514,
65.9998795227288));
#55007=CARTESIAN_POINT('Ctrl Pts',(1.79050088812788,-4.84728385216189,66.1549047192638));
#55008=CARTESIAN_POINT('Ctrl Pts',(5.04349004573647,-1.12483880283976,66.3136654815096));
#55009=CARTESIAN_POINT('Ctrl Pts',(3.68052305807757,3.62709307749002,66.4724262437556));
#55010=CARTESIAN_POINT('Ctrl Pts',(-1.05097105537457,5.05939858230018,66.6311870060014));
#55011=CARTESIAN_POINT('Ctrl Pts',(-4.02817917541877,2.53347937952348,66.7565748887179));
#55012=CARTESIAN_POINT('Ctrl Pts',(-4.36997991304344,0.541260167974116,
66.8290425173524));
#55013=CARTESIAN_POINT('Ctrl Pts',(-4.36678925203502,0.00282595512297222,
66.8485898919049));
#55014=CARTESIAN_POINT('Origin',(0.,0.,24.1514101080949));
#55015=CARTESIAN_POINT('',(-4.36505611781897,0.00102009982110932,64.6514101080949));
#55016=CARTESIAN_POINT('',(-4.37221209240493,-0.00398401159164008,64.848589891905));
#55017=CARTESIAN_POINT('',(-4.372,3.82579154166093E-12,24.1514101080949));
#55018=CARTESIAN_POINT('Ctrl Pts',(-4.36505611781897,0.00102009982110941,
64.6514101080949));
#55019=CARTESIAN_POINT('Ctrl Pts',(-4.36340207653842,-0.791374776421536,
64.680148734729));
#55020=CARTESIAN_POINT('Ctrl Pts',(-3.7780282066601,-3.04518855619851,64.7618076154451));
#55021=CARTESIAN_POINT('Ctrl Pts',(-0.163070050579303,-5.16482928804609,
64.8963867502428));
#55022=CARTESIAN_POINT('Ctrl Pts',(4.25068252576661,-2.93832460446375,65.0551475124889));
#55023=CARTESIAN_POINT('Ctrl Pts',(4.77408061574266,1.97742450941745,65.2139082747347));
#55024=CARTESIAN_POINT('Ctrl Pts',(0.928094299999949,5.08337431106172,65.3726690369806));
#55025=CARTESIAN_POINT('Ctrl Pts',(-3.38499698876322,3.66278651613716,65.518502981434));
#55026=CARTESIAN_POINT('Ctrl Pts',(-4.36151272681657,1.09462141415472,65.6114166718055));
#55027=CARTESIAN_POINT('Ctrl Pts',(-4.37150619923976,-0.00399650483370689,
65.6514101080949));
#55028=CARTESIAN_POINT('Ctrl Pts',(-4.37221209240492,-0.00398401159164036,
64.848589891905));
#55029=CARTESIAN_POINT('Ctrl Pts',(-4.37526481066381,-0.335581023561335,
64.8606661350355));
#55030=CARTESIAN_POINT('Ctrl Pts',(-4.18939334686749,-2.11690750379085,
64.925662632248));
#55031=CARTESIAN_POINT('Ctrl Pts',(-1.75071636731768,-4.86179456322688,
65.0435793835425));
#55032=CARTESIAN_POINT('Ctrl Pts',(3.1349787773885,-4.10779286711735,65.2023401457884));
#55033=CARTESIAN_POINT('Ctrl Pts',(5.15144558585509,0.405786335144852,65.3611009080343));
#55034=CARTESIAN_POINT('Ctrl Pts',(2.45315204119292,4.54797748857745,65.5198616702802));
#55035=CARTESIAN_POINT('Ctrl Pts',(-2.49034118407384,4.52772072468283,65.6786224325261));
#55036=CARTESIAN_POINT('Ctrl Pts',(-4.32920116011288,1.65362984026736,65.788198506401));
#55037=CARTESIAN_POINT('Ctrl Pts',(-4.37877945245337,0.104032299273348,
65.844854326194));
#55038=CARTESIAN_POINT('Ctrl Pts',(-4.37824072692977,0.00182550535674642,
65.8485898919049));
#55039=CARTESIAN_POINT('Origin',(0.,0.,24.1514101080949));
#55040=CARTESIAN_POINT('',(-4.37524640365158,0.00345929889477671,63.6514101080949));
#55041=CARTESIAN_POINT('',(-4.36492309298158,0.000643490633093768,63.848589891905));
#55042=CARTESIAN_POINT('',(-4.372,3.82579154166093E-12,24.1514101080949));
#55043=CARTESIAN_POINT('Ctrl Pts',(-4.37524640365158,0.00345929889477663,
63.6514101080949));
#55044=CARTESIAN_POINT('Ctrl Pts',(-4.36466684100657,-1.21764908937452,
63.6959605435705));
#55045=CARTESIAN_POINT('Ctrl Pts',(-3.19636598506899,-3.90702309781776,
63.7934312331281));
#55046=CARTESIAN_POINT('Ctrl Pts',(1.36078442693529,-4.98500944427043,63.9438221767676));
#55047=CARTESIAN_POINT('Ctrl Pts',(4.92612583383742,-1.56055685101642,64.1025829390136));
#55048=CARTESIAN_POINT('Ctrl Pts',(3.98292640713875,3.29216504011747,64.2613437012594));
#55049=CARTESIAN_POINT('Ctrl Pts',(-0.605568927444514,5.13179692604536,
64.4201044635054));
#55050=CARTESIAN_POINT('Ctrl Pts',(-3.90955357406592,2.79184753823524,64.5501265991171));
#55051=CARTESIAN_POINT('Ctrl Pts',(-4.36644788265656,0.667767259764548,
64.627228480647));
#55052=CARTESIAN_POINT('Ctrl Pts',(-4.36505611781897,0.00102009982110941,
64.6514101080949));
#55053=CARTESIAN_POINT('Ctrl Pts',(-4.36492309298158,0.000643490633093699,
63.8485898919049));
#55054=CARTESIAN_POINT('Ctrl Pts',(-4.36391231627522,-0.768357459497397,
63.876477943877));
#55055=CARTESIAN_POINT('Ctrl Pts',(-3.80373422012026,-2.9979881039429,63.9572862499311));
#55056=CARTESIAN_POINT('Ctrl Pts',(-0.245853021615901,-5.16155116855183,
64.0910148100673));
#55057=CARTESIAN_POINT('Ctrl Pts',(4.20302825930282,-3.00609507922124,64.249775572313));
#55058=CARTESIAN_POINT('Ctrl Pts',(4.80516969413782,1.90063104898239,64.408536334559));
#55059=CARTESIAN_POINT('Ctrl Pts',(1.00947304907845,5.06784158562605,64.5672970968048));
#55060=CARTESIAN_POINT('Ctrl Pts',(-3.35112485942778,3.70870379987186,64.7139816159202));
#55061=CARTESIAN_POINT('Ctrl Pts',(-4.36188725407156,1.11753630245885,64.8077458809536));
#55062=CARTESIAN_POINT('Ctrl Pts',(-4.37221209240492,-0.00398401159164036,
64.848589891905));
#55063=CARTESIAN_POINT('Origin',(0.,0.,24.1514101080949));
#55064=CARTESIAN_POINT('',(-4.37595036350582,-0.00321178070193251,62.6514101080949));
#55065=CARTESIAN_POINT('',(-4.37457294606715,0.00364650982632456,62.848589891905));
#55066=CARTESIAN_POINT('',(-4.372,3.82579154166093E-12,24.1514101080949));
#55067=CARTESIAN_POINT('Ctrl Pts',(-4.37595036350582,-0.00321178070193263,
62.6514101080949));
#55068=CARTESIAN_POINT('Ctrl Pts',(-4.37763091892069,-0.207108192738585,
62.6588520983301));
#55069=CARTESIAN_POINT('Ctrl Pts',(-4.27203828701875,-1.85916971844638,
62.7192143426473));
#55070=CARTESIAN_POINT('Ctrl Pts',(-2.16819641913028,-4.69051998227545,
62.8324968410464));
#55071=CARTESIAN_POINT('Ctrl Pts',(2.76465101981334,-4.3656337632353,62.9912576032923));
#55072=CARTESIAN_POINT('Ctrl Pts',(5.16720539805885,-0.0451861740625634,
63.1500183655382));
#55073=CARTESIAN_POINT('Ctrl Pts',(2.8405755616569,4.31661718184185,63.308779127784));
#55074=CARTESIAN_POINT('Ctrl Pts',(-2.08583579528372,4.72772064013601,63.46753989003));
#55075=CARTESIAN_POINT('Ctrl Pts',(-4.25650552345673,1.91071093035616,63.5817502168002));
#55076=CARTESIAN_POINT('Ctrl Pts',(-4.37723401655206,0.232872448270317,
63.6430402894885));
#55077=CARTESIAN_POINT('Ctrl Pts',(-4.37524640365158,0.00345929889477663,
63.6514101080949));
#55078=CARTESIAN_POINT('Ctrl Pts',(-4.37457294606715,0.00364650982632473,
62.848589891905));
#55079=CARTESIAN_POINT('Ctrl Pts',(-4.36385410668696,-1.19462603572661,
62.8922897527186));
#55080=CARTESIAN_POINT('Ctrl Pts',(-3.23292058066413,-3.86178527014851,
62.9889098676142));
#55081=CARTESIAN_POINT('Ctrl Pts',(1.28068854395033,-5.00618527695598,63.1384502365919));
#55082=CARTESIAN_POINT('Ctrl Pts',(4.90047350742458,-1.63933327204883,63.2972109988377));
#55083=CARTESIAN_POINT('Ctrl Pts',(4.03519542999152,3.22788661752423,63.4559717610837));
#55084=CARTESIAN_POINT('Ctrl Pts',(-0.523216761619089,5.14084607765855,
63.6147325233295));
#55085=CARTESIAN_POINT('Ctrl Pts',(-3.886148042221,2.83920884682887,63.7456052336033));
#55086=CARTESIAN_POINT('Ctrl Pts',(-4.3658303620453,0.690895618159912,63.8235576897951));
#55087=CARTESIAN_POINT('Ctrl Pts',(-4.36492309298158,0.000643490633093699,
63.8485898919049));
#55088=CARTESIAN_POINT('Origin',(0.,0.,24.1514101080949));
#55089=CARTESIAN_POINT('',(-4.36526954399882,-0.00142033253192601,61.6514101080949));
#55090=CARTESIAN_POINT('',(-4.37655926179451,-0.0029470014875782,61.848589891905));
#55091=CARTESIAN_POINT('',(-4.372,3.82579154166093E-12,24.1514101080949));
#55092=CARTESIAN_POINT('Ctrl Pts',(-4.36526954399882,-0.00142033253192606,
61.6514101080949));
#55093=CARTESIAN_POINT('Ctrl Pts',(-4.36713817680575,-0.642506710603713,
61.6746639071717));
#55094=CARTESIAN_POINT('Ctrl Pts',(-3.93449886856382,-2.74015675637768,
61.7508379603305));
#55095=CARTESIAN_POINT('Ctrl Pts',(-0.695222522116061,-5.12042176590928,
61.879932267571));
#55096=CARTESIAN_POINT('Ctrl Pts',(3.92474305071123,-3.3613160223265,62.038693029817));
#55097=CARTESIAN_POINT('Ctrl Pts',(4.95266390069012,1.47416881762428,62.1974537920629));
#55098=CARTESIAN_POINT('Ctrl Pts',(1.4477554676688,4.96044932661243,62.3562145543087));
#55099=CARTESIAN_POINT('Ctrl Pts',(-3.15577720759182,3.95616660035224,62.5075333263195));
#55100=CARTESIAN_POINT('Ctrl Pts',(-4.36568043030908,1.24280635839108,62.6059318442481));
#55101=CARTESIAN_POINT('Ctrl Pts',(-4.37595036350582,-0.00321178070193263,
62.6514101080949));
#55102=CARTESIAN_POINT('Ctrl Pts',(-4.37655926179451,-0.00294700148757761,
61.848589891905));
#55103=CARTESIAN_POINT('Ctrl Pts',(-4.37795768436782,-0.183473677232841,
61.8551813074782));
#55104=CARTESIAN_POINT('Ctrl Pts',(-4.28584228404936,-1.81194987404807,
61.9146929771335));
#55105=CARTESIAN_POINT('Ctrl Pts',(-2.24311745571471,-4.65515609337478,
62.0271249008706));
#55106=CARTESIAN_POINT('Ctrl Pts',(2.69430472161155,-4.40939635788372,62.1858856631165));
#55107=CARTESIAN_POINT('Ctrl Pts',(5.16581691910958,-0.128022388891978,
62.3446464253625));
#55108=CARTESIAN_POINT('Ctrl Pts',(2.90941568030617,4.27052158090844,62.5034071876082));
#55109=CARTESIAN_POINT('Ctrl Pts',(-2.00977165837252,4.76055375508134,62.6621679498542));
#55110=CARTESIAN_POINT('Ctrl Pts',(-4.24182569275328,1.95798917979278,62.7772288512864));
#55111=CARTESIAN_POINT('Ctrl Pts',(-4.37683455314381,0.256474411491908,
62.8393694986367));
#55112=CARTESIAN_POINT('Ctrl Pts',(-4.37457294606715,0.00364650982632473,
62.848589891905));
#55113=CARTESIAN_POINT('Origin',(0.,0.,24.1514101080949));
#55114=CARTESIAN_POINT('',(-4.37074823605818,0.00396461597538121,60.6514101080949));
#55115=CARTESIAN_POINT('',(-4.36552637203463,-0.001773948386046,60.848589891905));
#55116=CARTESIAN_POINT('',(-4.372,3.82579154166093E-12,24.1514101080949));
#55117=CARTESIAN_POINT('Ctrl Pts',(-4.37074823605818,0.00396461597538186,
60.6514101080949));
#55118=CARTESIAN_POINT('Ctrl Pts',(-4.36120638422482,-1.0696402047533,60.6904757160132));
#55119=CARTESIAN_POINT('Ctrl Pts',(-3.42125648388678,-3.61254525965742,
60.7824615780135));
#55120=CARTESIAN_POINT('Ctrl Pts',(0.839052987504236,-5.09882765939536,
60.9273676940957));
#55121=CARTESIAN_POINT('Ctrl Pts',(4.73876879287487,-2.06061246810993,61.0861284563416));
#55122=CARTESIAN_POINT('Ctrl Pts',(4.30141865142892,2.86353819621711,61.2448892185875));
#55123=CARTESIAN_POINT('Ctrl Pts',(-0.0727212283482856,5.16689123545314,
61.4036499808334));
#55124=CARTESIAN_POINT('Ctrl Pts',(-3.74936971792349,3.0966186529212,61.5391569440025));
#55125=CARTESIAN_POINT('Ctrl Pts',(-4.36288560187799,0.816457216282587,
61.6217436530897));
#55126=CARTESIAN_POINT('Ctrl Pts',(-4.36526954399882,-0.00142033253192606,
61.6514101080949));
#55127=CARTESIAN_POINT('Ctrl Pts',(-4.36552637203463,-0.00177394838604503,
60.848589891905));
#55128=CARTESIAN_POINT('Ctrl Pts',(-4.36778246279527,-0.619319994324535,
60.8709931163198));
#55129=CARTESIAN_POINT('Ctrl Pts',(-3.95683545179798,-2.6927488906017,60.9463165948165));
#55130=CARTESIAN_POINT('Ctrl Pts',(-0.777225152475865,-5.10861774222493,
61.0745603273954));
#55131=CARTESIAN_POINT('Ctrl Pts',(3.87034915924295,-3.42380658907068,61.2333210896411));
#55132=CARTESIAN_POINT('Ctrl Pts',(4.97566169906822,1.39457693593507,61.3920818518871));
#55133=CARTESIAN_POINT('Ctrl Pts',(1.52709666834069,4.93660105126586,61.550842614133));
#55134=CARTESIAN_POINT('Ctrl Pts',(-3.11790932935563,4.00102289357066,61.7030119608056));
#55135=CARTESIAN_POINT('Ctrl Pts',(-4.36673022084793,1.26591415802506,61.8022610533963));
#55136=CARTESIAN_POINT('Ctrl Pts',(-4.37655926179451,-0.00294700148757761,
61.848589891905));
#55137=CARTESIAN_POINT('Origin',(0.,0.,24.1514101080949));
#55138=CARTESIAN_POINT('',(-4.37890245970854,-0.00098741172007078,59.6514101080949));
#55139=CARTESIAN_POINT('',(-4.37007084553272,0.00389455484668386,59.848589891905));
#55140=CARTESIAN_POINT('',(-4.372,3.82579154166093E-12,24.1514101080949));
#55141=CARTESIAN_POINT('Ctrl Pts',(-4.37890245970854,-0.000987411720070989,
59.6514101080949));
#55142=CARTESIAN_POINT('Ctrl Pts',(-4.37906627500205,-0.054514724532804,
59.6533672707728));
#55143=CARTESIAN_POINT('Ctrl Pts',(-4.35392740184128,-1.55522413176342,
59.7082446875327));
#55144=CARTESIAN_POINT('Ctrl Pts',(-2.6406923556686,-4.44171107781315,59.8160423583745));
#55145=CARTESIAN_POINT('Ctrl Pts',(2.29934455736468,-4.62764173446609,59.9748031206204));
#55146=CARTESIAN_POINT('Ctrl Pts',(5.13495109710383,-0.578213322578349,
60.1335638828663));
#55147=CARTESIAN_POINT('Ctrl Pts',(3.27089354364999,4.00041358388897,60.2923246451122));
#55148=CARTESIAN_POINT('Ctrl Pts',(-1.58678569169648,4.91773978415717,60.451085407358));
#55149=CARTESIAN_POINT('Ctrl Pts',(-4.15423631088884,2.21598713963915,60.5707805616856));
#55150=CARTESIAN_POINT('Ctrl Pts',(-4.37413226072698,0.384719343814296,
60.6375554619313));
#55151=CARTESIAN_POINT('Ctrl Pts',(-4.37074823605818,0.00396461597538186,
60.6514101080949));
#55152=CARTESIAN_POINT('Ctrl Pts',(-4.37007084553272,0.00389455484668389,
59.848589891905));
#55153=CARTESIAN_POINT('Ctrl Pts',(-4.36101477584936,-1.0467484993519,59.8868049251613));
#55154=CARTESIAN_POINT('Ctrl Pts',(-3.45386988791881,-3.56635453916342,
59.9779402124996));
#55155=CARTESIAN_POINT('Ctrl Pts',(0.757199388556149,-5.11162432694214,
60.12199575392));
#55156=CARTESIAN_POINT('Ctrl Pts',(4.70512351821232,-2.13632086826434,60.2807565161658));
#55157=CARTESIAN_POINT('Ctrl Pts',(4.34677488413138,2.79420870381954,60.4395172784118));
#55158=CARTESIAN_POINT('Ctrl Pts',(0.0101251021257834,5.16739311995163,
60.5982780406576));
#55159=CARTESIAN_POINT('Ctrl Pts',(-3.72252569100569,3.14370820853236,60.7346355784887));
#55160=CARTESIAN_POINT('Ctrl Pts',(-4.36245318991586,0.839429561242695,
60.8180728622378));
#55161=CARTESIAN_POINT('Ctrl Pts',(-4.36552637203463,-0.00177394838604503,
60.848589891905));
#55162=CARTESIAN_POINT('Origin',(0.,0.,24.1514101080949));
#55163=CARTESIAN_POINT('',(-4.36785354673662,-0.00333986239341869,58.6514101080949));
#55164=CARTESIAN_POINT('',(-4.37908572622912,-0.000563059365845109,58.848589891905));
#55165=CARTESIAN_POINT('',(-4.372,3.82579154166093E-12,24.1514101080949));
#55166=CARTESIAN_POINT('Ctrl Pts',(-4.36785354673662,-0.00333986239341826,
58.6514101080949));
#55167=CARTESIAN_POINT('Ctrl Pts',(-4.3713354267805,-0.492488022383476,
58.6691790796144));
#55168=CARTESIAN_POINT('Ctrl Pts',(-4.0698257693161,-2.43426901092249,58.7398683052158));
#55169=CARTESIAN_POINT('Ctrl Pts',(-1.21995052871669,-5.02133190732686,
58.8634777848992));
#55170=CARTESIAN_POINT('Ctrl Pts',(3.55689020801282,-3.74841105859499,59.022238547145));
#55171=CARTESIAN_POINT('Ctrl Pts',(5.07835637974298,0.955170087669591,59.1809993093909));
#55172=CARTESIAN_POINT('Ctrl Pts',(1.95195567231696,4.78455039364876,59.3397600716368));
#55173=CARTESIAN_POINT('Ctrl Pts',(-2.90036961753982,4.24173919554959,59.4965636712048));
#55174=CARTESIAN_POINT('Ctrl Pts',(-4.37463682871597,1.39282484839483,59.6004470166909));
#55175=CARTESIAN_POINT('Ctrl Pts',(-4.37890245970854,-0.000987411720070989,
59.6514101080949));
#55176=CARTESIAN_POINT('Ctrl Pts',(-4.37908572622912,-0.000563059365844233,
58.848589891905));
#55177=CARTESIAN_POINT('Ctrl Pts',(-4.37914057971478,-0.0308242308936409,
58.8496964799209));
#55178=CARTESIAN_POINT('Ctrl Pts',(-4.36515029335745,-1.50821048731078,
58.9037233220189));
#55179=CARTESIAN_POINT('Ctrl Pts',(-2.71156370034918,-4.39880398208026,
59.0106704181988));
#55180=CARTESIAN_POINT('Ctrl Pts',(2.22485747409188,-4.66391074033302,59.1694311804446));
#55181=CARTESIAN_POINT('Ctrl Pts',(5.12502112908765,-0.660463928024547,
59.3281919426906));
#55182=CARTESIAN_POINT('Ctrl Pts',(3.33460890093368,3.94745964534539,59.4869527049363));
#55183=CARTESIAN_POINT('Ctrl Pts',(-1.5077392503099,4.94254757457034,59.6457134671823));
#55184=CARTESIAN_POINT('Ctrl Pts',(-4.13672535981933,2.2634000371691,59.7662591961718));
#55185=CARTESIAN_POINT('Ctrl Pts',(-4.37355563916387,0.408184092349566,
59.8338846710794));
#55186=CARTESIAN_POINT('Ctrl Pts',(-4.37007084553272,0.00389455484668389,
59.848589891905));
#55187=CARTESIAN_POINT('Origin',(0.,0.,24.1514101080949));
#55188=CARTESIAN_POINT('',(-4.36690348533115,0.0028923709500598,57.6514101080949));
#55189=CARTESIAN_POINT('',(-4.36842637263245,-0.00353866609716813,57.848589891905));
#55190=CARTESIAN_POINT('',(-4.372,3.82579154166093E-12,24.1514101080949));
#55191=CARTESIAN_POINT('Ctrl Pts',(-4.36690348533115,0.00289237095005987,
57.6514101080949));
#55192=CARTESIAN_POINT('Ctrl Pts',(-4.36128421030265,-0.922032505654121,
57.6849908884559));
#55193=CARTESIAN_POINT('Ctrl Pts',(-3.62122223271516,-3.31277225264101,
57.7714919228989));
#55194=CARTESIAN_POINT('Ctrl Pts',(0.308361079608735,-5.1581941472416,57.9109132114238));
#55195=CARTESIAN_POINT('Ctrl Pts',(4.50080518836808,-2.53866226040682,58.0696739736697));
#55196=CARTESIAN_POINT('Ctrl Pts',(4.57397490984839,2.40433087160068,58.2284347359156));
#55197=CARTESIAN_POINT('Ctrl Pts',(0.460903079952699,5.14680694867653,58.3871954981615));
#55198=CARTESIAN_POINT('Ctrl Pts',(-3.56644148611271,3.39903679271645,58.5281872888879));
#55199=CARTESIAN_POINT('Ctrl Pts',(-4.36096555385885,0.964312382866099,
58.6162588255324));
#55200=CARTESIAN_POINT('Ctrl Pts',(-4.36785354673662,-0.00333986239341826,
58.6514101080949));
#55201=CARTESIAN_POINT('Ctrl Pts',(-4.36842637263245,-0.00353866609716848,
57.848589891905));
#55202=CARTESIAN_POINT('Ctrl Pts',(-4.37197022738872,-0.469118111917197,
57.8655082887625));
#55203=CARTESIAN_POINT('Ctrl Pts',(-4.08900712877109,-2.3868217079302,57.935346939702));
#55204=CARTESIAN_POINT('Ctrl Pts',(-1.30029709065152,-5.00112803773905,
58.0581058447233));
#55205=CARTESIAN_POINT('Ctrl Pts',(3.49633757827368,-3.80495436405849,58.2168666069693));
#55206=CARTESIAN_POINT('Ctrl Pts',(5.09301729854088,0.873629767452735,58.3756273692151));
#55207=CARTESIAN_POINT('Ctrl Pts',(2.02841201894453,4.75264125042254,58.5343881314611));
#55208=CARTESIAN_POINT('Ctrl Pts',(-2.85835725119982,4.28517149950547,58.6920423056909));
#55209=CARTESIAN_POINT('Ctrl Pts',(-4.37651732665532,1.41635291451315,58.796776225839));
#55210=CARTESIAN_POINT('Ctrl Pts',(-4.37908572622912,-0.000563059365844233,
58.848589891905));
#55211=CARTESIAN_POINT('Origin',(0.,0.,24.1514101080949));
#55212=CARTESIAN_POINT('',(-4.37833561871486,0.00173199218209078,56.6514101080949));
#55213=CARTESIAN_POINT('',(-4.36645415447485,0.00261097933498017,56.848589891905));
#55214=CARTESIAN_POINT('',(-4.372,3.82579154166093E-12,24.1514101080949));
#55215=CARTESIAN_POINT('Ctrl Pts',(-4.37833561871486,0.00173199218209092,
56.6514101080949));
#55216=CARTESIAN_POINT('Ctrl Pts',(-4.3715252071243,-1.34959412873374,56.7008026972975));
#55217=CARTESIAN_POINT('Ctrl Pts',(-2.97623248528167,-4.16090558093235,
56.803115540582));
#55218=CARTESIAN_POINT('Ctrl Pts',(1.8094827870843,-4.8402298973603,56.9583486379485));
#55219=CARTESIAN_POINT('Ctrl Pts',(5.04785929713791,-1.10506557830443,57.1171094001944));
#55220=CARTESIAN_POINT('Ctrl Pts',(3.66628078958101,3.64148851268323,57.2758701624403));
#55221=CARTESIAN_POINT('Ctrl Pts',(-1.07078988460527,5.05524108614831,57.4346309246862));
#55222=CARTESIAN_POINT('Ctrl Pts',(-4.03315651405818,2.52188158975817,57.559810906571));
#55223=CARTESIAN_POINT('Ctrl Pts',(-4.37013967640761,0.535564934025079,
57.632070634374));
#55224=CARTESIAN_POINT('Ctrl Pts',(-4.36690348533115,0.00289237095005987,
57.6514101080949));
#55225=CARTESIAN_POINT('Ctrl Pts',(-4.36645415447485,0.00261097933498031,
56.848589891905));
#55226=CARTESIAN_POINT('Ctrl Pts',(-4.36154135054989,-0.899119064739272,
56.881320097604));
#55227=CARTESIAN_POINT('Ctrl Pts',(-3.65007828630307,-3.26593148213623,
56.9669705573851));
#55228=CARTESIAN_POINT('Ctrl Pts',(0.225623900899773,-5.162474990657,57.1055412712481));
#55229=CARTESIAN_POINT('Ctrl Pts',(4.45952627223033,-2.61049412968195,57.2643020334939));
#55230=CARTESIAN_POINT('Ctrl Pts',(4.61193398121205,2.33069069735948,57.4230627957398));
#55231=CARTESIAN_POINT('Ctrl Pts',(0.543358837230748,5.13875620630321,57.5818235579857));
#55232=CARTESIAN_POINT('Ctrl Pts',(-3.53595095853239,3.44562506237492,57.7236659233741));
#55233=CARTESIAN_POINT('Ctrl Pts',(-4.36088515262005,0.98720087478414,57.8125880346805));
#55234=CARTESIAN_POINT('Ctrl Pts',(-4.36842637263245,-0.00353866609716848,
57.848589891905));
#55235=CARTESIAN_POINT('Origin',(0.,0.,24.1514101080949));
#55236=CARTESIAN_POINT('',(-4.37203889039062,-0.00399078471529107,55.6514101080949));
#55237=CARTESIAN_POINT('',(-4.37792086111113,0.00210556704416318,55.848589891905));
#55238=CARTESIAN_POINT('',(-4.372,3.82579154166093E-12,24.1514101080949));
#55239=CARTESIAN_POINT('Ctrl Pts',(-4.37203889039062,-0.0039907847152907,
55.6514101080949));
#55240=CARTESIAN_POINT('Ctrl Pts',(-4.37513795036318,-0.341330640933386,
55.6636942520571));
#55241=CARTESIAN_POINT('Ctrl Pts',(-4.18538392269166,-2.12848606629693,
55.7288986501012));
#55242=CARTESIAN_POINT('Ctrl Pts',(-1.7316503614075,-4.86861791907028,55.8470233022273));
#55243=CARTESIAN_POINT('Ctrl Pts',(3.15105239533607,-4.09547582313724,56.0057840644731));
#55244=CARTESIAN_POINT('Ctrl Pts',(5.14981574971942,0.425970844068908,56.1645448267191));
#55245=CARTESIAN_POINT('Ctrl Pts',(2.43531042678924,4.55755598333432,56.3233055889649));
#55246=CARTESIAN_POINT('Ctrl Pts',(-2.50806538626398,4.517926674292,56.4820663512109));
#55247=CARTESIAN_POINT('Ctrl Pts',(-4.33218063910257,1.64211842271798,56.5914345242541));
#55248=CARTESIAN_POINT('Ctrl Pts',(-4.37882202467515,0.0982449665847532,
56.6478824432155));
#55249=CARTESIAN_POINT('Ctrl Pts',(-4.37833561871486,0.00173199218209092,
56.6514101080949));
#55250=CARTESIAN_POINT('Ctrl Pts',(-4.37792086111113,0.00210556704416347,
55.848589891905));
#55251=CARTESIAN_POINT('Ctrl Pts',(-4.37002924341455,-1.32628327647185,
55.8971319064456));
#55252=CARTESIAN_POINT('Ctrl Pts',(-3.01639925320847,-4.11679727890053,
55.9985941750683));
#55253=CARTESIAN_POINT('Ctrl Pts',(1.73165038597632,-4.86861798815274,56.1529766977727));
#55254=CARTESIAN_POINT('Ctrl Pts',(5.02949388480597,-1.18585219842773,56.3117374600186));
#55255=CARTESIAN_POINT('Ctrl Pts',(3.72419095237009,3.58224174562538,56.4704982222645));
#55256=CARTESIAN_POINT('Ctrl Pts',(-0.989605296568694,5.07175862308326,
56.6292589845104));
#55257=CARTESIAN_POINT('Ctrl Pts',(-4.01260884555851,2.56932936205486,56.7552895410572));
#55258=CARTESIAN_POINT('Ctrl Pts',(-4.36948468076768,0.558854755667328,
56.8283998435221));
#55259=CARTESIAN_POINT('Ctrl Pts',(-4.36645415447485,0.00261097933498031,
56.848589891905));
#55260=CARTESIAN_POINT('Origin',(0.,0.,24.1514101080949));
#55261=CARTESIAN_POINT('',(-4.36494997391578,0.000736207605459677,54.651410108095));
#55262=CARTESIAN_POINT('',(-4.37274842293649,-0.00394778047225652,54.848589891905));
#55263=CARTESIAN_POINT('',(-4.372,3.82579154166093E-12,24.1514101080949));
#55264=CARTESIAN_POINT('Ctrl Pts',(-4.36494997391578,0.000736207605459838,
54.651410108095));
#55265=CARTESIAN_POINT('Ctrl Pts',(-4.36378453680234,-0.773985575709198,
54.6795060608986));
#55266=CARTESIAN_POINT('Ctrl Pts',(-3.79750074957444,-3.0095293451424,54.7605222677843));
#55267=CARTESIAN_POINT('Ctrl Pts',(-0.22562389770033,-5.16247491740555,
54.8944587287519));
#55268=CARTESIAN_POINT('Ctrl Pts',(4.21477629650059,-2.98960100791253,55.0532194909978));
#55269=CARTESIAN_POINT('Ctrl Pts',(4.79768448212587,1.91944706257383,55.2119802532437));
#55270=CARTESIAN_POINT('Ctrl Pts',(0.989605282528937,5.07175855111871,55.3707410154895));
#55271=CARTESIAN_POINT('Ctrl Pts',(-3.35946002969715,3.69749334286384,55.5172176337734));
#55272=CARTESIAN_POINT('Ctrl Pts',(-4.36178715915881,1.11193390546508,55.6107739979751));
#55273=CARTESIAN_POINT('Ctrl Pts',(-4.37203889039062,-0.0039907847152907,
55.6514101080949));
#55274=CARTESIAN_POINT('Ctrl Pts',(-4.37274842293649,-0.00394778047225635,
54.848589891905));
#55275=CARTESIAN_POINT('Ctrl Pts',(-4.37564665776889,-0.317799192266558,
54.8600234612052));
#55276=CARTESIAN_POINT('Ctrl Pts',(-4.20162062889501,-2.08112280559727,
54.9243772845874));
#55277=CARTESIAN_POINT('Ctrl Pts',(-1.80948281276126,-4.84022996603858,
55.0416513620516));
#55278=CARTESIAN_POINT('Ctrl Pts',(3.08498768485217,-4.1454680264268,55.2004121242973));
#55279=CARTESIAN_POINT('Ctrl Pts',(5.15598322111311,0.34335287594041,55.3591728865433));
#55280=CARTESIAN_POINT('Ctrl Pts',(2.50806542185317,4.51792673839683,55.5179336487891));
#55281=CARTESIAN_POINT('Ctrl Pts',(-2.43531046134262,4.55755604800332,55.6766944110351));
#55282=CARTESIAN_POINT('Ctrl Pts',(-4.31984022389642,1.68922674479917,55.7869131587403));
#55283=CARTESIAN_POINT('Ctrl Pts',(-4.37863264435646,0.121919394632788,
55.8442116523636));
#55284=CARTESIAN_POINT('Ctrl Pts',(-4.37792086111113,0.00210556704416347,
55.848589891905));
#55285=CARTESIAN_POINT('Origin',(0.,0.,24.1514101080949));
#55286=CARTESIAN_POINT('',(-4.37473956626258,0.00360433591460132,53.6514101080949));
#55287=CARTESIAN_POINT('',(-4.36486283016371,0.00035491530368581,53.848589891905));
#55288=CARTESIAN_POINT('',(-4.372,3.82579154166093E-12,24.1514101080949));
#55289=CARTESIAN_POINT('Ctrl Pts',(-4.37473956626258,0.00360433591460166,
53.6514101080949));
#55290=CARTESIAN_POINT('Ctrl Pts',(-4.36404265119134,-1.20025020685171,
53.6953178697402));
#55291=CARTESIAN_POINT('Ctrl Pts',(-3.22404333927935,-3.87285840602707,
53.7921458854674));
#55292=CARTESIAN_POINT('Ctrl Pts',(1.30029707219943,-5.00112796677752,53.9418941552766));
#55293=CARTESIAN_POINT('Ctrl Pts',(4.90686007449561,-1.62011654684958,54.1006549175225));
#55294=CARTESIAN_POINT('Ctrl Pts',(4.02251485462088,3.2436750238594,54.2594156797684));
#55295=CARTESIAN_POINT('Ctrl Pts',(-0.543358829519001,5.13875613338857,
54.4181764420142));
#55296=CARTESIAN_POINT('Ctrl Pts',(-3.89191662696183,2.82763508414209,54.5488412514565));
#55297=CARTESIAN_POINT('Ctrl Pts',(-4.3659797009454,0.685245008222085,54.6265858068167));
#55298=CARTESIAN_POINT('Ctrl Pts',(-4.36494997391578,0.000736207605459838,
54.651410108095));
#55299=CARTESIAN_POINT('Ctrl Pts',(-4.36486283016371,0.000354915303685741,
53.848589891905));
#55300=CARTESIAN_POINT('Ctrl Pts',(-4.36431860610875,-0.750950458311704,
53.8758352700467));
#55301=CARTESIAN_POINT('Ctrl Pts',(-3.82280092431587,-2.96229440941745,
53.9560009022705));
#55302=CARTESIAN_POINT('Ctrl Pts',(-0.308361083986154,-5.15819422043212,
54.0890867885761));
#55303=CARTESIAN_POINT('Ctrl Pts',(4.16630456733569,-3.05678923480409,54.2478475508221));
#55304=CARTESIAN_POINT('Ctrl Pts',(4.82784101720183,1.84228262935957,54.4066083130679));
#55305=CARTESIAN_POINT('Ctrl Pts',(1.07078989980086,5.0552411578777,54.5653690753139));
#55306=CARTESIAN_POINT('Ctrl Pts',(-3.3251283689399,3.74330363517374,54.7126962682595));
#55307=CARTESIAN_POINT('Ctrl Pts',(-4.36223218327779,1.13486147913407,54.8071032071232));
#55308=CARTESIAN_POINT('Ctrl Pts',(-4.37274842293649,-0.00394778047225635,
54.848589891905));
#55309=CARTESIAN_POINT('Origin',(0.,0.,24.1514101080949));
#55310=CARTESIAN_POINT('',(-4.37641405919053,-0.00301495007056918,52.6514101080949));
#55311=CARTESIAN_POINT('',(-4.37405090679819,0.00376197565890995,52.848589891905));
#55312=CARTESIAN_POINT('',(-4.372,3.82579154166093E-12,24.1514101080949));
#55313=CARTESIAN_POINT('Ctrl Pts',(-4.37641405919053,-0.00301495007056837,
52.651410108095));
#55314=CARTESIAN_POINT('Ctrl Pts',(-4.37788112208874,-0.189251796122769,
52.6582094244998));
#55315=CARTESIAN_POINT('Ctrl Pts',(-4.28250642368832,-1.82348881026957,
52.7179289949866));
#55316=CARTESIAN_POINT('Ctrl Pts',(-2.22485744252472,-4.66391067415503,
52.8305688195554));
#55317=CARTESIAN_POINT('Ctrl Pts',(2.71156366187259,-4.39880391966578,52.9893295818012));
#55318=CARTESIAN_POINT('Ctrl Pts',(5.16627887713359,-0.107777454683187,
53.1480903440472));
#55319=CARTESIAN_POINT('Ctrl Pts',(2.89265785799892,4.28189022893068,53.306851106293));
#55320=CARTESIAN_POINT('Ctrl Pts',(-2.02841199016113,4.75264118298715,53.4656118685389));
#55321=CARTESIAN_POINT('Ctrl Pts',(-4.24545291415805,1.94643078465362,53.5804648691395));
#55322=CARTESIAN_POINT('Ctrl Pts',(-4.37693521146432,0.250707115811383,
53.6423976156582));
#55323=CARTESIAN_POINT('Ctrl Pts',(-4.37473956626258,0.00360433591460166,
53.6514101080949));
#55324=CARTESIAN_POINT('Ctrl Pts',(-4.37405090679819,0.00376197565890985,
52.848589891905));
#55325=CARTESIAN_POINT('Ctrl Pts',(-4.36331136726339,-1.17725226132736,
52.8916470788883));
#55326=CARTESIAN_POINT('Ctrl Pts',(-3.26012737634599,-3.8274917595608,52.9876245199536));
#55327=CARTESIAN_POINT('Ctrl Pts',(1.21995054602492,-5.021331978576,53.1365222151008));
#55328=CARTESIAN_POINT('Ctrl Pts',(4.88025534693686,-1.69857643999627,53.2952829773467));
#55329=CARTESIAN_POINT('Ctrl Pts',(4.07400138499168,3.17876814016096,53.4540437395925));
#55330=CARTESIAN_POINT('Ctrl Pts',(-0.460903086490536,5.14680702170578,
53.6128045018385));
#55331=CARTESIAN_POINT('Ctrl Pts',(-3.86811921206171,2.87497489714133,53.7443198859426));
#55332=CARTESIAN_POINT('Ctrl Pts',(-4.365375683574,0.708352879597865,53.8229150159648));
#55333=CARTESIAN_POINT('Ctrl Pts',(-4.36486283016371,0.000354915303685741,
53.848589891905));
#55334=CARTESIAN_POINT('Origin',(0.,0.,24.1514101080949));
#55335=CARTESIAN_POINT('',(-4.36545824626946,-0.00168887658937792,51.651410108095));
#55336=CARTESIAN_POINT('',(-4.37699111974124,-0.00272425946348631,51.848589891905));
#55337=CARTESIAN_POINT('',(-4.372,3.82579154166093E-12,24.1514101080949));
#55338=CARTESIAN_POINT('Ctrl Pts',(-4.36545824626946,-0.00168887658937779,
51.651410108095));
#55339=CARTESIAN_POINT('Ctrl Pts',(-4.36762412827266,-0.624989998325019,
51.6740212333413));
#55340=CARTESIAN_POINT('Ctrl Pts',(-3.95142248851676,-2.70433810681889,
51.7495526126697));
#55341=CARTESIAN_POINT('Ctrl Pts',(-0.757199377814005,-5.111624254412,51.87800424608));
#55342=CARTESIAN_POINT('Ctrl Pts',(3.88373669535471,-3.40861301664037,52.0367650083259));
#55343=CARTESIAN_POINT('Ctrl Pts',(4.97015831465276,1.41406497140078,52.1955257705718));
#55344=CARTESIAN_POINT('Ctrl Pts',(1.50773922891819,4.94254750443899,52.3542865328176));
#55345=CARTESIAN_POINT('Ctrl Pts',(-3.12722350039883,3.99007665346195,52.5062479786588));
#55346=CARTESIAN_POINT('Ctrl Pts',(-4.36646271813384,1.26026174695854,52.6052891704178));
#55347=CARTESIAN_POINT('Ctrl Pts',(-4.37641405919053,-0.00301495007056837,
52.651410108095));
#55348=CARTESIAN_POINT('Ctrl Pts',(-4.37699111974124,-0.00272425946348602,
51.848589891905));
#55349=CARTESIAN_POINT('Ctrl Pts',(-4.37818018489292,-0.165607164620367,
51.8545386336479));
#55350=CARTESIAN_POINT('Ctrl Pts',(-4.29599872620153,-1.77629134844302,
51.9134076294728));
#55351=CARTESIAN_POINT('Ctrl Pts',(-2.2993445899923,-4.62764180012773,52.0251968793796));
#55352=CARTESIAN_POINT('Ctrl Pts',(2.64069239313623,-4.44171114083851,52.1839576416255));
#55353=CARTESIAN_POINT('Ctrl Pts',(5.16388703706709,-0.190590771620509,
52.3427184038713));
#55354=CARTESIAN_POINT('Ctrl Pts',(2.96093453169081,4.23496409345547,52.5014791661172));
#55355=CARTESIAN_POINT('Ctrl Pts',(-1.95195570001178,4.78455046153847,52.6602399283632));
#55356=CARTESIAN_POINT('Ctrl Pts',(-4.23045159262607,1.99372864599193,52.7759435036257));
#55357=CARTESIAN_POINT('Ctrl Pts',(-4.37651100246309,0.274295735060812,
52.8387268248063));
#55358=CARTESIAN_POINT('Ctrl Pts',(-4.37405090679819,0.00376197565890985,
52.848589891905));
#55359=CARTESIAN_POINT('Origin',(0.,0.,24.1514101080949));
#55360=CARTESIAN_POINT('',(-4.3702345064702,0.00391522497022664,50.651410108095));
#55361=CARTESIAN_POINT('',(-4.36575804463348,-0.0020306512688445,50.848589891905));
#55362=CARTESIAN_POINT('',(-4.372,3.82579154166093E-12,24.1514101080949));
#55363=CARTESIAN_POINT('Ctrl Pts',(-4.3702345064702,0.00391522497022637,
50.651410108095));
#55364=CARTESIAN_POINT('Ctrl Pts',(-4.36105392339508,-1.0523431449496,50.6898330421829));
#55365=CARTESIAN_POINT('Ctrl Pts',(-3.44595349118066,-3.57765592823792,
50.7811762303528));
#55366=CARTESIAN_POINT('Ctrl Pts',(0.777225141445664,-5.10861766973804,
50.9254396726047));
#55367=CARTESIAN_POINT('Ctrl Pts',(4.71345919711634,-2.11786586288516,51.0842004348506));
#55368=CARTESIAN_POINT('Ctrl Pts',(4.33579142110028,2.81122147273531,51.2429611970965));
#55369=CARTESIAN_POINT('Ctrl Pts',(-0.0101251019801382,5.16739304663044,
51.4017219593423));
#55370=CARTESIAN_POINT('Ctrl Pts',(-3.72913776533524,3.13220382459871,51.5378715963418));
#55371=CARTESIAN_POINT('Ctrl Pts',(-4.36255498533209,0.833816380056773,
51.6211009792594));
#55372=CARTESIAN_POINT('Ctrl Pts',(-4.36545824626946,-0.00168887658937779,
51.651410108095));
#55373=CARTESIAN_POINT('Ctrl Pts',(-4.36575804463348,-0.00203065126884408,
50.848589891905));
#55374=CARTESIAN_POINT('Ctrl Pts',(-4.36827427270984,-0.601781773597835,
50.8703504424894));
#55375=CARTESIAN_POINT('Ctrl Pts',(-3.97337829241374,-2.65691780935309,
50.9450312471558));
#55376=CARTESIAN_POINT('Ctrl Pts',(-0.839052999411725,-5.09882773174331,
51.0726323059043));
#55377=CARTESIAN_POINT('Ctrl Pts',(3.82858979556074,-3.47044008032763,51.2313930681501));
#55378=CARTESIAN_POINT('Ctrl Pts',(4.99219026383802,1.33420033857639,51.390153830396));
#55379=CARTESIAN_POINT('Ctrl Pts',(1.58678571421362,4.91773985393535,51.548914592642));
#55380=CARTESIAN_POINT('Ctrl Pts',(-3.08887708143298,4.03478571508497,51.7017266131449));
#55381=CARTESIAN_POINT('Ctrl Pts',(-4.36760221182464,1.28340593748707,51.8016183795659));
#55382=CARTESIAN_POINT('Ctrl Pts',(-4.37699111974124,-0.00272425946348602,
51.848589891905));
#55383=CARTESIAN_POINT('Origin',(0.,0.,24.1514101080949));
#55384=CARTESIAN_POINT('',(-4.3790496246733,-0.000667733410364872,49.651410108095));
#55385=CARTESIAN_POINT('',(-4.36957357182231,0.00381643768188569,49.848589891905));
#55386=CARTESIAN_POINT('',(-4.372,3.82579154166093E-12,24.1514101080949));
#55387=CARTESIAN_POINT('Ctrl Pts',(-4.3790496246733,-0.000667733410364751,
49.651410108095));
#55388=CARTESIAN_POINT('Ctrl Pts',(-4.37912616480055,-0.0366150338825652,
49.6527245969425));
#55389=CARTESIAN_POINT('Ctrl Pts',(-4.36244279655587,-1.51969860268292,
49.706959339872));
#55390=CARTESIAN_POINT('Ctrl Pts',(-2.69430468338317,-4.40939629531691,
49.8141143368835));
#55391=CARTESIAN_POINT('Ctrl Pts',(2.2431174238849,-4.6551560273227,49.9728750991294));
#55392=CARTESIAN_POINT('Ctrl Pts',(5.12756994789964,-0.640374769530455,
50.1316358613752));
#55393=CARTESIAN_POINT('Ctrl Pts',(3.31911383193326,3.96049703783808,50.2903966236212));
#55394=CARTESIAN_POINT('Ctrl Pts',(-1.52709664667054,4.93660098122003,50.4491573858669));
#55395=CARTESIAN_POINT('Ctrl Pts',(-4.14104743841719,2.25180987009099,50.569495214025));
#55396=CARTESIAN_POINT('Ctrl Pts',(-4.37369842336595,0.402451046051582,
50.636912788101));
#55397=CARTESIAN_POINT('Ctrl Pts',(-4.3702345064702,0.00391522497022637,
50.651410108095));
#55398=CARTESIAN_POINT('Ctrl Pts',(-4.36957357182231,0.00381643768188559,
49.848589891905));
#55399=CARTESIAN_POINT('Ctrl Pts',(-4.36092390126923,-1.02945575440987,
49.886162251331));
#55400=CARTESIAN_POINT('Ctrl Pts',(-3.47811671755736,-3.53137427358546,
49.976654864839));
#55401=CARTESIAN_POINT('Ctrl Pts',(0.695222531978707,-5.12042183856424,
50.1200677324289));
#55402=CARTESIAN_POINT('Ctrl Pts',(4.67889927324325,-2.19316113513354,50.2788284946747));
#55403=CARTESIAN_POINT('Ctrl Pts',(4.38030448079635,2.74134763015048,50.4375892569207));
#55404=CARTESIAN_POINT('Ctrl Pts',(0.0727212293821569,5.16689130876717,
50.5963500191666));
#55405=CARTESIAN_POINT('Ctrl Pts',(-3.70187703653703,3.1792474229629,50.733350230828));
#55406=CARTESIAN_POINT('Ctrl Pts',(-4.36215496848489,0.85677423381658,50.8174301884075));
#55407=CARTESIAN_POINT('Ctrl Pts',(-4.36575804463348,-0.00203065126884408,
50.848589891905));
#55408=CARTESIAN_POINT('Origin',(0.,0.,24.1514101080949));
#55409=CARTESIAN_POINT('',(-4.36828286829859,-0.0034930826256922,48.651410108095));
#55410=CARTESIAN_POINT('',(-4.37915940465982,-0.00023684953408154,48.848589891905));
#55411=CARTESIAN_POINT('',(-4.372,3.82579154166093E-12,24.1514101080949));
#55412=CARTESIAN_POINT('Ctrl Pts',(-4.36828286829859,-0.00349308262569223,
48.651410108095));
#55413=CARTESIAN_POINT('Ctrl Pts',(-4.37181608551705,-0.47483281190334,
48.6685364057841));
#55414=CARTESIAN_POINT('Ctrl Pts',(-4.08436231910608,-2.39841849396994,
48.7385829575551));
#55415=CARTESIAN_POINT('Ctrl Pts',(-1.2806885257803,-5.00618520592171,48.8615497634081));
#55416=CARTESIAN_POINT('Ctrl Pts',(3.51122164426531,-3.79122354667958,49.020310525654));
#55417=CARTESIAN_POINT('Ctrl Pts',(5.0895545138177,0.893581706914796,49.1790712878999));
#55418=CARTESIAN_POINT('Ctrl Pts',(2.00977162985725,4.76055368753214,49.3378320501457));
#55419=CARTESIAN_POINT('Ctrl Pts',(-2.86868632585708,4.274578831514,49.4952783235442));
#55420=CARTESIAN_POINT('Ctrl Pts',(-4.37604472140215,1.41059410609646,49.5998043428605));
#55421=CARTESIAN_POINT('Ctrl Pts',(-4.3790496246733,-0.000667733410364751,
49.651410108095));
#55422=CARTESIAN_POINT('Ctrl Pts',(-4.37915940465982,-0.000236849534081855,
48.848589891905));
#55423=CARTESIAN_POINT('Ctrl Pts',(-4.37916937864932,-0.0129226461636581,
48.8490538060906));
#55424=CARTESIAN_POINT('Ctrl Pts',(-4.37337449519616,-1.47271062880396,
48.9024379743582));
#55425=CARTESIAN_POINT('Ctrl Pts',(-2.76465105904324,-4.36563382517906,
49.0087423967076));
#55426=CARTESIAN_POINT('Ctrl Pts',(2.16819644989342,-4.69052004883103,49.1675031589536));
#55427=CARTESIAN_POINT('Ctrl Pts',(5.11664433946473,-0.72249904999246,49.3262639211995));
#55428=CARTESIAN_POINT('Ctrl Pts',(3.38218303962157,3.90677514842007,49.4850246834453));
#55429=CARTESIAN_POINT('Ctrl Pts',(-1.44775548820939,4.96044939699782,49.6437854456913));
#55430=CARTESIAN_POINT('Ctrl Pts',(-4.12319150304179,2.29923281750856,49.7649738485111));
#55431=CARTESIAN_POINT('Ctrl Pts',(-4.37310686689576,0.425896738132308,
49.833241997249));
#55432=CARTESIAN_POINT('Ctrl Pts',(-4.36957357182231,0.00381643768188559,
49.848589891905));
#55433=CARTESIAN_POINT('Origin',(0.,0.,24.1514101080949));
#55434=CARTESIAN_POINT('',(-4.36655943089002,0.00268207779483023,47.651410108095));
#55435=CARTESIAN_POINT('',(-4.36888289277856,-0.00366680700230215,47.848589891905));
#55436=CARTESIAN_POINT('',(-4.372,3.82579154166093E-12,24.1514101080949));
#55437=CARTESIAN_POINT('Ctrl Pts',(-4.36655943089002,0.00268207779483047,
47.651410108095));
#55438=CARTESIAN_POINT('Ctrl Pts',(-4.36147330371707,-0.90472081724388,
47.6843482146256));
#55439=CARTESIAN_POINT('Ctrl Pts',(-3.64307749349284,-3.2773877690834,47.7702065752383));
#55440=CARTESIAN_POINT('Ctrl Pts',(0.245853018125491,-5.16155109531365,
47.9089851899327));
#55441=CARTESIAN_POINT('Ctrl Pts',(4.46972204405066,-2.59299792999961,48.0677459521787));
#55442=CARTESIAN_POINT('Ctrl Pts',(4.60276492582317,2.34874614500311,48.2265067144246));
#55443=CARTESIAN_POINT('Ctrl Pts',(0.523216754197009,5.14084600471386,48.3852674766704));
#55444=CARTESIAN_POINT('Ctrl Pts',(-3.54345722553092,3.4342468351364,48.5269019412272));
#55445=CARTESIAN_POINT('Ctrl Pts',(-4.36089844550389,0.981606792564894,
48.6156161517021));
#55446=CARTESIAN_POINT('Ctrl Pts',(-4.36828286829859,-0.00349308262569223,
48.651410108095));
#55447=CARTESIAN_POINT('Ctrl Pts',(-4.36888289277856,-0.00366680700230278,
47.848589891905));
#55448=CARTESIAN_POINT('Ctrl Pts',(-4.37244155465394,-0.451442255901039,
47.8648656149322));
#55449=CARTESIAN_POINT('Ctrl Pts',(-4.10318789366455,-2.35097548418382,
47.9340615920413));
#55450=CARTESIAN_POINT('Ctrl Pts',(-1.36078444624568,-4.98500951500319,
48.0561778232324));
#55451=CARTESIAN_POINT('Ctrl Pts',(3.44998850215064,-3.84702917961962,48.2149385854782));
#55452=CARTESIAN_POINT('Ctrl Pts',(5.10322659210776,0.811869769988193,48.3736993477241));
#55453=CARTESIAN_POINT('Ctrl Pts',(2.08583582488191,4.72772070721777,48.53246010997));
#55454=CARTESIAN_POINT('Ctrl Pts',(-2.82618015492052,4.31781852687336,48.6907569580302));
#55455=CARTESIAN_POINT('Ctrl Pts',(-4.37803161206443,1.43418891395024,48.7961335520086));
#55456=CARTESIAN_POINT('Ctrl Pts',(-4.37915940465982,-0.000236849534081855,
48.848589891905));
#55457=CARTESIAN_POINT('Origin',(0.,0.,24.1514101080949));
#55458=CARTESIAN_POINT('',(-4.37802849378088,0.00201652107500087,46.651410108095));
#55459=CARTESIAN_POINT('',(-4.36614763918315,0.00238232933584437,46.848589891905));
#55460=CARTESIAN_POINT('',(-4.372,3.82579154166093E-12,24.1514101080949));
#55461=CARTESIAN_POINT('Ctrl Pts',(-4.37802849378088,0.00201652107500106,
46.651410108095));
#55462=CARTESIAN_POINT('Ctrl Pts',(-4.37038284048536,-1.33197484216078,
46.7001600234672));
#55463=CARTESIAN_POINT('Ctrl Pts',(-3.00664095593531,-4.12759897737828,
46.8018301929213));
#55464=CARTESIAN_POINT('Ctrl Pts',(1.75071634247466,-4.86179449424254,46.9564206164574));
#55465=CARTESIAN_POINT('Ctrl Pts',(5.03410234489664,-1.16613335307792,47.1151813787034));
#55466=CARTESIAN_POINT('Ctrl Pts',(3.71012411261097,3.59680865283067,47.2739421409492));
#55467=CARTESIAN_POINT('Ctrl Pts',(-1.00947303475291,5.06784151371782,47.4327029031951));
#55468=CARTESIAN_POINT('Ctrl Pts',(-4.01767618670528,2.55773240591479,47.5585255589103));
#55469=CARTESIAN_POINT('Ctrl Pts',(-4.36964496780575,0.553164799693178,
47.6314279605436));
#55470=CARTESIAN_POINT('Ctrl Pts',(-4.36655943089002,0.00268207779483047,
47.651410108095));
#55471=CARTESIAN_POINT('Ctrl Pts',(-4.36614763918315,0.00238232933584499,
46.848589891905));
#55472=CARTESIAN_POINT('Ctrl Pts',(-4.36177165814571,-0.881797305075611,
46.8806774237737));
#55473=CARTESIAN_POINT('Ctrl Pts',(-3.67150621186276,-3.23048848803606,
46.9656852097244));
#55474=CARTESIAN_POINT('Ctrl Pts',(0.163070052891163,-5.16482936133098,
47.103613249757));
#55475=CARTESIAN_POINT('Ctrl Pts',(4.42757599841828,-2.66432448325026,47.2623740120029));
#55476=CARTESIAN_POINT('Ctrl Pts',(4.63982914812316,2.27465154475207,47.4211347742487));
#55477=CARTESIAN_POINT('Ctrl Pts',(0.605568936039063,5.13179699886122,47.5798955364947));
#55478=CARTESIAN_POINT('Ctrl Pts',(-3.51252635231322,3.4807591641629,47.7223805757134));
#55479=CARTESIAN_POINT('Ctrl Pts',(-4.36087062227061,1.00449248124495,47.8119453608502));
#55480=CARTESIAN_POINT('Ctrl Pts',(-4.36888289277856,-0.00366680700230278,
47.848589891905));
#55481=CARTESIAN_POINT('Origin',(0.,0.,24.1514101080949));
#55482=CARTESIAN_POINT('',(-4.37257478030532,-0.00396203305634906,45.651410108095));
#55483=CARTESIAN_POINT('',(-4.37756404870526,0.00237073416934012,45.848589891905));
#55484=CARTESIAN_POINT('',(-4.372,3.82579154166093E-12,24.1514101080949));
#55485=CARTESIAN_POINT('Ctrl Pts',(-4.37257478030532,-0.00396203305634935,
45.651410108095));
#55486=CARTESIAN_POINT('Ctrl Pts',(-4.3755247754399,-0.323552849206446,
45.6630515782267));
#55487=CARTESIAN_POINT('Ctrl Pts',(-4.19769260696374,-2.0926975991144,45.7276133024405));
#55488=CARTESIAN_POINT('Ctrl Pts',(-1.79050086272392,-4.84728378338218,
45.8450952807362));
#55489=CARTESIAN_POINT('Ctrl Pts',(3.1012093298518,-4.13334659912459,46.0038560429821));
#55490=CARTESIAN_POINT('Ctrl Pts',(5.15459801607478,0.363555647367575,46.162616805228));
#55491=CARTESIAN_POINT('Ctrl Pts',(2.49034114873962,4.52772066043712,46.3213775674739));
#55492=CARTESIAN_POINT('Ctrl Pts',(-2.45315200638293,4.54797742404625,46.4801383297198));
#55493=CARTESIAN_POINT('Ctrl Pts',(-4.32289330486948,1.67770933141668,46.5901491765935));
#55494=CARTESIAN_POINT('Ctrl Pts',(-4.37868254545781,0.116133556522668,
46.6472397693852));
#55495=CARTESIAN_POINT('Ctrl Pts',(-4.37802849378088,0.00201652107500106,
46.651410108095));
#55496=CARTESIAN_POINT('Ctrl Pts',(-4.37756404870526,0.00237073416934035,
45.848589891905));
#55497=CARTESIAN_POINT('Ctrl Pts',(-4.36898434288233,-1.30871296070451,
45.8964892326153));
#55498=CARTESIAN_POINT('Ctrl Pts',(-3.04632193268225,-4.08332402648612,
45.9973088274075));
#55499=CARTESIAN_POINT('Ctrl Pts',(1.67254576409749,-4.88923765436041,46.1510486762816));
#55500=CARTESIAN_POINT('Ctrl Pts',(5.01475964555148,-1.2466915701828,46.3098094385276));
#55501=CARTESIAN_POINT('Ctrl Pts',(3.76731232156889,3.53686471971598,46.4685702007735));
#55502=CARTESIAN_POINT('Ctrl Pts',(-0.928094313166731,5.08337438319113,
46.6273309630193));
#55503=CARTESIAN_POINT('Ctrl Pts',(-3.99675882839479,2.60517577302872,46.7540041933965));
#55504=CARTESIAN_POINT('Ctrl Pts',(-4.36898873016318,0.576432985076398,
46.8277571696918));
#55505=CARTESIAN_POINT('Ctrl Pts',(-4.36614763918315,0.00238232933584499,
46.848589891905));
#55506=CARTESIAN_POINT('Origin',(0.,0.,24.1514101080949));
#55507=CARTESIAN_POINT('',(-4.36487844624636,0.000448538275869127,44.651410108095));
#55508=CARTESIAN_POINT('',(-4.37328422903404,-0.00388840045026428,44.848589891905));
#55509=CARTESIAN_POINT('',(-4.372,3.82579154166093E-12,24.1514101080949));
#55510=CARTESIAN_POINT('Ctrl Pts',(-4.36487844624636,0.00044853827586927,
44.651410108095));
#55511=CARTESIAN_POINT('Ctrl Pts',(-4.36418527448618,-0.756583014477848,
44.6788633870683));
#55512=CARTESIAN_POINT('Ctrl Pts',(-3.8166662948363,-2.9738437257919,44.7592369201236));
#55513=CARTESIAN_POINT('Ctrl Pts',(-0.288144634510089,-5.15936295347187,
44.8925307072609));
#55514=CARTESIAN_POINT('Ctrl Pts',(4.17825154873217,-3.04043868735616,45.0512914695067));
#55515=CARTESIAN_POINT('Ctrl Pts',(4.8205842882194,1.86118793683688,45.2100522317526));
#55516=CARTESIAN_POINT('Ctrl Pts',(1.05097104046387,5.05939851051103,45.3688129939986));
#55517=CARTESIAN_POINT('Ctrl Pts',(-3.33357615425217,3.73211986818334,45.5159322861126));
#55518=CARTESIAN_POINT('Ctrl Pts',(-4.36211457120495,1.12925568798617,45.6101313241448));
#55519=CARTESIAN_POINT('Ctrl Pts',(-4.37257478030532,-0.00396203305634935,
45.651410108095));
#55520=CARTESIAN_POINT('Ctrl Pts',(-4.37328422903404,-0.00388840045026397,
44.848589891905));
#55521=CARTESIAN_POINT('Ctrl Pts',(-4.37601255181714,-0.300005218706897,
44.8593807873749));
#55522=CARTESIAN_POINT('Ctrl Pts',(-4.21359764945945,-2.04535030654532,
44.9230919369267));
#55523=CARTESIAN_POINT('Ctrl Pts',(-1.8679837165673,-4.81795506501003,45.0397233405604));
#55524=CARTESIAN_POINT('Ctrl Pts',(3.03454387031403,-4.18253483822383,45.1984841028063));
#55525=CARTESIAN_POINT('Ctrl Pts',(5.15976421573454,0.280869029694986,45.3572448650522));
#55526=CARTESIAN_POINT('Ctrl Pts',(2.56261074386464,4.4872129823807,45.5160056272982));
#55527=CARTESIAN_POINT('Ctrl Pts',(-2.37992235675453,4.58672254988638,45.6747663895439));
#55528=CARTESIAN_POINT('Ctrl Pts',(-4.31025055648257,1.72484198053187,45.7856278110796));
#55529=CARTESIAN_POINT('Ctrl Pts',(-4.37846339218375,0.139801386813307,
45.8435689785333));
#55530=CARTESIAN_POINT('Ctrl Pts',(-4.37756404870526,0.00237073416934035,
45.848589891905));
#55531=CARTESIAN_POINT('Origin',(0.,0.,24.1514101080949));
#55532=CARTESIAN_POINT('',(-4.37422072754471,0.00372710199133062,43.651410108095));
#55533=CARTESIAN_POINT('',(-4.36483752583336,6.45211600033835E-5,43.848589891905));
#55534=CARTESIAN_POINT('',(-4.372,3.82579154166093E-12,24.1514101080949));
#55535=CARTESIAN_POINT('Ctrl Pts',(-4.37422072754471,0.00372710199133028,
43.651410108095));
#55536=CARTESIAN_POINT('Ctrl Pts',(-4.36348027804383,-1.18287063932153,
43.6946751959099));
#55537=CARTESIAN_POINT('Ctrl Pts',(-3.25136487986307,-3.83859580238497,
43.7908605378067));
#55538=CARTESIAN_POINT('Ctrl Pts',(1.23961889884326,-5.01651257365967,43.9399661337855));
#55539=CARTESIAN_POINT('Ctrl Pts',(4.88687423334376,-1.67943849054845,44.0987268960314));
#55540=CARTESIAN_POINT('Ctrl Pts',(4.06151299797099,3.19470899822934,44.2574876582773));
#55541=CARTESIAN_POINT('Ctrl Pts',(-0.481068993674721,5.1449612281707,44.4162484205232));
#55542=CARTESIAN_POINT('Ctrl Pts',(-3.87398394218857,2.8634067002645,44.5475559037957));
#55543=CARTESIAN_POINT('Ctrl Pts',(-4.36552146553668,0.702707227634927,
44.6259431329863));
#55544=CARTESIAN_POINT('Ctrl Pts',(-4.36487844624636,0.00044853827586927,
44.651410108095));
#55545=CARTESIAN_POINT('Ctrl Pts',(-4.36483752583336,6.45211600032447E-5,
43.848589891905));
#55546=CARTESIAN_POINT('Ctrl Pts',(-4.36474095456816,-0.733529397636361,
43.8751925962164));
#55547=CARTESIAN_POINT('Ctrl Pts',(-3.84156354313547,-2.92657717231582,
43.9547155546098));
#55548=CARTESIAN_POINT('Ctrl Pts',(-0.370823894361365,-5.15408030721166,
44.0871587670851));
#55549=CARTESIAN_POINT('Ctrl Pts',(4.12896947009338,-3.10703480650815,44.245919529331));
#55550=CARTESIAN_POINT('Ctrl Pts',(4.84980385450403,1.78366385472551,44.4046802915768));
#55551=CARTESIAN_POINT('Ctrl Pts',(1.13194961208497,5.04189887339256,44.5634410538228));
#55552=CARTESIAN_POINT('Ctrl Pts',(-3.29878256966109,3.77781872906067,44.7114109205989));
#55553=CARTESIAN_POINT('Ctrl Pts',(-4.36263242638615,1.15219838236422,44.8064605332929));
#55554=CARTESIAN_POINT('Ctrl Pts',(-4.37328422903404,-0.00388840045026397,
44.848589891905));
#55555=CARTESIAN_POINT('Origin',(0.,0.,24.1514101080949));
#55556=CARTESIAN_POINT('',(-4.37685426135052,-0.00279837449763291,42.651410108095));
#55557=CARTESIAN_POINT('',(-4.37352103895722,0.00385464862035001,42.848589891905));
#55558=CARTESIAN_POINT('',(-4.372,3.82579154166093E-12,24.1514101080949));
#55559=CARTESIAN_POINT('Ctrl Pts',(-4.37685426135052,-0.00279837449763325,
42.651410108095));
#55560=CARTESIAN_POINT('Ctrl Pts',(-4.37811047462212,-0.171387646022154,
42.6575667506695));
#55561=CARTESIAN_POINT('Ctrl Pts',(-4.29273874071207,-1.78782473877565,
42.7166436473259));
#55562=CARTESIAN_POINT('Ctrl Pts',(-2.28119196804685,-4.63661693705371,
42.8286407980642));
#55563=CARTESIAN_POINT('Ctrl Pts',(2.65807838191241,-4.43132855153674,42.9874015603103));
#55564=CARTESIAN_POINT('Ctrl Pts',(5.1645942046841,-0.170352918960309,43.146162322556));
#55565=CARTESIAN_POINT('Ctrl Pts',(2.94431565674484,4.24653490854626,43.304923084802));
#55566=CARTESIAN_POINT('Ctrl Pts',(-1.97069051554003,4.77686427565358,43.4636838470478));
#55567=CARTESIAN_POINT('Ctrl Pts',(-4.23415771881522,1.98216556151801,43.5791795214788));
#55568=CARTESIAN_POINT('Ctrl Pts',(-4.37661759834636,0.26853179933828,43.6417549418279));
#55569=CARTESIAN_POINT('Ctrl Pts',(-4.37422072754471,0.00372710199133028,
43.651410108095));
#55570=CARTESIAN_POINT('Ctrl Pts',(-4.37352103895722,0.00385464862035015,
42.848589891905));
#55571=CARTESIAN_POINT('Ctrl Pts',(-4.36282818723577,-1.15989502481933,
42.891004405058));
#55572=CARTESIAN_POINT('Ctrl Pts',(-3.28698059005484,-3.79310505340026,
42.9863391722929));
#55573=CARTESIAN_POINT('Ctrl Pts',(1.15903352033341,-5.0357417996319,43.1345941936098));
#55574=CARTESIAN_POINT('Ctrl Pts',(4.85932100888344,-1.75757034181863,43.2933549558556));
#55575=CARTESIAN_POINT('Ctrl Pts',(4.11220948021047,3.12918317851219,43.4521157181016));
#55576=CARTESIAN_POINT('Ctrl Pts',(-0.398521773825228,5.15201267172389,
43.6108764803474));
#55577=CARTESIAN_POINT('Ctrl Pts',(-3.84979170382512,2.91072243457703,43.7430345382819));
#55578=CARTESIAN_POINT('Ctrl Pts',(-4.36493306195062,0.725795042513237,
43.8222723421345));
#55579=CARTESIAN_POINT('Ctrl Pts',(-4.36483752583336,6.45211600032447E-5,
43.848589891905));
#55580=CARTESIAN_POINT('Origin',(0.,0.,24.1514101080949));
#55581=CARTESIAN_POINT('',(-4.36567955402809,-0.00194869704108157,41.651410108095));
#55582=CARTESIAN_POINT('',(-4.37739485101806,-0.00248321819134589,41.848589891905));
#55583=CARTESIAN_POINT('',(-4.372,3.82579154166093E-12,24.1514101080949));
#55584=CARTESIAN_POINT('Ctrl Pts',(-4.3656795540281,-0.00194869704108112,
41.651410108095));
#55585=CARTESIAN_POINT('Ctrl Pts',(-4.36811474531132,-0.607457052316279,
41.673378559511));
#55586=CARTESIAN_POINT('Ctrl Pts',(-3.96805804018506,-2.66850978845469,
41.748267265009));
#55587=CARTESIAN_POINT('Ctrl Pts',(-0.819065114488867,-5.10207661195736,
41.8760762245889));
#55588=CARTESIAN_POINT('Ctrl Pts',(3.8421604015636,-3.45540979692878,42.0348369868349));
#55589=CARTESIAN_POINT('Ctrl Pts',(4.98692335778749,1.35375361111553,42.1935977490807));
#55590=CARTESIAN_POINT('Ctrl Pts',(1.56750172940691,4.92392036332446,42.3523585113267));
#55591=CARTESIAN_POINT('Ctrl Pts',(-3.09830846639719,4.02387607629251,42.504962630998));
#55592=CARTESIAN_POINT('Ctrl Pts',(-4.36731252351321,1.27774424309386,42.6046464965875));
#55593=CARTESIAN_POINT('Ctrl Pts',(-4.37685426135052,-0.00279837449763325,
42.651410108095));
#55594=CARTESIAN_POINT('Ctrl Pts',(-4.37739485101806,-0.00248321819134518,
41.8485898919051));
#55595=CARTESIAN_POINT('Ctrl Pts',(-4.37838119777137,-0.1477338083412,41.8538959598176));
#55596=CARTESIAN_POINT('Ctrl Pts',(-4.30592187837124,-1.74065025431473,
41.9121222818121));
#55597=CARTESIAN_POINT('Ctrl Pts',(-2.35523429540729,-4.59944840035779,
42.0232688578885));
#55598=CARTESIAN_POINT('Ctrl Pts',(2.58669254300161,-4.47337410259821,42.1820296201345));
#55599=CARTESIAN_POINT('Ctrl Pts',(5.16119935450289,-0.253131185149624,
42.3407903823802));
#55600=CARTESIAN_POINT('Ctrl Pts',(3.01201886587614,4.19878512494061,42.4995511446263));
#55601=CARTESIAN_POINT('Ctrl Pts',(-1.89385329211466,4.80784503512363,42.6583119068721));
#55602=CARTESIAN_POINT('Ctrl Pts',(-4.21883224032928,2.02948215439444,42.774658155965));
#55603=CARTESIAN_POINT('Ctrl Pts',(-4.37616957413132,0.292106279171763,
42.838084150976));
#55604=CARTESIAN_POINT('Ctrl Pts',(-4.37352103895722,0.00385464862035015,
42.848589891905));
#55605=CARTESIAN_POINT('Origin',(0.,0.,24.1514101080949));
#55606=CARTESIAN_POINT('',(-4.36973282931957,0.00384403733829788,40.651410108095));
#55607=CARTESIAN_POINT('',(-4.36602112377814,-0.00227682230535847,40.848589891905));
#55608=CARTESIAN_POINT('',(-4.372,3.82579154166093E-12,24.1514101080949));
#55609=CARTESIAN_POINT('Ctrl Pts',(-4.36973282931958,0.00384403733829777,
40.651410108095));
#55610=CARTESIAN_POINT('Ctrl Pts',(-4.36094828703741,-1.03504959539527,
40.6891903683526));
#55611=CARTESIAN_POINT('Ctrl Pts',(-3.47031004267523,-3.54269738683393,
40.7798908826921));
#55612=CARTESIAN_POINT('Ctrl Pts',(0.715283237582617,-5.11765799033974,
40.9235116511136));
#55613=CARTESIAN_POINT('Ctrl Pts',(4.6874579011302,-2.17480846080452,41.0822724133595));
#55614=CARTESIAN_POINT('Ctrl Pts',(4.36952791329752,2.75849220244841,41.2410331756054));
#55615=CARTESIAN_POINT('Ctrl Pts',(0.052472510246957,5.16713654277911,41.3997939378513));
#55616=CARTESIAN_POINT('Ctrl Pts',(-3.70859131189293,3.16775466245737,41.5365862486812));
#55617=CARTESIAN_POINT('Ctrl Pts',(-4.36224856298441,0.851164468294318,
41.620458305429));
#55618=CARTESIAN_POINT('Ctrl Pts',(-4.3656795540281,-0.00194869704108112,
41.651410108095));
#55619=CARTESIAN_POINT('Ctrl Pts',(-4.36602112377814,-0.00227682230535861,
40.848589891905));
#55620=CARTESIAN_POINT('Ctrl Pts',(-4.36876880712171,-0.584227201261346,
40.8697077686591));
#55621=CARTESIAN_POINT('Ctrl Pts',(-3.98963601281,-2.62107929020566,40.9437458994952));
#55622=CARTESIAN_POINT('Ctrl Pts',(-0.90075771530386,-5.08828946819429,
41.0707042844132));
#55623=CARTESIAN_POINT('Ctrl Pts',(3.78626858625262,-3.51656428443629,41.2294650466591));
#55624=CARTESIAN_POINT('Ctrl Pts',(5.00798622459088,1.27362794729248,41.3882258089049));
#55625=CARTESIAN_POINT('Ctrl Pts',(1.64624189925253,4.89815697818699,41.5469865711509));
#55626=CARTESIAN_POINT('Ctrl Pts',(-3.0594815075565,4.0684328488748,41.7004412654842));
#55627=CARTESIAN_POINT('Ctrl Pts',(-4.36854383389695,1.30092803749072,41.8009757057356));
#55628=CARTESIAN_POINT('Ctrl Pts',(-4.37739485101806,-0.00248321819134518,
41.8485898919051));
#55629=CARTESIAN_POINT('Origin',(0.,0.,24.1514101080949));
#55630=CARTESIAN_POINT('',(-4.37914188721017,-0.000342719191574727,39.651410108095));
#55631=CARTESIAN_POINT('',(-4.36909141260198,0.00371732487008336,39.848589891905));
#55632=CARTESIAN_POINT('',(-4.372,3.82579154166093E-12,24.1514101080949));
#55633=CARTESIAN_POINT('Ctrl Pts',(-4.37914188721017,-0.000342719191574457,
39.651410108095));
#55634=CARTESIAN_POINT('Ctrl Pts',(-4.37916257714185,-0.0187137896541573,
39.6520819231122));
#55635=CARTESIAN_POINT('Ctrl Pts',(-4.37073789868075,-1.48419245149001,
39.7056739922113));
#55636=CARTESIAN_POINT('Ctrl Pts',(-2.74752162183386,-4.3764344338297,39.8121863153924));
#55637=CARTESIAN_POINT('Ctrl Pts',(2.18656111288008,-4.68198717594309,39.9709470776383));
#55638=CARTESIAN_POINT('Ctrl Pts',(5.11943632770732,-0.702442241472902,
40.1297078398842));
#55639=CARTESIAN_POINT('Ctrl Pts',(3.36684704019806,3.9199992887709,40.2884686021301));
#55640=CARTESIAN_POINT('Ctrl Pts',(-1.46718350018236,4.95473773199425,40.4472293643759));
#55641=CARTESIAN_POINT('Ctrl Pts',(-4.12759825135317,2.28764036559584,40.5682098663642));
#55642=CARTESIAN_POINT('Ctrl Pts',(-4.37325313105903,0.420168410874277,
40.6362701142706));
#55643=CARTESIAN_POINT('Ctrl Pts',(-4.36973282931958,0.00384403733829777,
40.651410108095));
#55644=CARTESIAN_POINT('Ctrl Pts',(-4.36909141260198,0.0037173248700835,
39.848589891905));
#55645=CARTESIAN_POINT('Ctrl Pts',(-4.36087746473157,-1.01216450930882,
39.8855195775007));
#55646=CARTESIAN_POINT('Ctrl Pts',(-3.50202565789313,-3.49632888214117,
39.9753695171783));
#55647=CARTESIAN_POINT('Ctrl Pts',(0.6331436514814,-5.12846792818335,40.1181397109379));
#55648=CARTESIAN_POINT('Ctrl Pts',(4.65198839971611,-2.2496795555641,40.2769004731838));
#55649=CARTESIAN_POINT('Ctrl Pts',(4.41319126769477,2.68808426366416,40.4356612354296));
#55650=CARTESIAN_POINT('Ctrl Pts',(0.135306684796697,5.16563125618407,40.5944219976755));
#55651=CARTESIAN_POINT('Ctrl Pts',(-3.68091103301737,3.21474907678104,40.7320648831673));
#55652=CARTESIAN_POINT('Ctrl Pts',(-4.36188326164895,0.874108893605594,
40.8167875145772));
#55653=CARTESIAN_POINT('Ctrl Pts',(-4.36602112377814,-0.00227682230535861,
40.848589891905));
#55654=CARTESIAN_POINT('Origin',(0.,0.,24.1514101080949));
#55655=CARTESIAN_POINT('',(-4.36873305544013,-0.00362749675167218,38.651410108095));
#55656=CARTESIAN_POINT('',(-4.37917310725098,9.13219796030052E-5,38.848589891905));
#55657=CARTESIAN_POINT('',(-4.372,3.82579154166093E-12,24.1514101080949));
#55658=CARTESIAN_POINT('Ctrl Pts',(-4.36873305544013,-0.00362749675167234,
38.651410108095));
#55659=CARTESIAN_POINT('Ctrl Pts',(-4.37228988643661,-0.457161961038693,
38.6678937319537));
#55660=CARTESIAN_POINT('Ctrl Pts',(-4.0986296928328,-2.36257101965516,38.7372976098944));
#55661=CARTESIAN_POINT('Ctrl Pts',(-1.34123858177823,-4.99030384674165,
38.8596217419171));
#55662=CARTESIAN_POINT('Ctrl Pts',(3.46503780867414,-3.83347967263602,39.0183825041629));
#55663=CARTESIAN_POINT('Ctrl Pts',(5.10000575566994,0.831862193027325,39.1771432664089));
#55664=CARTESIAN_POINT('Ctrl Pts',(2.06729265337245,4.73585837007054,39.3359040286547));
#55665=CARTESIAN_POINT('Ctrl Pts',(-2.83663011433148,4.30727362250648,39.4939929758834));
#55666=CARTESIAN_POINT('Ctrl Pts',(-4.37753278856417,1.42841330898948,39.5991616690302));
#55667=CARTESIAN_POINT('Ctrl Pts',(-4.37914188721017,-0.000342719191574457,
39.651410108095));
#55668=CARTESIAN_POINT('Ctrl Pts',(-4.37917310725098,9.13219796029981E-5,
38.848589891905));
#55669=CARTESIAN_POINT('Ctrl Pts',(-4.37872965626048,-1.44211984317019,
38.9013313863422));
#55670=CARTESIAN_POINT('Ctrl Pts',(-2.81178331229755,-4.33225607926283,
39.0069931348614));
#55671=CARTESIAN_POINT('Ctrl Pts',(2.11121724282438,-4.71644102342194,39.1655751374625));
#55672=CARTESIAN_POINT('Ctrl Pts',(5.10751668218689,-0.784428145210908,
39.3243358997084));
#55673=CARTESIAN_POINT('Ctrl Pts',(3.42926084288352,3.86551733216684,39.4830966619543));
#55674=CARTESIAN_POINT('Ctrl Pts',(-1.38755926796319,4.97762327338117,39.6418574242002));
#55675=CARTESIAN_POINT('Ctrl Pts',(-4.1093944849834,2.33507192947434,39.7636885008504));
#55676=CARTESIAN_POINT('Ctrl Pts',(-4.37264805528242,0.443594561337992,
39.8325993234187));
#55677=CARTESIAN_POINT('Ctrl Pts',(-4.36909141260198,0.0037173248700835,
39.848589891905));
#55678=CARTESIAN_POINT('Origin',(0.,0.,24.1514101080949));
#55679=CARTESIAN_POINT('',(-4.36624352627694,0.00245771687439172,37.651410108095));
#55680=CARTESIAN_POINT('',(-4.36935764006,-0.00377501215838794,37.848589891905));
#55681=CARTESIAN_POINT('',(-4.372,3.82579154166093E-12,24.1514101080949));
#55682=CARTESIAN_POINT('Ctrl Pts',(-4.36624352627694,0.00245771687439181,
37.651410108095));
#55683=CARTESIAN_POINT('Ctrl Pts',(-4.36169382655995,-0.887401680305794,
37.6837055407953));
#55684=CARTESIAN_POINT('Ctrl Pts',(-3.66460952904662,-3.24195865307006,
37.7689212275775));
#55685=CARTESIAN_POINT('Ctrl Pts',(0.183308877707052,-5.16415058566349,
37.9070571684418));
#55686=CARTESIAN_POINT('Ctrl Pts',(4.43798296793759,-2.64695307709652,38.0658179306876));
#55687=CARTESIAN_POINT('Ctrl Pts',(4.63087948595682,2.29281673986369,38.2245786929335));
#55688=CARTESIAN_POINT('Ctrl Pts',(0.585453646372677,5.13413064150142,38.3833394551794));
#55689=CARTESIAN_POINT('Ctrl Pts',(-3.52014057613125,3.46939996827985,38.5256165935665));
#55690=CARTESIAN_POINT('Ctrl Pts',(-4.36087077121817,0.99889887186349,38.6149734778717));
#55691=CARTESIAN_POINT('Ctrl Pts',(-4.36873305544013,-0.00362749675167234,
38.651410108095));
#55692=CARTESIAN_POINT('Ctrl Pts',(-4.36935764006,-0.00377501215838787,
37.848589891905));
#55693=CARTESIAN_POINT('Ctrl Pts',(-4.37290446571934,-0.43375111631892,
37.8642229411018));
#55694=CARTESIAN_POINT('Ctrl Pts',(-4.11710236903147,-2.31513392579321,
37.9327762443806));
#55695=CARTESIAN_POINT('Ctrl Pts',(-1.42107210669624,-4.96815944202542,
38.0542498017413));
#55696=CARTESIAN_POINT('Ctrl Pts',(3.40313314014881,-3.88853944357485,38.2130105639872));
#55697=CARTESIAN_POINT('Ctrl Pts',(5.11268698707437,0.749990630619295,38.3717713262331));
#55698=CARTESIAN_POINT('Ctrl Pts',(2.14295353437204,4.70210637090854,38.5305320884789));
#55699=CARTESIAN_POINT('Ctrl Pts',(-2.78807645035559,4.35071073283309,38.6892928507248));
#55700=CARTESIAN_POINT('Ctrl Pts',(-4.37695363416618,1.45696557727882,38.7953121185335));
#55701=CARTESIAN_POINT('Ctrl Pts',(-4.37917461026378,0.0049794875180062,
38.8484111322603));
#55702=CARTESIAN_POINT('Ctrl Pts',(-4.37917310725098,9.13219796029981E-5,
38.848589891905));
#55703=CARTESIAN_POINT('Origin',(0.,0.,24.1514101080949));
#55704=CARTESIAN_POINT('',(-4.37768323182342,0.00228667983145002,36.651410108095));
#55705=CARTESIAN_POINT('',(-4.36587095680509,0.00214125659340675,36.848589891905));
#55706=CARTESIAN_POINT('',(-4.372,3.82579154166093E-12,24.1514101080949));
#55707=CARTESIAN_POINT('Ctrl Pts',(-4.37768323182342,0.00228667983144982,
36.651410108095));
#55708=CARTESIAN_POINT('Ctrl Pts',(-4.36931436006514,-1.31439298482965,
36.6995173496368));
#55709=CARTESIAN_POINT('Ctrl Pts',(-3.03668215072675,-4.09416581339981,
36.8005448452606));
#55710=CARTESIAN_POINT('Ctrl Pts',(1.69169298020808,-4.88264562268956,36.9544925949664));
#55711=CARTESIAN_POINT('Ctrl Pts',(5.01960663803976,-1.22702999775959,37.1132533572123));
#55712=CARTESIAN_POINT('Ctrl Pts',(3.75342297485632,3.55160096123927,37.2720141194582));
#55713=CARTESIAN_POINT('Ctrl Pts',(-0.94800804471325,5.07969823544803,37.430774881704));
#55714=CARTESIAN_POINT('Ctrl Pts',(-4.00191688963235,2.59358013793749,37.5572402112497));
#55715=CARTESIAN_POINT('Ctrl Pts',(-4.36914909948521,0.570748326013101,
37.6307852867133));
#55716=CARTESIAN_POINT('Ctrl Pts',(-4.36624352627694,0.00245771687439181,
37.651410108095));
#55717=CARTESIAN_POINT('Ctrl Pts',(-4.36587095680509,0.00214125659340626,
36.848589891905));
#55718=CARTESIAN_POINT('Ctrl Pts',(-4.36203103509102,-0.864466812036311,
36.8800347499434));
#55719=CARTESIAN_POINT('Ctrl Pts',(-3.6926137083843,-3.19500429871341,36.9643998620637));
#55720=CARTESIAN_POINT('Ctrl Pts',(0.100492274349119,-5.16642579319712,
37.101685228266));
#55721=CARTESIAN_POINT('Ctrl Pts',(4.39497597774354,-2.71776384714963,37.2604459905118));
#55722=CARTESIAN_POINT('Ctrl Pts',(4.66704342001788,2.21827858698683,37.4192067527577));
#55723=CARTESIAN_POINT('Ctrl Pts',(0.66769016759438,5.12408470011126,37.5779675150036));
#55724=CARTESIAN_POINT('Ctrl Pts',(-3.48876670478196,3.51583248140767,37.7210952280527));
#55725=CARTESIAN_POINT('Ctrl Pts',(-4.36089792030941,1.02178352666142,37.8113026870198));
#55726=CARTESIAN_POINT('Ctrl Pts',(-4.36935764006,-0.00377501215838787,
37.848589891905));
#55727=CARTESIAN_POINT('Origin',(0.,0.,24.1514101080949));
#55728=CARTESIAN_POINT('',(-4.37311107145795,-0.00391014173522758,35.651410108095));
#55729=CARTESIAN_POINT('',(-4.3771739373938,0.00261949572194539,35.848589891905));
#55730=CARTESIAN_POINT('',(-4.372,3.82579154166093E-12,24.1514101080949));
#55731=CARTESIAN_POINT('Ctrl Pts',(-4.37311107145795,-0.00391014173522778,
35.651410108095));
#55732=CARTESIAN_POINT('Ctrl Pts',(-4.3758959220056,-0.305762745961795,
35.6624089043964));
#55733=CARTESIAN_POINT('Ctrl Pts',(-4.20975035875682,-2.05692106559916,
35.7263279547798));
#55734=CARTESIAN_POINT('Ctrl Pts',(-1.84908860800444,-4.8252383087059,35.8431672592452));
#55735=CARTESIAN_POINT('Ctrl Pts',(3.05091116183891,-4.17061080641931,36.0019280214911));
#55736=CARTESIAN_POINT('Ctrl Pts',(5.15862384507246,0.301087098868051,36.1606887837369));
#55737=CARTESIAN_POINT('Ctrl Pts',(2.54500641307862,4.49722089444621,36.3194495459828));
#55738=CARTESIAN_POINT('Ctrl Pts',(-2.39787862639785,4.5773607580263,36.4782103082287));
#55739=CARTESIAN_POINT('Ctrl Pts',(-4.31337783157312,1.71331867151843,36.5888638289328));
#55740=CARTESIAN_POINT('Ctrl Pts',(-4.37852051709334,0.134017278681583,
36.6465970955549));
#55741=CARTESIAN_POINT('Ctrl Pts',(-4.37768323182342,0.00228667983144982,
36.651410108095));
#55742=CARTESIAN_POINT('Ctrl Pts',(-4.3771739373938,0.00261949572194524,
35.848589891905));
#55743=CARTESIAN_POINT('Ctrl Pts',(-4.36801132265503,-1.29117660831409,
35.8958465587849));
#55744=CARTESIAN_POINT('Ctrl Pts',(-3.07587918570516,-4.04972946385307,
35.9960234797468));
#55745=CARTESIAN_POINT('Ctrl Pts',(1.61319569609569,-4.90913982484862,36.1491206547906));
#55746=CARTESIAN_POINT('Ctrl Pts',(4.99928949022287,-1.30734798992603,36.3078814170365));
#55747=CARTESIAN_POINT('Ctrl Pts',(3.80988083761225,3.49096865884117,36.4666421792824));
#55748=CARTESIAN_POINT('Ctrl Pts',(-0.866447131906533,5.09424415801081,
36.6254029415283));
#55749=CARTESIAN_POINT('Ctrl Pts',(-3.9806269029927,2.64101706972627,36.7527188457358));
#55750=CARTESIAN_POINT('Ctrl Pts',(-4.36849344724489,0.59399482660225,36.8271144958614));
#55751=CARTESIAN_POINT('Ctrl Pts',(-4.36587095680509,0.00214125659340626,
36.848589891905));
#55752=CARTESIAN_POINT('Origin',(0.,0.,24.1514101080949));
#55753=CARTESIAN_POINT('',(-4.36484181559087,0.000158569877717519,34.651410108095));
#55754=CARTESIAN_POINT('',(-4.37381658707025,-0.00380592486605935,34.848589891905));
#55755=CARTESIAN_POINT('',(-4.372,3.82579154166093E-12,24.1514101080949));
#55756=CARTESIAN_POINT('Ctrl Pts',(-4.36484181559087,0.000158569877717965,
34.651410108095));
#55757=CARTESIAN_POINT('Ctrl Pts',(-4.36460260997581,-0.739166555623858,
34.6782207132379));
#55758=CARTESIAN_POINT('Ctrl Pts',(-3.83552704168218,-2.93813387262851,
34.7579515724629));
#55759=CARTESIAN_POINT('Ctrl Pts',(-0.350623086089188,-5.15549385292585,
34.8906026857698));
#55760=CARTESIAN_POINT('Ctrl Pts',(4.14111364246891,-3.09083018236409,35.0493634480157));
#55761=CARTESIAN_POINT('Ctrl Pts',(4.84277667347619,1.80265568173448,35.2081242102616));
#55762=CARTESIAN_POINT('Ctrl Pts',(1.11218256837853,5.0462960030749,35.3668849725075));
#55763=CARTESIAN_POINT('Ctrl Pts',(-3.30734354987895,3.76666274637145,35.5146469384519));
#55764=CARTESIAN_POINT('Ctrl Pts',(-4.36249672862818,1.14658859078299,35.6094886503144));
#55765=CARTESIAN_POINT('Ctrl Pts',(-4.37311107145795,-0.00391014173522778,
35.651410108095));
#55766=CARTESIAN_POINT('Ctrl Pts',(-4.37381658707025,-0.00380592486605963,
34.848589891905));
#55767=CARTESIAN_POINT('Ctrl Pts',(-4.37636167316891,-0.282199643018631,
34.8587381135445));
#55768=CARTESIAN_POINT('Ctrl Pts',(-4.22532647145104,-2.00959079533273,
34.921806589266));
#55769=CARTESIAN_POINT('Ctrl Pts',(-1.92621049372714,-4.7949731289833,35.0377953190694));
#55770=CARTESIAN_POINT('Ctrl Pts',(2.98365473640471,-4.21898786295316,35.1965560813153));
#55771=CARTESIAN_POINT('Ctrl Pts',(5.16278801485838,0.21834396591395,35.3553168435612));
#55772=CARTESIAN_POINT('Ctrl Pts',(2.61678000270041,4.45584072777334,35.514077605807));
#55773=CARTESIAN_POINT('Ctrl Pts',(-2.32418499851494,4.61521595014736,35.672838368053));
#55774=CARTESIAN_POINT('Ctrl Pts',(-4.30043031041834,1.76047520998047,35.7843424634189));
#55775=CARTESIAN_POINT('Ctrl Pts',(-4.37827205266511,0.157677555053939,
35.842926304703));
#55776=CARTESIAN_POINT('Ctrl Pts',(-4.3771739373938,0.00261949572194524,
35.848589891905));
#55777=CARTESIAN_POINT('Origin',(0.,0.,24.1514101080949));
#55778=CARTESIAN_POINT('',(-4.37369305382679,0.00382718076316987,33.651410108095));
#55779=CARTESIAN_POINT('',(-4.36484727915486,-0.000226203520788115,33.848589891905));
#55780=CARTESIAN_POINT('',(-4.372,3.82579154166093E-12,24.1514101080949));
#55781=CARTESIAN_POINT('Ctrl Pts',(-4.37369305382679,0.00382718076316957,
33.651410108095));
#55782=CARTESIAN_POINT('Ctrl Pts',(-4.36297801900768,-1.16550827733193,
33.6940325220795));
#55783=CARTESIAN_POINT('Ctrl Pts',(-3.27833228748252,-3.80423885928109,
33.789575190146));
#55784=CARTESIAN_POINT('Ctrl Pts',(1.17875881138994,-5.0311610072254,33.9380381122944));
#55785=CARTESIAN_POINT('Ctrl Pts',(4.86617124330449,-1.73851397661661,34.0967988745404));
#55786=CARTESIAN_POINT('Ctrl Pts',(4.09991511421076,3.14527414899259,34.2555596367862));
#55787=CARTESIAN_POINT('Ctrl Pts',(-0.418708560946466,5.15041129979394,
34.4143203990322));
#55788=CARTESIAN_POINT('Ctrl Pts',(-3.85575329743435,2.89916044399897,34.5462705561351));
#55789=CARTESIAN_POINT('Ctrl Pts',(-4.36507476723817,0.720154234863851,
34.625300459156));
#55790=CARTESIAN_POINT('Ctrl Pts',(-4.36484181559087,0.000158569877717965,
34.651410108095));
#55791=CARTESIAN_POINT('Ctrl Pts',(-4.36484727915486,-0.000226203520787838,
33.848589891905));
#55792=CARTESIAN_POINT('Ctrl Pts',(-4.36517770844991,-0.716093813355663,
33.8745499223861));
#55793=CARTESIAN_POINT('Ctrl Pts',(-3.86002428520416,-2.89083849180258,
33.9534302069491));
#55794=CARTESIAN_POINT('Ctrl Pts',(-0.433232286323001,-5.1492100326073,
34.085230745594));
#55795=CARTESIAN_POINT('Ctrl Pts',(4.0910284465022,-3.15682442079478,34.24399150784));
#55796=CARTESIAN_POINT('Ctrl Pts',(4.87105498299758,1.72478332738662,34.4027522700858));
#55797=CARTESIAN_POINT('Ctrl Pts',(1.1929432107418,5.02781669015105,34.5615130323318));
#55798=CARTESIAN_POINT('Ctrl Pts',(-3.27208568972255,3.81224566198089,34.7101255729381));
#55799=CARTESIAN_POINT('Ctrl Pts',(-4.36308973176021,1.16954893154173,34.8058178594626));
#55800=CARTESIAN_POINT('Ctrl Pts',(-4.37381658707025,-0.00380592486605963,
34.848589891905));
#55801=CARTESIAN_POINT('Origin',(0.,0.,24.1514101080949));
#55802=CARTESIAN_POINT('',(-4.37726747931578,-0.00256312102853162,32.651410108095));
#55803=CARTESIAN_POINT('',(-4.37298639645094,0.00392429018828133,32.848589891905));
#55804=CARTESIAN_POINT('',(-4.372,3.82579154166093E-12,24.1514101080949));
#55805=CARTESIAN_POINT('Ctrl Pts',(-4.37726747931578,-0.0025631210285324,
32.651410108095));
#55806=CARTESIAN_POINT('Ctrl Pts',(-4.37831848753371,-0.153516427525766,
32.6569240768391));
#55807=CARTESIAN_POINT('Ctrl Pts',(-4.30273715326605,-1.7521779604483,32.7153582996652));
#55808=CARTESIAN_POINT('Ctrl Pts',(-2.33719172860392,-4.60864277632799,
32.8267127765732));
#55809=CARTESIAN_POINT('Ctrl Pts',(2.60420302889879,-4.4632028858578,32.9854735388192));
#55810=CARTESIAN_POINT('Ctrl Pts',(5.16215162793603,-0.232903383943239,
33.144234301065));
#55811=CARTESIAN_POINT('Ctrl Pts',(2.99554137711165,4.21055640908263,33.302995063311));
#55812=CARTESIAN_POINT('Ctrl Pts',(-1.91267984204806,4.80038636339596,33.4617558255568));
#55813=CARTESIAN_POINT('Ctrl Pts',(-4.22261792613804,2.01791460332865,33.5778941738182));
#55814=CARTESIAN_POINT('Ctrl Pts',(-4.37628187282812,0.286345894322504,
33.6411122679975));
#55815=CARTESIAN_POINT('Ctrl Pts',(-4.37369305382679,0.00382718076316957,
33.651410108095));
#55816=CARTESIAN_POINT('Ctrl Pts',(-4.37298639645094,0.00392429018828126,
32.848589891905));
#55817=CARTESIAN_POINT('Ctrl Pts',(-4.36240284050621,-1.14255230782506,
32.8903617312276));
#55818=CARTESIAN_POINT('Ctrl Pts',(-3.31348194711132,-3.75862865123049,
32.9850538246322));
#55819=CARTESIAN_POINT('Ctrl Pts',(1.09794640645064,-5.04941262548215,33.1326661721187));
#55820=CARTESIAN_POINT('Ctrl Pts',(4.83767356537879,-1.81630632015957,33.2914269343646));
#55821=CARTESIAN_POINT('Ctrl Pts',(4.14981410860918,3.07913900917197,33.4501876966104));
#55822=CARTESIAN_POINT('Ctrl Pts',(-0.336081978081961,5.15646226378366,
33.6089484588564));
#55823=CARTESIAN_POINT('Ctrl Pts',(-3.83116330074657,2.94644944182165,33.7417491906212));
#55824=CARTESIAN_POINT('Ctrl Pts',(-4.36450411901545,0.743222493270702,
33.8216296683041));
#55825=CARTESIAN_POINT('Ctrl Pts',(-4.36484727915486,-0.000226203520787838,
33.848589891905));
#55826=CARTESIAN_POINT('Origin',(0.,0.,24.1514101080949));
#55827=CARTESIAN_POINT('',(-4.36593258301536,-0.00219842154078257,31.651410108095));
#55828=CARTESIAN_POINT('',(-4.37776688532802,-0.00222515354369623,31.848589891905));
#55829=CARTESIAN_POINT('',(-4.372,3.82579154166093E-12,24.1514101080949));
#55830=CARTESIAN_POINT('Ctrl Pts',(-4.36593258301536,-0.00219842154078276,
31.651410108095));
#55831=CARTESIAN_POINT('Ctrl Pts',(-4.36860855649085,-0.589907775928666,
31.6727358856806));
#55832=CARTESIAN_POINT('Ctrl Pts',(-3.98440775127391,-2.63267349583233,
31.7469819173483));
#55833=CARTESIAN_POINT('Ctrl Pts',(-0.880810653343035,-5.09178023966167,
31.8741482030979));
#55834=CARTESIAN_POINT('Ctrl Pts',(3.80002027066033,-3.5016994957634,32.0329089653438));
#55835=CARTESIAN_POINT('Ctrl Pts',(5.00295656982363,1.29324358746212,32.1916697275897));
#55836=CARTESIAN_POINT('Ctrl Pts',(1.62703419898677,4.90457063680218,32.3504304898356));
#55837=CARTESIAN_POINT('Ctrl Pts',(-3.06903058869073,4.05756105615878,32.5036772833373));
#55838=CARTESIAN_POINT('Ctrl Pts',(-4.36823144777778,1.29525626325957,32.6040038227571));
#55839=CARTESIAN_POINT('Ctrl Pts',(-4.37726747931578,-0.0025631210285324,
32.651410108095));
#55840=CARTESIAN_POINT('Ctrl Pts',(-4.37776688532802,-0.00222515354369674,
31.848589891905));
#55841=CARTESIAN_POINT('Ctrl Pts',(-4.37856029699079,-0.129854311945594,
31.8532532859872));
#55842=CARTESIAN_POINT('Ctrl Pts',(-4.31561362407578,-1.70502699061033,
31.9108369341514));
#55843=CARTESIAN_POINT('Ctrl Pts',(-2.41077837014428,-4.57058003144683,
32.0213408363975));
#55844=CARTESIAN_POINT('Ctrl Pts',(2.53231309568674,-4.50438059662262,32.1801015986434));
#55845=CARTESIAN_POINT('Ctrl Pts',(5.15775426583447,-0.31563445167244,32.3388623608893));
#55846=CARTESIAN_POINT('Ctrl Pts',(3.06266118623515,4.16198998462816,32.4976231231351));
#55847=CARTESIAN_POINT('Ctrl Pts',(-1.83547296121064,4.83043405735769,32.6563838853811));
#55848=CARTESIAN_POINT('Ctrl Pts',(-4.20696559908301,2.06524898522119,32.7733728083043));
#55849=CARTESIAN_POINT('Ctrl Pts',(-4.37581102359723,0.309905468748449,
32.8374414771457));
#55850=CARTESIAN_POINT('Ctrl Pts',(-4.37298639645094,0.00392429018828126,
32.848589891905));
#55851=CARTESIAN_POINT('Origin',(0.,0.,24.1514101080949));
#55852=CARTESIAN_POINT('',(-4.36924553642194,0.00375164274966603,30.651410108095));
#55853=CARTESIAN_POINT('',(-4.36631454878401,-0.00251114173366096,30.848589891905));
#55854=CARTESIAN_POINT('',(-4.372,3.82579154166093E-12,24.1514101080949));
#55855=CARTESIAN_POINT('Ctrl Pts',(-4.36924553642194,0.00375164274966585,
30.651410108095));
#55856=CARTESIAN_POINT('Ctrl Pts',(-4.36088767272676,-1.01775802631581,
30.6885476945222));
#55857=CARTESIAN_POINT('Ctrl Pts',(-3.49432807348169,-3.50767273053874,
30.7786055350314));
#55858=CARTESIAN_POINT('Ctrl Pts',(0.653236365857992,-5.12594729451212,
30.9215836296226));
#55859=CARTESIAN_POINT('Ctrl Pts',(4.6607687206244,-2.23143190555148,31.0803443918685));
#55860=CARTESIAN_POINT('Ctrl Pts',(4.4026231771807,2.70535812338375,31.2391051541143));
#55861=CARTESIAN_POINT('Ctrl Pts',(0.115062422136807,5.16612176153803,31.3978659163603));
#55862=CARTESIAN_POINT('Ctrl Pts',(-3.68772820349694,3.20326873769824,31.5353009010205));
#55863=CARTESIAN_POINT('Ctrl Pts',(-4.36196808602404,0.868502274330174,
31.6198156315987));
#55864=CARTESIAN_POINT('Ctrl Pts',(-4.36593258301536,-0.00219842154078276,
31.651410108095));
#55865=CARTESIAN_POINT('Ctrl Pts',(-4.36631454878401,-0.0025111417336611,
30.848589891905));
#55866=CARTESIAN_POINT('Ctrl Pts',(-4.36926463444175,-0.566656242129838,
30.8690650948288));
#55867=CARTESIAN_POINT('Ctrl Pts',(-4.00561083840711,-2.58523495481153,
30.9424605518345));
#55868=CARTESIAN_POINT('Ctrl Pts',(-0.962330244988123,-5.07700449806455,
31.0687762629221));
#55869=CARTESIAN_POINT('Ctrl Pts',(3.74339174195905,-3.56217243267071,31.2275370251681));
#55870=CARTESIAN_POINT('Ctrl Pts',(5.02304726326813,1.21286865108392,31.3862977874139));
#55871=CARTESIAN_POINT('Ctrl Pts',(1.70545649826175,4.87785529780762,31.5450585496599));
#55872=CARTESIAN_POINT('Ctrl Pts',(-3.02972114369421,4.10196041210765,31.6991559178235));
#55873=CARTESIAN_POINT('Ctrl Pts',(-4.36955665156738,1.31848296597982,31.8003330319052));
#55874=CARTESIAN_POINT('Ctrl Pts',(-4.37776688532802,-0.00222515354369674,
31.848589891905));
#55875=CARTESIAN_POINT('Origin',(0.,0.,24.1514101080949));
#55876=CARTESIAN_POINT('',(-4.37917542201394,-1.48878467067329E-5,29.651410108095));
#55877=CARTESIAN_POINT('',(-4.36862654983539,0.00359793095617206,29.848589891905));
#55878=CARTESIAN_POINT('',(-4.372,3.82579154166093E-12,24.1514101080949));
#55879=CARTESIAN_POINT('Ctrl Pts',(-4.3791753974872,-1.48877958181532E-5,
29.651410108095));
#55880=CARTESIAN_POINT('Ctrl Pts',(-4.37917543773958,-0.000811749618496727,
29.6514392492818));
#55881=CARTESIAN_POINT('Ctrl Pts',(-4.37881439934298,-1.44870578249893,
29.7043886445506));
#55882=CARTESIAN_POINT('Ctrl Pts',(-2.80033535833003,-4.34283033250174,
29.8102582939013));
#55883=CARTESIAN_POINT('Ctrl Pts',(2.12968392236957,-4.70813124181331,29.9690190561473));
#55884=CARTESIAN_POINT('Ctrl Pts',(5.11055143098187,-0.764406630547101,
30.1277798183931));
#55885=CARTESIAN_POINT('Ctrl Pts',(3.41408616315334,3.87892628001712,30.286540580639));
#55886=CARTESIAN_POINT('Ctrl Pts',(-1.4070550442568,4.97214737476293,30.4453013428849));
#55887=CARTESIAN_POINT('Ctrl Pts',(-4.11388660080008,2.32347755138503,30.5669245187036));
#55888=CARTESIAN_POINT('Ctrl Pts',(-4.37279744697119,0.437871066329566,
30.6356274404402));
#55889=CARTESIAN_POINT('Ctrl Pts',(-4.36924553642194,0.00375164274966585,
30.651410108095));
#55890=CARTESIAN_POINT('Ctrl Pts',(-4.36862654983539,0.0035979309561724,
29.848589891905));
#55891=CARTESIAN_POINT('Ctrl Pts',(-4.36087365922317,-0.994873321808196,
29.8848769036703));
#55892=CARTESIAN_POINT('Ctrl Pts',(-3.52559867611562,-3.46122138486278,
29.9740841695176));
#55893=CARTESIAN_POINT('Ctrl Pts',(0.570971856938151,-5.13576141485164,
30.1162116894468));
#55894=CARTESIAN_POINT('Ctrl Pts',(4.62439484690811,-2.30586783557282,30.2749724516927));
#55895=CARTESIAN_POINT('Ctrl Pts',(4.44543041863472,2.63442642081081,30.4337332139386));
#55896=CARTESIAN_POINT('Ctrl Pts',(0.1978722839815,5.16361314708889,30.5924939761844));
#55897=CARTESIAN_POINT('Ctrl Pts',(-3.65962554388572,3.25021066517935,30.7307795355066));
#55898=CARTESIAN_POINT('Ctrl Pts',(-4.361639836624,0.891434413344724,30.8161448407468));
#55899=CARTESIAN_POINT('Ctrl Pts',(-4.36631454878401,-0.0025111417336611,
30.848589891905));
#55900=CARTESIAN_POINT('Origin',(0.,0.,24.1514101080949));
#55901=CARTESIAN_POINT('',(-4.36920210772109,-0.00374225457618444,28.651410108095));
#55902=CARTESIAN_POINT('',(-4.379125585284,0.000418740495046069,28.848589891905));
#55903=CARTESIAN_POINT('',(-4.372,3.82579154166093E-12,24.1514101080949));
#55904=CARTESIAN_POINT('Ctrl Pts',(-4.36920210772109,-0.00374225457618473,
28.651410108095));
#55905=CARTESIAN_POINT('Ctrl Pts',(-4.37275566211042,-0.439475723050513,
28.6672510581234));
#55906=CARTESIAN_POINT('Ctrl Pts',(-4.11263026215736,-2.3267277008933,28.7360122622337));
#55907=CARTESIAN_POINT('Ctrl Pts',(-1.40159165779937,-4.9736902589037,28.857693720426));
#55908=CARTESIAN_POINT('Ctrl Pts',(3.41834539873403,-3.87517318393326,29.0164544826719));
#55909=CARTESIAN_POINT('Ctrl Pts',(5.10970861334159,0.770020576487015,29.1752152449178));
#55910=CARTESIAN_POINT('Ctrl Pts',(2.12451027984608,4.71046807932676,29.3339760071637));
#55911=CARTESIAN_POINT('Ctrl Pts',(-2.80419982800075,4.33981931003669,29.4927076282227));
#55912=CARTESIAN_POINT('Ctrl Pts',(-4.37910233962271,1.44628545901738,29.5985189951998));
#55913=CARTESIAN_POINT('Ctrl Pts',(-4.3791753974872,-1.48877958181532E-5,
29.651410108095));
#55914=CARTESIAN_POINT('Ctrl Pts',(-4.379125585284,0.000418740495045835,
28.848589891905));
#55915=CARTESIAN_POINT('Ctrl Pts',(-4.37717920749743,-1.42426027511931,
28.9006887125119));
#55916=CARTESIAN_POINT('Ctrl Pts',(-2.84412638479826,-4.2996753084771,29.0057077872007));
#55917=CARTESIAN_POINT('Ctrl Pts',(2.05392820456428,-4.74166985111631,29.1636471159715));
#55918=CARTESIAN_POINT('Ctrl Pts',(5.09763950196961,-0.846242130327758,
29.3224078782173));
#55919=CARTESIAN_POINT('Ctrl Pts',(3.47583539931961,3.82369225364773,29.4811686404633));
#55920=CARTESIAN_POINT('Ctrl Pts',(-1.32715942194175,4.9940666821606,29.6399294027091));
#55921=CARTESIAN_POINT('Ctrl Pts',(-4.09533214146315,2.37091623060187,29.7624031531897));
#55922=CARTESIAN_POINT('Ctrl Pts',(-4.37218032023241,0.461277235079317,
29.8319566495884));
#55923=CARTESIAN_POINT('Ctrl Pts',(-4.36862654983539,0.0035979309561724,
29.848589891905));
#55924=CARTESIAN_POINT('Origin',(0.,0.,24.1514101080949));
#55925=CARTESIAN_POINT('',(-4.36594998909341,0.00221597220681413,27.651410108095));
#55926=CARTESIAN_POINT('',(-4.36984836444492,-0.00386263586949487,27.848589891905));
#55927=CARTESIAN_POINT('',(-4.372,3.82579154166093E-12,24.1514101080949));
#55928=CARTESIAN_POINT('Ctrl Pts',(-4.36594998909341,0.00221597220681394,
27.651410108095));
#55929=CARTESIAN_POINT('Ctrl Pts',(-4.36193991209169,-0.870076739562532,
27.6830628669649));
#55930=CARTESIAN_POINT('Ctrl Pts',(-3.68583197785541,-3.20648009630763,
27.7676358799168));
#55931=CARTESIAN_POINT('Ctrl Pts',(0.12074539761077,-5.16599709979471,27.9051291469506));
#55932=CARTESIAN_POINT('Ctrl Pts',(4.40558866999103,-2.70051724468854,28.0638899091966));
#55933=CARTESIAN_POINT('Ctrl Pts',(4.65831652566081,2.23654953809766,28.2226506714425));
#55934=CARTESIAN_POINT('Ctrl Pts',(0.647603546994949,5.12666253671564,28.3814114336883));
#55935=CARTESIAN_POINT('Ctrl Pts',(-3.49648913171247,3.50449301705117,28.5243312459059));
#55936=CARTESIAN_POINT('Ctrl Pts',(-4.36088421495349,1.0161898665986,28.6143308040414));
#55937=CARTESIAN_POINT('Ctrl Pts',(-4.36920210772109,-0.00374225457618473,
28.651410108095));
#55938=CARTESIAN_POINT('Ctrl Pts',(-4.36984836444492,-0.00386263586949508,
27.848589891905));
#55939=CARTESIAN_POINT('Ctrl Pts',(-4.37335795381477,-0.41604489030568,
27.8635802672715));
#55940=CARTESIAN_POINT('Ctrl Pts',(-4.13075387899131,-2.27929715120676,
27.9314908967199));
#55941=CARTESIAN_POINT('Ctrl Pts',(-1.48115027726835,-4.95058115072351,
28.0523217802503));
#55942=CARTESIAN_POINT('Ctrl Pts',(3.35577787359124,-3.92947861571792,28.2110825424961));
#55943=CARTESIAN_POINT('Ctrl Pts',(5.12139735341277,0.688001195909337,28.369843304742));
#55944=CARTESIAN_POINT('Ctrl Pts',(2.1997566305386,4.67580212267651,28.5286040669879));
#55945=CARTESIAN_POINT('Ctrl Pts',(-2.7351680780718,4.38416569184913,28.6873648292338));
#55946=CARTESIAN_POINT('Ctrl Pts',(-4.36882639464741,1.49245678983841,28.7940267708728));
#55947=CARTESIAN_POINT('Ctrl Pts',(-4.37915627350017,0.0228814185571984,
28.8477684584299));
#55948=CARTESIAN_POINT('Ctrl Pts',(-4.379125585284,0.000418740495045835,
28.848589891905));
#55949=CARTESIAN_POINT('Origin',(0.,0.,24.1514101080949));
#55950=CARTESIAN_POINT('',(-4.37688026104952,0.00226901643694793,26.651410108095));
#55951=CARTESIAN_POINT('',(-4.36558297706963,0.00185075076461538,26.848589891905));
#55952=CARTESIAN_POINT('',(-4.372,3.82579154166093E-12,24.1514101080949));
#55953=CARTESIAN_POINT('Ctrl Pts',(-4.37688026104952,0.00226901643694839,
26.651410108095));
#55954=CARTESIAN_POINT('Ctrl Pts',(-4.36778028862692,-1.29719233300268,
26.6988746758065));
#55955=CARTESIAN_POINT('Ctrl Pts',(-3.06703503858937,-4.06017418671544,
26.7992594975999));
#55956=CARTESIAN_POINT('Ctrl Pts',(1.63279456941769,-4.90302026906412,26.9525645734753));
#55957=CARTESIAN_POINT('Ctrl Pts',(5.00417945325775,-1.28762125191842,27.1113253357213));
#55958=CARTESIAN_POINT('Ctrl Pts',(3.79627275763131,3.50580663842047,27.2700860979671));
#55959=CARTESIAN_POINT('Ctrl Pts',(-0.886457053099411,5.09084367591115,
27.428846860213));
#55960=CARTESIAN_POINT('Ctrl Pts',(-3.98586478860146,2.62941579049566,27.5559548635889));
#55961=CARTESIAN_POINT('Ctrl Pts',(-4.3686443606578,0.588309625125352,27.6301426128829));
#55962=CARTESIAN_POINT('Ctrl Pts',(-4.36594998909341,0.00221597220681394,
27.651410108095));
#55963=CARTESIAN_POINT('Ctrl Pts',(-4.36558297706963,0.00185075076461511,
26.848589891905));
#55964=CARTESIAN_POINT('Ctrl Pts',(-4.36229437398082,-0.847147845875526,
26.879392076113));
#55965=CARTESIAN_POINT('Ctrl Pts',(-3.7134735047561,-3.15941742864277,26.963114514403));
#55966=CARTESIAN_POINT('Ctrl Pts',(0.037946527963305,-5.16730646950401,
27.0997572067749));
#55967=CARTESIAN_POINT('Ctrl Pts',(4.36170657063856,-2.77078223288025,27.2585179690208));
#55968=CARTESIAN_POINT('Ctrl Pts',(4.69358555482947,2.16156853417802,27.4172787312667));
#55969=CARTESIAN_POINT('Ctrl Pts',(0.729706757950081,5.11562647870316,27.5760394935125));
#55970=CARTESIAN_POINT('Ctrl Pts',(-3.46466751885718,3.55083973542589,27.719809880392));
#55971=CARTESIAN_POINT('Ctrl Pts',(-4.36096811322469,1.03907475143884,27.8106600131895));
#55972=CARTESIAN_POINT('Ctrl Pts',(-4.36984836444492,-0.00386263586949508,
27.848589891905));
#55973=CARTESIAN_POINT('Ctrl Pts',(-1.91898364243938,3.92834389788497,25.6709103465619));
#55974=CARTESIAN_POINT('Ctrl Pts',(-2.57208606313318,3.60930541889036,25.6973704736029));
#55975=CARTESIAN_POINT('Ctrl Pts',(-3.70615701990389,2.63929385761509,25.7502907276849));
#55976=CARTESIAN_POINT('Ctrl Pts',(-4.81803798679934,-0.15958129715831,
25.8561312358487));
#55977=CARTESIAN_POINT('Ctrl Pts',(-3.30234769881301,-3.97407004593024,
25.9884318710537));
#55978=CARTESIAN_POINT('Ctrl Pts',(1.55593458522165,-4.93043777696371,26.1471926332996));
#55979=CARTESIAN_POINT('Ctrl Pts',(4.98187809541805,-1.36671674862893,26.3059533955455));
#55980=CARTESIAN_POINT('Ctrl Pts',(3.85252000415521,3.44398917781397,26.4647141577913));
#55981=CARTESIAN_POINT('Ctrl Pts',(-0.805001512196143,5.10466442465425,
26.6234749200372));
#55982=CARTESIAN_POINT('Ctrl Pts',(-4.72460311480109,2.09234479401288,26.7822356822831));
#55983=CARTESIAN_POINT('Ctrl Pts',(-4.32070810303542,-2.83440458431113,
26.940996444529));
#55984=CARTESIAN_POINT('Ctrl Pts',(0.037946527963305,-5.16730646950401,
27.0997572067749));
#55985=CARTESIAN_POINT('Ctrl Pts',(4.36170657063856,-2.77078223288025,27.2585179690208));
#55986=CARTESIAN_POINT('Ctrl Pts',(4.69358555482947,2.16156853417802,27.4172787312667));
#55987=CARTESIAN_POINT('Ctrl Pts',(0.729706757950081,5.11562647870316,27.5760394935125));
#55988=CARTESIAN_POINT('Ctrl Pts',(-3.90199850336257,3.38768554797952,27.7348002557585));
#55989=CARTESIAN_POINT('Ctrl Pts',(-4.96248778940575,-1.44075757294651,
27.8935610180043));
#55990=CARTESIAN_POINT('Ctrl Pts',(-1.48115027726835,-4.95058115072351,
28.0523217802503));
#55991=CARTESIAN_POINT('Ctrl Pts',(3.35577787359124,-3.92947861571792,28.2110825424961));
#55992=CARTESIAN_POINT('Ctrl Pts',(5.12139735341277,0.688001195909337,28.369843304742));
#55993=CARTESIAN_POINT('Ctrl Pts',(2.1997566305386,4.67580212267651,28.5286040669879));
#55994=CARTESIAN_POINT('Ctrl Pts',(-2.7351680780718,4.38416569184913,28.6873648292338));
#55995=CARTESIAN_POINT('Ctrl Pts',(-5.16678366281907,0.0800071286185968,
28.8461255914797));
#55996=CARTESIAN_POINT('Ctrl Pts',(-2.86960088841888,-4.29737651997417,
29.0048863537256));
#55997=CARTESIAN_POINT('Ctrl Pts',(2.05392820456428,-4.74166985111631,29.1636471159715));
#55998=CARTESIAN_POINT('Ctrl Pts',(5.09763950196961,-0.846242130327758,
29.3224078782173));
#55999=CARTESIAN_POINT('Ctrl Pts',(3.47583539931961,3.82369225364773,29.4811686404633));
#56000=CARTESIAN_POINT('Ctrl Pts',(-1.32715942194175,4.9940666821606,29.6399294027091));
#56001=CARTESIAN_POINT('Ctrl Pts',(-4.9154974066526,1.59371874196162,29.798690164955));
#56002=CARTESIAN_POINT('Ctrl Pts',(-4.00502201634919,-3.26524927403143,
29.9574509272009));
#56003=CARTESIAN_POINT('Ctrl Pts',(0.570971856938151,-5.13576141485164,
30.1162116894468));
#56004=CARTESIAN_POINT('Ctrl Pts',(4.62439484690811,-2.30586783557282,30.2749724516927));
#56005=CARTESIAN_POINT('Ctrl Pts',(4.44543041863472,2.63442642081081,30.4337332139386));
#56006=CARTESIAN_POINT('Ctrl Pts',(0.1978722839815,5.16361314708889,30.5924939761844));
#56007=CARTESIAN_POINT('Ctrl Pts',(-4.23078460916092,2.96690339662622,30.7512547384304));
#56008=CARTESIAN_POINT('Ctrl Pts',(-4.7872981969476,-1.94520696772118,30.9100155006763));
#56009=CARTESIAN_POINT('Ctrl Pts',(-0.962330244988123,-5.07700449806455,
31.0687762629221));
#56010=CARTESIAN_POINT('Ctrl Pts',(3.74339174195905,-3.56217243267071,31.2275370251681));
#56011=CARTESIAN_POINT('Ctrl Pts',(5.02304726326813,1.21286865108392,31.3862977874139));
#56012=CARTESIAN_POINT('Ctrl Pts',(1.70545649826175,4.87785529780762,31.5450585496599));
#56013=CARTESIAN_POINT('Ctrl Pts',(-3.17302014780288,4.07847977994959,31.7038193119056));
#56014=CARTESIAN_POINT('Ctrl Pts',(-5.14745183343486,-0.453645011306304,
31.8625800741516));
#56015=CARTESIAN_POINT('Ctrl Pts',(-2.41077837014428,-4.57058003144683,
32.0213408363975));
#56016=CARTESIAN_POINT('Ctrl Pts',(2.53231309568674,-4.50438059662262,32.1801015986434));
#56017=CARTESIAN_POINT('Ctrl Pts',(5.15775426583447,-0.31563445167244,32.3388623608893));
#56018=CARTESIAN_POINT('Ctrl Pts',(3.06266118623515,4.16198998462816,32.4976231231351));
#56019=CARTESIAN_POINT('Ctrl Pts',(-1.83547296121064,4.83043405735769,32.6563838853811));
#56020=CARTESIAN_POINT('Ctrl Pts',(-5.05372618930481,1.07791733326401,32.8151446476269));
#56021=CARTESIAN_POINT('Ctrl Pts',(-3.64665484087083,-3.66114225964655,
32.9739054098729));
#56022=CARTESIAN_POINT('Ctrl Pts',(1.09794640645064,-5.04941262548215,33.1326661721187));
#56023=CARTESIAN_POINT('Ctrl Pts',(4.83767356537879,-1.81630632015957,33.2914269343646));
#56024=CARTESIAN_POINT('Ctrl Pts',(4.14981410860918,3.07913900917197,33.4501876966104));
#56025=CARTESIAN_POINT('Ctrl Pts',(-0.336081978081961,5.15646226378366,
33.6089484588564));
#56026=CARTESIAN_POINT('Ctrl Pts',(-4.51438557267483,2.51443374838985,33.7677092211023));
#56027=CARTESIAN_POINT('Ctrl Pts',(-4.56098559745287,-2.42888133790924,
33.9264699833482));
#56028=CARTESIAN_POINT('Ctrl Pts',(-0.433232286323001,-5.1492100326073,
34.085230745594));
#56029=CARTESIAN_POINT('Ctrl Pts',(4.0910284465022,-3.15682442079478,34.24399150784));
#56030=CARTESIAN_POINT('Ctrl Pts',(4.87105498299758,1.72478332738662,34.4027522700858));
#56031=CARTESIAN_POINT('Ctrl Pts',(1.1929432107418,5.02781669015105,34.5615130323318));
#56032=CARTESIAN_POINT('Ctrl Pts',(-3.5769866269097,3.72923864142877,34.7202737945776));
#56033=CARTESIAN_POINT('Ctrl Pts',(-5.07314904313429,-0.982452523006609,
34.8790345568235));
#56034=CARTESIAN_POINT('Ctrl Pts',(-1.92621049372714,-4.7949731289833,35.0377953190694));
#56035=CARTESIAN_POINT('Ctrl Pts',(2.98365473640471,-4.21898786295316,35.1965560813153));
#56036=CARTESIAN_POINT('Ctrl Pts',(5.16278801485838,0.21834396591395,35.3553168435612));
#56037=CARTESIAN_POINT('Ctrl Pts',(2.61678000270041,4.45584072777334,35.514077605807));
#56038=CARTESIAN_POINT('Ctrl Pts',(-2.32418499851494,4.61521595014736,35.672838368053));
#56039=CARTESIAN_POINT('Ctrl Pts',(-5.13798489593422,0.55060456133973,35.8315991302988));
#56040=CARTESIAN_POINT('Ctrl Pts',(-3.24934407480239,-4.01793694044132,
35.9903598925447));
#56041=CARTESIAN_POINT('Ctrl Pts',(1.61319569609569,-4.90913982484862,36.1491206547906));
#56042=CARTESIAN_POINT('Ctrl Pts',(4.99928949022287,-1.30734798992603,36.3078814170365));
#56043=CARTESIAN_POINT('Ctrl Pts',(3.80988083761225,3.49096865884117,36.4666421792824));
#56044=CARTESIAN_POINT('Ctrl Pts',(-0.866447131906533,5.09424415801081,
36.6254029415283));
#56045=CARTESIAN_POINT('Ctrl Pts',(-4.74977622033223,2.03511179805508,36.7841637037742));
#56046=CARTESIAN_POINT('Ctrl Pts',(-4.28596502810612,-2.88661704277997,
36.94292446602));
#56047=CARTESIAN_POINT('Ctrl Pts',(0.100492274349119,-5.16642579319712,
37.101685228266));
#56048=CARTESIAN_POINT('Ctrl Pts',(4.39497597774354,-2.71776384714963,37.2604459905118));
#56049=CARTESIAN_POINT('Ctrl Pts',(4.66704342001788,2.21827858698683,37.4192067527577));
#56050=CARTESIAN_POINT('Ctrl Pts',(0.66769016759438,5.12408470011126,37.5779675150036));
#56051=CARTESIAN_POINT('Ctrl Pts',(-3.9427535210732,3.34017197848871,37.7367282772495));
#56052=CARTESIAN_POINT('Ctrl Pts',(-4.94466875428017,-1.50076816472822,
37.8954890394954));
#56053=CARTESIAN_POINT('Ctrl Pts',(-1.42107210669624,-4.96815944202542,
38.0542498017413));
#56054=CARTESIAN_POINT('Ctrl Pts',(3.40313314014881,-3.88853944357485,38.2130105639872));
#56055=CARTESIAN_POINT('Ctrl Pts',(5.11268698707437,0.749990630619295,38.3717713262331));
#56056=CARTESIAN_POINT('Ctrl Pts',(2.14295353437204,4.70210637090854,38.5305320884789));
#56057=CARTESIAN_POINT('Ctrl Pts',(-2.78807645035559,4.35071073283309,38.6892928507248));
#56058=CARTESIAN_POINT('Ctrl Pts',(-5.16737370481374,0.0174117378790549,
38.8480536129707));
#56059=CARTESIAN_POINT('Ctrl Pts',(-2.81733270514135,-4.33182301143032,
39.0068143752166));
#56060=CARTESIAN_POINT('Ctrl Pts',(2.11121724282438,-4.71644102342194,39.1655751374625));
#56061=CARTESIAN_POINT('Ctrl Pts',(5.10751668218689,-0.784428145210908,
39.3243358997084));
#56062=CARTESIAN_POINT('Ctrl Pts',(3.42926084288352,3.86551733216684,39.4830966619543));
#56063=CARTESIAN_POINT('Ctrl Pts',(-1.38755926796319,4.97762327338117,39.6418574242002));
#56064=CARTESIAN_POINT('Ctrl Pts',(-4.93444275322028,1.53405635131447,39.8006181864461));
#56065=CARTESIAN_POINT('Ctrl Pts',(-3.96517350621375,-3.31352580183661,
39.959378948692));
#56066=CARTESIAN_POINT('Ctrl Pts',(0.6331436514814,-5.12846792818335,40.1181397109379));
#56067=CARTESIAN_POINT('Ctrl Pts',(4.65198839971611,-2.2496795555641,40.2769004731838));
#56068=CARTESIAN_POINT('Ctrl Pts',(4.41319126769477,2.68808426366416,40.4356612354296));
#56069=CARTESIAN_POINT('Ctrl Pts',(0.135306684796697,5.16563125618407,40.5944219976755));
#56070=CARTESIAN_POINT('Ctrl Pts',(-4.26641470902384,2.91543473678309,40.7531827599214));
#56071=CARTESIAN_POINT('Ctrl Pts',(-4.7633830418116,-2.00305670683536,40.9119435221673));
#56072=CARTESIAN_POINT('Ctrl Pts',(-0.90075771530386,-5.08828946819429,
41.0707042844132));
#56073=CARTESIAN_POINT('Ctrl Pts',(3.78626858625262,-3.51656428443629,41.2294650466591));
#56074=CARTESIAN_POINT('Ctrl Pts',(5.00798622459088,1.27362794729248,41.3882258089049));
#56075=CARTESIAN_POINT('Ctrl Pts',(1.64624189925253,4.89815697818699,41.5469865711509));
#56076=CARTESIAN_POINT('Ctrl Pts',(-3.22219329739529,4.03974312649174,41.7057473333967));
#56077=CARTESIAN_POINT('Ctrl Pts',(-5.14157876509112,-0.515967030129218,
41.8645080956427));
#56078=CARTESIAN_POINT('Ctrl Pts',(-2.35523429540729,-4.59944840035779,
42.0232688578885));
#56079=CARTESIAN_POINT('Ctrl Pts',(2.58669254300161,-4.47337410259821,42.1820296201345));
#56080=CARTESIAN_POINT('Ctrl Pts',(5.16119935450289,-0.253131185149624,
42.3407903823802));
#56081=CARTESIAN_POINT('Ctrl Pts',(3.01201886587614,4.19878512494061,42.4995511446263));
#56082=CARTESIAN_POINT('Ctrl Pts',(-1.89385329211466,4.80784503512363,42.6583119068721));
#56083=CARTESIAN_POINT('Ctrl Pts',(-5.0664130686601,1.01661831162269,42.817072669118));
#56084=CARTESIAN_POINT('Ctrl Pts',(-3.6020368491656,-3.70504854368597,42.9758334313639));
#56085=CARTESIAN_POINT('Ctrl Pts',(1.15903352033341,-5.0357417996319,43.1345941936098));
#56086=CARTESIAN_POINT('Ctrl Pts',(4.85932100888344,-1.75757034181863,43.2933549558556));
#56087=CARTESIAN_POINT('Ctrl Pts',(4.11220948021047,3.12918317851219,43.4521157181016));
#56088=CARTESIAN_POINT('Ctrl Pts',(-0.398521773825228,5.15201267172389,
43.6108764803474));
#56089=CARTESIAN_POINT('Ctrl Pts',(-4.54451372744996,2.45956279749778,43.7696372425933));
#56090=CARTESIAN_POINT('Ctrl Pts',(-4.53122790373328,-2.48395407732217,
43.9283980048393));
#56091=CARTESIAN_POINT('Ctrl Pts',(-0.370823894361365,-5.15408030721166,
44.0871587670851));
#56092=CARTESIAN_POINT('Ctrl Pts',(4.12896947009338,-3.10703480650815,44.245919529331));
#56093=CARTESIAN_POINT('Ctrl Pts',(4.84980385450403,1.78366385472551,44.4046802915768));
#56094=CARTESIAN_POINT('Ctrl Pts',(1.13194961208497,5.04189887339256,44.5634410538228));
#56095=CARTESIAN_POINT('Ctrl Pts',(-3.62189949116538,3.68563403632435,44.7222018160687));
#56096=CARTESIAN_POINT('Ctrl Pts',(-5.06087554774066,-1.0438356499454,44.8809625783145));
#56097=CARTESIAN_POINT('Ctrl Pts',(-1.8679837165673,-4.81795506501003,45.0397233405604));
#56098=CARTESIAN_POINT('Ctrl Pts',(3.03454387031403,-4.18253483822383,45.1984841028063));
#56099=CARTESIAN_POINT('Ctrl Pts',(5.15976421573454,0.280869029694986,45.3572448650522));
#56100=CARTESIAN_POINT('Ctrl Pts',(2.56261074386464,4.4872129823807,45.5160056272982));
#56101=CARTESIAN_POINT('Ctrl Pts',(-2.37992235675453,4.58672254988638,45.6747663895439));
#56102=CARTESIAN_POINT('Ctrl Pts',(-5.14427782079704,0.488323536471552,
45.8335271517899));
#56103=CARTESIAN_POINT('Ctrl Pts',(-3.20043308923407,-4.05700409355871,
45.9922879140358));
#56104=CARTESIAN_POINT('Ctrl Pts',(1.67254576409749,-4.88923765436041,46.1510486762816));
#56105=CARTESIAN_POINT('Ctrl Pts',(5.01475964555148,-1.2466915701828,46.3098094385276));
#56106=CARTESIAN_POINT('Ctrl Pts',(3.76731232156889,3.53686471971598,46.4685702007735));
#56107=CARTESIAN_POINT('Ctrl Pts',(-0.928094313166731,5.08337438319113,
46.6273309630193));
#56108=CARTESIAN_POINT('Ctrl Pts',(-4.77408068348225,1.97742453747749,46.7860917252652));
#56109=CARTESIAN_POINT('Ctrl Pts',(-4.25068258608159,-2.93832464615453,
46.9448524875111));
#56110=CARTESIAN_POINT('Ctrl Pts',(0.163070052891163,-5.16482936133098,
47.103613249757));
#56111=CARTESIAN_POINT('Ctrl Pts',(4.42757599841828,-2.66432448325026,47.2623740120029));
#56112=CARTESIAN_POINT('Ctrl Pts',(4.63982914812316,2.27465154475207,47.4211347742487));
#56113=CARTESIAN_POINT('Ctrl Pts',(0.605568936039063,5.13179699886122,47.5798955364947));
#56114=CARTESIAN_POINT('Ctrl Pts',(-3.982926463652,3.29216508683222,47.7386562987406));
#56115=CARTESIAN_POINT('Ctrl Pts',(-4.92612590373581,-1.56055687315755,
47.8974170609864));
#56116=CARTESIAN_POINT('Ctrl Pts',(-1.36078444624568,-4.98500951500319,
48.0561778232324));
#56117=CARTESIAN_POINT('Ctrl Pts',(3.44998850215064,-3.84702917961962,48.2149385854782));
#56118=CARTESIAN_POINT('Ctrl Pts',(5.10322659210776,0.811869769988193,48.3736993477241));
#56119=CARTESIAN_POINT('Ctrl Pts',(2.08583582488191,4.72772070721777,48.53246010997));
#56120=CARTESIAN_POINT('Ctrl Pts',(-2.8405756019607,4.31661724309231,48.6912208722158));
#56121=CARTESIAN_POINT('Ctrl Pts',(-5.16720547137737,-0.0451861747017031,
48.8499816344618));
#56122=CARTESIAN_POINT('Ctrl Pts',(-2.76465105904324,-4.36563382517906,
49.0087423967076));
#56123=CARTESIAN_POINT('Ctrl Pts',(2.16819644989342,-4.69052004883103,49.1675031589536));
#56124=CARTESIAN_POINT('Ctrl Pts',(5.11664433946473,-0.72249904999246,49.3262639211995));
#56125=CARTESIAN_POINT('Ctrl Pts',(3.38218303962157,3.90677514842007,49.4850246834453));
#56126=CARTESIAN_POINT('Ctrl Pts',(-1.44775548820939,4.96044939699782,49.6437854456913));
#56127=CARTESIAN_POINT('Ctrl Pts',(-4.95266397096391,1.47416883854343,49.8025462079371));
#56128=CARTESIAN_POINT('Ctrl Pts',(-3.92474310640146,-3.36131607001936,
49.961306970183));
#56129=CARTESIAN_POINT('Ctrl Pts',(0.695222531978707,-5.12042183856424,
50.1200677324289));
#56130=CARTESIAN_POINT('Ctrl Pts',(4.67889927324325,-2.19316113513354,50.2788284946747));
#56131=CARTESIAN_POINT('Ctrl Pts',(4.38030448079635,2.74134763015048,50.4375892569207));
#56132=CARTESIAN_POINT('Ctrl Pts',(0.0727212293821569,5.16689130876717,
50.5963500191666));
#56133=CARTESIAN_POINT('Ctrl Pts',(-4.30141871246148,2.86353823685011,50.7551107814125));
#56134=CARTESIAN_POINT('Ctrl Pts',(-4.73876886011502,-2.06061249734653,
50.9138715436583));
#56135=CARTESIAN_POINT('Ctrl Pts',(-0.839052999411725,-5.09882773174331,
51.0726323059043));
#56136=CARTESIAN_POINT('Ctrl Pts',(3.82858979556074,-3.47044008032763,51.2313930681501));
#56137=CARTESIAN_POINT('Ctrl Pts',(4.99219026383802,1.33420033857639,51.390153830396));
#56138=CARTESIAN_POINT('Ctrl Pts',(1.58678571421362,4.91773985393535,51.548914592642));
#56139=CARTESIAN_POINT('Ctrl Pts',(-3.27089359005984,4.00041364065291,51.7076753548878));
#56140=CARTESIAN_POINT('Ctrl Pts',(-5.1349511699649,-0.578213330780779,
51.8664361171337));
#56141=CARTESIAN_POINT('Ctrl Pts',(-2.2993445899923,-4.62764180012773,52.0251968793796));
#56142=CARTESIAN_POINT('Ctrl Pts',(2.64069239313623,-4.44171114083851,52.1839576416255));
#56143=CARTESIAN_POINT('Ctrl Pts',(5.16388703706709,-0.190590771620509,
52.3427184038713));
#56144=CARTESIAN_POINT('Ctrl Pts',(2.96093453169081,4.23496409345547,52.5014791661172));
#56145=CARTESIAN_POINT('Ctrl Pts',(-1.95195570001178,4.78455046153847,52.6602399283632));
#56146=CARTESIAN_POINT('Ctrl Pts',(-5.07835645180041,0.955170101224678,
52.819000690609));
#56147=CARTESIAN_POINT('Ctrl Pts',(-3.5568902584837,-3.7484111117806,52.9777614528549));
#56148=CARTESIAN_POINT('Ctrl Pts',(1.21995054602492,-5.021331978576,53.1365222151008));
#56149=CARTESIAN_POINT('Ctrl Pts',(4.88025534693686,-1.69857643999627,53.2952829773467));
#56150=CARTESIAN_POINT('Ctrl Pts',(4.07400138499168,3.17876814016096,53.4540437395925));
#56151=CARTESIAN_POINT('Ctrl Pts',(-0.460903086490536,5.14680702170578,
53.6128045018385));
#56152=CARTESIAN_POINT('Ctrl Pts',(-4.57397497474849,2.404330905718,53.7715652640843));
#56153=CARTESIAN_POINT('Ctrl Pts',(-4.5008052522319,-2.53866229642665,53.9303260263303));
#56154=CARTESIAN_POINT('Ctrl Pts',(-0.308361083986154,-5.15819422043212,
54.0890867885761));
#56155=CARTESIAN_POINT('Ctrl Pts',(4.16630456733569,-3.05678923480409,54.2478475508221));
#56156=CARTESIAN_POINT('Ctrl Pts',(4.82784101720183,1.84228262935957,54.4066083130679));
#56157=CARTESIAN_POINT('Ctrl Pts',(1.07078989980086,5.0552411578777,54.5653690753139));
#56158=CARTESIAN_POINT('Ctrl Pts',(-3.66628084160122,3.64148856435446,54.7241298375597));
#56159=CARTESIAN_POINT('Ctrl Pts',(-5.04785936876341,-1.10506559398251,
54.8828905998056));
#56160=CARTESIAN_POINT('Ctrl Pts',(-1.80948281276126,-4.84022996603858,
55.0416513620516));
#56161=CARTESIAN_POINT('Ctrl Pts',(3.08498768485217,-4.1454680264268,55.2004121242973));
#56162=CARTESIAN_POINT('Ctrl Pts',(5.15598322111311,0.34335287594041,55.3591728865433));
#56163=CARTESIAN_POINT('Ctrl Pts',(2.50806542185317,4.51792673839683,55.5179336487891));
#56164=CARTESIAN_POINT('Ctrl Pts',(-2.43531046134262,4.55755604800332,55.6766944110351));
#56165=CARTESIAN_POINT('Ctrl Pts',(-5.14981582279099,0.425970850115064,
55.8354551732808));
#56166=CARTESIAN_POINT('Ctrl Pts',(-3.15105244004859,-4.09547588124754,
55.9942159355269));
#56167=CARTESIAN_POINT('Ctrl Pts',(1.73165038597632,-4.86861798815274,56.1529766977727));
#56168=CARTESIAN_POINT('Ctrl Pts',(5.02949388480597,-1.18585219842773,56.3117374600186));
#56169=CARTESIAN_POINT('Ctrl Pts',(3.72419095237009,3.58224174562538,56.4704982222645));
#56170=CARTESIAN_POINT('Ctrl Pts',(-0.989605296568694,5.07175862308326,
56.6292589845104));
#56171=CARTESIAN_POINT('Ctrl Pts',(-4.79768455020047,1.91944708981109,56.7880197467563));
#56172=CARTESIAN_POINT('Ctrl Pts',(-4.21477635630603,-2.98960105033098,
56.9467805090022));
#56173=CARTESIAN_POINT('Ctrl Pts',(0.225623900899773,-5.162474990657,57.1055412712481));
#56174=CARTESIAN_POINT('Ctrl Pts',(4.45952627223033,-2.61049412968195,57.2643020334939));
#56175=CARTESIAN_POINT('Ctrl Pts',(4.61193398121205,2.33069069735948,57.4230627957398));
#56176=CARTESIAN_POINT('Ctrl Pts',(0.543358837230748,5.13875620630321,57.5818235579857));
#56177=CARTESIAN_POINT('Ctrl Pts',(-4.02251491169591,3.24367506988608,57.7405843202316));
#56178=CARTESIAN_POINT('Ctrl Pts',(-4.90686014412063,-1.62011656983585,
57.8993450824775));
#56179=CARTESIAN_POINT('Ctrl Pts',(-1.30029709065152,-5.00112803773905,
58.0581058447233));
#56180=CARTESIAN_POINT('Ctrl Pts',(3.49633757827368,-3.80495436405849,58.2168666069693));
#56181=CARTESIAN_POINT('Ctrl Pts',(5.09301729854088,0.873629767452735,58.3756273692151));
#56182=CARTESIAN_POINT('Ctrl Pts',(2.02841201894453,4.75264125042254,58.5343881314611));
#56183=CARTESIAN_POINT('Ctrl Pts',(-2.89265789904175,4.2818902896884,58.6931488937069));
#56184=CARTESIAN_POINT('Ctrl Pts',(-5.16627895043901,-0.107777456210482,
58.8519096559528));
#56185=CARTESIAN_POINT('Ctrl Pts',(-2.71156370034918,-4.39880398208026,
59.0106704181988));
#56186=CARTESIAN_POINT('Ctrl Pts',(2.22485747409188,-4.66391074033302,59.1694311804446));
#56187=CARTESIAN_POINT('Ctrl Pts',(5.12502112908765,-0.660463928024547,
59.3281919426906));
#56188=CARTESIAN_POINT('Ctrl Pts',(3.33460890093368,3.94745964534539,59.4869527049363));
#56189=CARTESIAN_POINT('Ctrl Pts',(-1.5077392503099,4.94254757457034,59.6457134671823));
#56190=CARTESIAN_POINT('Ctrl Pts',(-4.97015838517481,1.41406499146713,59.8044742294282));
#56191=CARTESIAN_POINT('Ctrl Pts',(-3.88373675046313,-3.40861306500439,
59.963234991674));
#56192=CARTESIAN_POINT('Ctrl Pts',(0.757199388556149,-5.11162432694214,
60.12199575392));
#56193=CARTESIAN_POINT('Ctrl Pts',(4.70512351821232,-2.13632086826434,60.2807565161658));
#56194=CARTESIAN_POINT('Ctrl Pts',(4.34677488413138,2.79420870381954,60.4395172784118));
#56195=CARTESIAN_POINT('Ctrl Pts',(0.0101251021257834,5.16739311995163,
60.5982780406576));
#56196=CARTESIAN_POINT('Ctrl Pts',(-4.33579148262063,2.81122151262594,60.7570388029036));
#56197=CARTESIAN_POINT('Ctrl Pts',(-4.71345926399734,-2.11786589293417,
60.9157995651493));
#56198=CARTESIAN_POINT('Ctrl Pts',(-0.777225152475865,-5.10861774222493,
61.0745603273954));
#56199=CARTESIAN_POINT('Ctrl Pts',(3.87034915924295,-3.42380658907068,61.2333210896411));
#56200=CARTESIAN_POINT('Ctrl Pts',(4.97566169906822,1.39457693593507,61.3920818518871));
#56201=CARTESIAN_POINT('Ctrl Pts',(1.52709666834069,4.93660105126586,61.550842614133));
#56202=CARTESIAN_POINT('Ctrl Pts',(-3.3191138790273,3.96049709403562,61.7096033763789));
#56203=CARTESIAN_POINT('Ctrl Pts',(-5.12757002065602,-0.640374778614905,
61.8683641386248));
#56204=CARTESIAN_POINT('Ctrl Pts',(-2.24311745571471,-4.65515609337478,
62.0271249008706));
#56205=CARTESIAN_POINT('Ctrl Pts',(2.69430472161155,-4.40939635788372,62.1858856631165));
#56206=CARTESIAN_POINT('Ctrl Pts',(5.16581691910958,-0.128022388891978,
62.3446464253625));
#56207=CARTESIAN_POINT('Ctrl Pts',(2.90941568030617,4.27052158090844,62.5034071876082));
#56208=CARTESIAN_POINT('Ctrl Pts',(-2.00977165837252,4.76055375508134,62.6621679498542));
#56209=CARTESIAN_POINT('Ctrl Pts',(-5.08955458603407,0.893581719595941,
62.8209287121001));
#56210=CARTESIAN_POINT('Ctrl Pts',(-3.51122169408817,-3.79122360047265,
62.9796894743459));
#56211=CARTESIAN_POINT('Ctrl Pts',(1.28068854395033,-5.00618527695598,63.1384502365919));
#56212=CARTESIAN_POINT('Ctrl Pts',(4.90047350742458,-1.63933327204883,63.2972109988377));
#56213=CARTESIAN_POINT('Ctrl Pts',(4.03519542999152,3.22788661752423,63.4559717610837));
#56214=CARTESIAN_POINT('Ctrl Pts',(-0.523216761619089,5.14084607765855,
63.6147325233295));
#56215=CARTESIAN_POINT('Ctrl Pts',(-4.60276499113179,2.34874617833169,63.7734932855755));
#56216=CARTESIAN_POINT('Ctrl Pts',(-4.46972210747346,-2.59299796679048,
63.9322540478212));
#56217=CARTESIAN_POINT('Ctrl Pts',(-0.245853021615901,-5.16155116855183,
64.0910148100673));
#56218=CARTESIAN_POINT('Ctrl Pts',(4.20302825930282,-3.00609507922124,64.249775572313));
#56219=CARTESIAN_POINT('Ctrl Pts',(4.80516969413782,1.90063104898239,64.408536334559));
#56220=CARTESIAN_POINT('Ctrl Pts',(1.00947304907845,5.06784158562605,64.5672970968048));
#56221=CARTESIAN_POINT('Ctrl Pts',(-3.71012416525332,3.59680870386789,64.7260578590508));
#56222=CARTESIAN_POINT('Ctrl Pts',(-5.03410241632698,-1.16613336962256,
64.8848186212966));
#56223=CARTESIAN_POINT('Ctrl Pts',(-1.75071636731768,-4.86179456322688,
65.0435793835425));
#56224=CARTESIAN_POINT('Ctrl Pts',(3.1349787773885,-4.10779286711735,65.2023401457884));
#56225=CARTESIAN_POINT('Ctrl Pts',(5.15144558585509,0.405786335144852,65.3611009080343));
#56226=CARTESIAN_POINT('Ctrl Pts',(2.45315204119292,4.54797748857745,65.5198616702802));
#56227=CARTESIAN_POINT('Ctrl Pts',(-2.49034118407384,4.52772072468283,65.6786224325261));
#56228=CARTESIAN_POINT('Ctrl Pts',(-5.15459808921429,0.363555652528053,
65.837383194772));
#56229=CARTESIAN_POINT('Ctrl Pts',(-3.10120937385697,-4.13334665777235,
65.9961439570178));
#56230=CARTESIAN_POINT('Ctrl Pts',(1.79050088812788,-4.84728385216189,66.1549047192638));
#56231=CARTESIAN_POINT('Ctrl Pts',(5.04349004573647,-1.12483880283976,66.3136654815096));
#56232=CARTESIAN_POINT('Ctrl Pts',(3.68052305807757,3.62709307749002,66.4724262437556));
#56233=CARTESIAN_POINT('Ctrl Pts',(-1.05097105537457,5.05939858230018,66.6311870060014));
#56234=CARTESIAN_POINT('Ctrl Pts',(-4.82058435661895,1.86118796324735,66.7899477682473));
#56235=CARTESIAN_POINT('Ctrl Pts',(-4.17825160801934,-3.04043873049599,
66.9487085304932));
#56236=CARTESIAN_POINT('Ctrl Pts',(0.288144638596748,-5.15936302667923,
67.1074692927391));
#56237=CARTESIAN_POINT('Ctrl Pts',(4.49082211047655,-2.55628068604989,67.266230054985));
#56238=CARTESIAN_POINT('Ctrl Pts',(4.58336201290063,2.38638782106256,67.4249908172308));
#56239=CARTESIAN_POINT('Ctrl Pts',(0.481069000502546,5.14496130117338,67.5837515794768));
#56240=CARTESIAN_POINT('Ctrl Pts',(-4.06151305559941,3.19470904356121,67.7425123417227));
#56241=CARTESIAN_POINT('Ctrl Pts',(-4.88687430268524,-1.67943851437657,
67.9012731039685));
#56242=CARTESIAN_POINT('Ctrl Pts',(-1.23961891643423,-5.01651264483955,
68.0600338662145));
#56243=CARTESIAN_POINT('Ctrl Pts',(3.54217356679019,-3.76232117137135,68.2187946284603));
#56244=CARTESIAN_POINT('Ctrl Pts',(5.08206060458778,0.935261559732356,68.3775553907062));
#56245=CARTESIAN_POINT('Ctrl Pts',(1.97069054350433,4.77686434343271,68.5363161529522));
#56246=CARTESIAN_POINT('Ctrl Pts',(-2.9443156985208,4.2465349688023,68.695076915198));
#56247=CARTESIAN_POINT('Ctrl Pts',(-5.16459427796565,-0.170352921375672,
68.8538376774439));
#56248=CARTESIAN_POINT('Ctrl Pts',(-2.65807841962993,-4.43132861441282,
69.0125984396897));
#56249=CARTESIAN_POINT('Ctrl Pts',(2.2811920004135,-4.63661700284439,69.1713592019357));
#56250=CARTESIAN_POINT('Ctrl Pts',(5.1326458217616,-0.598331882962418,69.3301199641815));
#56251=CARTESIAN_POINT('Ctrl Pts',(3.28654540832559,3.98756485249208,69.4888807264275));
#56252=CARTESIAN_POINT('Ctrl Pts',(-1.56750175164667,4.92392043319156,69.6476414886732));
#56253=CARTESIAN_POINT('Ctrl Pts',(-4.98692342854749,1.35375363032602,69.8064022509193));
#56254=CARTESIAN_POINT('Ctrl Pts',(-3.84216045608199,-3.45540984595692,
69.965163013165));
#56255=CARTESIAN_POINT('Ctrl Pts',(0.819065126108891,-5.102076684352,70.1239237754111));
#56256=CARTESIAN_POINT('Ctrl Pts',(4.73065728621489,-2.07916709626671,70.2826845376568));
#56257=CARTESIAN_POINT('Ctrl Pts',(4.31260739816882,2.84665972730784,70.4414452999028));
#56258=CARTESIAN_POINT('Ctrl Pts',(-0.0524725109896868,5.16713661609669,
70.6002060621488));
#56259=CARTESIAN_POINT('Ctrl Pts',(-4.36952797529665,2.75849224159072,70.7589668243945));
#56260=CARTESIAN_POINT('Ctrl Pts',(-4.68745796764224,-2.17480849166161,
70.9177275866405));
#56261=CARTESIAN_POINT('Ctrl Pts',(-0.715283247733823,-5.11765806295492,
71.0764883488864));
#56262=CARTESIAN_POINT('Ctrl Pts',(3.91154054911197,-3.37667065413102,71.2352491111322));
#56263=CARTESIAN_POINT('Ctrl Pts',(4.95840295584866,1.45474887910182,71.3940098733782));
#56264=CARTESIAN_POINT('Ctrl Pts',(1.46718352100222,4.95473780229749,71.552770635624));
#56265=CARTESIAN_POINT('Ctrl Pts',(-3.36684708796952,3.91999934439373,71.7115313978699));
#56266=CARTESIAN_POINT('Ctrl Pts',(-5.11943640034826,-0.702442251438138,
71.8702921601158));
#56267=CARTESIAN_POINT('Ctrl Pts',(-2.18656114390733,-4.68198724237597,
72.0290529223616));
#56268=CARTESIAN_POINT('Ctrl Pts',(2.74752166081747,-4.3764344959288,72.1878136846077));
#56269=CARTESIAN_POINT('Ctrl Pts',(5.16698871742013,-0.0654352188752399,
72.3465744468534));
#56270=CARTESIAN_POINT('Ctrl Pts',(2.85746987211454,4.30545236923763,72.5053352090995));
#56271=CARTESIAN_POINT('Ctrl Pts',(-2.06729268270395,4.73585843726931,72.6640959713451));
#56272=CARTESIAN_POINT('Ctrl Pts',(-5.10000582803462,0.831862204832684,
72.8228567335913));
#56273=CARTESIAN_POINT('Ctrl Pts',(-3.46503785784167,-3.83347972702879,
72.9816174958369));
#56274=CARTESIAN_POINT('Ctrl Pts',(1.34123860080759,-4.99030391755056,73.140378258083));
#56275=CARTESIAN_POINT('Ctrl Pts',(4.91997252333115,-1.57984953191204,73.2991390203287));
#56276=CARTESIAN_POINT('Ctrl Pts',(3.99579730998455,3.27653140246455,73.4578997825747));
#56277=CARTESIAN_POINT('Ctrl Pts',(-0.585453654677876,5.13413071435083,
73.6166605448206));
#56278=CARTESIAN_POINT('Ctrl Pts',(-4.63087955166449,2.29281677239862,73.7754213070665));
#56279=CARTESIAN_POINT('Ctrl Pts',(-4.43798303090997,-2.64695311465312,
73.9341820693124));
#56280=CARTESIAN_POINT('Ctrl Pts',(-0.183308880309829,-5.16415065893858,
74.0929428315583));
#56281=CARTESIAN_POINT('Ctrl Pts',(4.23913515679244,-2.95495977912772,74.2517035938041));
#56282=CARTESIAN_POINT('Ctrl Pts',(4.78179321232898,1.95870055096247,74.4104643560501));
#56283=CARTESIAN_POINT('Ctrl Pts',(0.948008058166557,5.07969830752458,74.5692251182959));
#56284=CARTESIAN_POINT('Ctrl Pts',(-3.75342302811316,3.55160101163497,74.7279858805418));
#56285=CARTESIAN_POINT('Ctrl Pts',(-5.01960670926438,-1.22703001516843,
74.8867466427878));
#56286=CARTESIAN_POINT('Ctrl Pts',(-1.69169300421356,-4.88264569196979,
75.0455074050335));
#56287=CARTESIAN_POINT('Ctrl Pts',(3.18450981172911,-4.06951488912588,75.2042681672795));
#56288=CARTESIAN_POINT('Ctrl Pts',(5.14615197585861,0.468160245196775,75.3630289295254));
#56289=CARTESIAN_POINT('Ctrl Pts',(2.39787866042351,4.57736082297456,75.5217896917712));
#56290=CARTESIAN_POINT('Ctrl Pts',(-2.54500644918866,4.49722095825909,75.6805504540172));
#56291=CARTESIAN_POINT('Ctrl Pts',(-5.15862391826907,0.301087103142032,
75.839311216263));
#56292=CARTESIAN_POINT('Ctrl Pts',(-3.05091120513038,-4.17061086559584,
75.9980719785089));
#56293=CARTESIAN_POINT('Ctrl Pts',(1.84908863423975,-4.82523837717284,76.1568327407549));
#56294=CARTESIAN_POINT('Ctrl Pts',(5.05674607440601,-1.06366033713594,76.3155935030006));
#56295=CARTESIAN_POINT('Ctrl Pts',(3.63631504695578,3.6714121333759,76.4743542652466));
#56296=CARTESIAN_POINT('Ctrl Pts',(-1.11218258415778,5.04629607467818,76.6331150274925));
#56297=CARTESIAN_POINT('Ctrl Pts',(-4.84277674219067,1.80265570731443,76.7918757897383));
#56298=CARTESIAN_POINT('Ctrl Pts',(-4.1411137012291,-3.09083022621898,76.9506365519843));
#56299=CARTESIAN_POINT('Ctrl Pts',(0.350623091062388,-5.15549392607834,
77.1093973142301));
#56300=CARTESIAN_POINT('Ctrl Pts',(4.52145892049186,-2.50169210817825,77.268158076476));
#56301=CARTESIAN_POINT('Ctrl Pts',(4.55411743612604,2.44173474230699,77.4269188387219));
#56302=CARTESIAN_POINT('Ctrl Pts',(0.4187085668894,5.15041137287398,77.5856796009678));
#56303=CARTESIAN_POINT('Ctrl Pts',(-4.09991517238411,3.14527419362299,77.7444403632137));
#56304=CARTESIAN_POINT('Ctrl Pts',(-4.86617131235222,-1.738514001283,77.9032011254596));
#56305=CARTESIAN_POINT('Ctrl Pts',(-1.17875882811733,-5.03116107861318,
78.0619618877055));
#56306=CARTESIAN_POINT('Ctrl Pts',(3.58748974126774,-3.71913585798031,78.2207226499514));
#56307=CARTESIAN_POINT('Ctrl Pts',(5.07035811814355,0.996756102360001,78.3794834121972));
#56308=CARTESIAN_POINT('Ctrl Pts',(1.91267986918918,4.80038643150889,78.5382441744432));
#56309=CARTESIAN_POINT('Ctrl Pts',(-2.99554141961442,4.21055646882815,78.697004936689));
#56310=CARTESIAN_POINT('Ctrl Pts',(-5.16215170118294,-0.232903387246084,
78.855765698935));
#56311=CARTESIAN_POINT('Ctrl Pts',(-2.60420306585193,-4.46320294918618,
79.0145264611808));
#56312=CARTESIAN_POINT('Ctrl Pts',(2.33719176176521,-4.60864284172174,79.1732872234268));
#56313=CARTESIAN_POINT('Ctrl Pts',(5.13951729856278,-0.536112032685121,
79.3320479856725));
#56314=CARTESIAN_POINT('Ctrl Pts',(3.23799961511593,4.02708488442023,79.4908087479186));
#56315=CARTESIAN_POINT('Ctrl Pts',(-1.62703422207133,4.90457070639472,79.6495695101643));
#56316=CARTESIAN_POINT('Ctrl Pts',(-5.00295664081116,1.29324360581397,79.8083302724103));
#56317=CARTESIAN_POINT('Ctrl Pts',(-3.80002032458076,-3.5016995454484,79.9670910346561));
#56318=CARTESIAN_POINT('Ctrl Pts',(0.880810665839244,-5.09178031191025,
80.125851796902));
#56319=CARTESIAN_POINT('Ctrl Pts',(4.75549683016874,-2.02170820645871,80.2846125591479));
#56320=CARTESIAN_POINT('Ctrl Pts',(4.27780703699033,2.89869300342805,80.4433733213939));
#56321=CARTESIAN_POINT('Ctrl Pts',(-0.11506242376767,5.16612183484124,80.6021340836397));
#56322=CARTESIAN_POINT('Ctrl Pts',(-4.40262323964949,2.70535816177208,80.7608948458856));
#56323=CARTESIAN_POINT('Ctrl Pts',(-4.66076878675771,-2.23143193721207,
80.9196556081315));
#56324=CARTESIAN_POINT('Ctrl Pts',(-0.653236375128765,-5.12594736724498,
81.0784163703773));
#56325=CARTESIAN_POINT('Ctrl Pts',(3.95215792026738,-3.32903919274863,81.2371771326234));
#56326=CARTESIAN_POINT('Ctrl Pts',(4.94041656702063,1.51470733791976,81.3959378948691));
#56327=CARTESIAN_POINT('Ctrl Pts',(1.40705506422376,4.97214744531344,81.5546986571151));
#56328=CARTESIAN_POINT('Ctrl Pts',(-3.41408621159557,3.87892633505682,81.713459419361));
#56329=CARTESIAN_POINT('Ctrl Pts',(-5.11055150349599,-0.76440664139103,
81.8722201816067));
#56330=CARTESIAN_POINT('Ctrl Pts',(-2.12968395259116,-4.7081313086182,82.0309809438528));
#56331=CARTESIAN_POINT('Ctrl Pts',(2.80033539806548,-4.3428303941221,82.1897417060986));
#56332=CARTESIAN_POINT('Ctrl Pts',(5.16740226597732,-0.00283844241944707,
82.3485024683445));
#56333=CARTESIAN_POINT('Ctrl Pts',(2.80510471878759,4.33975132503298,82.5072632305904));
#56334=CARTESIAN_POINT('Ctrl Pts',(-2.12451031000386,4.71046814615349,82.6660239928362));
#56335=CARTESIAN_POINT('Ctrl Pts',(-5.10970868581842,0.770020587436124,
82.8247847550823));
#56336=CARTESIAN_POINT('Ctrl Pts',(-3.41834544728425,-3.87517323895607,
82.983545517328));
#56337=CARTESIAN_POINT('Ctrl Pts',(1.40159167776471,-4.9736903294079,83.142306279574));
#56338=CARTESIAN_POINT('Ctrl Pts',(4.93874982643145,-1.52013376024582,83.3010670418199));
#56339=CARTESIAN_POINT('Ctrl Pts',(3.95581224496304,3.32469499516411,83.4598278040656));
#56340=CARTESIAN_POINT('Ctrl Pts',(-0.647603556591826,5.12666260907039,
83.6185885663118));
#56341=CARTESIAN_POINT('Ctrl Pts',(-4.65831659106839,2.23654957051732,83.7773493285574));
#56342=CARTESIAN_POINT('Ctrl Pts',(-4.40558873364168,-2.70051728419629,
83.9361100908035));
#56343=CARTESIAN_POINT('Ctrl Pts',(-0.120745397495975,-5.1659971710397,
84.0948708530492));
#56344=CARTESIAN_POINT('Ctrl Pts',(4.27463443926266,-2.90338152834273,84.2536316152952));
#56345=CARTESIAN_POINT('Ctrl Pts',(4.75768727179541,2.01646478129229,84.412392377541));
#56346=CARTESIAN_POINT('Ctrl Pts',(0.886457060193665,5.09084373843816,84.571153139787));
#56347=CARTESIAN_POINT('Ctrl Pts',(-3.79627280569434,3.50580670373394,84.7299139020329));
#56348=CARTESIAN_POINT('Ctrl Pts',(-5.00417952636703,-1.28762129421282,
84.8886746642788));
#56349=CARTESIAN_POINT('Ctrl Pts',(-1.63279460579437,-4.90302030367583,
85.0474354265246));
#56350=CARTESIAN_POINT('Ctrl Pts',(3.23428855022947,-4.03017982392474,85.2061961887705));
#56351=CARTESIAN_POINT('Ctrl Pts',(5.13873193725801,0.529582954402255,85.3649569510164));
#56352=CARTESIAN_POINT('Ctrl Pts',(2.34489518331184,4.6077777382683,85.5237177132623));
#56353=CARTESIAN_POINT('Ctrl Pts',(-2.60449736313211,4.46265913321349,85.6824784755082));
#56354=CARTESIAN_POINT('Ctrl Pts',(-4.72633661207834,0.94905134843793,85.8147791107131));
#56355=CARTESIAN_POINT('Ctrl Pts',(-4.08944266318188,-1.99447502555823,
85.9206196188771));
#56356=CARTESIAN_POINT('Ctrl Pts',(-3.130164636136,-3.13763950664809,85.973539872959));
#56357=CARTESIAN_POINT('Ctrl Pts',(-2.53835875722777,-3.5596515025498,86.));
#56358=CARTESIAN_POINT('Ctrl Pts',(-2.00237954638818,4.09906332620103,25.7806068977079));
#56359=CARTESIAN_POINT('Ctrl Pts',(-2.68386473467845,3.76615995447791,25.8070670247489));
#56360=CARTESIAN_POINT('Ctrl Pts',(-3.86722056834447,2.75399327045732,25.8599872788309));
#56361=CARTESIAN_POINT('Ctrl Pts',(-5.02742207131257,-0.166516440447624,
25.9658277869948));
#56362=CARTESIAN_POINT('Ctrl Pts',(-3.44586235178049,-4.14677665817345,
26.0981284221997));
#56363=CARTESIAN_POINT('Ctrl Pts',(1.62355296838563,-5.14470657330929,26.2568891844456));
#56364=CARTESIAN_POINT('Ctrl Pts',(5.19838240423087,-1.42611203276403,26.4156499466915));
#56365=CARTESIAN_POINT('Ctrl Pts',(4.01994424953236,3.59365933878956,26.5744107089374));
#56366=CARTESIAN_POINT('Ctrl Pts',(-0.839985566934964,5.3265048273725,26.7331714711833));
#56367=CARTESIAN_POINT('Ctrl Pts',(-4.92992667194028,2.18327469128225,26.8919322334291));
#56368=CARTESIAN_POINT('Ctrl Pts',(-4.50847904072441,-2.95758319158922,
27.050692995675));
#56369=CARTESIAN_POINT('Ctrl Pts',(0.0395956222711487,-5.39186919347605,
27.2094537579209));
#56370=CARTESIAN_POINT('Ctrl Pts',(4.55125923496193,-2.89119591637671,27.3682145201668));
#56371=CARTESIAN_POINT('Ctrl Pts',(4.89756113932563,2.25550678246132,27.5269752824127));
#56372=CARTESIAN_POINT('Ctrl Pts',(0.761418625289898,5.33794327443822,27.6857360446586));
#56373=CARTESIAN_POINT('Ctrl Pts',(-4.07157300373756,3.53490884489523,27.8444968069045));
#56374=CARTESIAN_POINT('Ctrl Pts',(-5.17814942709716,-1.503370550728,28.0032575691504));
#56375=CARTESIAN_POINT('Ctrl Pts',(-1.54551865619794,-5.1657253452884,28.1620183313962));
#56376=CARTESIAN_POINT('Ctrl Pts',(3.50161451494142,-4.10024735702302,28.3207790936422));
#56377=CARTESIAN_POINT('Ctrl Pts',(5.34396494196453,0.717900607442646,28.479539855888));
#56378=CARTESIAN_POINT('Ctrl Pts',(2.29535447129834,4.8790048681726,28.6383006181339));
#56379=CARTESIAN_POINT('Ctrl Pts',(-2.85403402839988,4.57469439300441,28.7970613803798));
#56380=CARTESIAN_POINT('Ctrl Pts',(-5.391323666464,0.0834841081329312,28.9558221426257));
#56381=CARTESIAN_POINT('Ctrl Pts',(-2.99430906975439,-4.48413350506007,
29.1145829048716));
#56382=CARTESIAN_POINT('Ctrl Pts',(2.14318857941972,-4.94773510082165,29.2733436671175));
#56383=CARTESIAN_POINT('Ctrl Pts',(5.31917461298845,-0.88301843516797,29.4321044293634));
#56384=CARTESIAN_POINT('Ctrl Pts',(3.62688954521853,3.98986369193538,29.5908651916093));
#56385=CARTESIAN_POINT('Ctrl Pts',(-1.3848356090803,5.21110068710349,29.7496259538552));
#56386=CARTESIAN_POINT('Ctrl Pts',(-5.12911691883564,1.66297916304394,29.9083867161011));
#56387=CARTESIAN_POINT('Ctrl Pts',(-4.17907375081987,-3.40715168987467,
30.0671474783469));
#56388=CARTESIAN_POINT('Ctrl Pts',(0.595785363987352,-5.35895324212101,
30.2259082405928));
#56389=CARTESIAN_POINT('Ctrl Pts',(4.82536351591838,-2.40607709649645,30.3846690028387));
#56390=CARTESIAN_POINT('Ctrl Pts',(4.63862158504372,2.74891430277669,30.5434297650846));
#56391=CARTESIAN_POINT('Ctrl Pts',(0.206471491199163,5.38801536528353,30.7021905273305));
#56392=CARTESIAN_POINT('Ctrl Pts',(-4.41464761825083,3.09584018650688,30.8609512895764));
#56393=CARTESIAN_POINT('Ctrl Pts',(-4.99534638025495,-2.02974249468088,
31.0197120518223));
#56394=CARTESIAN_POINT('Ctrl Pts',(-1.00415155023673,-5.29764284541871,
31.1784728140681));
#56395=CARTESIAN_POINT('Ctrl Pts',(3.90607345078174,-3.71697864543531,31.3372335763141));
#56396=CARTESIAN_POINT('Ctrl Pts',(5.24134071706976,1.26557794744869,31.4959943385599));
#56397=CARTESIAN_POINT('Ctrl Pts',(1.77957286026287,5.08983894524214,31.6547551008058));
#56398=CARTESIAN_POINT('Ctrl Pts',(-3.31091443601954,4.25572386919705,31.8135158630518));
#56399=CARTESIAN_POINT('Ctrl Pts',(-5.37115170725749,-0.473359684716424,
31.9722766252976));
#56400=CARTESIAN_POINT('Ctrl Pts',(-2.51554687204882,-4.76920999621703,
32.1310373875435));
#56401=CARTESIAN_POINT('Ctrl Pts',(2.6423632988389,-4.70013364176394,32.2897981497894));
#56402=CARTESIAN_POINT('Ctrl Pts',(5.38190186659124,-0.329351410916935,
32.4485589120353));
#56403=CARTESIAN_POINT('Ctrl Pts',(3.19575945370633,4.34286329137105,32.6073196742812));
#56404=CARTESIAN_POINT('Ctrl Pts',(-1.91523962695419,5.04035685490976,32.7660804365271));
#56405=CARTESIAN_POINT('Ctrl Pts',(-5.27335289927007,1.12476186513028,32.9248411987729));
#56406=CARTESIAN_POINT('Ctrl Pts',(-3.80513252151237,-3.82024953991496,
33.0836019610189));
#56407=CARTESIAN_POINT('Ctrl Pts',(1.14566136921973,-5.26885187498842,33.2423627232647));
#56408=CARTESIAN_POINT('Ctrl Pts',(5.04791098015974,-1.89524003489642,33.4011234855106));
#56409=CARTESIAN_POINT('Ctrl Pts',(4.330158271609,3.21295337599341,33.5598842477565));
#56410=CARTESIAN_POINT('Ctrl Pts',(-0.350687553524876,5.38055371623537,
33.7186450100024));
#56411=CARTESIAN_POINT('Ctrl Pts',(-4.71057341778202,2.62370694422547,33.8774057722483));
#56412=CARTESIAN_POINT('Ctrl Pts',(-4.75919860374648,-2.53443656531169,
34.0361665344942));
#56413=CARTESIAN_POINT('Ctrl Pts',(-0.452059855948003,-5.3729863149027,
34.19492729674));
#56414=CARTESIAN_POINT('Ctrl Pts',(4.2688178803622,-3.29401486909083,34.353688058986));
#56415=CARTESIAN_POINT('Ctrl Pts',(5.08274309982495,1.79973960190727,34.5124488212318));
#56416=CARTESIAN_POINT('Ctrl Pts',(1.2447865799184,5.24631741547787,34.6712095834778));
#56417=CARTESIAN_POINT('Ctrl Pts',(-3.73243664043062,3.89130527955111,34.8299703457236));
#56418=CARTESIAN_POINT('Ctrl Pts',(-5.2936198386959,-1.02514830968824,34.9887311079695));
#56419=CARTESIAN_POINT('Ctrl Pts',(-2.00992046486332,-5.00335485233809,
35.1474918702154));
#56420=CARTESIAN_POINT('Ctrl Pts',(3.11331951223216,-4.40233820466419,35.3062526324613));
#56421=CARTESIAN_POINT('Ctrl Pts',(5.38715437415002,0.227832839089729,35.4650133947072));
#56422=CARTESIAN_POINT('Ctrl Pts',(2.73050100007286,4.64948430926405,35.6237741569531));
#56423=CARTESIAN_POINT('Ctrl Pts',(-2.42519029351004,4.81578571925249,35.782534919199));
#56424=CARTESIAN_POINT('Ctrl Pts',(-5.36127335207045,0.574532938890892,
35.9412956814449));
#56425=CARTESIAN_POINT('Ctrl Pts',(-3.39055527658917,-4.19254993648074,
36.1000564436907));
#56426=CARTESIAN_POINT('Ctrl Pts',(1.68330255388594,-5.12248304687996,36.2588172059367));
#56427=CARTESIAN_POINT('Ctrl Pts',(5.21655046989866,-1.36416320449261,36.4175779681825));
#56428=CARTESIAN_POINT('Ctrl Pts',(3.97545205425126,3.64268047155399,36.5763387304284));
#56429=CARTESIAN_POINT('Ctrl Pts',(-0.904101513210989,5.31563171291061,
36.7350994926743));
#56430=CARTESIAN_POINT('Ctrl Pts',(-4.95619375964226,2.12355444252664,36.8938602549202));
#56431=CARTESIAN_POINT('Ctrl Pts',(-4.47222608833935,-3.01206471847277,
37.0526210171661));
#56432=CARTESIAN_POINT('Ctrl Pts',(0.10485950493631,-5.39095024441108,37.211381779412));
#56433=CARTESIAN_POINT('Ctrl Pts',(4.58597447631896,-2.83587343794507,37.3701425416579));
#56434=CARTESIAN_POINT('Ctrl Pts',(4.8698655265602,2.31468136181031,37.5289033039037));
#56435=CARTESIAN_POINT('Ctrl Pts',(0.696706894914159,5.34676907637412,37.6876640661497));
#56436=CARTESIAN_POINT('Ctrl Pts',(-4.1140991681465,3.48533041305234,37.8464248283955));
#56437=CARTESIAN_POINT('Ctrl Pts',(-5.15955600572413,-1.56598910509857,
38.0051855906414));
#56438=CARTESIAN_POINT('Ctrl Pts',(-1.48282958617279,-5.18406756050325,
38.1639463528873));
#56439=CARTESIAN_POINT('Ctrl Pts',(3.55102776426338,-4.05752903512989,38.3227071151332));
#56440=CARTESIAN_POINT('Ctrl Pts',(5.33487603729029,0.782584002032494,38.4814678773791));
#56441=CARTESIAN_POINT('Ctrl Pts',(2.23608280507879,4.90645225619513,38.640228639625));
#56442=CARTESIAN_POINT('Ctrl Pts',(-2.90924171237944,4.53978553595244,38.7989894018709));
#56443=CARTESIAN_POINT('Ctrl Pts',(-5.39193935072285,0.0181684236512802,
38.9577501641167));
#56444=CARTESIAN_POINT('Ctrl Pts',(-2.93976939635272,-4.52007698493724,
39.1165109263627));
#56445=CARTESIAN_POINT('Ctrl Pts',(2.20296730598482,-4.92140986936197,39.2752716886085));
#56446=CARTESIAN_POINT('Ctrl Pts',(5.32948103937253,-0.818518114924823,
39.4340324508545));
#56447=CARTESIAN_POINT('Ctrl Pts',(3.5782909344085,4.03350642025291,39.5927932131003));
#56448=CARTESIAN_POINT('Ctrl Pts',(-1.44786033404595,5.19394267455733,39.7515539753462));
#56449=CARTESIAN_POINT('Ctrl Pts',(-5.14888559931178,1.60072394206216,39.9103147375921));
#56450=CARTESIAN_POINT('Ctrl Pts',(-4.13749348932905,-3.45752623695775,
40.069075499838));
#56451=CARTESIAN_POINT('Ctrl Pts',(0.660659043471872,-5.3513427923999,40.2278362620838));
#56452=CARTESIAN_POINT('Ctrl Pts',(4.85415623959407,-2.3474469653437,40.3865970243298));
#56453=CARTESIAN_POINT('Ctrl Pts',(4.60498137310684,2.80490402809622,40.5453577865757));
#56454=CARTESIAN_POINT('Ctrl Pts',(0.141186892964701,5.39012117811339,40.7041185488216));
#56455=CARTESIAN_POINT('Ctrl Pts',(-4.45182614422856,3.04213478252601,40.8628793110674));
#56456=CARTESIAN_POINT('Ctrl Pts',(-4.97039191142365,-2.09010628924604,
41.0216400733134));
#56457=CARTESIAN_POINT('Ctrl Pts',(-0.939903178686041,-5.30941824197221,
41.1804008355592));
#56458=CARTESIAN_POINT('Ctrl Pts',(3.95081365290143,-3.66938844135355,41.3391615978052));
#56459=CARTESIAN_POINT('Ctrl Pts',(5.22562515017917,1.32897774372121,41.497922360051));
#56460=CARTESIAN_POINT('Ctrl Pts',(1.71778489121437,5.11102290358859,41.6566831222969));
#56461=CARTESIAN_POINT('Ctrl Pts',(-3.36222457061253,4.21530378386431,41.8154438845428));
#56462=CARTESIAN_POINT('Ctrl Pts',(-5.36502340492809,-0.538390116983158,
41.9742046467887));
#56463=CARTESIAN_POINT('Ctrl Pts',(-2.4575889422798,-4.7993329374274,42.1329654090346));
#56464=CARTESIAN_POINT('Ctrl Pts',(2.69910598837468,-4.66777965600471,42.2917261712804));
#56465=CARTESIAN_POINT('Ctrl Pts',(5.38549667320271,-0.26413185422043,42.4504869335264));
#56466=CARTESIAN_POINT('Ctrl Pts',(3.14291630057783,4.38125748855891,42.6092476957722));
#56467=CARTESIAN_POINT('Ctrl Pts',(-1.97615707196429,5.01678615055665,42.7680084580181));
#56468=CARTESIAN_POINT('Ctrl Pts',(-5.28659112974097,1.06079888783667,42.926769220264));
#56469=CARTESIAN_POINT('Ctrl Pts',(-3.75857550455005,-3.86606391955536,
43.0855299825098));
#56470=CARTESIAN_POINT('Ctrl Pts',(1.20940322958872,-5.25458693731027,43.2442907447559));
#56471=CARTESIAN_POINT('Ctrl Pts',(5.07049918630525,-1.83395148659098,43.4030515070016));
#56472=CARTESIAN_POINT('Ctrl Pts',(4.29091940730092,3.26517238343396,43.5618122692476));
#56473=CARTESIAN_POINT('Ctrl Pts',(-0.41584088110511,5.37591075215103,43.7205730314935));
#56474=CARTESIAN_POINT('Ctrl Pts',(-4.74201089309862,2.56645139116746,43.8793337937394));
#56475=CARTESIAN_POINT('Ctrl Pts',(-4.72814768911957,-2.59190267629106,
44.0380945559852));
#56476=CARTESIAN_POINT('Ctrl Pts',(-0.386939296906612,-5.3780682437099,
44.1968553182311));
#56477=CARTESIAN_POINT('Ctrl Pts',(4.30840775904998,-3.24206147925195,44.3556160804771));
#56478=CARTESIAN_POINT('Ctrl Pts',(5.06056843189549,1.86117898107469,44.5143768427229));
#56479=CARTESIAN_POINT('Ctrl Pts',(1.18114229879479,5.26101158746959,44.6731376049688));
#56480=CARTESIAN_POINT('Ctrl Pts',(-3.77930134462421,3.84580568932092,44.8318983672147));
#56481=CARTESIAN_POINT('Ctrl Pts',(-5.2808129571804,-1.08919904735859,44.9906591294605));
#56482=CARTESIAN_POINT('Ctrl Pts',(-1.94916324679306,-5.02733554587743,
45.1494198917065));
#56483=CARTESIAN_POINT('Ctrl Pts',(3.16642020502591,-4.36430099084551,45.3081806539524));
#56484=CARTESIAN_POINT('Ctrl Pts',(5.38399916564066,0.293075140317788,45.4669414161982));
#56485=CARTESIAN_POINT('Ctrl Pts',(2.67397763346517,4.68221995096551,45.6257021784443));
#56486=CARTESIAN_POINT('Ctrl Pts',(-2.48334990656791,4.78605404221895,45.7844629406899));
#56487=CARTESIAN_POINT('Ctrl Pts',(-5.3678397571995,0.509545282109415,45.9432237029359));
#56488=CARTESIAN_POINT('Ctrl Pts',(-3.3395186992418,-4.23331488444999,46.1019844651818));
#56489=CARTESIAN_POINT('Ctrl Pts',(1.74523187918884,-5.10171596047391,46.2607452274276));
#56490=CARTESIAN_POINT('Ctrl Pts',(5.232692932984,-1.30087075552908,46.4195059896737));
#56491=CARTESIAN_POINT('Ctrl Pts',(3.93103357982541,3.69057110049061,46.5782667519194));
#56492=CARTESIAN_POINT('Ctrl Pts',(-0.96842778057353,5.30428955537918,46.7370275141654));
#56493=CARTESIAN_POINT('Ctrl Pts',(-4.98155445517987,2.06336018755066,46.8957882764112));
#56494=CARTESIAN_POINT('Ctrl Pts',(-4.43541032884349,-3.06601945008181,
47.0545490386572));
#56495=CARTESIAN_POINT('Ctrl Pts',(0.170156811823045,-5.3892844342159,47.213309800903));
#56496=CARTESIAN_POINT('Ctrl Pts',(4.61999124080161,-2.78011168631907,47.3720705631489));
#56497=CARTESIAN_POINT('Ctrl Pts',(4.8414685667286,2.37350419651411,47.5308313253948));
#56498=CARTESIAN_POINT('Ctrl Pts',(0.631885975802691,5.35481653906792,47.6895920876407));
#56499=CARTESIAN_POINT('Ctrl Pts',(-4.15601796138632,3.43523722006585,47.8483528498866));
#56500=CARTESIAN_POINT('Ctrl Pts',(-5.14020731309298,-1.62837613342762,
48.0071136121325));
#56501=CARTESIAN_POINT('Ctrl Pts',(-1.41992192218023,-5.20164991021152,
48.1658743743783));
#56502=CARTESIAN_POINT('Ctrl Pts',(3.59991938399174,-4.01421480270452,48.3246351366243));
#56503=CARTESIAN_POINT('Ctrl Pts',(5.32500450896511,0.847152308025391,48.4833958988701));
#56504=CARTESIAN_POINT('Ctrl Pts',(2.17648285295299,4.93317974984624,48.642156661116));
#56505=CARTESIAN_POINT('Ctrl Pts',(-2.96402239161607,4.50421039867032,48.800917423362));
#56506=CARTESIAN_POINT('Ctrl Pts',(-5.39176380613531,-0.0471498922667038,
48.9596781856078));
#56507=CARTESIAN_POINT('Ctrl Pts',(-2.88479829170963,-4.55535716158905,
49.1184389478537));
#56508=CARTESIAN_POINT('Ctrl Pts',(2.26242273659985,-4.89436241142882,49.2771997100995));
#56509=CARTESIAN_POINT('Ctrl Pts',(5.33900536977086,-0.753897682082513,
49.4359604723455));
#56510=CARTESIAN_POINT('Ctrl Pts',(3.52916720648512,4.07655723401027,49.5947212345913));
#56511=CARTESIAN_POINT('Ctrl Pts',(-1.51067258399179,5.1760224494748,49.7534819968373));
#56512=CARTESIAN_POINT('Ctrl Pts',(-5.16789868150448,1.53823381551562,49.9122427590831));
#56513=CARTESIAN_POINT('Ctrl Pts',(-4.09530605018365,-3.5073933923671,50.0710035213291));
#56514=CARTESIAN_POINT('Ctrl Pts',(0.72543577101732,-5.34294703282935,50.2297642835748));
#56515=CARTESIAN_POINT('Ctrl Pts',(4.88223661585912,-2.28847234640404,50.3885250458209));
#56516=CARTESIAN_POINT('Ctrl Pts',(4.57066538000743,2.86048213374822,50.5472858080667));
#56517=CARTESIAN_POINT('Ctrl Pts',(0.0758815755810925,5.39143599052969,
50.7060465703126));
#56518=CARTESIAN_POINT('Ctrl Pts',(-4.48835136464999,2.98798294522175,50.8648073325585));
#56519=CARTESIAN_POINT('Ctrl Pts',(-4.94470803747584,-2.15016336068061,
51.0235680948044));
#56520=CARTESIAN_POINT('Ctrl Pts',(-0.875516876330153,-5.32041448129303,
51.1823288570502));
#56521=CARTESIAN_POINT('Ctrl Pts',(3.99497407304406,-3.62125975444968,51.3410896192962));
#56522=CARTESIAN_POINT('Ctrl Pts',(5.20914272269644,1.39218251248544,51.499850381542));
#56523=CARTESIAN_POINT('Ctrl Pts',(1.65574483720076,5.13145681922537,51.658611143788));
#56524=CARTESIAN_POINT('Ctrl Pts',(-3.41304129868565,4.17426510262078,51.8173719060338));
#56525=CARTESIAN_POINT('Ctrl Pts',(-5.35810778531101,-0.603341540490118,
51.9761326682797));
#56526=CARTESIAN_POINT('Ctrl Pts',(-2.39927036128639,-4.82875157643711,
52.1348934305256));
#56527=CARTESIAN_POINT('Ctrl Pts',(2.75545258405494,-4.6347406734915,52.2936541927715));
#56528=CARTESIAN_POINT('Ctrl Pts',(5.38830115807414,-0.198873536169234,
52.4524149550174));
#56529=CARTESIAN_POINT('Ctrl Pts',(3.08961192442195,4.41900873612634,52.6111757172633));
#56530=CARTESIAN_POINT('Ctrl Pts',(-2.03678451588621,4.99247923273975,52.7699364795092));
#56531=CARTESIAN_POINT('Ctrl Pts',(-5.29905355286222,0.996680238285941,
52.928697241755));
#56532=CARTESIAN_POINT('Ctrl Pts',(-3.71146691656038,-3.91131095424147,
53.087458004001));
#56533=CARTESIAN_POINT('Ctrl Pts',(1.27296761001063,-5.23955088889833,53.2462187662468));
#56534=CARTESIAN_POINT('Ctrl Pts',(5.09234329659795,-1.77239380586966,53.4049795284928));
#56535=CARTESIAN_POINT('Ctrl Pts',(4.25105085048754,3.31691222676463,53.5637402907385));
#56536=CARTESIAN_POINT('Ctrl Pts',(-0.48093318402806,5.37047887306077,53.7225010529846));
#56537=CARTESIAN_POINT('Ctrl Pts',(-4.77275247822576,2.50881921131856,53.8812618152303));
#56538=CARTESIAN_POINT('Ctrl Pts',(-4.69640291872861,-2.64898842550301,
54.0400225774763));
#56539=CARTESIAN_POINT('Ctrl Pts',(-0.321761954516003,-5.38236094089921,
54.1987833397221));
#56540=CARTESIAN_POINT('Ctrl Pts',(4.34736537881655,-3.18963231682882,54.3575441019682));
#56541=CARTESIAN_POINT('Ctrl Pts',(5.03765112545161,1.92234523219103,54.5163048642139));
#56542=CARTESIAN_POINT('Ctrl Pts',(1.11732468501616,5.27493370590994,54.6750656264599));
#56543=CARTESIAN_POINT('Ctrl Pts',(-3.82561143627296,3.79974172703212,54.8338263887057));
#56544=CARTESIAN_POINT('Ctrl Pts',(-5.26723111626224,-1.15308994504782,
54.9925871509516));
#56545=CARTESIAN_POINT('Ctrl Pts',(-1.88811998897897,-5.05057847782898,
55.1513479131975));
#56546=CARTESIAN_POINT('Ctrl Pts',(3.21905622559384,-4.32562331577277,55.3101086754434));
#56547=CARTESIAN_POINT('Ctrl Pts',(5.38005385515049,0.358274432763269,55.4688694376893));
#56548=CARTESIAN_POINT('Ctrl Pts',(2.61706186058861,4.71426847679935,55.6276301999351));
#56549=CARTESIAN_POINT('Ctrl Pts',(-2.54114508797937,4.75562001166302,55.7863909621812));
#56550=CARTESIAN_POINT('Ctrl Pts',(-5.37361843174121,0.444482849548049,
55.9451517244269));
#56551=CARTESIAN_POINT('Ctrl Pts',(-3.28799204746135,-4.27345859337873,
56.1039124866729));
#56552=CARTESIAN_POINT('Ctrl Pts',(1.80690509167997,-5.08020019715291,56.2626732489186));
#56553=CARTESIAN_POINT('Ctrl Pts',(5.24806749828111,-1.23738740375719,56.4214340111647));
#56554=CARTESIAN_POINT('Ctrl Pts',(3.88603822614634,3.73792013804749,56.5801947734104));
#56555=CARTESIAN_POINT('Ctrl Pts',(-1.03261193114073,5.2921689932538,56.7389555356565));
#56556=CARTESIAN_POINT('Ctrl Pts',(-5.00618410750568,2.00286313442759,56.8977162979023));
#56557=CARTESIAN_POINT('Ctrl Pts',(-4.3979436727968,-3.11952424327782,57.0564770601482));
#56558=CARTESIAN_POINT('Ctrl Pts',(0.235429148194338,-5.38682774642662,
57.2152378223941));
#56559=CARTESIAN_POINT('Ctrl Pts',(4.65333002148106,-2.72394195324985,57.37399858464));
#56560=CARTESIAN_POINT('Ctrl Pts',(4.81236112129208,2.43197871943155,57.5327593468858));
#56561=CARTESIAN_POINT('Ctrl Pts',(0.566972327412124,5.36207818233195,57.6915201091318));
#56562=CARTESIAN_POINT('Ctrl Pts',(-4.19732685891063,3.38463990595143,57.8502808713776));
#56563=CARTESIAN_POINT('Ctrl Pts',(-5.12010429494008,-1.6905241975279,58.0090416336235));
#56564=CARTESIAN_POINT('Ctrl Pts',(-1.35680588461835,-5.21846891769574,
58.1678023958695));
#56565=CARTESIAN_POINT('Ctrl Pts',(3.64828271548151,-3.97031148417985,58.3265631581153));
#56566=CARTESIAN_POINT('Ctrl Pts',(5.31435153612611,0.911596294400786,58.4853239203612));
#56567=CARTESIAN_POINT('Ctrl Pts',(2.11656350192684,4.95918329927446,58.6440846826071));
#56568=CARTESIAN_POINT('Ctrl Pts',(-3.01836810050987,4.46797426842589,58.8028454448529));
#56569=CARTESIAN_POINT('Ctrl Pts',(-5.39079702010585,-0.112461288937121,
58.9616062070989));
#56570=CARTESIAN_POINT('Ctrl Pts',(-2.8294038428619,-4.58996883949007,59.1203669693448));
#56571=CARTESIAN_POINT('Ctrl Pts',(2.32154615663493,-4.86659670571795,59.2791277315906));
#56572=CARTESIAN_POINT('Ctrl Pts',(5.34774620102881,-0.689166614740877,
59.4378884938366));
#56573=CARTESIAN_POINT('Ctrl Pts',(3.47952557320649,4.11900981291542,59.5966492560824));
#56574=CARTESIAN_POINT('Ctrl Pts',(-1.5732631427069,5.15734264299855,59.7554100183284));
#56575=CARTESIAN_POINT('Ctrl Pts',(-5.18615337446655,1.47551795312722,59.9141707805741));
#56576=CARTESIAN_POINT('Ctrl Pts',(-4.05251762479693,-3.55674583772888,
60.0729315428202));
#56577=CARTESIAN_POINT('Ctrl Pts',(0.790106040849496,-5.33376719567931,
60.2316923050659));
#56578=CARTESIAN_POINT('Ctrl Pts',(4.90960052380718,-2.22916189410365,60.3904530673119));
#56579=CARTESIAN_POINT('Ctrl Pts',(4.53567864167587,2.91564046359228,60.5492138295578));
#56580=CARTESIAN_POINT('Ctrl Pts',(0.0105651225747838,5.39195960961101,
60.7079745918036));
#56581=CARTESIAN_POINT('Ctrl Pts',(-4.52421791942263,2.93339262136295,60.8667353540496));
#56582=CARTESIAN_POINT('Ctrl Pts',(-4.91829852752871,-2.20990489560075,
61.0254961162954));
#56583=CARTESIAN_POINT('Ctrl Pts',(-0.811002091855911,-5.3306299496867,
61.1842568785414));
#56584=CARTESIAN_POINT('Ctrl Pts',(4.03854823066489,-3.57259964760746,61.3430176407872));
#56585=CARTESIAN_POINT('Ctrl Pts',(5.19189585341926,1.4551829784393,61.5017784030331));
#56586=CARTESIAN_POINT('Ctrl Pts',(1.5934618026005,5.15113769347555,61.660539165279));
#56587=CARTESIAN_POINT('Ctrl Pts',(-3.4633571628827,4.1326138478934,61.8192999275249));
#56588=CARTESIAN_POINT('Ctrl Pts',(-5.35040586327371,-0.668204423614378,
61.9780606897707));
#56589=CARTESIAN_POINT('Ctrl Pts',(-2.34059968732153,-4.85746159606041,
62.1368214520167));
#56590=CARTESIAN_POINT('Ctrl Pts',(2.81139481701569,-4.60102154269558,62.2955822142625));
#56591=CARTESIAN_POINT('Ctrl Pts',(5.39031490964729,-0.133586033422769,
62.4543429765085));
#56592=CARTESIAN_POINT('Ctrl Pts',(3.03585414765692,4.45611149407704,62.6131037387543));
#56593=CARTESIAN_POINT('Ctrl Pts',(-2.09711306164141,4.96743966849971,62.7718645010003));
#56594=CARTESIAN_POINT('Ctrl Pts',(-5.310738339773,0.932415325891086,62.930625263246));
#56595=CARTESIAN_POINT('Ctrl Pts',(-3.66381367072956,-3.95598400396999,
63.089386025492));
#56596=CARTESIAN_POINT('Ctrl Pts',(1.33634518241131,-5.223745936293,63.2481467877379));
#56597=CARTESIAN_POINT('Ctrl Pts',(5.11344010541426,-1.71057602632341,63.4069075499838));
#56598=CARTESIAN_POINT('Ctrl Pts',(4.21055845188033,3.36816531316245,63.5656683122297));
#56599=CARTESIAN_POINT('Ctrl Pts',(-0.545954909997053,5.36425887609291,
63.7244290744756));
#56600=CARTESIAN_POINT('Ctrl Pts',(-4.80279366183524,2.45081886220229,63.8831898367214));
#56601=CARTESIAN_POINT('Ctrl Pts',(-4.66396895111927,-2.70568543561274,
64.0419505989674));
#56602=CARTESIAN_POINT('Ctrl Pts',(-0.256537393552353,-5.38586377651727,
64.2007113612132));
#56603=CARTESIAN_POINT('Ctrl Pts',(4.38568502263036,-3.13673507580205,64.3594721234591));
#56604=CARTESIAN_POINT('Ctrl Pts',(5.01399454360851,1.98322937910761,64.5182328857051));
#56605=CARTESIAN_POINT('Ctrl Pts',(1.05334310381863,5.28808172772786,64.6769936479507));
#56606=CARTESIAN_POINT('Ctrl Pts',(-3.87136011937014,3.75312015257198,64.8357544101969));
#56607=CARTESIAN_POINT('Ctrl Pts',(-5.25287630907674,-1.21681162676554,
64.9945151724425));
#56608=CARTESIAN_POINT('Ctrl Pts',(-1.82679964952023,-5.07308023729216,
65.1532759346887));
#56609=CARTESIAN_POINT('Ctrl Pts',(3.27121984959904,-4.28631085539543,65.3120366969344));
#56610=CARTESIAN_POINT('Ctrl Pts',(5.3753190216539,0.423421148429019,65.4707974591804));
#56611=CARTESIAN_POINT('Ctrl Pts',(2.55976203383379,4.7456251836438,65.6295582214262));
#56612=CARTESIAN_POINT('Ctrl Pts',(-2.59856735630046,4.7244880937792,65.7883189836722));
#56613=CARTESIAN_POINT('Ctrl Pts',(-5.37860852767513,0.379355189119878,
65.947079745918));
#56614=CARTESIAN_POINT('Ctrl Pts',(-3.23598288278473,-4.31297517217702,
66.1058405081639));
#56615=CARTESIAN_POINT('Ctrl Pts',(1.86831314081432,-5.05793891435551,66.2646012704098));
#56616=CARTESIAN_POINT('Ctrl Pts',(5.26267190957225,-1.17372246536004,66.4233620326557));
#56617=CARTESIAN_POINT('Ctrl Pts',(3.84047259628301,3.78472063575253,66.5821227949015));
#56618=CARTESIAN_POINT('Ctrl Pts',(-1.09664454588739,5.27927180522719,66.7408835571475));
#56619=CARTESIAN_POINT('Ctrl Pts',(-5.03007910221774,1.94207216110101,66.8996443193933));
#56620=CARTESIAN_POINT('Ctrl Pts',(-4.35983161843177,-3.17257124623133,
67.0584050816393));
#56621=CARTESIAN_POINT('Ctrl Pts',(0.300666935333765,-5.38358054156236,
67.2171658438851));
#56622=CARTESIAN_POINT('Ctrl Pts',(4.68598592589077,-2.66737248164657,67.375926606131));
#56623=CARTESIAN_POINT('Ctrl Pts',(4.78254746176859,2.49009634942548,67.534687368377));
#56624=CARTESIAN_POINT('Ctrl Pts',(0.50197547582154,5.3685529405199,67.6934481306227));
#56625=CARTESIAN_POINT('Ctrl Pts',(-4.23801979863793,3.33354589586587,67.8522088928688));
#56626=CARTESIAN_POINT('Ctrl Pts',(-5.09924990138375,-1.75242417716988,
68.0109696551145));
#56627=CARTESIAN_POINT('Ctrl Pts',(-1.29349073576672,-5.2345221147663,68.1697304173606));
#56628=CARTESIAN_POINT('Ctrl Pts',(3.69611066141296,-3.92582552236859,68.3284911796063));
#56629=CARTESIAN_POINT('Ctrl Pts',(5.30291868209728,0.975906504002708,68.4872519418522));
#56630=CARTESIAN_POINT('Ctrl Pts',(2.05633354516605,4.98445908845845,68.6460127040982));
#56631=CARTESIAN_POINT('Ctrl Pts',(-3.07227086382722,4.43108246287181,68.804773466344));
#56632=CARTESIAN_POINT('Ctrl Pts',(-5.38903913451035,-0.177756181911403,
68.96353422859));
#56633=CARTESIAN_POINT('Ctrl Pts',(-2.77359417894579,-4.62390693937597,
69.1222949908358));
#56634=CARTESIAN_POINT('Ctrl Pts',(2.38032888972716,-4.83811682684714,69.2810557530817));
#56635=CARTESIAN_POINT('Ctrl Pts',(5.35570225042921,-0.624334412185203,
69.4398165153275));
#56636=CARTESIAN_POINT('Ctrl Pts',(3.42937331948324,4.16085792705156,69.5985772775736));
#56637=CARTESIAN_POINT('Ctrl Pts',(-1.63562282502583,5.13790599639058,69.7573380398193));
#56638=CARTESIAN_POINT('Ctrl Pts',(-5.20364699932156,1.4125855584507,69.9160988020653));
#56639=CARTESIAN_POINT('Ctrl Pts',(-4.00913449237088,-3.60557633057093,
70.0748595643111));
#56640=CARTESIAN_POINT('Ctrl Pts',(0.854660362605124,-5.32380462809097,
70.233620326557));
#56641=CARTESIAN_POINT('Ctrl Pts',(4.93624394778424,-2.1695243122525,70.392381088803));
#56642=CARTESIAN_POINT('Ctrl Pts',(4.50002629241666,2.97037092314251,70.5511418510488));
#56643=CARTESIAN_POINT('Ctrl Pts',(-0.0547528808636342,5.39169195851627,
70.7099026132947));
#56644=CARTESIAN_POINT('Ctrl Pts',(-4.55942054512895,2.87837182208054,70.8686633755406));
#56645=CARTESIAN_POINT('Ctrl Pts',(-4.89116725717831,-2.26932212693528,
71.0274241377865));
#56646=CARTESIAN_POINT('Ctrl Pts',(-0.746368292808977,-5.34006314803305,
71.1861849000323));
#56647=CARTESIAN_POINT('Ctrl Pts',(4.08152973125557,-3.52341526169831,71.3449456622782));
#56648=CARTESIAN_POINT('Ctrl Pts',(5.17388707332602,1.51796989626334,71.5037064245242));
#56649=CARTESIAN_POINT('Ctrl Pts',(1.53094492744998,5.1700626381705,71.66246718677));
#56650=CARTESIAN_POINT('Ctrl Pts',(-3.51316477934987,4.09035613200449,71.8212279490159));
#56651=CARTESIAN_POINT('Ctrl Pts',(-5.34191876907334,-0.732969247726808,
71.9799887112618));
#56652=CARTESIAN_POINT('Ctrl Pts',(-2.28158553030752,-4.88545878310146,
72.1387494735077));
#56653=CARTESIAN_POINT('Ctrl Pts',(2.86692447773331,-4.56662721189998,72.2975102357536));
#56654=CARTESIAN_POINT('Ctrl Pts',(5.39153763240408,-0.0682789269231456,
72.4562709979995));
#56655=CARTESIAN_POINT('Ctrl Pts',(2.98165085923738,4.49256031758063,72.6150317602455));
#56656=CARTESIAN_POINT('Ctrl Pts',(-2.15713385601469,4.94167113239301,72.7737925224911));
#56657=CARTESIAN_POINT('Ctrl Pts',(-5.32164377573057,0.868013581529248,
72.9325532847373));
#56658=CARTESIAN_POINT('Ctrl Pts',(-3.61562276017225,-4.00007651297025,
73.091314046983));
#56659=CARTESIAN_POINT('Ctrl Pts',(1.39952664613108,-5.20717439887132,73.250074809229));
#56660=CARTESIAN_POINT('Ctrl Pts',(5.13378651679711,-1.64850721971224,73.4088355714748));
#56661=CARTESIAN_POINT('Ctrl Pts',(4.16944815373948,3.41892412123604,73.5675963337207));
#56662=CARTESIAN_POINT('Ctrl Pts',(-0.610896517072584,5.35725167403211,
73.7263570959665));
#56663=CARTESIAN_POINT('Ctrl Pts',(-4.83213003538284,2.39245885537094,73.8851178582126));
#56664=CARTESIAN_POINT('Ctrl Pts',(-4.63085054597687,-2.76198538633308,
74.0438786204583));
#56665=CARTESIAN_POINT('Ctrl Pts',(-0.191275185721079,-5.38857623652284,
74.2026393827044));
#56666=CARTESIAN_POINT('Ctrl Pts',(4.42336106708315,-3.08337751884262,74.3614001449501));
#56667=CARTESIAN_POINT('Ctrl Pts',(4.98960215796993,2.04382248707493,74.5201609071961));
#56668=CARTESIAN_POINT('Ctrl Pts',(0.989206944500219,5.30045372345089,74.678921669442));
#56669=CARTESIAN_POINT('Ctrl Pts',(-3.9165406802957,3.70594780765739,74.8376824316877));
#56670=CARTESIAN_POINT('Ctrl Pts',(-5.23775064219211,-1.2803547413539,74.9964431939339));
#56671=CARTESIAN_POINT('Ctrl Pts',(-1.76521122717783,-5.09483752213321,
75.1552039561795));
#56672=CARTESIAN_POINT('Ctrl Pts',(3.32290342202856,-4.24636937881787,75.3139647184255));
#56673=CARTESIAN_POINT('Ctrl Pts',(5.36979535998785,0.488505727033064,75.4727254806714));
#56674=CARTESIAN_POINT('Ctrl Pts',(2.50208656195135,4.77628546990172,75.6314862429173));
#56675=CARTESIAN_POINT('Ctrl Pts',(-2.65560828481232,4.69266285717694,75.7902470051632));
#56676=CARTESIAN_POINT('Ctrl Pts',(-5.38280931270438,0.314171858310403,
75.9490077674091));
#56677=CARTESIAN_POINT('Ctrl Pts',(-3.18349883755812,-4.35185882178607,
76.107768529655));
#56678=CARTESIAN_POINT('Ctrl Pts',(1.92944701495941,-5.03493537892548,76.2665292919008));
#56679=CARTESIAN_POINT('Ctrl Pts',(5.27650402365974,-1.10988528316864,76.4252900541468));
#56680=CARTESIAN_POINT('Ctrl Pts',(3.7943433769926,3.83096572563162,76.5840508163925));
#56681=CARTESIAN_POINT('Ctrl Pts',(-1.16051622802576,5.26559988396195,76.7428115786386));
#56682=CARTESIAN_POINT('Ctrl Pts',(-5.0532359327251,1.88099618864767,76.9015723408843));
#56683=CARTESIAN_POINT('Ctrl Pts',(-4.32107975869319,-3.22515267429361,
77.0603331031303));
#56684=CARTESIAN_POINT('Ctrl Pts',(0.365860599594574,-5.37954329615034,
77.2190938653761));
#56685=CARTESIAN_POINT('Ctrl Pts',(4.7179541617759,-2.61041157308061,77.3778546276221));
#56686=CARTESIAN_POINT('Ctrl Pts',(4.75203196331349,2.54784855773221,77.5366153898679));
#56687=CARTESIAN_POINT('Ctrl Pts',(0.436904959320356,5.37423986346092,77.6953761521139));
#56688=CARTESIAN_POINT('Ctrl Pts',(-4.27809080887851,3.28196268785622,77.8541369143598));
#56689=CARTESIAN_POINT('Ctrl Pts',(-5.07764719280662,-1.81406698853016,
78.0128976766055));
#56690=CARTESIAN_POINT('Ctrl Pts',(-1.22998576712498,-5.24980714561609,
78.1716584388517));
#56691=CARTESIAN_POINT('Ctrl Pts',(3.74339620303386,-3.88076344558682,78.3304192010973));
#56692=CARTESIAN_POINT('Ctrl Pts',(5.29070762465021,1.0400734993063,78.4891799633433));
#56693=CARTESIAN_POINT('Ctrl Pts',(1.99580182141817,5.00900340817564,78.6479407255891));
#56694=CARTESIAN_POINT('Ctrl Pts',(-3.12572277133616,4.39354039588141,78.8067014878351));
#56695=CARTESIAN_POINT('Ctrl Pts',(-5.38649040731852,-0.243024989162281,
78.965462250081));
#56696=CARTESIAN_POINT('Ctrl Pts',(-2.71737749003105,-4.65716648082978,
79.1242230123268));
#56697=CARTESIAN_POINT('Ctrl Pts',(2.43876230950906,-4.8089269542393,79.2829837745728));
#56698=CARTESIAN_POINT('Ctrl Pts',(5.36287235042167,-0.559410588542699,
79.4417445368186));
#56699=CARTESIAN_POINT('Ctrl Pts',(3.37871780515969,4.20209543520715,79.6005052990646));
#56700=CARTESIAN_POINT('Ctrl Pts',(-1.69774247966381,5.11771536197905,79.7592660613104));
#56701=CARTESIAN_POINT('Ctrl Pts',(-5.2203769888794,1.34944586681667,79.9180268235563));
#56702=CARTESIAN_POINT('Ctrl Pts',(-3.96516301938171,-3.65387770501744,
80.0767875858022));
#56703=CARTESIAN_POINT('Ctrl Pts',(0.91908926293675,-5.31306079207099,80.235548348048));
#56704=CARTESIAN_POINT('Ctrl Pts',(4.96216297786599,-2.10956835266785,80.3943091102941));
#56705=CARTESIAN_POINT('Ctrl Pts',(4.46371356421533,3.02466548070436,80.5530698725397));
#56706=CARTESIAN_POINT('Ctrl Pts',(-0.120062849320441,5.39063307652007,
80.7118306347859));
#56707=CARTESIAN_POINT('Ctrl Pts',(-4.59395407577343,2.82292862168424,80.8705913970315));
#56708=CARTESIAN_POINT('Ctrl Pts',(-4.86331820795707,-2.32840633521552,
81.0293521592777));
#56709=CARTESIAN_POINT('Ctrl Pts',(-0.681624964166643,-5.34871269198804,
81.1881129215234));
#56710=CARTESIAN_POINT('Ctrl Pts',(4.12391226721417,-3.47371381457424,81.3468736837694));
#56711=CARTESIAN_POINT('Ctrl Pts',(5.15511902533117,1.58053405205645,81.5056344460152));
#56712=CARTESIAN_POINT('Ctrl Pts',(1.46820338586184,5.18822887591951,81.6643952082611));
#56713=CARTESIAN_POINT('Ctrl Pts',(-3.56245683835765,4.04749815657105,81.823155970507));
#56714=CARTESIAN_POINT('Ctrl Pts',(-5.33264774907332,-0.797626509155247,
81.9819167327528));
#56715=CARTESIAN_POINT('Ctrl Pts',(-2.22223654888384,-4.91273902788576,
82.1406774949988));
#56716=CARTESIAN_POINT('Ctrl Pts',(2.92203341399256,-4.53156273055457,82.2994382572446));
#56717=CARTESIAN_POINT('Ctrl Pts',(5.39196915310808,-0.0029617965042665,
82.4581990194906));
#56718=CARTESIAN_POINT('Ctrl Pts',(2.92701000162586,4.52834985013744,82.6169597817364));
#56719=CARTESIAN_POINT('Ctrl Pts',(-2.21683806821556,4.91517742057454,82.7757205439824));
#56720=CARTESIAN_POINT('Ctrl Pts',(-5.33176830391211,0.803484428152502,
82.9344813062282));
#56721=CARTESIAN_POINT('Ctrl Pts',(-3.56690117349271,-4.04358195702611,
83.0932420684741));
#56722=CARTESIAN_POINT('Ctrl Pts',(1.46250256952503,-5.18983881124397,83.2520028307201));
#56723=CARTESIAN_POINT('Ctrl Pts',(5.15337985091046,-1.58619629785924,83.4107635929658));
#56724=CARTESIAN_POINT('Ctrl Pts',(4.12772540290961,3.46918082523772,83.5695243552118));
#56725=CARTESIAN_POINT('Ctrl Pts',(-0.675747352509778,5.34945901705833,
83.7282851174576));
#56726=CARTESIAN_POINT('Ctrl Pts',(-4.86075944383677,2.33374637252957,83.8870458797035));
#56727=CARTESIAN_POINT('Ctrl Pts',(-4.59704844530487,-2.81787736745293,
84.0458066419496));
#56728=CARTESIAN_POINT('Ctrl Pts',(-0.125992795831606,-5.39050299503273,
84.2045674041953));
#56729=CARTESIAN_POINT('Ctrl Pts',(4.46040309055735,-3.02955776127604,84.3633281664412));
#56730=CARTESIAN_POINT('Ctrl Pts',(4.96444861251837,2.10409705678322,84.5220889286871));
#56731=CARTESIAN_POINT('Ctrl Pts',(0.924981040394022,5.31208351664113,84.6808496909329));
#56732=CARTESIAN_POINT('Ctrl Pts',(-3.96125263942776,3.65816335371309,84.8396104531789));
#56733=CARTESIAN_POINT('Ctrl Pts',(-5.22165301904991,-1.3435792187099,84.9983712154247));
#56734=CARTESIAN_POINT('Ctrl Pts',(-1.70375320028204,-5.11609758128303,
85.1571319776708));
#56735=CARTESIAN_POINT('Ctrl Pts',(3.37484546343723,-4.20532487574203,85.3158927399164));
#56736=CARTESIAN_POINT('Ctrl Pts',(5.36205285859353,0.552597767150946,85.4746535021625));
#56737=CARTESIAN_POINT('Ctrl Pts',(2.4468005092104,4.80802425479881,85.6334142644084));
#56738=CARTESIAN_POINT('Ctrl Pts',(-2.7176845769921,4.65659903150035,85.7921750266542));
#56739=CARTESIAN_POINT('Ctrl Pts',(-4.93173550418608,0.99029557446776,85.9244756618591));
#56740=CARTESIAN_POINT('Ctrl Pts',(-4.26716318148111,-2.08115166207624,
86.0303161700231));
#56741=CARTESIAN_POINT('Ctrl Pts',(-3.26619649360748,-3.2739962098191,86.083236424105));
#56742=CARTESIAN_POINT('Ctrl Pts',(-2.64867169498456,-3.71434815979703,
86.109696551146));
#56743=CARTESIAN_POINT('Ctrl Pts',(-2.08577545033697,4.2697827545171,25.890303448854));
#56744=CARTESIAN_POINT('Ctrl Pts',(-2.79564340622372,3.92301449006545,25.9167635758949));
#56745=CARTESIAN_POINT('Ctrl Pts',(-4.02828411678504,2.86869268329956,25.9696838299769));
#56746=CARTESIAN_POINT('Ctrl Pts',(-5.2368061558258,-0.173451583736938,
26.0755243381408));
#56747=CARTESIAN_POINT('Ctrl Pts',(-3.58937700474797,-4.31948327041665,
26.2078249733457));
#56748=CARTESIAN_POINT('Ctrl Pts',(1.69117135154962,-5.35897536965486,26.3665857355916));
#56749=CARTESIAN_POINT('Ctrl Pts',(5.4148867130437,-1.48550731689914,26.5253464978375));
#56750=CARTESIAN_POINT('Ctrl Pts',(4.18736849490951,3.74332949976516,26.6841072600834));
#56751=CARTESIAN_POINT('Ctrl Pts',(-0.874969621673782,5.54834523009075,
26.8428680223293));
#56752=CARTESIAN_POINT('Ctrl Pts',(-5.13525022907948,2.27420458855161,27.0016287845751));
#56753=CARTESIAN_POINT('Ctrl Pts',(-4.6962499784134,-3.08076179886732,27.1603895468211));
#56754=CARTESIAN_POINT('Ctrl Pts',(0.0412447165789918,-5.61643191744809,
27.319150309067));
#56755=CARTESIAN_POINT('Ctrl Pts',(4.7408118992853,-3.01160959987317,27.4779110713129));
#56756=CARTESIAN_POINT('Ctrl Pts',(5.1015367238218,2.34944503074463,27.6366718335587));
#56757=CARTESIAN_POINT('Ctrl Pts',(0.793130492629709,5.56026007017329,27.7954325958046));
#56758=CARTESIAN_POINT('Ctrl Pts',(-4.24114750411255,3.68213214181093,27.9541933580505));
#56759=CARTESIAN_POINT('Ctrl Pts',(-5.39381106478857,-1.56598352850948,
28.1129541202964));
#56760=CARTESIAN_POINT('Ctrl Pts',(-1.60988703512753,-5.3808695398533,28.2717148825423));
#56761=CARTESIAN_POINT('Ctrl Pts',(3.6474511562916,-4.2710160983281,28.4304756447882));
#56762=CARTESIAN_POINT('Ctrl Pts',(5.5665325305163,0.747800018975952,28.5892364070341));
#56763=CARTESIAN_POINT('Ctrl Pts',(2.39095231205807,5.08220761366869,28.74799716928));
#56764=CARTESIAN_POINT('Ctrl Pts',(-2.97289997872796,4.76522309415968,28.9067579315259));
#56765=CARTESIAN_POINT('Ctrl Pts',(-5.61586367010893,0.0869610876472672,
29.0655186937718));
#56766=CARTESIAN_POINT('Ctrl Pts',(-3.11901725108991,-4.67089049014597,
29.2242794560176));
#56767=CARTESIAN_POINT('Ctrl Pts',(2.23244895427517,-5.15380035052699,29.3830402182635));
#56768=CARTESIAN_POINT('Ctrl Pts',(5.54070972400729,-0.91979474000819,29.5418009805094));
#56769=CARTESIAN_POINT('Ctrl Pts',(3.77794369111745,4.15603513022305,29.7005617427553));
#56770=CARTESIAN_POINT('Ctrl Pts',(-1.44251179621886,5.42813469204637,29.8593225050012));
#56771=CARTESIAN_POINT('Ctrl Pts',(-5.34273643101869,1.73223958412626,30.0180832672471));
#56772=CARTESIAN_POINT('Ctrl Pts',(-4.35312548529055,-3.54905410571791,
30.176844029493));
#56773=CARTESIAN_POINT('Ctrl Pts',(0.620598871036556,-5.58214506939038,
30.3356047917389));
#56774=CARTESIAN_POINT('Ctrl Pts',(5.02633218492865,-2.50628635742007,30.4943655539847));
#56775=CARTESIAN_POINT('Ctrl Pts',(4.83181275145273,2.86340218474256,30.6531263162307));
#56776=CARTESIAN_POINT('Ctrl Pts',(0.215070698416827,5.61241758347815,30.8118870784765));
#56777=CARTESIAN_POINT('Ctrl Pts',(-4.59851062734073,3.22477697638755,30.9706478407224));
#56778=CARTESIAN_POINT('Ctrl Pts',(-5.2033945635623,-2.11427802164059,31.1294086029683));
#56779=CARTESIAN_POINT('Ctrl Pts',(-1.04597285548533,-5.51828119277288,
31.2881693652142));
#56780=CARTESIAN_POINT('Ctrl Pts',(4.06875515960443,-3.87178485819991,31.4469301274601));
#56781=CARTESIAN_POINT('Ctrl Pts',(5.4596341708714,1.31828724381346,31.605690889706));
#56782=CARTESIAN_POINT('Ctrl Pts',(1.853689222264,5.30182259267667,31.7644516519519));
#56783=CARTESIAN_POINT('Ctrl Pts',(-3.4488087242362,4.43296795844451,31.9232124141977));
#56784=CARTESIAN_POINT('Ctrl Pts',(-5.59485158108012,-0.493074358126545,
32.0819731764437));
#56785=CARTESIAN_POINT('Ctrl Pts',(-2.62031537395337,-4.96783996098723,
32.2407339386895));
#56786=CARTESIAN_POINT('Ctrl Pts',(2.75241350199106,-4.89588668690527,32.3994947009355));
#56787=CARTESIAN_POINT('Ctrl Pts',(5.60604946734801,-0.343068370161422,
32.5582554631813));
#56788=CARTESIAN_POINT('Ctrl Pts',(3.3288577211775,4.52373659811392,32.7170162254272));
#56789=CARTESIAN_POINT('Ctrl Pts',(-1.99500629269775,5.25027965246184,32.8757769876731));
#56790=CARTESIAN_POINT('Ctrl Pts',(-5.49297960923532,1.17160639699654,33.034537749919));
#56791=CARTESIAN_POINT('Ctrl Pts',(-3.96361020215392,-3.97935682018335,
33.1932985121649));
#56792=CARTESIAN_POINT('Ctrl Pts',(1.19337633198882,-5.48829112449471,33.3520592744107));
#56793=CARTESIAN_POINT('Ctrl Pts',(5.25814839494067,-1.97417374963327,33.5108200366567));
#56794=CARTESIAN_POINT('Ctrl Pts',(4.51050243460883,3.34676774281486,33.6695807989025));
#56795=CARTESIAN_POINT('Ctrl Pts',(-0.365293128967798,5.60464516868708,
33.8283415611484));
#56796=CARTESIAN_POINT('Ctrl Pts',(-4.9067612628892,2.73298014006108,33.9871023233943));
#56797=CARTESIAN_POINT('Ctrl Pts',(-4.95741161004009,-2.63999179271414,
34.1458630856402));
#56798=CARTESIAN_POINT('Ctrl Pts',(-0.470887425572999,-5.59676259719809,
34.3046238478861));
#56799=CARTESIAN_POINT('Ctrl Pts',(4.4466073142222,-3.43120531738688,34.463384610132));
#56800=CARTESIAN_POINT('Ctrl Pts',(5.29443121665232,1.87469587642792,34.6221453723779));
#56801=CARTESIAN_POINT('Ctrl Pts',(1.296629949095,5.4648181408047,34.7809061346238));
#56802=CARTESIAN_POINT('Ctrl Pts',(-3.88788665395154,4.05337191767345,34.9396668968696));
#56803=CARTESIAN_POINT('Ctrl Pts',(-5.51409063425751,-1.06784409636987,
35.0984276591156));
#56804=CARTESIAN_POINT('Ctrl Pts',(-2.09363043599948,-5.21173657569289,
35.2571884213614));
#56805=CARTESIAN_POINT('Ctrl Pts',(3.2429842880596,-4.58568854637521,35.4159491836074));
#56806=CARTESIAN_POINT('Ctrl Pts',(5.61152073344166,0.237321712265504,35.5747099458532));
#56807=CARTESIAN_POINT('Ctrl Pts',(2.8442219974453,4.84312789075476,35.7334707080991));
#56808=CARTESIAN_POINT('Ctrl Pts',(-2.52619558850515,5.01635548835761,35.892231470345));
#56809=CARTESIAN_POINT('Ctrl Pts',(-5.58456180820669,0.598461316442061,
36.0509922325909));
#56810=CARTESIAN_POINT('Ctrl Pts',(-3.53176647837594,-4.36716293252018,
36.2097529948368));
#56811=CARTESIAN_POINT('Ctrl Pts',(1.7534094116762,-5.33582626891128,36.3685137570827));
#56812=CARTESIAN_POINT('Ctrl Pts',(5.43381144957445,-1.4209784190592,36.5272745193285));
#56813=CARTESIAN_POINT('Ctrl Pts',(4.14102327089027,3.79439228426682,36.6860352815745));
#56814=CARTESIAN_POINT('Ctrl Pts',(-0.941755894515449,5.5370192678104,36.8447960438203));
#56815=CARTESIAN_POINT('Ctrl Pts',(-5.16261129895229,2.2119970869982,37.0035568060662));
#56816=CARTESIAN_POINT('Ctrl Pts',(-4.65848714857258,-3.13751239416556,
37.1623175683121));
#56817=CARTESIAN_POINT('Ctrl Pts',(0.109226735523501,-5.61547469562505,
37.321078330558));
#56818=CARTESIAN_POINT('Ctrl Pts',(4.77697297489437,-2.95398302874052,37.4798390928039));
#56819=CARTESIAN_POINT('Ctrl Pts',(5.07268763310252,2.4110841366338,37.6385998550498));
#56820=CARTESIAN_POINT('Ctrl Pts',(0.725723622233936,5.56945345263699,37.7973606172957));
#56821=CARTESIAN_POINT('Ctrl Pts',(-4.2854448152198,3.63048884761598,37.9561213795416));
#56822=CARTESIAN_POINT('Ctrl Pts',(-5.37444325716809,-1.63121004546892,
38.1148821417874));
#56823=CARTESIAN_POINT('Ctrl Pts',(-1.54458706564933,-5.39997567898108,
38.2736429040334));
#56824=CARTESIAN_POINT('Ctrl Pts',(3.69892238837796,-4.22651862668493,38.4324036662792));
#56825=CARTESIAN_POINT('Ctrl Pts',(5.55706508750621,0.815177373445694,38.5911644285252));
#56826=CARTESIAN_POINT('Ctrl Pts',(2.32921207578554,5.11079814148172,38.749925190771));
#56827=CARTESIAN_POINT('Ctrl Pts',(-3.0304069744033,4.7288603390718,38.908685953017));
#56828=CARTESIAN_POINT('Ctrl Pts',(-5.61650499663195,0.0189251094235045,
39.0674467152627));
#56829=CARTESIAN_POINT('Ctrl Pts',(-3.0622060875641,-4.70833095844415,39.2262074775087));
#56830=CARTESIAN_POINT('Ctrl Pts',(2.29471736914525,-5.126378715302,39.3849682397545));
#56831=CARTESIAN_POINT('Ctrl Pts',(5.55144539655818,-0.852608084638733,
39.5437290020005));
#56832=CARTESIAN_POINT('Ctrl Pts',(3.72732102593349,4.20149550833897,39.7024897642464));
#56833=CARTESIAN_POINT('Ctrl Pts',(-1.50816140012871,5.41026207573349,39.8612505264922));
#56834=CARTESIAN_POINT('Ctrl Pts',(-5.3633284454033,1.66739153280986,40.0200112887382));
#56835=CARTESIAN_POINT('Ctrl Pts',(-4.30981347244434,-3.60152667207889,
40.178772050984));
#56836=CARTESIAN_POINT('Ctrl Pts',(0.688174435462339,-5.57421765661644,
40.3375328132299));
#56837=CARTESIAN_POINT('Ctrl Pts',(5.05632407947203,-2.4452143751233,40.4962935754758));
#56838=CARTESIAN_POINT('Ctrl Pts',(4.79677147851891,2.92172379252827,40.6550543377217));
#56839=CARTESIAN_POINT('Ctrl Pts',(0.147067101132706,5.61461110004271,40.8138150999676));
#56840=CARTESIAN_POINT('Ctrl Pts',(-4.63723757943327,3.16883482826894,40.9725758622135));
#56841=CARTESIAN_POINT('Ctrl Pts',(-5.1774007810357,-2.17715587165673,41.1313366244594));
#56842=CARTESIAN_POINT('Ctrl Pts',(-0.979048642068222,-5.53054701575012,
41.2900973867053));
#56843=CARTESIAN_POINT('Ctrl Pts',(4.11535871955024,-3.82221259827082,41.4488581489512));
#56844=CARTESIAN_POINT('Ctrl Pts',(5.44326407576748,1.38432754014994,41.607618911197));
#56845=CARTESIAN_POINT('Ctrl Pts',(1.7893278831762,5.32388882899019,41.7663796734429));
#56846=CARTESIAN_POINT('Ctrl Pts',(-3.50225584382976,4.39086444123689,41.9251404356888));
#56847=CARTESIAN_POINT('Ctrl Pts',(-5.58846804476507,-0.560813203837097,
42.0839011979347));
#56848=CARTESIAN_POINT('Ctrl Pts',(-2.55994358915231,-4.99921747449702,
42.2426619601806));
#56849=CARTESIAN_POINT('Ctrl Pts',(2.81151943374774,-4.86218520941121,42.4014227224265));
#56850=CARTESIAN_POINT('Ctrl Pts',(5.60979399190252,-0.275132523291236,
42.5601834846724));
#56851=CARTESIAN_POINT('Ctrl Pts',(3.27381373527952,4.56372985217721,42.7189442469183));
#56852=CARTESIAN_POINT('Ctrl Pts',(-2.05846085181392,5.22572726598967,42.8777050091642));
#56853=CARTESIAN_POINT('Ctrl Pts',(-5.50676919082185,1.10497946405063,43.03646577141));
#56854=CARTESIAN_POINT('Ctrl Pts',(-3.91511415993451,-4.02707929542473,
43.1952265336559));
#56855=CARTESIAN_POINT('Ctrl Pts',(1.25977293884402,-5.47343207498865,43.3539872959018));
#56856=CARTESIAN_POINT('Ctrl Pts',(5.28167736372706,-1.91033263136333,43.5127480581477));
#56857=CARTESIAN_POINT('Ctrl Pts',(4.46962933439137,3.40116158835573,43.6715088203935));
#56858=CARTESIAN_POINT('Ctrl Pts',(-0.433159988384986,5.59980883257818,
43.8302695826396));
#56859=CARTESIAN_POINT('Ctrl Pts',(-4.93950805874728,2.67333998483713,43.9890303448854));
#56860=CARTESIAN_POINT('Ctrl Pts',(-4.92506747450587,-2.69985127525994,
44.1477911071313));
#56861=CARTESIAN_POINT('Ctrl Pts',(-0.403054699451855,-5.60205618020814,
44.3065518693771));
#56862=CARTESIAN_POINT('Ctrl Pts',(4.48784604800658,-3.37708815199574,44.4653126316231));
#56863=CARTESIAN_POINT('Ctrl Pts',(5.27133300928694,1.93869410742388,44.6240733938689));
#56864=CARTESIAN_POINT('Ctrl Pts',(1.2303349855046,5.48012430154663,44.7828341561148));
#56865=CARTESIAN_POINT('Ctrl Pts',(-3.93670319808305,4.00597734231749,44.9415949183607));
#56866=CARTESIAN_POINT('Ctrl Pts',(-5.50075036662014,-1.13456244477178,
45.1003556806066));
#56867=CARTESIAN_POINT('Ctrl Pts',(-2.03034277701881,-5.23671602674481,
45.2591164428525));
#56868=CARTESIAN_POINT('Ctrl Pts',(3.2982965397378,-4.5460671434672,45.4178772050984));
#56869=CARTESIAN_POINT('Ctrl Pts',(5.60823411554676,0.305281250940591,45.5766379673442));
#56870=CARTESIAN_POINT('Ctrl Pts',(2.78534452306571,4.87722691955032,45.7353987295903));
#56871=CARTESIAN_POINT('Ctrl Pts',(-2.5867774563813,4.98538553455152,45.894159491836));
#56872=CARTESIAN_POINT('Ctrl Pts',(-5.59140169360195,0.53076702774728,46.052920254082));
#56873=CARTESIAN_POINT('Ctrl Pts',(-3.47860430924953,-4.40962567534128,
46.2116810163279));
#56874=CARTESIAN_POINT('Ctrl Pts',(1.81791799428017,-5.3141942665874,46.3704417785737));
#56875=CARTESIAN_POINT('Ctrl Pts',(5.45062622041652,-1.35504994087535,46.5292025408197));
#56876=CARTESIAN_POINT('Ctrl Pts',(4.09475483808194,3.84427748126524,46.6879633030655));
#56877=CARTESIAN_POINT('Ctrl Pts',(-1.00876124798033,5.52520472756723,46.8467240653114));
#56878=CARTESIAN_POINT('Ctrl Pts',(-5.18902822687748,2.14929583762384,47.0054848275573));
#56879=CARTESIAN_POINT('Ctrl Pts',(-4.62013807160538,-3.19371425400909,
47.1642455898032));
#56880=CARTESIAN_POINT('Ctrl Pts',(0.177243570754919,-5.61373950710082,
47.3230063520491));
#56881=CARTESIAN_POINT('Ctrl Pts',(4.81240648318495,-2.89589888938787,47.4817671142949));
#56882=CARTESIAN_POINT('Ctrl Pts',(5.04310798533405,2.47235684827615,47.6405278765409));
#56883=CARTESIAN_POINT('Ctrl Pts',(0.658203015566318,5.57783607927463,47.7992886387866));
#56884=CARTESIAN_POINT('Ctrl Pts',(-4.32910945912064,3.57830935329949,47.9580494010327));
#56885=CARTESIAN_POINT('Ctrl Pts',(-5.35428872245015,-1.69619539369769,
48.1168101632785));
#56886=CARTESIAN_POINT('Ctrl Pts',(-1.47905939811478,-5.41829030541985,
48.2755709255244));
#56887=CARTESIAN_POINT('Ctrl Pts',(3.74985026583283,-4.18140042578941,48.4343316877703));
#56888=CARTESIAN_POINT('Ctrl Pts',(5.54678242582246,0.882434846062579,48.5930924500162));
#56889=CARTESIAN_POINT('Ctrl Pts',(2.26712988102407,5.13863879247473,48.7518532122621));
#56890=CARTESIAN_POINT('Ctrl Pts',(-3.08746918127143,4.69180355424833,48.9106139745079));
#56891=CARTESIAN_POINT('Ctrl Pts',(-5.61632214089325,-0.0491136098317049,
49.0693747367539));
#56892=CARTESIAN_POINT('Ctrl Pts',(-3.00494552437603,-4.74508049799904,
49.2281354989997));
#56893=CARTESIAN_POINT('Ctrl Pts',(2.35664902330628,-5.09820477402661,49.3868962612456));
#56894=CARTESIAN_POINT('Ctrl Pts',(5.561366400077,-0.785296314172567,49.5456570234916));
#56895=CARTESIAN_POINT('Ctrl Pts',(3.67615137334867,4.24633931960047,49.7044177857373));
#56896=CARTESIAN_POINT('Ctrl Pts',(-1.57358967977417,5.39159550195178,49.8631785479833));
#56897=CARTESIAN_POINT('Ctrl Pts',(-5.38313339204505,1.60229879248781,50.0219393102291));
#56898=CARTESIAN_POINT('Ctrl Pts',(-4.26586899396583,-3.65347071471485,
50.1807000724751));
#56899=CARTESIAN_POINT('Ctrl Pts',(0.755649010055931,-5.56547222709447,
50.339460834721));
#56900=CARTESIAN_POINT('Ctrl Pts',(5.08557395847498,-2.38378355767454,50.4982215969668));
#56901=CARTESIAN_POINT('Ctrl Pts',(4.76102627921851,2.97961663734597,50.6569823592128));
#56902=CARTESIAN_POINT('Ctrl Pts',(0.0790419217800287,5.61598067229221,
50.8157431214586));
#56903=CARTESIAN_POINT('Ctrl Pts',(-4.6752840168385,3.11242765359339,50.9745038837046));
#56904=CARTESIAN_POINT('Ctrl Pts',(-5.15064721483666,-2.2397142240147,51.1332646459504));
#56905=CARTESIAN_POINT('Ctrl Pts',(-0.911980753248584,-5.54200123084275,
51.2920254081963));
#56906=CARTESIAN_POINT('Ctrl Pts',(4.16135835052739,-3.77207942857173,51.4507861704422));
#56907=CARTESIAN_POINT('Ctrl Pts',(5.42609518155485,1.45016468639448,51.6095469326881));
#56908=CARTESIAN_POINT('Ctrl Pts',(1.72470396018791,5.34517378451539,51.768307694934));
#56909=CARTESIAN_POINT('Ctrl Pts',(-3.55518900731147,4.34811656458864,51.9270684571799));
#56910=CARTESIAN_POINT('Ctrl Pts',(-5.58126440065713,-0.62846975019945,
52.0858292194257));
#56911=CARTESIAN_POINT('Ctrl Pts',(-2.49919613258049,-5.0298613527465,52.2445899816716));
#56912=CARTESIAN_POINT('Ctrl Pts',(2.87021277497366,-4.82777020614449,52.4033507439175));
#56913=CARTESIAN_POINT('Ctrl Pts',(5.61271527908117,-0.207156300717966,
52.5621115061634));
#56914=CARTESIAN_POINT('Ctrl Pts',(3.2182893171531,4.60305337879721,52.7208722684093));
#56915=CARTESIAN_POINT('Ctrl Pts',(-2.12161333176065,5.20040800394102,52.8796330306552));
#56916=CARTESIAN_POINT('Ctrl Pts',(-5.51975065392403,1.03819037534721,53.038393792901));
#56917=CARTESIAN_POINT('Ctrl Pts',(-3.86604357463707,-4.07421079670234,
53.197154555147));
#56918=CARTESIAN_POINT('Ctrl Pts',(1.32598467399636,-5.45776979922066,53.3559153173929));
#56919=CARTESIAN_POINT('Ctrl Pts',(5.30443124625904,-1.84621117174306,53.5146760796387));
#56920=CARTESIAN_POINT('Ctrl Pts',(4.4281003159834,3.4550563133683,53.6734368418847));
#56921=CARTESIAN_POINT('Ctrl Pts',(-0.500963281565584,5.59415072441577,
53.8321976041305));
#56922=CARTESIAN_POINT('Ctrl Pts',(-4.97152998170303,2.61330751691913,53.9909583663765));
#56923=CARTESIAN_POINT('Ctrl Pts',(-4.89200058522532,-2.75931455457936,
54.1497191286223));
#56924=CARTESIAN_POINT('Ctrl Pts',(-0.33516282504586,-5.60652766136632,
54.3084798908682));
#56925=CARTESIAN_POINT('Ctrl Pts',(4.5284261902974,-3.32247539885354,54.4672406531142));
#56926=CARTESIAN_POINT('Ctrl Pts',(5.24746123370139,2.00240783502248,54.6260014153599));
#56927=CARTESIAN_POINT('Ctrl Pts',(1.16385947023147,5.49462625394218,54.7847621776059));
#56928=CARTESIAN_POINT('Ctrl Pts',(-3.9849420309447,3.95799488970978,54.9435229398517));
#56929=CARTESIAN_POINT('Ctrl Pts',(-5.48660286376106,-1.20111429611312,
55.1022837020977));
#56930=CARTESIAN_POINT('Ctrl Pts',(-1.96675716519669,-5.26092698961938,
55.2610444643435));
#56931=CARTESIAN_POINT('Ctrl Pts',(3.35312476633552,-4.50577860511874,55.4198052265895));
#56932=CARTESIAN_POINT('Ctrl Pts',(5.60412448918787,0.373195989586127,55.5785659888352));
#56933=CARTESIAN_POINT('Ctrl Pts',(2.72605829932405,4.91061021520187,55.7373267510813));
#56934=CARTESIAN_POINT('Ctrl Pts',(-2.64697971461612,4.95368397532273,55.8960875133271));
#56935=CARTESIAN_POINT('Ctrl Pts',(-5.59742104069143,0.462994848981032,
56.054848275573));
#56936=CARTESIAN_POINT('Ctrl Pts',(-3.4249316548741,-4.45144130550992,56.2136090378189));
#56937=CARTESIAN_POINT('Ctrl Pts',(1.88215979738361,-5.29178240615308,56.3723698000648));
#56938=CARTESIAN_POINT('Ctrl Pts',(5.46664111175626,-1.28892260908666,56.5311305623107));
#56939=CARTESIAN_POINT('Ctrl Pts',(4.04788549992257,3.8935985304696,56.6898913245566));
#56940=CARTESIAN_POINT('Ctrl Pts',(-1.07561856571275,5.51257936342436,56.8486520868024));
#56941=CARTESIAN_POINT('Ctrl Pts',(-5.21468366481089,2.08627917904408,57.0074128490483));
#56942=CARTESIAN_POINT('Ctrl Pts',(-4.58111098928757,-3.24944743622466,
57.1661736112942));
#56943=CARTESIAN_POINT('Ctrl Pts',(0.245234395488895,-5.61118050219625,
57.3249343735402));
#56944=CARTESIAN_POINT('Ctrl Pts',(4.84713377073179,-2.83738977681774,57.4836951357859));
#56945=CARTESIAN_POINT('Ctrl Pts',(5.01278826137211,2.53326674150361,57.6424558980319));
#56946=CARTESIAN_POINT('Ctrl Pts',(0.590585817593506,5.58540015836071,57.8012166602777));
#56947=CARTESIAN_POINT('Ctrl Pts',(-4.37213880612535,3.52560474201678,57.9599774225237));
#56948=CARTESIAN_POINT('Ctrl Pts',(-5.33334844575954,-1.76093182521995,
58.1187381847696));
#56949=CARTESIAN_POINT('Ctrl Pts',(-1.41331467858517,-5.43580979765242,
58.2774989470154));
#56950=CARTESIAN_POINT('Ctrl Pts',(3.80022785268933,-4.1356686043012,58.4362597092614));
#56951=CARTESIAN_POINT('Ctrl Pts',(5.53568577371134,0.949562821348838,58.5950204715072));
#56952=CARTESIAN_POINT('Ctrl Pts',(2.20471498490915,5.16572534812638,58.7537812337531));
#56953=CARTESIAN_POINT('Ctrl Pts',(-3.144078301978,4.65405824716339,58.9125419959989));
#56954=CARTESIAN_POINT('Ctrl Pts',(-5.61531508977269,-0.117145121663757,
59.071302758245));
#56955=CARTESIAN_POINT('Ctrl Pts',(-2.94724398537462,-4.78113369689988,
59.2300635204908));
#56956=CARTESIAN_POINT('Ctrl Pts',(2.41823483917798,-5.06928267110287,59.3888242827367));
#56957=CARTESIAN_POINT('Ctrl Pts',(5.57047127296998,-0.717869301457213,
59.5475850449825));
#56958=CARTESIAN_POINT('Ctrl Pts',(3.6244422454793,4.29055998048545,59.7063458072285));
#56959=CARTESIAN_POINT('Ctrl Pts',(-1.63878703510391,5.37213771142675,59.8651065694744));
#56960=CARTESIAN_POINT('Ctrl Pts',(-5.40214836375828,1.53697091478732,60.0238673317203));
#56961=CARTESIAN_POINT('Ctrl Pts',(-4.22129849913074,-3.70487861045338,
60.1826280939661));
#56962=CARTESIAN_POINT('Ctrl Pts',(0.823012693142843,-5.55591006441646,
60.3413888562121));
#56963=CARTESIAN_POINT('Ctrl Pts',(5.11407752940203,-2.32200291994295,60.5001496184578));
#56964=CARTESIAN_POINT('Ctrl Pts',(4.72458239922035,3.03707222336503,60.6589103807039));
#56965=CARTESIAN_POINT('Ctrl Pts',(0.0110051430237869,5.61652609927038,
60.8176711429496));
#56966=CARTESIAN_POINT('Ctrl Pts',(-4.71264435622464,3.05556373009997,60.9764319051957));
#56967=CARTESIAN_POINT('Ctrl Pts',(-5.12313779106008,-2.30194389826733,
61.1351926674413));
#56968=CARTESIAN_POINT('Ctrl Pts',(-0.844779031235954,-5.55264215714847,
61.2939534296875));
#56969=CARTESIAN_POINT('Ctrl Pts',(4.20674730208683,-3.72139270614424,61.4527141919332));
#56970=CARTESIAN_POINT('Ctrl Pts',(5.4081300077703,1.51578902094353,61.6114749541792));
#56971=CARTESIAN_POINT('Ctrl Pts',(1.65982693686032,5.36567433568524,61.770235716425));
#56972=CARTESIAN_POINT('Ctrl Pts',(-3.60760044673811,4.30473060175118,61.9289964786709));
#56973=CARTESIAN_POINT('Ctrl Pts',(-5.5732417058914,-0.696034068613847,
62.0877572409168));
#56974=CARTESIAN_POINT('Ctrl Pts',(-2.43808191892836,-5.05976709874605,
62.2465180031627));
#56975=CARTESIAN_POINT('Ctrl Pts',(2.92848491241984,-4.79264672750744,62.4052787654085));
#56976=CARTESIAN_POINT('Ctrl Pts',(5.61481290018499,-0.139149677953565,
62.5640395276545));
#56977=CARTESIAN_POINT('Ctrl Pts',(3.16229261500766,4.64170140724564,62.7228002899003));
#56978=CARTESIAN_POINT('Ctrl Pts',(-2.18445446491029,5.17432558191808,62.8815610521463));
#56979=CARTESIAN_POINT('Ctrl Pts',(-5.53192209351194,0.97124893218624,63.0403218143921));
#56980=CARTESIAN_POINT('Ctrl Pts',(-3.81640564737093,-4.12074440746734,
63.199082576638));
#56981=CARTESIAN_POINT('Ctrl Pts',(1.39200182087229,-5.44130659563001,63.357843338884));
#56982=CARTESIAN_POINT('Ctrl Pts',(5.32640670340396,-1.78181878059799,63.5166041011298));
#56983=CARTESIAN_POINT('Ctrl Pts',(4.38592147376913,3.50844400880067,63.6753648633758));
#56984=CARTESIAN_POINT('Ctrl Pts',(-0.568693058375023,5.58767167452727,
63.8341256256215));
#56985=CARTESIAN_POINT('Ctrl Pts',(-5.00282233253868,2.55289154607289,63.9928863878675));
#56986=CARTESIAN_POINT('Ctrl Pts',(-4.85821579476509,-2.818372904435,64.1516471501133));
#56987=CARTESIAN_POINT('Ctrl Pts',(-0.267221765488804,-5.61017638448271,
64.3104079123593));
#56988=CARTESIAN_POINT('Ctrl Pts',(4.56834178595791,-3.26737507238287,64.4691686746051));
#56989=CARTESIAN_POINT('Ctrl Pts',(5.2228193930792,2.06582770923283,64.6279294368511));
#56990=CARTESIAN_POINT('Ctrl Pts',(1.0972131585588,5.50832186982966,64.7866901990968));
#56991=CARTESIAN_POINT('Ctrl Pts',(-4.03259607348695,3.90943160127608,64.9454509613429));
#56992=CARTESIAN_POINT('Ctrl Pts',(-5.4716502018265,-1.26748988390853,65.1042117235886));
#56993=CARTESIAN_POINT('Ctrl Pts',(-1.90288293172278,-5.28436591135743,
65.2629724858347));
#56994=CARTESIAN_POINT('Ctrl Pts',(3.40746092180959,-4.46482884367352,65.4217332480805));
#56995=CARTESIAN_POINT('Ctrl Pts',(5.59919245745271,0.441055961713188,65.5804940103263));
#56996=CARTESIAN_POINT('Ctrl Pts',(2.66637202647467,4.94327287871016,65.7392547725723));
#56997=CARTESIAN_POINT('Ctrl Pts',(-2.70679352852708,4.92125546287557,65.8980155348181));
#56998=CARTESIAN_POINT('Ctrl Pts',(-5.60261896613596,0.395154725711709,
66.0567762970641));
#56999=CARTESIAN_POINT('Ctrl Pts',(-3.37075639171248,-4.49260368658171,
66.2155370593099));
#57000=CARTESIAN_POINT('Ctrl Pts',(1.94612539350076,-5.26859397654912,66.3742978215559));
#57001=CARTESIAN_POINT('Ctrl Pts',(5.48185377340806,-1.22260612788034,66.5330585838017));
#57002=CARTESIAN_POINT('Ctrl Pts',(4.00042213448843,3.94234819401505,66.6918193460476));
#57003=CARTESIAN_POINT('Ctrl Pts',(-1.1423180364002,5.49914502815419,66.8505801082935));
#57004=CARTESIAN_POINT('Ctrl Pts',(-5.23957384781653,2.02295635895467,67.0093408705393));
#57005=CARTESIAN_POINT('Ctrl Pts',(-4.54141162884421,-3.30470376196668,
67.1681016327853));
#57006=CARTESIAN_POINT('Ctrl Pts',(0.31318923207078,-5.60779805644547,67.3268623950311));
#57007=CARTESIAN_POINT('Ctrl Pts',(4.88114974130499,-2.77846427724327,67.4856231572771));
#57008=CARTESIAN_POINT('Ctrl Pts',(4.98173291063654,2.59380487778839,67.6443839195229));
#57009=CARTESIAN_POINT('Ctrl Pts',(0.522881951140529,5.59214457986643,67.8031446817689));
#57010=CARTESIAN_POINT('Ctrl Pts',(-4.41452654167645,3.47238274817052,67.9619054440147));
#57011=CARTESIAN_POINT('Ctrl Pts',(-5.31162550008227,-1.82540983996319,
68.1206662062607));
#57012=CARTESIAN_POINT('Ctrl Pts',(-1.34736255509922,-5.45253158469304,
68.2794269685065));
#57013=CARTESIAN_POINT('Ctrl Pts',(3.85004775603573,-4.08932987336585,68.4381877307524));
#57014=CARTESIAN_POINT('Ctrl Pts',(5.52377675960678,1.01655144827307,68.5969484929983));
#57015=CARTESIAN_POINT('Ctrl Pts',(2.14197654682777,5.19205383348419,68.7557092552442));
#57016=CARTESIAN_POINT('Ctrl Pts',(-3.20022602913364,4.61562995694134,68.9144700174901));
#57017=CARTESIAN_POINT('Ctrl Pts',(-5.61348399105505,-0.185159442447144,
69.073230779736));
#57018=CARTESIAN_POINT('Ctrl Pts',(-2.88910993826166,-4.81648526433911,
69.2319915419818));
#57019=CARTESIAN_POINT('Ctrl Pts',(2.47946577904082,-5.0396166508499,69.3907523042278));
#57020=CARTESIAN_POINT('Ctrl Pts',(5.57875867909682,-0.650336941407984,
69.5495130664736));
#57021=CARTESIAN_POINT('Ctrl Pts',(3.57220123064088,4.33415100161104,69.7082738287195));
#57022=CARTESIAN_POINT('Ctrl Pts',(-1.70374389840499,5.35189155958961,69.8670345909654));
#57023=CARTESIAN_POINT('Ctrl Pts',(-5.42037057009564,1.47141748657539,70.0257953532113));
#57024=CARTESIAN_POINT('Ctrl Pts',(-4.17610852865976,-3.75574281518495,
70.1845561154572));
#57025=CARTESIAN_POINT('Ctrl Pts',(0.89025559910136,-5.54553257182993,70.343316877703));
#57026=CARTESIAN_POINT('Ctrl Pts',(5.14183060935358,-2.2598815282383,70.5020776399489));
#57027=CARTESIAN_POINT('Ctrl Pts',(4.68744518666451,3.09408211897719,70.6608384021949));
#57028=CARTESIAN_POINT('Ctrl Pts',(-0.0570332507375796,5.61624730093583,
70.8195991644407));
#57029=CARTESIAN_POINT('Ctrl Pts',(-4.74931311496125,2.99825140257037,70.9783599266866));
#57030=CARTESIAN_POINT('Ctrl Pts',(-5.09487654671437,-2.36383576220895,
71.1371206889325));
#57031=CARTESIAN_POINT('Ctrl Pts',(-0.777453337884133,-5.56246823311117,
71.2958814511784));
#57032=CARTESIAN_POINT('Ctrl Pts',(4.25151891339917,-3.67015986926562,71.4546422134243));
#57033=CARTESIAN_POINT('Ctrl Pts',(5.38937119080337,1.58119091342487,71.6134029756702));
#57034=CARTESIAN_POINT('Ctrl Pts',(1.59470633389773,5.38538747404349,71.7721637379161));
#57035=CARTESIAN_POINT('Ctrl Pts',(-3.65948247073021,4.26071291961525,71.9309245001618));
#57036=CARTESIAN_POINT('Ctrl Pts',(-5.56440113779842,-0.763496244015491,
72.089685262408));
#57037=CARTESIAN_POINT('Ctrl Pts',(-2.3766099167077,-5.08893032382693,72.2484460246537));
#57038=CARTESIAN_POINT('Ctrl Pts',(2.98632729464914,-4.75681992787116,72.4072067868998));
#57039=CARTESIAN_POINT('Ctrl Pts',(5.61608654738804,-0.0711226349710497,
72.5659675491454));
#57040=CARTESIAN_POINT('Ctrl Pts',(3.10583184636022,4.67966826592364,72.7247283113916));
#57041=CARTESIAN_POINT('Ctrl Pts',(-2.24697502932542,5.14748382751671,72.8834890736371));
#57042=CARTESIAN_POINT('Ctrl Pts',(-5.54328172342653,0.904164958225804,
73.0422498358833));
#57043=CARTESIAN_POINT('Ctrl Pts',(-3.76620766250282,-4.1666732989117,73.2010105981289));
#57044=CARTESIAN_POINT('Ctrl Pts',(1.45781469145456,-5.42404488019209,73.3597713603751));
#57045=CARTESIAN_POINT('Ctrl Pts',(5.34760051026307,-1.71716490751244,73.5185321226207));
#57046=CARTESIAN_POINT('Ctrl Pts',(4.3430989974944,3.56131684000752,73.6772928848668));
#57047=CARTESIAN_POINT('Ctrl Pts',(-0.636339379467287,5.58037263371339,
73.8360536471125));
#57048=CARTESIAN_POINT('Ctrl Pts',(-5.03338051910119,2.49210093834326,73.9948144093586));
#57049=CARTESIAN_POINT('Ctrl Pts',(-4.82371806104376,-2.87701765801306,
74.1535751716043));
#57050=CARTESIAN_POINT('Ctrl Pts',(-0.199241491132339,-5.61300181410709,
74.3123359338505));
#57051=CARTESIAN_POINT('Ctrl Pts',(4.60758697737389,-3.21179525855753,74.4710966960961));
#57052=CARTESIAN_POINT('Ctrl Pts',(5.19741110361085,2.12894442318739,74.6298574583422));
#57053=CARTESIAN_POINT('Ctrl Pts',(1.0304058308339,5.52120913937719,74.7886182205879));
#57054=CARTESIAN_POINT('Ctrl Pts',(-4.07965833247825,3.86029460367982,74.9473789828338));
#57055=CARTESIAN_POINT('Ctrl Pts',(-5.45589457511983,-1.33367946753936,
75.1061397450798));
#57056=CARTESIAN_POINT('Ctrl Pts',(-1.8387294501421,-5.30702935229665,75.2649005073255));
#57057=CARTESIAN_POINT('Ctrl Pts',(3.46129703232802,-4.42322386850986,75.4236612695716));
#57058=CARTESIAN_POINT('Ctrl Pts',(5.5934387441171,0.508851208869345,75.5824220318174));
#57059=CARTESIAN_POINT('Ctrl Pts',(2.60629446347919,4.97521011682889,75.7411827940634));
#57060=CARTESIAN_POINT('Ctrl Pts',(-2.76621012043596,4.88810475609477,75.8999435563092));
#57061=CARTESIAN_POINT('Ctrl Pts',(-5.60699470713969,0.327256613478776,
76.0587043185551));
#57062=CARTESIAN_POINT('Ctrl Pts',(-3.31608646998587,-4.53310677797631,
76.2174650808009));
#57063=CARTESIAN_POINT('Ctrl Pts',(2.00980539567907,-5.24463238067812,76.3762258430469));
#57064=CARTESIAN_POINT('Ctrl Pts',(5.49626197291347,-1.15611022920134,76.5349866052928));
#57065=CARTESIAN_POINT('Ctrl Pts',(3.95237170702942,3.99051931788734,76.6937473675386));
#57066=CARTESIAN_POINT('Ctrl Pts',(-1.20884987189374,5.48490369324573,76.8525081297847));
#57067=CARTESIAN_POINT('Ctrl Pts',(-5.26369512325953,1.95933666998091,77.0112688920303));
#57068=CARTESIAN_POINT('Ctrl Pts',(-4.50104581615728,-3.35947512236825,
77.1700296542764));
#57069=CARTESIAN_POINT('Ctrl Pts',(0.381098108126755,-5.60359266622235,
77.3287904165222));
#57070=CARTESIAN_POINT('Ctrl Pts',(4.91444940305996,-2.71913103798297,77.4875511787681));
#57071=CARTESIAN_POINT('Ctrl Pts',(4.94994649050095,2.65396237315744,77.646311941014));
#57072=CARTESIAN_POINT('Ctrl Pts',(0.455101351751309,5.59806835404786,77.8050727032599));
#57073=CARTESIAN_POINT('Ctrl Pts',(-4.45626644537291,3.41865118208945,77.9638334655057));
#57074=CARTESIAN_POINT('Ctrl Pts',(-5.28912307326102,-1.88961997577731,
78.1225942277517));
#57075=CARTESIAN_POINT('Ctrl Pts',(-1.28121270613263,-5.468453212619,78.2813549899975));
#57076=CARTESIAN_POINT('Ctrl Pts',(3.89930266479998,-4.04239103319333,78.4401157522435));
#57077=CARTESIAN_POINT('Ctrl Pts',(5.51105713115687,1.08339089625261,78.5988765144893));
#57078=CARTESIAN_POINT('Ctrl Pts',(2.07892377364716,5.21762038484239,78.7576372767352));
#57079=CARTESIAN_POINT('Ctrl Pts',(-3.2559041230579,4.57652432293467,78.9163980389812));
#57080=CARTESIAN_POINT('Ctrl Pts',(-5.61082911345409,-0.253146591078478,
79.0751588012269));
#57081=CARTESIAN_POINT('Ctrl Pts',(-2.83055191421017,-4.85113001247338,
79.2339195634729));
#57082=CARTESIAN_POINT('Ctrl Pts',(2.54033285725292,-5.00921106675685,79.3926803257188));
#57083=CARTESIAN_POINT('Ctrl Pts',(5.58622740228054,-0.582709144400273,
79.5514410879646));
#57084=CARTESIAN_POINT('Ctrl Pts',(3.51943599520346,4.37710598599406,79.7102018502106));
#57085=CARTESIAN_POINT('Ctrl Pts',(-1.7684507372563,5.33086001756339,79.8689626124564));
#57086=CARTESIAN_POINT('Ctrl Pts',(-5.43779733694764,1.40564812781938,80.0277233747023));
#57087=CARTESIAN_POINT('Ctrl Pts',(-4.13030571418267,-3.80605586458648,
80.1864841369483));
#57088=CARTESIAN_POINT('Ctrl Pts',(0.95736786003426,-5.53434127223174,80.345244899194));
#57089=CARTESIAN_POINT('Ctrl Pts',(5.16882912556325,-2.19742849887699,80.5040056614401));
#57090=CARTESIAN_POINT('Ctrl Pts',(4.64962009144032,3.15063795798068,80.6627664236858));
#57091=CARTESIAN_POINT('Ctrl Pts',(-0.125063274873211,5.61514431819889,
80.8215271859319));
#57092=CARTESIAN_POINT('Ctrl Pts',(-4.78528491189737,2.9404990815964,80.9802879481776));
#57093=CARTESIAN_POINT('Ctrl Pts',(-5.06586762915643,-2.42538073321897,
81.1390487104236));
#57094=CARTESIAN_POINT('Ctrl Pts',(-0.710013553204522,-5.5714780167311,
81.2978094726694));
#57095=CARTESIAN_POINT('Ctrl Pts',(4.29566661416096,-3.61838843639986,81.4565702349154));
#57096=CARTESIAN_POINT('Ctrl Pts',(5.36982148364171,1.64636076619313,81.6153309971612));
#57097=CARTESIAN_POINT('Ctrl Pts',(1.52935170749991,5.4043103065256,81.7740917594071));
#57098=CARTESIAN_POINT('Ctrl Pts',(-3.71082746511973,4.21606997808528,81.932852521653));
#57099=CARTESIAN_POINT('Ctrl Pts',(-5.55474399465067,-0.830846376919461,
82.0916132838989));
#57100=CARTESIAN_POINT('Ctrl Pts',(-2.3147891451765,-5.11734674715333,82.2503740461448));
#57101=CARTESIAN_POINT('Ctrl Pts',(3.04373142991963,-4.72029506698704,82.4091348083907));
#57102=CARTESIAN_POINT('Ctrl Pts',(5.61653604023885,-0.00308515058908493,
82.5678955706366));
#57103=CARTESIAN_POINT('Ctrl Pts',(3.04891528446413,4.71694837524191,82.7266563328824));
#57104=CARTESIAN_POINT('Ctrl Pts',(-2.30916582642725,5.11988669499558,82.8854170951283));
#57105=CARTESIAN_POINT('Ctrl Pts',(-5.55382792200581,0.836948268868883,
83.0441778573743));
#57106=CARTESIAN_POINT('Ctrl Pts',(-3.71545689970117,-4.21199067509615,
83.2029386196201));
#57107=CARTESIAN_POINT('Ctrl Pts',(1.52341346128536,-5.40598729308003,83.3616993818661));
#57108=CARTESIAN_POINT('Ctrl Pts',(5.36800987538946,-1.65225883547266,83.5204601441119));
#57109=CARTESIAN_POINT('Ctrl Pts',(4.29963856085619,3.61366665531133,83.6792209063577));
#57110=CARTESIAN_POINT('Ctrl Pts',(-0.703891148427739,5.57225542504627,
83.8379816686037));
#57111=CARTESIAN_POINT('Ctrl Pts',(-5.06320229660515,2.43094317454181,83.9967424308495));
#57112=CARTESIAN_POINT('Ctrl Pts',(-4.78850815696806,-2.93523745070957,
84.1555031930955));
#57113=CARTESIAN_POINT('Ctrl Pts',(-0.131240194167233,-5.61500881902578,
84.3142639553413));
#57114=CARTESIAN_POINT('Ctrl Pts',(4.64617174185204,-3.15573399420934,84.4730247175873));
#57115=CARTESIAN_POINT('Ctrl Pts',(5.17120995324134,2.19172933227414,84.6317854798331));
#57116=CARTESIAN_POINT('Ctrl Pts',(0.963505020594375,5.53332329484411,84.790546242079));
#57117=CARTESIAN_POINT('Ctrl Pts',(-4.12623247316118,3.81052000369223,84.949307004325));
#57118=CARTESIAN_POINT('Ctrl Pts',(-5.43912651173278,-1.39953714320699,
85.1080677665708));
#57119=CARTESIAN_POINT('Ctrl Pts',(-1.77471179476972,-5.32917485889023,
85.2668285288167));
#57120=CARTESIAN_POINT('Ctrl Pts',(3.51540237664497,-4.38046992755931,85.4255892910626));
#57121=CARTESIAN_POINT('Ctrl Pts',(5.58537377992907,0.575612579899635,85.5843500533083));
#57122=CARTESIAN_POINT('Ctrl Pts',(2.54870583510895,5.00827077132932,85.7431108155546));
#57123=CARTESIAN_POINT('Ctrl Pts',(-2.83087179085208,4.8505389297872,85.9018715778));
#57124=CARTESIAN_POINT('Ctrl Pts',(-5.13713439629382,1.0315398004976,86.0341722130053));
#57125=CARTESIAN_POINT('Ctrl Pts',(-4.44488369978034,-2.16782829859426,
86.140012721169));
#57126=CARTESIAN_POINT('Ctrl Pts',(-3.40222835107896,-3.41035291299011,
86.1929329752511));
#57127=CARTESIAN_POINT('Ctrl Pts',(-2.75898463274135,-3.86904481704426,
86.219393102292));
#57128=CARTESIAN_POINT('Ctrl Pts',(-2.16917135428577,4.44050218283316,26.));
#57129=CARTESIAN_POINT('Ctrl Pts',(-2.90742207776898,4.07986902565299,26.026460127041));
#57130=CARTESIAN_POINT('Ctrl Pts',(-4.18934766522561,2.98339209614179,26.0793803811229));
#57131=CARTESIAN_POINT('Ctrl Pts',(-5.44619024033903,-0.180386727026251,
26.1852208892869));
#57132=CARTESIAN_POINT('Ctrl Pts',(-3.73289165771545,-4.49218988265986,
26.3175215244917));
#57133=CARTESIAN_POINT('Ctrl Pts',(1.7587897347136,-5.57324416600043,26.4762822867377));
#57134=CARTESIAN_POINT('Ctrl Pts',(5.63139102185651,-1.54490260103424,26.6350430489835));
#57135=CARTESIAN_POINT('Ctrl Pts',(4.35479274028667,3.89299966074075,26.7938038112295));
#57136=CARTESIAN_POINT('Ctrl Pts',(-0.909953676412603,5.770185632809,26.9525645734753));
#57137=CARTESIAN_POINT('Ctrl Pts',(-5.34057378621867,2.36513448582097,27.1113253357212));
#57138=CARTESIAN_POINT('Ctrl Pts',(-4.88402091610239,-3.20394040614541,
27.2700860979671));
#57139=CARTESIAN_POINT('Ctrl Pts',(0.0428938108868349,-5.84099464142013,
27.428846860213));
#57140=CARTESIAN_POINT('Ctrl Pts',(4.93036456360867,-3.13202328336963,27.5876076224589));
#57141=CARTESIAN_POINT('Ctrl Pts',(5.30551230831797,2.44338327902792,27.7463683847048));
#57142=CARTESIAN_POINT('Ctrl Pts',(0.824842359969521,5.78257686590837,27.9051291469507));
#57143=CARTESIAN_POINT('Ctrl Pts',(-4.41072200448754,3.82935543872663,28.0638899091965));
#57144=CARTESIAN_POINT('Ctrl Pts',(-5.60947270247999,-1.62859650629097,
28.2226506714425));
#57145=CARTESIAN_POINT('Ctrl Pts',(-1.67425541405712,-5.59601373441819,
28.3814114336883));
#57146=CARTESIAN_POINT('Ctrl Pts',(3.79328779764178,-4.44178483963319,28.5401721959342));
#57147=CARTESIAN_POINT('Ctrl Pts',(5.78910011906805,0.777699430509262,28.6989329581801));
#57148=CARTESIAN_POINT('Ctrl Pts',(2.48655015281781,5.28541035916478,28.8576937204261));
#57149=CARTESIAN_POINT('Ctrl Pts',(-3.09176592905605,4.95575179531496,29.0164544826718));
#57150=CARTESIAN_POINT('Ctrl Pts',(-5.84040367375386,0.0904380671616019,
29.1752152449178));
#57151=CARTESIAN_POINT('Ctrl Pts',(-3.24372543242543,-4.85764747523187,
29.3339760071636));
#57152=CARTESIAN_POINT('Ctrl Pts',(2.32170932913062,-5.35986560023234,29.4927367694096));
#57153=CARTESIAN_POINT('Ctrl Pts',(5.76224483502612,-0.956571044848404,
29.6514975316554));
#57154=CARTESIAN_POINT('Ctrl Pts',(3.92899783701638,4.32220656851071,29.8102582939014));
#57155=CARTESIAN_POINT('Ctrl Pts',(-1.50018798335741,5.64516869698926,29.9690190561472));
#57156=CARTESIAN_POINT('Ctrl Pts',(-5.55635594320173,1.80150000520858,30.1277798183931));
#57157=CARTESIAN_POINT('Ctrl Pts',(-4.52717721976122,-3.69095652156115,
30.286540580639));
#57158=CARTESIAN_POINT('Ctrl Pts',(0.645412378085751,-5.80533689665976,
30.4453013428849));
#57159=CARTESIAN_POINT('Ctrl Pts',(5.22730085393893,-2.60649561834369,30.6040621051308));
#57160=CARTESIAN_POINT('Ctrl Pts',(5.02500391786172,2.97789006670843,30.7628228673767));
#57161=CARTESIAN_POINT('Ctrl Pts',(0.223669905634492,5.83681980167278,30.9215836296225));
#57162=CARTESIAN_POINT('Ctrl Pts',(-4.78237363643064,3.35371376626822,31.0803443918685));
#57163=CARTESIAN_POINT('Ctrl Pts',(-5.41144274686964,-2.19881354860029,
31.2391051541144));
#57164=CARTESIAN_POINT('Ctrl Pts',(-1.08779416073393,-5.73891954012705,
31.3978659163602));
#57165=CARTESIAN_POINT('Ctrl Pts',(4.23143686842713,-4.0265910709645,31.5566266786062));
#57166=CARTESIAN_POINT('Ctrl Pts',(5.67792762467303,1.37099654017823,31.715387440852));
#57167=CARTESIAN_POINT('Ctrl Pts',(1.92780558426513,5.51380624011119,31.8741482030979));
#57168=CARTESIAN_POINT('Ctrl Pts',(-3.58670301245285,4.61021204769197,32.0329089653438));
#57169=CARTESIAN_POINT('Ctrl Pts',(-5.81855145490275,-0.512789031536669,
32.1916697275897));
#57170=CARTESIAN_POINT('Ctrl Pts',(-2.72508387585791,-5.16646992575742,
32.3504304898355));
#57171=CARTESIAN_POINT('Ctrl Pts',(2.86246370514321,-5.09163973204659,32.5091912520815));
#57172=CARTESIAN_POINT('Ctrl Pts',(5.83019706810478,-0.35678532940591,32.6679520143274));
#57173=CARTESIAN_POINT('Ctrl Pts',(3.46195598864868,4.7046099048568,32.8267127765732));
#57174=CARTESIAN_POINT('Ctrl Pts',(-2.0747729584413,5.46020245001391,32.9854735388191));
#57175=CARTESIAN_POINT('Ctrl Pts',(-5.71260631920057,1.21845092886281,33.144234301065));
#57176=CARTESIAN_POINT('Ctrl Pts',(-4.12208788279547,-4.13846410045175,
33.3029950633109));
#57177=CARTESIAN_POINT('Ctrl Pts',(1.24109129475792,-5.70773037400097,33.4617558255568));
#57178=CARTESIAN_POINT('Ctrl Pts',(5.46838580972161,-2.05310746437012,33.6205165878027));
#57179=CARTESIAN_POINT('Ctrl Pts',(4.69084659760865,3.48058210963631,33.7792773500486));
#57180=CARTESIAN_POINT('Ctrl Pts',(-0.379898704410712,5.82873662113877,
33.9380381122945));
#57181=CARTESIAN_POINT('Ctrl Pts',(-5.1029491079964,2.8422533358967,34.0967988745404));
#57182=CARTESIAN_POINT('Ctrl Pts',(-5.15562461633369,-2.74554702011659,
34.2555596367863));
#57183=CARTESIAN_POINT('Ctrl Pts',(-0.489714995198005,-5.82053887949348,
34.4143203990321));
#57184=CARTESIAN_POINT('Ctrl Pts',(4.62439674808221,-3.56839576568293,34.573081161278));
#57185=CARTESIAN_POINT('Ctrl Pts',(5.50611933347969,1.94965215094856,34.7318419235239));
#57186=CARTESIAN_POINT('Ctrl Pts',(1.3484733182716,5.68331886613153,34.8906026857698));
#57187=CARTESIAN_POINT('Ctrl Pts',(-4.04333666747246,4.2154385557958,35.0493634480157));
#57188=CARTESIAN_POINT('Ctrl Pts',(-5.73456142981912,-1.11053988305151,
35.2081242102616));
#57189=CARTESIAN_POINT('Ctrl Pts',(-2.17734040713567,-5.42011829904768,
35.3668849725075));
#57190=CARTESIAN_POINT('Ctrl Pts',(3.37264906388706,-4.76903888808624,35.5256457347534));
#57191=CARTESIAN_POINT('Ctrl Pts',(5.83588709273329,0.246810585441287,35.6844064969993));
#57192=CARTESIAN_POINT('Ctrl Pts',(2.95794299481775,5.03677147224547,35.8431672592451));
#57193=CARTESIAN_POINT('Ctrl Pts',(-2.62720088350026,5.21692525746274,36.001928021491));
#57194=CARTESIAN_POINT('Ctrl Pts',(-5.80785026434291,0.622389693993225,
36.160688783737));
#57195=CARTESIAN_POINT('Ctrl Pts',(-3.67297768016272,-4.54177592855961,
36.3194495459828));
#57196=CARTESIAN_POINT('Ctrl Pts',(1.82351626946645,-5.54916949094261,36.4782103082287));
#57197=CARTESIAN_POINT('Ctrl Pts',(5.65107242925025,-1.47779363362579,36.6369710704746));
#57198=CARTESIAN_POINT('Ctrl Pts',(4.30659448752927,3.94610409697964,36.7957318327205));
#57199=CARTESIAN_POINT('Ctrl Pts',(-0.979410275819905,5.7584068227102,36.9544925949664));
#57200=CARTESIAN_POINT('Ctrl Pts',(-5.36902883826232,2.30043973146977,37.1132533572123));
#57201=CARTESIAN_POINT('Ctrl Pts',(-4.84474820880581,-3.26296006985836,
37.2720141194581));
#57202=CARTESIAN_POINT('Ctrl Pts',(0.113593966110691,-5.839999146839,37.4307748817041));
#57203=CARTESIAN_POINT('Ctrl Pts',(4.96797147346979,-3.07209261953597,37.5895356439499));
#57204=CARTESIAN_POINT('Ctrl Pts',(5.27550973964484,2.50748691145728,37.7482964061959));
#57205=CARTESIAN_POINT('Ctrl Pts',(0.754740349553719,5.79213782889985,37.9070571684417));
#57206=CARTESIAN_POINT('Ctrl Pts',(-4.4567904622931,3.77564728217961,38.0658179306876));
#57207=CARTESIAN_POINT('Ctrl Pts',(-5.58933050861204,-1.69643098583928,
38.2245786929334));
#57208=CARTESIAN_POINT('Ctrl Pts',(-1.60634454512588,-5.6158837974589,38.3833394551794));
#57209=CARTESIAN_POINT('Ctrl Pts',(3.84681701249253,-4.39550821823998,38.5421002174252));
#57210=CARTESIAN_POINT('Ctrl Pts',(5.77925413772213,0.847770744858901,38.7008609796712));
#57211=CARTESIAN_POINT('Ctrl Pts',(2.42234134649229,5.31514402676831,38.859621741917));
#57212=CARTESIAN_POINT('Ctrl Pts',(-3.15157223642715,4.91793514219116,39.018382504163));
#57213=CARTESIAN_POINT('Ctrl Pts',(-5.84107064254106,0.0196817951957224,
39.1771432664088));
#57214=CARTESIAN_POINT('Ctrl Pts',(-3.18464277877548,-4.89658493195106,
39.3359040286547));
#57215=CARTESIAN_POINT('Ctrl Pts',(2.38646743230569,-5.33134756124203,39.4946647909006));
#57216=CARTESIAN_POINT('Ctrl Pts',(5.77340975374383,-0.886698054352646,
39.6534255531465));
#57217=CARTESIAN_POINT('Ctrl Pts',(3.87635111745847,4.36948459642503,39.8121863153924));
#57218=CARTESIAN_POINT('Ctrl Pts',(-1.56846246621147,5.62658147690965,39.9709470776383));
#57219=CARTESIAN_POINT('Ctrl Pts',(-5.57777129149482,1.73405912355756,40.1297078398841));
#57220=CARTESIAN_POINT('Ctrl Pts',(-4.48213345555963,-3.74552710720003,
40.2884686021301));
#57221=CARTESIAN_POINT('Ctrl Pts',(0.7156898274528,-5.79709252083298,40.4472293643759));
#57222=CARTESIAN_POINT('Ctrl Pts',(5.25849191934999,-2.5429817849029,40.6059901266219));
#57223=CARTESIAN_POINT('Ctrl Pts',(4.98856158393098,3.03854355696032,40.7647508888677));
#57224=CARTESIAN_POINT('Ctrl Pts',(0.152947309300711,5.83910102197203,40.9235116511136));
#57225=CARTESIAN_POINT('Ctrl Pts',(-4.82264901463799,3.29553487401187,41.0822724133595));
#57226=CARTESIAN_POINT('Ctrl Pts',(-5.38440965064774,-2.26420545406742,
41.2410331756054));
#57227=CARTESIAN_POINT('Ctrl Pts',(-1.0181941054504,-5.75167578952804,41.3997939378513));
#57228=CARTESIAN_POINT('Ctrl Pts',(4.27990378619904,-3.97503675518808,41.5585547000972));
#57229=CARTESIAN_POINT('Ctrl Pts',(5.66090300135578,1.43967733657867,41.7173154623431));
#57230=CARTESIAN_POINT('Ctrl Pts',(1.86087087513805,5.53675475439179,41.8760762245889));
#57231=CARTESIAN_POINT('Ctrl Pts',(-3.64228711704701,4.56642509860946,42.0348369868349));
#57232=CARTESIAN_POINT('Ctrl Pts',(-5.81191268460203,-0.583236290691027,
42.1935977490807));
#57233=CARTESIAN_POINT('Ctrl Pts',(-2.66229823602482,-5.19910201156664,
42.3523585113267));
#57234=CARTESIAN_POINT('Ctrl Pts',(2.92393287912081,-5.05659076281771,42.5111192735725));
#57235=CARTESIAN_POINT('Ctrl Pts',(5.83409131060233,-0.286133192362046,
42.6698800358184));
#57236=CARTESIAN_POINT('Ctrl Pts',(3.4047111699812,4.74620221579552,42.8286407980643));
#57237=CARTESIAN_POINT('Ctrl Pts',(-2.14076463166355,5.43466838142269,42.9874015603102));
#57238=CARTESIAN_POINT('Ctrl Pts',(-5.72694725190272,1.1491600402646,43.1461623225561));
#57239=CARTESIAN_POINT('Ctrl Pts',(-4.07165281531897,-4.18809467129411,
43.3049230848019));
#57240=CARTESIAN_POINT('Ctrl Pts',(1.31014264809932,-5.69227721266703,43.4636838470478));
#57241=CARTESIAN_POINT('Ctrl Pts',(5.49285554114887,-1.98671377613569,43.6224446092938));
#57242=CARTESIAN_POINT('Ctrl Pts',(4.64833926148183,3.53715079327751,43.7812053715396));
#57243=CARTESIAN_POINT('Ctrl Pts',(-0.450479095664875,5.82370691300532,
43.9399661337855));
#57244=CARTESIAN_POINT('Ctrl Pts',(-5.13700522439592,2.78022857850681,44.0987268960314));
#57245=CARTESIAN_POINT('Ctrl Pts',(-5.12198725989218,-2.80779987422883,
44.2574876582773));
#57246=CARTESIAN_POINT('Ctrl Pts',(-0.419170101997096,-5.82604411670637,
44.4162484205232));
#57247=CARTESIAN_POINT('Ctrl Pts',(4.66728433696318,-3.51211482473953,44.575009182769));
#57248=CARTESIAN_POINT('Ctrl Pts',(5.48209758667841,2.01620923377307,44.733769945015));
#57249=CARTESIAN_POINT('Ctrl Pts',(1.27952767221442,5.69923701562366,44.8925307072609));
#57250=CARTESIAN_POINT('Ctrl Pts',(-4.09410505154189,4.16614899531406,45.0512914695068));
#57251=CARTESIAN_POINT('Ctrl Pts',(-5.72068777605988,-1.17992584218497,
45.2100522317526));
#57252=CARTESIAN_POINT('Ctrl Pts',(-2.11152230724456,-5.4460965076122,45.3688129939986));
#57253=CARTESIAN_POINT('Ctrl Pts',(3.43017287444968,-4.72783329608889,45.5275737562444));
#57254=CARTESIAN_POINT('Ctrl Pts',(5.83246906545287,0.317487361563403,45.6863345184903));
#57255=CARTESIAN_POINT('Ctrl Pts',(2.89671141266624,5.07223388813511,45.8450952807362));
#57256=CARTESIAN_POINT('Ctrl Pts',(-2.69020500619468,5.1847170268841,46.003856042982));
#57257=CARTESIAN_POINT('Ctrl Pts',(-5.8149636300044,0.551988773385138,46.162616805228));
#57258=CARTESIAN_POINT('Ctrl Pts',(-3.61768991925726,-4.58593646623255,
46.3213775674738));
#57259=CARTESIAN_POINT('Ctrl Pts',(1.89060410937151,-5.5266725727009,46.4801383297198));
#57260=CARTESIAN_POINT('Ctrl Pts',(5.66855950784905,-1.40922912622162,46.6388990919655));
#57261=CARTESIAN_POINT('Ctrl Pts',(4.25847609633845,3.99798386203986,46.7976598542116));
#57262=CARTESIAN_POINT('Ctrl Pts',(-1.04909471538713,5.74611989975528,46.9564206164574));
#57263=CARTESIAN_POINT('Ctrl Pts',(-5.39650199857509,2.23523148769702,47.1151813787033));
#57264=CARTESIAN_POINT('Ctrl Pts',(-4.80486581436728,-3.32140905793637,
47.2739421409491));
#57265=CARTESIAN_POINT('Ctrl Pts',(0.184330329686807,-5.83819457998573,
47.4327029031951));
#57266=CARTESIAN_POINT('Ctrl Pts',(5.00482172556827,-3.01168609245668,47.5914636654409));
#57267=CARTESIAN_POINT('Ctrl Pts',(5.24474740393951,2.5712095000382,47.7502244276869));
#57268=CARTESIAN_POINT('Ctrl Pts',(0.684520055329939,5.80085561948134,47.9089851899327));
#57269=CARTESIAN_POINT('Ctrl Pts',(-4.50220095685495,3.72138148653313,48.0677459521787));
#57270=CARTESIAN_POINT('Ctrl Pts',(-5.56837013180732,-1.76401465396777,
48.2265067144245));
#57271=CARTESIAN_POINT('Ctrl Pts',(-1.53819687404933,-5.63493070062818,
48.3852674766705));
#57272=CARTESIAN_POINT('Ctrl Pts',(3.89978114767392,-4.3485860488743,48.5440282389163));
#57273=CARTESIAN_POINT('Ctrl Pts',(5.76856034267981,0.917717384099773,48.7027890011622));
#57274=CARTESIAN_POINT('Ctrl Pts',(2.35777690909515,5.34409783510322,48.8615497634081));
#57275=CARTESIAN_POINT('Ctrl Pts',(-3.21091597092679,4.87939670982634,49.020310525654));
#57276=CARTESIAN_POINT('Ctrl Pts',(-5.84088047565118,-0.0510773273967016,
49.1790712878999));
#57277=CARTESIAN_POINT('Ctrl Pts',(-3.12509275704243,-4.93480383440904,
49.3378320501458));
#57278=CARTESIAN_POINT('Ctrl Pts',(2.45087531001271,-5.3020471366244,49.4965928123917));
#57279=CARTESIAN_POINT('Ctrl Pts',(5.78372743038313,-0.816694946262622,
49.6553535746376));
#57280=CARTESIAN_POINT('Ctrl Pts',(3.82313554021223,4.41612140519068,49.8141143368834));
#57281=CARTESIAN_POINT('Ctrl Pts',(-1.63650677555656,5.60716855442876,49.9728750991293));
#57282=CARTESIAN_POINT('Ctrl Pts',(-5.59836810258563,1.66636376946,50.1316358613752));
#57283=CARTESIAN_POINT('Ctrl Pts',(-4.43643193774801,-3.79954803706259,
50.2903966236211));
#57284=CARTESIAN_POINT('Ctrl Pts',(0.785862249094534,-5.78799742135959,
50.4491573858669));
#57285=CARTESIAN_POINT('Ctrl Pts',(5.28891130109086,-2.47909476894502,50.6079181481129));
#57286=CARTESIAN_POINT('Ctrl Pts',(4.95138717842959,3.0987511409437,50.7666789103587));
#57287=CARTESIAN_POINT('Ctrl Pts',(0.0822022679789686,5.84052535405474,
50.9254396726047));
#57288=CARTESIAN_POINT('Ctrl Pts',(-4.86221666902701,3.23687236196503,51.0842004348505));
#57289=CARTESIAN_POINT('Ctrl Pts',(-5.35658639219748,-2.32926508734879,
51.2429611970965));
#57290=CARTESIAN_POINT('Ctrl Pts',(-0.948444630167017,-5.76358798039247,
51.4017219593423));
#57291=CARTESIAN_POINT('Ctrl Pts',(4.32774262801073,-3.92289910269379,51.5604827215883));
#57292=CARTESIAN_POINT('Ctrl Pts',(5.64304764041327,1.50814686030353,51.7192434838341));
#57293=CARTESIAN_POINT('Ctrl Pts',(1.79366308317505,5.55889074980541,51.87800424608));
#57294=CARTESIAN_POINT('Ctrl Pts',(-3.69733671593728,4.52196802655651,52.0367650083259));
#57295=CARTESIAN_POINT('Ctrl Pts',(-5.80442101600325,-0.653597959908777,
52.1955257705718));
#57296=CARTESIAN_POINT('Ctrl Pts',(-2.59912190387458,-5.2309711290559,52.3542865328177));
#57297=CARTESIAN_POINT('Ctrl Pts',(2.98497296589237,-5.02079973879747,52.5130472950635));
#57298=CARTESIAN_POINT('Ctrl Pts',(5.83712940008821,-0.215439065266698,
52.6718080573094));
#57299=CARTESIAN_POINT('Ctrl Pts',(3.34696670988424,4.78709802146808,52.8305688195553));
#57300=CARTESIAN_POINT('Ctrl Pts',(-2.20644214763509,5.4083367751423,52.9893295818012));
#57301=CARTESIAN_POINT('Ctrl Pts',(-5.74044775498584,1.07970051240847,53.1480903440471));
#57302=CARTESIAN_POINT('Ctrl Pts',(-4.02062023271376,-4.2371106391632,53.306851106293));
#57303=CARTESIAN_POINT('Ctrl Pts',(1.37900173798208,-5.675988709543,53.4656118685389));
#57304=CARTESIAN_POINT('Ctrl Pts',(5.51651919592013,-1.92002853761645,53.6243726307848));
#57305=CARTESIAN_POINT('Ctrl Pts',(4.60514978147925,3.59320039997198,53.7831333930307));
#57306=CARTESIAN_POINT('Ctrl Pts',(-0.520993379103106,5.81782257577076,
53.9418941552766));
#57307=CARTESIAN_POINT('Ctrl Pts',(-5.1703074851803,2.71779582251969,54.1006549175224));
#57308=CARTESIAN_POINT('Ctrl Pts',(-5.08759825172204,-2.86964068365571,
54.2594156797684));
#57309=CARTESIAN_POINT('Ctrl Pts',(-0.348563695575712,-5.83069438183342,
54.4181764420142));
#57310=CARTESIAN_POINT('Ctrl Pts',(4.70948700177826,-3.45531848087826,54.5769372042601));
#57311=CARTESIAN_POINT('Ctrl Pts',(5.45727134195117,2.08247043785393,54.735697966506));
#57312=CARTESIAN_POINT('Ctrl Pts',(1.21039425544677,5.71431880197442,54.8944587287519));
#57313=CARTESIAN_POINT('Ctrl Pts',(-4.14427262561643,4.11624805238744,55.0532194909978));
#57314=CARTESIAN_POINT('Ctrl Pts',(-5.70597461125989,-1.24913864717843,
55.2119802532437));
#57315=CARTESIAN_POINT('Ctrl Pts',(-2.04539434141439,-5.47127550140978,
55.3707410154896));
#57316=CARTESIAN_POINT('Ctrl Pts',(3.48719330707719,-4.68593389446471,55.5295017777355));
#57317=CARTESIAN_POINT('Ctrl Pts',(5.82819512322526,0.388117546408988,55.6882625399813));
#57318=CARTESIAN_POINT('Ctrl Pts',(2.83505473805949,5.10695195360438,55.8470233022273));
#57319=CARTESIAN_POINT('Ctrl Pts',(-2.75281434125286,5.15174793898243,56.0057840644731));
#57320=CARTESIAN_POINT('Ctrl Pts',(-5.82122364964165,0.481506848414017,
56.1645448267191));
#57321=CARTESIAN_POINT('Ctrl Pts',(-3.56187126228685,-4.6294240176411,56.3233055889649));
#57322=CARTESIAN_POINT('Ctrl Pts',(1.95741450308725,-5.50336461515325,56.4820663512108));
#57323=CARTESIAN_POINT('Ctrl Pts',(5.6852147252314,-1.34045781441613,56.6408271134567));
#57324=CARTESIAN_POINT('Ctrl Pts',(4.20973277369882,4.0492769228917,56.7995878757026));
#57325=CARTESIAN_POINT('Ctrl Pts',(-1.11862520028478,5.73298973359492,56.9583486379484));
#57326=CARTESIAN_POINT('Ctrl Pts',(-5.42318322211612,2.16969522366057,57.1171094001944));
#57327=CARTESIAN_POINT('Ctrl Pts',(-4.76427830577834,-3.3793706291715,57.2758701624402));
#57328=CARTESIAN_POINT('Ctrl Pts',(0.255039642783455,-5.83553325796587,
57.4346309246862));
#57329=CARTESIAN_POINT('Ctrl Pts',(5.04093751998252,-2.95083760038564,57.593391686932));
#57330=CARTESIAN_POINT('Ctrl Pts',(5.21321540145215,2.63455476357568,57.7521524491779));
#57331=CARTESIAN_POINT('Ctrl Pts',(0.614199307774883,5.80872213438946,57.9109132114238));
#57332=CARTESIAN_POINT('Ctrl Pts',(-4.54695075334007,3.66656957808212,58.0696739736697));
#57333=CARTESIAN_POINT('Ctrl Pts',(-5.54659259657899,-1.83133945291199,
58.2284347359156));
#57334=CARTESIAN_POINT('Ctrl Pts',(-1.469823472552,-5.65315067760911,58.3871954981615));
#57335=CARTESIAN_POINT('Ctrl Pts',(3.95217298989717,-4.30102572442254,58.5459562604074));
#57336=CARTESIAN_POINT('Ctrl Pts',(5.75702001129657,0.987529348296885,58.7047170226532));
#57337=CARTESIAN_POINT('Ctrl Pts',(2.29286646789146,5.37226739697831,58.8634777848992));
#57338=CARTESIAN_POINT('Ctrl Pts',(-3.26978850344612,4.84014222590088,59.022238547145));
#57339=CARTESIAN_POINT('Ctrl Pts',(-5.83983315943952,-0.121828954390395,
59.180999309391));
#57340=CARTESIAN_POINT('Ctrl Pts',(-3.06508412788734,-4.97229855430969,
59.3397600716368));
#57341=CARTESIAN_POINT('Ctrl Pts',(2.51492352172104,-5.27196863648781,59.4985208338828));
#57342=CARTESIAN_POINT('Ctrl Pts',(5.79319634491114,-0.746571988173542,
59.6572815961285));
#57343=CARTESIAN_POINT('Ctrl Pts',(3.76935891775212,4.46211014805548,59.8160423583745));
#57344=CARTESIAN_POINT('Ctrl Pts',(-1.70431092750091,5.58693277985496,59.9748031206203));
#57345=CARTESIAN_POINT('Ctrl Pts',(-5.61814335305001,1.59842387644741,60.1335638828663));
#57346=CARTESIAN_POINT('Ctrl Pts',(-4.39007937346456,-3.85301138317786,
60.2923246451121));
#57347=CARTESIAN_POINT('Ctrl Pts',(0.85591934543619,-5.77805293315363,60.451085407358));
#57348=CARTESIAN_POINT('Ctrl Pts',(5.31855453499689,-2.41484394578226,60.609846169604));
#57349=CARTESIAN_POINT('Ctrl Pts',(4.91348615676483,3.15850398313777,60.7686069318498));
#57350=CARTESIAN_POINT('Ctrl Pts',(0.0114451634727917,5.84109258892977,
60.9273676940957));
#57351=CARTESIAN_POINT('Ctrl Pts',(-4.90107079302665,3.17773483883697,61.0861284563416));
#57352=CARTESIAN_POINT('Ctrl Pts',(-5.32797705459145,-2.3939829009339,61.2448892185875));
#57353=CARTESIAN_POINT('Ctrl Pts',(-0.878555970616003,-5.77465436461024,
61.4036499808334));
#57354=CARTESIAN_POINT('Ctrl Pts',(4.37494637350877,-3.87018576468102,61.5624107430792));
#57355=CARTESIAN_POINT('Ctrl Pts',(5.62436416212133,1.57639506344776,61.7211715053253));
#57356=CARTESIAN_POINT('Ctrl Pts',(1.72619207112014,5.58021097789493,61.879932267571));
#57357=CARTESIAN_POINT('Ctrl Pts',(-3.75184373059352,4.47684735560896,62.038693029817));
#57358=CARTESIAN_POINT('Ctrl Pts',(-5.79607754850909,-0.723863713613315,
62.1974537920628));
#57359=CARTESIAN_POINT('Ctrl Pts',(-2.53556415053518,-5.26207260143168,
62.3562145543087));
#57360=CARTESIAN_POINT('Ctrl Pts',(3.04557500782399,-4.9842719123193,62.5149753165546));
#57361=CARTESIAN_POINT('Ctrl Pts',(5.8393108907227,-0.144713322484355,62.6737360788005));
#57362=CARTESIAN_POINT('Ctrl Pts',(3.28873108235841,4.82729132041423,62.8324968410464));
#57363=CARTESIAN_POINT('Ctrl Pts',(-2.27179586817918,5.38121149533645,62.9912576032922));
#57364=CARTESIAN_POINT('Ctrl Pts',(-5.75310584725087,1.01008253848138,63.1500183655383));
#57365=CARTESIAN_POINT('Ctrl Pts',(-3.96899762401232,-4.28550481096468,
63.3087791277839));
#57366=CARTESIAN_POINT('Ctrl Pts',(1.44765845933327,-5.65886725496703,63.4675398900301));
#57367=CARTESIAN_POINT('Ctrl Pts',(5.53937330139366,-1.85306153487257,63.6263006522757));
#57368=CARTESIAN_POINT('Ctrl Pts',(4.56128449565793,3.64872270443888,63.7850614145219));
#57369=CARTESIAN_POINT('Ctrl Pts',(-0.591431206752995,5.81108447296164,
63.9438221767675));
#57370=CARTESIAN_POINT('Ctrl Pts',(-5.20285100324211,2.65496422994348,64.1025829390136));
#57371=CARTESIAN_POINT('Ctrl Pts',(-5.05246263841092,-2.93106037325727,
64.2613437012593));
#57372=CARTESIAN_POINT('Ctrl Pts',(-0.277906137425253,-5.83448899244814,
64.4201044635054));
#57373=CARTESIAN_POINT('Ctrl Pts',(4.75099854928546,-3.3980150689637,64.5788652257511));
#57374=CARTESIAN_POINT('Ctrl Pts',(5.4316442425499,2.14842603935805,64.7376259879971));
#57375=CARTESIAN_POINT('Ctrl Pts',(1.14108321329899,5.72856201193147,64.896386750243));
#57376=CARTESIAN_POINT('Ctrl Pts',(-4.19383202760378,4.06574304998017,65.0551475124888));
#57377=CARTESIAN_POINT('Ctrl Pts',(-5.69042409457625,-1.31816814105151,
65.2139082747347));
#57378=CARTESIAN_POINT('Ctrl Pts',(-1.97896621392534,-5.49565158542271,
65.3726690369806));
#57379=CARTESIAN_POINT('Ctrl Pts',(3.54370199402013,-4.6433468319516,65.5314297992266));
#57380=CARTESIAN_POINT('Ctrl Pts',(5.82306589325152,0.458690774997357,65.6901905614723));
#57381=CARTESIAN_POINT('Ctrl Pts',(2.77298201911554,5.14092057377652,65.8489513237183));
#57382=CARTESIAN_POINT('Ctrl Pts',(-2.8150197007537,5.11802283197194,66.0077120859641));
#57383=CARTESIAN_POINT('Ctrl Pts',(-5.8266294045968,0.410954262303533,66.1664728482102));
#57384=CARTESIAN_POINT('Ctrl Pts',(-3.50552990064023,-4.67223220098639,
66.3252336104559));
#57385=CARTESIAN_POINT('Ctrl Pts',(2.0239376461872,-5.47924903874272,66.483994372702));
#57386=CARTESIAN_POINT('Ctrl Pts',(5.70103563724385,-1.27148979040063,66.6427551349476));
#57387=CARTESIAN_POINT('Ctrl Pts',(4.16037167269387,4.09997575227756,66.8015158971937));
#57388=CARTESIAN_POINT('Ctrl Pts',(-1.18799152691301,5.71901825108119,66.9602766594395));
#57389=CARTESIAN_POINT('Ctrl Pts',(-5.44906859341531,2.10384055680833,67.1190374216854));
#57390=CARTESIAN_POINT('Ctrl Pts',(-4.72299163925665,-3.43683627770202,
67.2777981839313));
#57391=CARTESIAN_POINT('Ctrl Pts',(0.325711528807802,-5.8320155713286,67.4365589461772));
#57392=CARTESIAN_POINT('Ctrl Pts',(5.07631355671921,-2.88955607283996,67.5953197084231));
#57393=CARTESIAN_POINT('Ctrl Pts',(5.18091835950451,2.6975134061513,67.754080470669));
#57394=CARTESIAN_POINT('Ctrl Pts',(0.54378842645952,5.81573621921296,67.9128412329148));
#57395=CARTESIAN_POINT('Ctrl Pts',(-4.59103328471497,3.61121960047518,68.0716019951608));
#57396=CARTESIAN_POINT('Ctrl Pts',(-5.52400109878079,-1.8983955027565,68.2303627574066));
#57397=CARTESIAN_POINT('Ctrl Pts',(-1.40123437443171,-5.67054105461978,
68.3891235196526));
#57398=CARTESIAN_POINT('Ctrl Pts',(4.00398485065851,-4.2528342243631,68.5478842818984));
#57399=CARTESIAN_POINT('Ctrl Pts',(5.74463483711628,1.05719639254342,68.7066450441444));
#57400=CARTESIAN_POINT('Ctrl Pts',(2.22761954848948,5.39964857850993,68.8654058063901));
#57401=CARTESIAN_POINT('Ctrl Pts',(-3.32818119444006,4.80017745101086,69.0241665686361));
#57402=CARTESIAN_POINT('Ctrl Pts',(-5.83792884759976,-0.192562702982879,
69.182927330882));
#57403=CARTESIAN_POINT('Ctrl Pts',(-3.00462569757752,-5.00906358930226,
69.3416880931278));
#57404=CARTESIAN_POINT('Ctrl Pts',(2.57860266835449,-5.24111647485266,69.5004488553739));
#57405=CARTESIAN_POINT('Ctrl Pts',(5.80181510776444,-0.676339470630766,
69.6592096176196));
#57406=CARTESIAN_POINT('Ctrl Pts',(3.71502914179852,4.50744407617051,69.8179703798656));
#57407=CARTESIAN_POINT('Ctrl Pts',(-1.77186497178415,5.56587712278864,69.9767311421114));
#57408=CARTESIAN_POINT('Ctrl Pts',(-5.63709414086971,1.53024941470006,70.1354919043573));
#57409=CARTESIAN_POINT('Ctrl Pts',(-4.34308256494864,-3.90590929979895,
70.2942526666033));
#57410=CARTESIAN_POINT('Ctrl Pts',(0.925850835597592,-5.7672605155689,70.453013428849));
#57411=CARTESIAN_POINT('Ctrl Pts',(5.34741727092293,-2.35023874422409,70.6117741910951));
#57412=CARTESIAN_POINT('Ctrl Pts',(4.87486408091236,3.21779331481187,70.7705349533408));
#57413=CARTESIAN_POINT('Ctrl Pts',(-0.0593136206115266,5.8408026433554,
70.9292957155867));
#57414=CARTESIAN_POINT('Ctrl Pts',(-4.93920568479356,3.11813098306019,71.0880564778327));
#57415=CARTESIAN_POINT('Ctrl Pts',(-5.29858583625043,-2.45834939748262,
71.2468172400784));
#57416=CARTESIAN_POINT('Ctrl Pts',(-0.808538382959287,-5.78487331818929,
71.4055780023245));
#57417=CARTESIAN_POINT('Ctrl Pts',(4.42150809554277,-3.81690447683292,71.5643387645703));
#57418=CARTESIAN_POINT('Ctrl Pts',(5.60485530828073,1.64441193058638,71.7230995268162));
#57419=CARTESIAN_POINT('Ctrl Pts',(1.65846774034549,5.6007123099165,71.8818602890621));
#57420=CARTESIAN_POINT('Ctrl Pts',(-3.80580016211055,4.43106970722601,72.040621051308));
#57421=CARTESIAN_POINT('Ctrl Pts',(-5.78688350652351,-0.794023240304163,
72.1993818135539));
#57422=CARTESIAN_POINT('Ctrl Pts',(-2.47163430310789,-5.29240186455242,
72.3581425757998));
#57423=CARTESIAN_POINT('Ctrl Pts',(3.10573011156498,-4.94701264384235,72.5169033380457));
#57424=CARTESIAN_POINT('Ctrl Pts',(5.84063546237199,-0.0739663430189528,
72.6756641002916));
#57425=CARTESIAN_POINT('Ctrl Pts',(3.23001283348305,4.86677621426665,72.8344248625374));
#57426=CARTESIAN_POINT('Ctrl Pts',(-2.33681620263615,5.35329652264041,72.9931856247833));
#57427=CARTESIAN_POINT('Ctrl Pts',(-5.76491967112249,0.940316334922364,
73.1519463870293));
#57428=CARTESIAN_POINT('Ctrl Pts',(-3.9167925648334,-4.33327008485316,73.3107071492751));
#57429=CARTESIAN_POINT('Ctrl Pts',(1.51610273677804,-5.64091536151285,73.469467911521));
#57430=CARTESIAN_POINT('Ctrl Pts',(5.56141450372903,-1.78582259531264,73.6282286737669));
#57431=CARTESIAN_POINT('Ctrl Pts',(4.51674984124932,3.70370955877901,73.7869894360128));
#57432=CARTESIAN_POINT('Ctrl Pts',(-0.661782241861996,5.80349359339467,
73.9457501982587));
#57433=CARTESIAN_POINT('Ctrl Pts',(-5.23463100281954,2.59174302131558,74.1045109605046));
#57434=CARTESIAN_POINT('Ctrl Pts',(-5.01658557611066,-2.99204992969303,
74.2632717227504));
#57435=CARTESIAN_POINT('Ctrl Pts',(-0.207207796543587,-5.83742739169134,
74.4220324849964));
#57436=CARTESIAN_POINT('Ctrl Pts',(4.79181288766461,-3.34021299827244,74.5807932472422));
#57437=CARTESIAN_POINT('Ctrl Pts',(5.4052200492518,2.21406635929985,74.7395540094881));
#57438=CARTESIAN_POINT('Ctrl Pts',(1.07160471716756,5.7419645553035,74.8983147717341));
#57439=CARTESIAN_POINT('Ctrl Pts',(-4.2427759846608,4.01464139970224,75.0570755339798));
#57440=CARTESIAN_POINT('Ctrl Pts',(-5.67403850804756,-1.38700419372482,
75.2158362962259));
#57441=CARTESIAN_POINT('Ctrl Pts',(-1.91224767310636,-5.51922118246009,
75.3745970584716));
#57442=CARTESIAN_POINT('Ctrl Pts',(3.59969064262747,-4.60007835820185,75.5333578207176));
#57443=CARTESIAN_POINT('Ctrl Pts',(5.81708212824635,0.529196690705634,75.6921185829634));
#57444=CARTESIAN_POINT('Ctrl Pts',(2.71050236500702,5.17413476375605,75.8508793452094));
#57445=CARTESIAN_POINT('Ctrl Pts',(-2.87681195605961,5.08354665501262,76.0096401074552));
#57446=CARTESIAN_POINT('Ctrl Pts',(-5.83118010157501,0.340341368647152,
76.1684008697012));
#57447=CARTESIAN_POINT('Ctrl Pts',(-3.4486741024136,-4.71435473416655,76.327161631947));
#57448=CARTESIAN_POINT('Ctrl Pts',(2.09016377639872,-5.45432938243075,76.4859223941929));
#57449=CARTESIAN_POINT('Ctrl Pts',(5.71601992216721,-1.20233517523405,76.6446831564388));
#57450=CARTESIAN_POINT('Ctrl Pts',(4.11040003706624,4.15007291014307,76.8034439186847));
#57451=CARTESIAN_POINT('Ctrl Pts',(-1.25718351576172,5.7042075025295,76.9622046809306));
#57452=CARTESIAN_POINT('Ctrl Pts',(-5.47415431379396,2.03767715131415,77.1209654431764));
#57453=CARTESIAN_POINT('Ctrl Pts',(-4.68101187362137,-3.49379757044288,
77.2797262054223));
#57454=CARTESIAN_POINT('Ctrl Pts',(0.39633561665894,-5.82764203629436,77.4384869676682));
#57455=CARTESIAN_POINT('Ctrl Pts',(5.11094464434401,-2.82785050288533,77.5972477299141));
#57456=CARTESIAN_POINT('Ctrl Pts',(5.1478610176884,2.76007618858267,77.75600849216));
#57457=CARTESIAN_POINT('Ctrl Pts',(0.473297744182263,5.82189684463481,77.9147692544059));
#57458=CARTESIAN_POINT('Ctrl Pts',(-4.63444208186731,3.55533967632268,78.0735300166519));
#57459=CARTESIAN_POINT('Ctrl Pts',(-5.50059895371541,-1.96517296302448,
78.2322907788976));
#57460=CARTESIAN_POINT('Ctrl Pts',(-1.33243964514028,-5.6870992796219,78.3910515411437));
#57461=CARTESIAN_POINT('Ctrl Pts',(4.0552091265661,-4.20401862079985,78.5498123033894));
#57462=CARTESIAN_POINT('Ctrl Pts',(5.73140663766353,1.12670829319891,78.7085730656353));
#57463=CARTESIAN_POINT('Ctrl Pts',(2.16204572587615,5.42623736150913,78.8673338278812));
#57464=CARTESIAN_POINT('Ctrl Pts',(-3.38608547477963,4.75950824998793,79.0260945901272));
#57465=CARTESIAN_POINT('Ctrl Pts',(-5.83516781958967,-0.263268192994679,
79.184855352373));
#57466=CARTESIAN_POINT('Ctrl Pts',(-2.94372633838929,-5.04509354411697,
79.3436161146189));
#57467=CARTESIAN_POINT('Ctrl Pts',(2.64190340499678,-5.2094951792744,79.5023768768649));
#57468=CARTESIAN_POINT('Ctrl Pts',(5.80958245413942,-0.606007700257848,
79.6611376391106));
#57469=CARTESIAN_POINT('Ctrl Pts',(3.66015418524723,4.55211653678098,79.8198984013567));
#57470=CARTESIAN_POINT('Ctrl Pts',(-1.8391589948488,5.54400467314773,79.9786591636023));
#57471=CARTESIAN_POINT('Ctrl Pts',(-5.65521768501588,1.46185038882208,80.1374199258485));
#57472=CARTESIAN_POINT('Ctrl Pts',(-4.29544840898361,-3.95823402415551,
80.2961806880941));
#57473=CARTESIAN_POINT('Ctrl Pts',(0.995646457131763,-5.7556217523925,80.4549414503402));
#57474=CARTESIAN_POINT('Ctrl Pts',(5.3754952732605,-2.28528864508612,80.613702212586));
#57475=CARTESIAN_POINT('Ctrl Pts',(4.83552661866532,3.27661043525698,80.7724629748319));
#57476=CARTESIAN_POINT('Ctrl Pts',(-0.130063700425983,5.83965555987772,
80.9312237370779));
#57477=CARTESIAN_POINT('Ctrl Pts',(-4.9766157480213,3.05806954150856,81.0899844993236));
#57478=CARTESIAN_POINT('Ctrl Pts',(-5.26841705035579,-2.52235513122241,
81.2487452615697));
#57479=CARTESIAN_POINT('Ctrl Pts',(-0.738402142242399,-5.79424334147416,
81.4075060238153));
#57480=CARTESIAN_POINT('Ctrl Pts',(4.46742096110774,-3.76306305822547,81.5662667860616));
#57481=CARTESIAN_POINT('Ctrl Pts',(5.58452394195224,1.71218748032981,81.7250275483071));
#57482=CARTESIAN_POINT('Ctrl Pts',(1.590500029138,5.62039173713168,81.8837883105533));
#57483=CARTESIAN_POINT('Ctrl Pts',(-3.85919809188181,4.38464179959952,82.0425490727989));
#57484=CARTESIAN_POINT('Ctrl Pts',(-5.776840240228,-0.864066244683674,82.201309835045));
#57485=CARTESIAN_POINT('Ctrl Pts',(-2.40734174146917,-5.3219544664209,82.3600705972908));
#57486=CARTESIAN_POINT('Ctrl Pts',(3.16542944584671,-4.9090274034195,82.5188313595367));
#57487=CARTESIAN_POINT('Ctrl Pts',(5.84110292736961,-0.00320850467390637,
82.6775921217826));
#57488=CARTESIAN_POINT('Ctrl Pts',(3.1708205673024,4.90554690034638,82.8363528840285));
#57489=CARTESIAN_POINT('Ctrl Pts',(-2.40149358463894,5.32459596941663,82.9951136462743));
#57490=CARTESIAN_POINT('Ctrl Pts',(-5.7758875400995,0.870412109585264,83.1538744085203));
#57491=CARTESIAN_POINT('Ctrl Pts',(-3.86401262590961,-4.3803993931662,83.3126351707661));
#57492=CARTESIAN_POINT('Ctrl Pts',(1.58432435304567,-5.62213577491609,83.4713959330121));
#57493=CARTESIAN_POINT('Ctrl Pts',(5.58263989986849,-1.71832137308609,83.6301566952579));
#57494=CARTESIAN_POINT('Ctrl Pts',(4.47155171880276,3.75815248538495,83.7889174575037));
#57495=CARTESIAN_POINT('Ctrl Pts',(-0.732034944345687,5.79505183303421,
83.9476782197497));
#57496=CARTESIAN_POINT('Ctrl Pts',(-5.26564514937354,2.52813997655405,84.1064389819955));
#57497=CARTESIAN_POINT('Ctrl Pts',(-4.97996786863125,-3.05259753396621,
84.2651997442416));
#57498=CARTESIAN_POINT('Ctrl Pts',(-0.136487592502867,-5.83951464301881,
84.4239605064873));
#57499=CARTESIAN_POINT('Ctrl Pts',(4.83194039314673,-3.28191022714265,84.5827212687333));
#57500=CARTESIAN_POINT('Ctrl Pts',(5.3779712939643,2.27936160776507,84.7414820309791));
#57501=CARTESIAN_POINT('Ctrl Pts',(1.00202900079473,5.75456307304708,84.9002427932251));
#57502=CARTESIAN_POINT('Ctrl Pts',(-4.29121230689459,3.96287665367137,85.059003555471));
#57503=CARTESIAN_POINT('Ctrl Pts',(-5.65660000441566,-1.45549506770408,
85.2177643177168));
#57504=CARTESIAN_POINT('Ctrl Pts',(-1.84567038925739,-5.54225213649743,
85.3765250799627));
#57505=CARTESIAN_POINT('Ctrl Pts',(3.65595928985271,-4.55561497937659,85.5352858422086));
#57506=CARTESIAN_POINT('Ctrl Pts',(5.8086947012646,0.598627392648328,85.6940466044544));
#57507=CARTESIAN_POINT('Ctrl Pts',(2.65061116100751,5.20851728785982,85.8528073667005));
#57508=CARTESIAN_POINT('Ctrl Pts',(-2.94405900471206,5.04447882807405,86.0115681289463));
#57509=CARTESIAN_POINT('Ctrl Pts',(-5.34253328840157,1.07278402652743,86.1438687641512));
#57510=CARTESIAN_POINT('Ctrl Pts',(-4.62260421807956,-2.25450493511227,
86.2497092723151));
#57511=CARTESIAN_POINT('Ctrl Pts',(-3.53826020855044,-3.54670961616112,
86.3026295263971));
#57512=CARTESIAN_POINT('Ctrl Pts',(-2.86929757049814,-4.02374147429149,
86.3290896534381));
#57513=CARTESIAN_POINT('',(-2.16917135428524,4.44050218283342,86.));
#57514=CARTESIAN_POINT('Ctrl Pts',(-2.17574227734826,4.44486702454923,86.));
#57515=CARTESIAN_POINT('Ctrl Pts',(-2.28013295862628,4.38716599510334,86.));
#57516=CARTESIAN_POINT('Ctrl Pts',(-2.38203491056673,4.32558764363711,86.));
#57517=CARTESIAN_POINT('Ctrl Pts',(-2.48120820121107,4.26013722079047,86.));
#57518=CARTESIAN_POINT('Ctrl Pts',(-2.60006688906204,4.18169521963978,86.));
#57519=CARTESIAN_POINT('Ctrl Pts',(-2.7150074127347,4.09769239705542,86.));
#57520=CARTESIAN_POINT('Ctrl Pts',(-2.825877147636,4.00855468944723,86.));
#57521=CARTESIAN_POINT('Ctrl Pts',(-2.93875239431318,3.9178045785764,86.));
#57522=CARTESIAN_POINT('Ctrl Pts',(-3.04740870522866,3.82173148785291,86.));
#57523=CARTESIAN_POINT('Ctrl Pts',(-3.15164741290182,3.72074618418362,86.));
#57524=CARTESIAN_POINT('Ctrl Pts',(-3.25648521909179,3.61918048051708,86.));
#57525=CARTESIAN_POINT('Ctrl Pts',(-3.35685490813916,3.51264518527105,86.));
#57526=CARTESIAN_POINT('Ctrl Pts',(-3.45251018852357,3.40153010769327,86.));
#57527=CARTESIAN_POINT('Ctrl Pts',(-3.48145067837577,3.36791225866138,86.));
#57528=CARTESIAN_POINT('Ctrl Pts',(-3.50995929996644,3.33387504208837,86.));
#57529=CARTESIAN_POINT('Ctrl Pts',(-3.53802835306874,3.2994289123823,86.));
#57530=CARTESIAN_POINT('Ctrl Pts',(-3.55893895860226,3.27376757539972,86.));
#57531=CARTESIAN_POINT('Ctrl Pts',(-3.57960560368256,3.24787929661303,86.));
#57532=CARTESIAN_POINT('Ctrl Pts',(-3.60002494885949,3.22176835839145,86.));
#57533=CARTESIAN_POINT('Ctrl Pts',(-3.61193639941707,3.20653676565705,86.));
#57534=CARTESIAN_POINT('Ctrl Pts',(-3.62375830311465,3.19123627397227,86.));
#57535=CARTESIAN_POINT('Ctrl Pts',(-3.63548790188773,3.17587102356872,86.));
#57536=CARTESIAN_POINT('Ctrl Pts',(-3.72304104356389,3.06118031918079,86.));
#57537=CARTESIAN_POINT('Ctrl Pts',(-3.80549810494951,2.94282892853622,86.));
#57538=CARTESIAN_POINT('Ctrl Pts',(-3.88269282098784,2.82123575460696,86.));
#57539=CARTESIAN_POINT('Ctrl Pts',(-3.96010237178875,2.69930418393253,86.));
#57540=CARTESIAN_POINT('Ctrl Pts',(-4.03222060518193,2.57411198603205,86.));
#57541=CARTESIAN_POINT('Ctrl Pts',(-4.09883515477919,2.44605409339683,86.));
#57542=CARTESIAN_POINT('Ctrl Pts',(-4.16485320331115,2.31914289723916,86.));
#57543=CARTESIAN_POINT('Ctrl Pts',(-4.2254659552961,2.18941632853557,86.));
#57544=CARTESIAN_POINT('Ctrl Pts',(-4.28041834739517,2.05724343991072,86.));
#57545=CARTESIAN_POINT('Ctrl Pts',(-4.33438117280193,1.92745068221766,86.));
#57546=CARTESIAN_POINT('Ctrl Pts',(-4.38288583069982,1.79529822126205,86.));
#57547=CARTESIAN_POINT('Ctrl Pts',(-4.42564090526442,1.66113144401598,86.));
#57548=CARTESIAN_POINT('Ctrl Pts',(-4.43255967958786,1.63942011119941,86.));
#57549=CARTESIAN_POINT('Ctrl Pts',(-4.43932777954855,1.61765603376178,86.));
#57550=CARTESIAN_POINT('Ctrl Pts',(-4.4459438397712,1.59584068384471,86.));
#57551=CARTESIAN_POINT('Ctrl Pts',(-4.45171251084707,1.57681945764039,86.));
#57552=CARTESIAN_POINT('Ctrl Pts',(-4.45736585345657,1.55775815091916,86.));
#57553=CARTESIAN_POINT('Ctrl Pts',(-4.46289825998277,1.53867450299572,86.));
#57554=CARTESIAN_POINT('Ctrl Pts',(-4.50224730205451,1.40294274476988,86.));
#57555=CARTESIAN_POINT('Ctrl Pts',(-4.53554254717084,1.2658880814313,86.));
#57556=CARTESIAN_POINT('Ctrl Pts',(-4.56258502829437,1.12787819891714,86.));
#57557=CARTESIAN_POINT('Ctrl Pts',(-4.58931759393923,0.991449953775849,
86.));
#57558=CARTESIAN_POINT('Ctrl Pts',(-4.60994008626122,0.854087541637941,
86.));
#57559=CARTESIAN_POINT('Ctrl Pts',(-4.62421031200347,0.716138535076822,
86.));
#57560=CARTESIAN_POINT('Ctrl Pts',(-4.63813932416541,0.581488009932714,
86.));
#57561=CARTESIAN_POINT('Ctrl Pts',(-4.64601628194546,0.446277995360083,
86.));
#57562=CARTESIAN_POINT('Ctrl Pts',(-4.64756630557454,0.310834136529796,
86.));
#57563=CARTESIAN_POINT('Ctrl Pts',(-4.64793240287716,0.278843894287929,
86.));
#57564=CARTESIAN_POINT('Ctrl Pts',(-4.6479453277195,0.246840640295154,86.));
#57565=CARTESIAN_POINT('Ctrl Pts',(-4.64760103388387,0.214828741346587,
86.));
#57566=CARTESIAN_POINT('Ctrl Pts',(-4.64657805635091,0.119713900408526,
86.));
#57567=CARTESIAN_POINT('Ctrl Pts',(-4.64240219271064,0.0245223992060761,
86.));
#57568=CARTESIAN_POINT('Ctrl Pts',(-4.63512171526216,-0.0706009649893001,
86.));
#57569=CARTESIAN_POINT('Ctrl Pts',(-4.63272301775774,-0.101941241491998,
86.));
#57570=CARTESIAN_POINT('Ctrl Pts',(-4.62998723239254,-0.133274083991166,
86.));
#57571=CARTESIAN_POINT('Ctrl Pts',(-4.62691585213729,-0.16459419159554,
86.));
#57572=CARTESIAN_POINT('Ctrl Pts',(-4.62511596030474,-0.182948417118559,
86.));
#57573=CARTESIAN_POINT('Ctrl Pts',(-4.62320081633973,-0.201298267969776,
86.));
#57574=CARTESIAN_POINT('Ctrl Pts',(-4.62117070299388,-0.21964266601306,
86.));
#57575=CARTESIAN_POINT('Ctrl Pts',(-4.61910605502354,-0.238299123921961,
86.));
#57576=CARTESIAN_POINT('Ctrl Pts',(-4.6169235721841,-0.256940116225532,
86.));
#57577=CARTESIAN_POINT('Ctrl Pts',(-4.61462417515337,-0.275562596752177,
86.));
#57578=CARTESIAN_POINT('Ctrl Pts',(-4.59791089402231,-0.410921018216574,
86.));
#57579=CARTESIAN_POINT('Ctrl Pts',(-4.57502130177171,-0.545336418557933,
86.));
#57580=CARTESIAN_POINT('Ctrl Pts',(-4.54619383694625,-0.678403869974182,
86.));
#57581=CARTESIAN_POINT('Ctrl Pts',(-4.51690235263596,-0.81361323330078,
86.));
#57582=CARTESIAN_POINT('Ctrl Pts',(-4.48148002405017,-0.947431726142265,
86.));
#57583=CARTESIAN_POINT('Ctrl Pts',(-4.44012512005541,-1.07942238906511,
86.));
#57584=CARTESIAN_POINT('Ctrl Pts',(-4.39891579514076,-1.21094841351862,
86.));
#57585=CARTESIAN_POINT('Ctrl Pts',(-4.35181516564808,-1.34066022876501,
86.));
#57586=CARTESIAN_POINT('Ctrl Pts',(-4.29897383984103,-1.46810153698611,
86.));
#57587=CARTESIAN_POINT('Ctrl Pts',(-4.26316764637209,-1.55445796480857,
86.));
#57588=CARTESIAN_POINT('Ctrl Pts',(-4.22472458946287,-1.639771352916,86.));
#57589=CARTESIAN_POINT('Ctrl Pts',(-4.18368102987994,-1.72389071907676,
86.));
#57590=CARTESIAN_POINT('Ctrl Pts',(-4.16189573536735,-1.76853999376555,
86.));
#57591=CARTESIAN_POINT('Ctrl Pts',(-4.13937765883534,-1.81285273679093,
86.));
#57592=CARTESIAN_POINT('Ctrl Pts',(-4.11613135978827,-1.85680534418916,
86.));
#57593=CARTESIAN_POINT('Ctrl Pts',(-4.10598652796122,-1.87598653985015,
86.));
#57594=CARTESIAN_POINT('Ctrl Pts',(-4.09570182816448,-1.8951012704791,86.));
#57595=CARTESIAN_POINT('Ctrl Pts',(-4.08528136703263,-1.91414066944428,
86.));
#57596=CARTESIAN_POINT('Ctrl Pts',(-4.07459370444932,-1.93366827665418,
86.));
#57597=CARTESIAN_POINT('Ctrl Pts',(-4.06376686324371,-1.95311008122927,
86.));
#57598=CARTESIAN_POINT('Ctrl Pts',(-4.05280165642382,-1.97246424292779,
86.));
#57599=CARTESIAN_POINT('Ctrl Pts',(-3.98545341209713,-2.09133740530588,
86.));
#57600=CARTESIAN_POINT('Ctrl Pts',(-3.91288886269624,-2.20690686036164,
86.));
#57601=CARTESIAN_POINT('Ctrl Pts',(-3.83535609314517,-2.31888838615919,
86.));
#57602=CARTESIAN_POINT('Ctrl Pts',(-3.75793727989042,-2.43070532348649,
86.));
#57603=CARTESIAN_POINT('Ctrl Pts',(-3.67556431499777,-2.53894540267671,
86.));
#57604=CARTESIAN_POINT('Ctrl Pts',(-3.58844692437017,-2.6432897533722,86.));
#57605=CARTESIAN_POINT('Ctrl Pts',(-3.55106838804729,-2.68805967903758,
86.));
#57606=CARTESIAN_POINT('Ctrl Pts',(-3.51281602034817,-2.7321119355856,86.));
#57607=CARTESIAN_POINT('Ctrl Pts',(-3.47370464217661,-2.77541893263456,
86.));
#57608=CARTESIAN_POINT('Ctrl Pts',(-3.45527487716358,-2.79582572514213,
86.));
#57609=CARTESIAN_POINT('Ctrl Pts',(-3.43665436275494,-2.81606701722102,
86.));
#57610=CARTESIAN_POINT('Ctrl Pts',(-3.41784457942235,-2.83613979970913,
86.));
#57611=CARTESIAN_POINT('Ctrl Pts',(-3.40161580152966,-2.85345827291681,
86.));
#57612=CARTESIAN_POINT('Ctrl Pts',(-3.38525177230088,-2.87064524159307,
86.));
#57613=CARTESIAN_POINT('Ctrl Pts',(-3.36875789576418,-2.88769480011766,
86.));
#57614=CARTESIAN_POINT('Ctrl Pts',(-3.27548691461708,-2.98410809920928,
86.));
#57615=CARTESIAN_POINT('Ctrl Pts',(-3.1780247285723,-3.07617507300169,86.));
#57616=CARTESIAN_POINT('Ctrl Pts',(-3.07658549505738,-3.16359906081916,
86.));
#57617=CARTESIAN_POINT('Ctrl Pts',(-2.97674507744291,-3.24964513146433,
86.));
#57618=CARTESIAN_POINT('Ctrl Pts',(-2.87305144560376,-3.33119379608769,
86.));
#57619=CARTESIAN_POINT('Ctrl Pts',(-2.76568166074672,-3.40792026882373,
86.));
#57620=CARTESIAN_POINT('Ctrl Pts',(-2.691638695275,-3.46083138882947,86.));
#57621=CARTESIAN_POINT('Ctrl Pts',(-2.61584694697416,-3.51144841450292,
86.));
#57622=CARTESIAN_POINT('Ctrl Pts',(-2.53835875722777,-3.5596515025498,86.));
#57623=CARTESIAN_POINT('Ctrl Pts',(-4.94096920053978,-0.0044629540342261,
85.1776795453431));
#57624=CARTESIAN_POINT('Ctrl Pts',(-4.94470425404279,-0.419442432737937,
85.1910411361343));
#57625=CARTESIAN_POINT('Ctrl Pts',(-4.89679105157154,-0.83357493998294,
85.2044027269256));
#57626=CARTESIAN_POINT('Ctrl Pts',(-4.79388045230233,-1.23355929227409,
85.2177643177168));
#57627=CARTESIAN_POINT('Ctrl Pts',(-4.38629013269605,-2.81774742396872,
85.2706845717988));
#57628=CARTESIAN_POINT('Ctrl Pts',(-3.11598026097668,-4.17999978023304,
85.3236048258808));
#57629=CARTESIAN_POINT('Ctrl Pts',(-1.5638870452654,-4.69668643217841,85.3765250799627));
#57630=CARTESIAN_POINT('Ctrl Pts',(-0.0117938295540432,-5.21337308412381,
85.4294453340447));
#57631=CARTESIAN_POINT('Ctrl Pts',(1.82208273014937,-4.88449403175019,85.4823655881266));
#57632=CARTESIAN_POINT('Ctrl Pts',(3.09781024523634,-3.86101411022591,85.5352858422086));
#57633=CARTESIAN_POINT('Ctrl Pts',(4.37353776032332,-2.83753418870164,85.5882060962905));
#57634=CARTESIAN_POINT('Ctrl Pts',(5.0911162307939,-1.11945339802691,85.6411263503725));
#57635=CARTESIAN_POINT('Ctrl Pts',(4.92355820931981,0.507901979845797,85.6940466044544));
#57636=CARTESIAN_POINT('Ctrl Pts',(4.75600018784572,2.1352573577185,85.7469668585364));
#57637=CARTESIAN_POINT('Ctrl Pts',(3.70330567442676,3.67188732278906,85.7998871126184));
#57638=CARTESIAN_POINT('Ctrl Pts',(2.24451339009742,4.41286256202677,85.8528073667004));
#57639=CARTESIAN_POINT('Ctrl Pts',(0.892016244518137,5.09984651908455,85.9018715778003));
#57640=CARTESIAN_POINT('Ctrl Pts',(-0.809554018707134,5.10290237899098,
85.9509357889001));
#57641=CARTESIAN_POINT('Ctrl Pts',(-2.17574227734751,4.44486702454959,86.));
#57642=CARTESIAN_POINT('',(-2.53835875722709,-3.55965150255029,26.));
#57643=CARTESIAN_POINT('Ctrl Pts',(-2.54472725763298,-3.56250530678305,
26.));
#57644=CARTESIAN_POINT('Ctrl Pts',(-2.63508309937759,-3.50703322951937,
26.));
#57645=CARTESIAN_POINT('Ctrl Pts',(-2.72311007746572,-3.44818980724315,
26.));
#57646=CARTESIAN_POINT('Ctrl Pts',(-2.80858488092082,-3.38601400346164,
26.));
#57647=CARTESIAN_POINT('Ctrl Pts',(-2.91385291450225,-3.30944027253914,
26.));
#57648=CARTESIAN_POINT('Ctrl Pts',(-3.01525129898596,-3.22781364096124,
26.));
#57649=CARTESIAN_POINT('Ctrl Pts',(-3.11268784287649,-3.1415518359691,26.));
#57650=CARTESIAN_POINT('Ctrl Pts',(-3.17680627098234,-3.08478698039414,
26.));
#57651=CARTESIAN_POINT('Ctrl Pts',(-3.23920859831056,-3.02601391139215,
26.));
#57652=CARTESIAN_POINT('Ctrl Pts',(-3.29986195943645,-2.96534150637499,
26.));
#57653=CARTESIAN_POINT('Ctrl Pts',(-3.33570437568566,-2.9294878363541,26.));
#57654=CARTESIAN_POINT('Ctrl Pts',(-3.37093593415121,-2.89297075792499,
26.));
#57655=CARTESIAN_POINT('Ctrl Pts',(-3.40554888779674,-2.85581160143786,
26.));
#57656=CARTESIAN_POINT('Ctrl Pts',(-3.4189115430604,-2.84146596069563,26.));
#57657=CARTESIAN_POINT('Ctrl Pts',(-3.43218080021828,-2.82702583304496,
26.));
#57658=CARTESIAN_POINT('Ctrl Pts',(-3.44534999888201,-2.81249952818835,
26.));
#57659=CARTESIAN_POINT('Ctrl Pts',(-3.53470458244056,-2.71393681725578,
26.));
#57660=CARTESIAN_POINT('Ctrl Pts',(-3.61953742655147,-2.6113223183339,26.));
#57661=CARTESIAN_POINT('Ctrl Pts',(-3.69975229053408,-2.50508736800556,
26.));
#57662=CARTESIAN_POINT('Ctrl Pts',(-3.78158309623279,-2.39671229701354,
26.));
#57663=CARTESIAN_POINT('Ctrl Pts',(-3.85860846570253,-2.28456889207013,
26.));
#57664=CARTESIAN_POINT('Ctrl Pts',(-3.93069241652625,-2.16907329602735,
26.));
#57665=CARTESIAN_POINT('Ctrl Pts',(-3.96222914501164,-2.11854397275863,
26.));
#57666=CARTESIAN_POINT('Ctrl Pts',(-3.99281958123178,-2.06737253695488,
26.));
#57667=CARTESIAN_POINT('Ctrl Pts',(-4.02244999738294,-2.01559181929177,
26.));
#57668=CARTESIAN_POINT('Ctrl Pts',(-4.03719360535128,-1.98982658543039,
26.));
#57669=CARTESIAN_POINT('Ctrl Pts',(-4.05169949925962,-1.96391048284628,
26.));
#57670=CARTESIAN_POINT('Ctrl Pts',(-4.06596584566683,-1.93784746217908,
26.));
#57671=CARTESIAN_POINT('Ctrl Pts',(-4.07831325232761,-1.91529012999318,
26.));
#57672=CARTESIAN_POINT('Ctrl Pts',(-4.09048280358417,-1.89261955019595,
26.));
#57673=CARTESIAN_POINT('Ctrl Pts',(-4.10246124623198,-1.86986160408455,
26.));
#57674=CARTESIAN_POINT('Ctrl Pts',(-4.16682782765767,-1.74757098296373,
26.));
#57675=CARTESIAN_POINT('Ctrl Pts',(-4.22575033277333,-1.62263418183686,
26.));
#57676=CARTESIAN_POINT('Ctrl Pts',(-4.27912376767658,-1.49549834075104,
26.));
#57677=CARTESIAN_POINT('Ctrl Pts',(-4.333101839857,-1.36692225005554,26.));
#57678=CARTESIAN_POINT('Ctrl Pts',(-4.38140486252481,-1.23609633060621,
26.));
#57679=CARTESIAN_POINT('Ctrl Pts',(-4.42388482122499,-1.10344716235086,
26.));
#57680=CARTESIAN_POINT('Ctrl Pts',(-4.46661826556875,-0.970006452370537,
26.));
#57681=CARTESIAN_POINT('Ctrl Pts',(-4.50345940350737,-0.83471991605117,
26.));
#57682=CARTESIAN_POINT('Ctrl Pts',(-4.53421101307421,-0.697996575960625,
26.));
#57683=CARTESIAN_POINT('Ctrl Pts',(-4.55727472024934,-0.595454070892716,
26.));
#57684=CARTESIAN_POINT('Ctrl Pts',(-4.57691215392772,-0.492102769524819,
26.));
#57685=CARTESIAN_POINT('Ctrl Pts',(-4.59302069983613,-0.388109915197262,
26.));
#57686=CARTESIAN_POINT('Ctrl Pts',(-4.59983051322201,-0.344147416318648,
26.));
#57687=CARTESIAN_POINT('Ctrl Pts',(-4.60600945165704,-0.300070227388598,
26.));
#57688=CARTESIAN_POINT('Ctrl Pts',(-4.61154878947915,-0.25589088056297,
26.));
#57689=CARTESIAN_POINT('Ctrl Pts',(-4.6146089290101,-0.231484539947162,
26.));
#57690=CARTESIAN_POINT('Ctrl Pts',(-4.61747426508659,-0.207042538674214,
26.));
#57691=CARTESIAN_POINT('Ctrl Pts',(-4.62014035545176,-0.182595807090288,
26.));
#57692=CARTESIAN_POINT('Ctrl Pts',(-4.6355064624287,-0.0416961970611351,
26.));
#57693=CARTESIAN_POINT('Ctrl Pts',(-4.64428121342256,0.099526957690747,
26.));
#57694=CARTESIAN_POINT('Ctrl Pts',(-4.64631642071577,0.240645210364403,
26.));
#57695=CARTESIAN_POINT('Ctrl Pts',(-4.64782495501833,0.345244739654039,
26.));
#57696=CARTESIAN_POINT('Ctrl Pts',(-4.64562987589745,0.449787288147385,
26.));
#57697=CARTESIAN_POINT('Ctrl Pts',(-4.6396534459514,0.554104703798643,26.));
#57698=CARTESIAN_POINT('Ctrl Pts',(-4.63179775743763,0.691224210145253,
26.));
#57699=CARTESIAN_POINT('Ctrl Pts',(-4.61741097334291,0.827954978565883,
26.));
#57700=CARTESIAN_POINT('Ctrl Pts',(-4.59676076751363,0.963919018344825,
26.));
#57701=CARTESIAN_POINT('Ctrl Pts',(-4.57581741441672,1.1018131835223,26.));
#57702=CARTESIAN_POINT('Ctrl Pts',(-4.54843137134414,1.23891944459888,26.));
#57703=CARTESIAN_POINT('Ctrl Pts',(-4.51482841662203,1.3748401921847,26.));
#57704=CARTESIAN_POINT('Ctrl Pts',(-4.50509310232456,1.41421861019102,26.));
#57705=CARTESIAN_POINT('Ctrl Pts',(-4.49483564045414,1.45349746044631,26.));
#57706=CARTESIAN_POINT('Ctrl Pts',(-4.48406073341117,1.49266688179373,26.));
#57707=CARTESIAN_POINT('Ctrl Pts',(-4.47783668509381,1.51529281908091,26.));
#57708=CARTESIAN_POINT('Ctrl Pts',(-4.47143997379187,1.53788224103568,26.));
#57709=CARTESIAN_POINT('Ctrl Pts',(-4.46487145429867,1.56043322804307,26.));
#57710=CARTESIAN_POINT('Ctrl Pts',(-4.45973334069111,1.57807335734872,26.));
#57711=CARTESIAN_POINT('Ctrl Pts',(-4.45449021537901,1.59568938184522,26.));
#57712=CARTESIAN_POINT('Ctrl Pts',(-4.44914654369818,1.61326759097873,26.));
#57713=CARTESIAN_POINT('Ctrl Pts',(-4.40827604464057,1.7477126360219,26.));
#57714=CARTESIAN_POINT('Ctrl Pts',(-4.36147201478811,1.88014056905998,26.));
#57715=CARTESIAN_POINT('Ctrl Pts',(-4.30904356529584,2.01016709268461,26.));
#57716=CARTESIAN_POINT('Ctrl Pts',(-4.25484746504965,2.14457752399178,26.));
#57717=CARTESIAN_POINT('Ctrl Pts',(-4.19464124103037,2.27642270082558,26.));
#57718=CARTESIAN_POINT('Ctrl Pts',(-4.12870910753944,2.4052752225727,26.));
#57719=CARTESIAN_POINT('Ctrl Pts',(-4.06277697404851,2.53412774431982,26.));
#57720=CARTESIAN_POINT('Ctrl Pts',(-3.991118562445,2.65998845878048,26.));
#57721=CARTESIAN_POINT('Ctrl Pts',(-3.91396546539836,2.78241449550764,26.));
#57722=CARTESIAN_POINT('Ctrl Pts',(-3.8599022254897,2.86820169586649,26.));
#57723=CARTESIAN_POINT('Ctrl Pts',(-3.80313988532888,2.95230207537908,26.));
#57724=CARTESIAN_POINT('Ctrl Pts',(-3.74376497539126,3.03461721426763,26.));
#57725=CARTESIAN_POINT('Ctrl Pts',(-3.71778845229355,3.07063008753137,26.));
#57726=CARTESIAN_POINT('Ctrl Pts',(-3.69131172751679,3.10630115823714,26.));
#57727=CARTESIAN_POINT('Ctrl Pts',(-3.66434142116742,3.1416216999591,26.));
#57728=CARTESIAN_POINT('Ctrl Pts',(-3.64886736739569,3.16188665189447,26.));
#57729=CARTESIAN_POINT('Ctrl Pts',(-3.63323082853231,3.18203621015477,26.));
#57730=CARTESIAN_POINT('Ctrl Pts',(-3.61743300165625,3.20206867796743,26.));
#57731=CARTESIAN_POINT('Ctrl Pts',(-3.60562290128194,3.21704450074792,26.));
#57732=CARTESIAN_POINT('Ctrl Pts',(-3.59372248215876,3.23195501636103,26.));
#57733=CARTESIAN_POINT('Ctrl Pts',(-3.58174179779154,3.24678792441536,26.));
#57734=CARTESIAN_POINT('Ctrl Pts',(-3.49102566491969,3.35910071195637,26.));
#57735=CARTESIAN_POINT('Ctrl Pts',(-3.39558140635013,3.46713215575717,26.));
#57736=CARTESIAN_POINT('Ctrl Pts',(-3.29573453983928,3.57065014592309,26.));
#57737=CARTESIAN_POINT('Ctrl Pts',(-3.19481521819522,3.67528002275919,26.));
#57738=CARTESIAN_POINT('Ctrl Pts',(-3.08939783097439,3.77529957447928,26.));
#57739=CARTESIAN_POINT('Ctrl Pts',(-2.97977151694561,3.87044492257043,26.));
#57740=CARTESIAN_POINT('Ctrl Pts',(-2.87044051512184,3.9653339673936,26.));
#57741=CARTESIAN_POINT('Ctrl Pts',(-2.75692276267532,4.05537559850027,26.));
#57742=CARTESIAN_POINT('Ctrl Pts',(-2.63946507568592,4.14027538885812,26.));
#57743=CARTESIAN_POINT('Ctrl Pts',(-2.52377549108901,4.22389717412067,26.));
#57744=CARTESIAN_POINT('Ctrl Pts',(-2.40426319127569,4.30253122094905,26.));
#57745=CARTESIAN_POINT('Ctrl Pts',(-2.28113248745318,4.37585694114117,26.));
#57746=CARTESIAN_POINT('Ctrl Pts',(-2.24413725288456,4.39788801977718,26.));
#57747=CARTESIAN_POINT('Ctrl Pts',(-2.20681518281834,4.41943960051781,26.));
#57748=CARTESIAN_POINT('Ctrl Pts',(-2.16917135428626,4.44050218283292,26.));
#57749=CARTESIAN_POINT('Ctrl Pts',(-2.54472725763282,-3.56250530678316,
26.));
#57750=CARTESIAN_POINT('Ctrl Pts',(-1.44818804155806,-4.33531677513798,
26.0490642110999));
#57751=CARTESIAN_POINT('Ctrl Pts',(1.63914523023693,-4.84388073813931,26.1510486762817));
#57752=CARTESIAN_POINT('Ctrl Pts',(4.98187809541805,-1.36671674862893,26.3059533955455));
#57753=CARTESIAN_POINT('Ctrl Pts',(3.85252000415521,3.44398917781397,26.4647141577913));
#57754=CARTESIAN_POINT('Ctrl Pts',(-0.805001512196143,5.10466442465425,
26.6234749200372));
#57755=CARTESIAN_POINT('Ctrl Pts',(-3.96413630374849,2.67678406505067,26.7514334980751));
#57756=CARTESIAN_POINT('Ctrl Pts',(-4.3679444184666,0.611489669763926,26.826471822031));
#57757=CARTESIAN_POINT('Ctrl Pts',(-4.36558297706963,0.00185075076461511,
26.848589891905));
#57758=CARTESIAN_POINT('Origin',(0.,0.,24.1514101080949));
#57759=CARTESIAN_POINT('',(2.5383587572269,-3.55965150255042,26.));
#57760=CARTESIAN_POINT('Origin',(0.,0.,26.));
#57761=CARTESIAN_POINT('Ctrl Pts',(2.53835875722654,-3.55965150255068,26.));
#57762=CARTESIAN_POINT('Ctrl Pts',(3.13016463613492,-3.13763950664917,26.026460127041));
#57763=CARTESIAN_POINT('Ctrl Pts',(4.08944058768451,-1.99447514282845,26.079380381123));
#57764=CARTESIAN_POINT('Ctrl Pts',(4.72633908941221,0.949051473338421,26.1852208892869));
#57765=CARTESIAN_POINT('Ctrl Pts',(2.60449620246589,4.46265906441401,26.3175215244918));
#57766=CARTESIAN_POINT('Ctrl Pts',(-2.34489469821123,4.60777770546463,26.4762822867377));
#57767=CARTESIAN_POINT('Ctrl Pts',(-4.30346090622908,1.74883727013167,26.5875784812721));
#57768=CARTESIAN_POINT('Ctrl Pts',(-4.3779262327693,0.151632086931482,26.6459544217245));
#57769=CARTESIAN_POINT('Ctrl Pts',(-4.37688026104952,0.00226901643694839,
26.651410108095));
#57770=CARTESIAN_POINT('Ctrl Pts',(2.86929757049756,-4.02374147429191,25.6709103465619));
#57771=CARTESIAN_POINT('Ctrl Pts',(3.53826020854994,-3.54670961616163,25.6973704736029));
#57772=CARTESIAN_POINT('Ctrl Pts',(4.62260187198943,-2.25450506767067,25.7502907276849));
#57773=CARTESIAN_POINT('Ctrl Pts',(5.34253608871791,1.0727841677129,25.8561312358488));
#57774=CARTESIAN_POINT('Ctrl Pts',(2.94405769272283,5.04447875030544,25.9884318710537));
#57775=CARTESIAN_POINT('Ctrl Pts',(-2.65061061266289,5.20851725077882,26.1471926332996));
#57776=CARTESIAN_POINT('Ctrl Pts',(-5.80869481541901,0.598627327994403,
26.3059533955455));
#57777=CARTESIAN_POINT('Ctrl Pts',(-3.6559591721986,-4.55561486272761,26.4647141577913));
#57778=CARTESIAN_POINT('Ctrl Pts',(1.84567034813922,-5.54225209737284,26.6234749200373));
#57779=CARTESIAN_POINT('Ctrl Pts',(5.65659992177503,-1.45549501989441,26.7822356822831));
#57780=CARTESIAN_POINT('Ctrl Pts',(4.29121225256454,3.96287657984353,26.940996444529));
#57781=CARTESIAN_POINT('Ctrl Pts',(-1.00202899277672,5.75456300236789,27.0997572067749));
#57782=CARTESIAN_POINT('Ctrl Pts',(-5.37797121296738,2.27936156876184,27.2585179690208));
#57783=CARTESIAN_POINT('Ctrl Pts',(-4.83194032779028,-3.28191017660925,
27.4172787312667));
#57784=CARTESIAN_POINT('Ctrl Pts',(0.136487592633803,-5.83951456248522,
27.5760394935126));
#57785=CARTESIAN_POINT('Ctrl Pts',(4.97996779668276,-3.05259748930662,27.7348002557585));
#57786=CARTESIAN_POINT('Ctrl Pts',(5.26564507543792,2.52813993990873,27.8935610180044));
#57787=CARTESIAN_POINT('Ctrl Pts',(0.732034933496452,5.79505175124635,28.0523217802503));
#57788=CARTESIAN_POINT('Ctrl Pts',(-4.47155165508331,3.75815243181214,28.2110825424962));
#57789=CARTESIAN_POINT('Ctrl Pts',(-5.58263982081247,-1.71832134856424,
28.369843304742));
#57790=CARTESIAN_POINT('Ctrl Pts',(-1.58432433047622,-5.62213569522022,
28.5286040669879));
#57791=CARTESIAN_POINT('Ctrl Pts',(3.86401257103054,-4.38039933096899,28.6873648292338));
#57792=CARTESIAN_POINT('Ctrl Pts',(5.77588745817332,0.870412097209825,28.8461255914797));
#57793=CARTESIAN_POINT('Ctrl Pts',(2.40149355054825,5.32459589387785,29.0048863537256));
#57794=CARTESIAN_POINT('Ctrl Pts',(-3.17082052230127,4.90554683073371,29.1636471159715));
#57795=CARTESIAN_POINT('Ctrl Pts',(-5.84110284449404,-0.00320850462351047,
29.3224078782174));
#57796=CARTESIAN_POINT('Ctrl Pts',(-3.16542940092975,-4.90902733376601,
29.4811686404633));
#57797=CARTESIAN_POINT('Ctrl Pts',(2.40734170730851,-5.32195439090584,29.6399294027091));
#57798=CARTESIAN_POINT('Ctrl Pts',(5.77684015826,-0.8640662324248,29.7986901649551));
#57799=CARTESIAN_POINT('Ctrl Pts',(3.85919803712304,4.38464173738479,29.9574509272009));
#57800=CARTESIAN_POINT('Ctrl Pts',(-1.59050000656898,5.62039165738282,30.1162116894468));
#57801=CARTESIAN_POINT('Ctrl Pts',(-5.58452386271215,1.71218745603623,30.2749724516927));
#57802=CARTESIAN_POINT('Ctrl Pts',(-4.46742089771919,-3.76306300482994,
30.4337332139386));
#57803=CARTESIAN_POINT('Ctrl Pts',(0.738402131764131,-5.79424325925859,
30.5924939761845));
#57804=CARTESIAN_POINT('Ctrl Pts',(5.26841697560084,-2.522355095433,30.7512547384304));
#57805=CARTESIAN_POINT('Ctrl Pts',(4.97661567740753,3.05806949811635,30.9100155006762));
#57806=CARTESIAN_POINT('Ctrl Pts',(0.130063698581311,5.83965547701761,31.0687762629222));
#57807=CARTESIAN_POINT('Ctrl Pts',(-4.83552655005252,3.27661038876524,31.227537025168));
#57808=CARTESIAN_POINT('Ctrl Pts',(-5.37549519698693,-2.28528861265885,
31.386297787414));
#57809=CARTESIAN_POINT('Ctrl Pts',(-0.995646443005195,-5.75562167072471,
31.5450585496598));
#57810=CARTESIAN_POINT('Ctrl Pts',(4.2954483480341,-3.95823396799194,31.7038193119058));
#57811=CARTESIAN_POINT('Ctrl Pts',(5.65521760477304,1.46185036807875,31.8625800741516));
#57812=CARTESIAN_POINT('Ctrl Pts',(1.83915896875347,5.54400459448242,32.0213408363975));
#57813=CARTESIAN_POINT('Ctrl Pts',(-3.66015413331184,4.5521164721907,32.1801015986434));
#57814=CARTESIAN_POINT('Ctrl Pts',(-5.80958237170622,-0.606007691658192,
32.3388623608893));
#57815=CARTESIAN_POINT('Ctrl Pts',(-2.64190336751104,-5.20949510535547,
32.4976231231352));
#57816=CARTESIAN_POINT('Ctrl Pts',(2.9437262966194,-5.04509347253155,32.6563838853811));
#57817=CARTESIAN_POINT('Ctrl Pts',(5.83516773679323,-0.263268189260048,
32.8151446476269));
#57818=CARTESIAN_POINT('Ctrl Pts',(3.3860854267346,4.75950818245377,32.9739054098728));
#57819=CARTESIAN_POINT('Ctrl Pts',(-2.1620456951976,5.42623728451552,33.1326661721187));
#57820=CARTESIAN_POINT('Ctrl Pts',(-5.73140655633933,1.12670827721268,33.2914269343647));
#57821=CARTESIAN_POINT('Ctrl Pts',(-4.0552090690265,-4.20401856114767,33.4501876966105));
#57822=CARTESIAN_POINT('Ctrl Pts',(1.33243962623321,-5.68709919892666,33.6089484588564));
#57823=CARTESIAN_POINT('Ctrl Pts',(5.50059887566598,-1.96517293514109,33.7677092211022));
#57824=CARTESIAN_POINT('Ctrl Pts',(4.63444201610888,3.55533962587452,33.9264699833482));
#57825=CARTESIAN_POINT('Ctrl Pts',(-0.473297737465698,5.82189676202686,
34.0852307455941));
#57826=CARTESIAN_POINT('Ctrl Pts',(-5.14786094464401,2.7600761494201,34.24399150784));
#57827=CARTESIAN_POINT('Ctrl Pts',(-5.11094457182416,-2.82785046275963,
34.4027522700858));
#57828=CARTESIAN_POINT('Ctrl Pts',(-0.396335611036177,-5.82764195360469,
34.5615130323317));
#57829=CARTESIAN_POINT('Ctrl Pts',(4.68101180720102,-3.49379752086946,34.7202737945776));
#57830=CARTESIAN_POINT('Ctrl Pts',(5.47415423612042,2.03767712240033,34.8790345568235));
#57831=CARTESIAN_POINT('Ctrl Pts',(1.2571834979241,5.7042074215912,35.0377953190694));
#57832=CARTESIAN_POINT('Ctrl Pts',(-4.11039997874232,4.15007285125745,35.1965560813153));
#57833=CARTESIAN_POINT('Ctrl Pts',(-5.71601984106162,-1.20233515817297,
35.3553168435612));
#57834=CARTESIAN_POINT('Ctrl Pts',(-2.09016374674189,-5.45432930503785,
35.5140776058071));
#57835=CARTESIAN_POINT('Ctrl Pts',(3.44867405347895,-4.71435466727419,35.6728383680529));
#57836=CARTESIAN_POINT('Ctrl Pts',(5.8311800188353,0.340341363817132,35.8315991302989));
#57837=CARTESIAN_POINT('Ctrl Pts',(2.87681191524069,5.0835465828807,35.9903598925447));
#57838=CARTESIAN_POINT('Ctrl Pts',(-2.7105023265463,5.17413469033962,36.1491206547906));
#57839=CARTESIAN_POINT('Ctrl Pts',(-5.81708204570653,0.529196683197753,
36.3078814170365));
#57840=CARTESIAN_POINT('Ctrl Pts',(-3.5996905915515,-4.60007829292986,36.4666421792824));
#57841=CARTESIAN_POINT('Ctrl Pts',(1.91224764597227,-5.51922110414707,36.6254029415283));
#57842=CARTESIAN_POINT('Ctrl Pts',(5.67403842753732,-1.38700417404515,36.7841637037742));
#57843=CARTESIAN_POINT('Ctrl Pts',(4.24277592445978,4.01464134273703,36.9429244660201));
#57844=CARTESIAN_POINT('Ctrl Pts',(-1.07160470196143,5.74196447382976,37.1016852282659));
#57845=CARTESIAN_POINT('Ctrl Pts',(-5.40521997255572,2.2140663278849,37.2604459905119));
#57846=CARTESIAN_POINT('Ctrl Pts',(-4.79181281967314,-3.34021295087678,
37.4192067527577));
#57847=CARTESIAN_POINT('Ctrl Pts',(0.207207793602656,-5.83742730886296,
37.5779675150036));
#57848=CARTESIAN_POINT('Ctrl Pts',(5.01658550492884,-2.99204988723897,37.7367282772495));
#57849=CARTESIAN_POINT('Ctrl Pts',(5.23463092854471,2.59174298453994,37.8954890394954));
#57850=CARTESIAN_POINT('Ctrl Pts',(0.661782232472825,5.80349351104764,38.0542498017413));
#57851=CARTESIAN_POINT('Ctrl Pts',(-4.51674977715968,3.70370950622708,38.2130105639872));
#57852=CARTESIAN_POINT('Ctrl Pts',(-5.5614144248173,-1.78582256997244,38.371771326233));
#57853=CARTESIAN_POINT('Ctrl Pts',(-1.51610271526659,-5.64091528147253,
38.530532088479));
#57854=CARTESIAN_POINT('Ctrl Pts',(3.91679250925652,-4.33327002336813,38.6892928507249));
#57855=CARTESIAN_POINT('Ctrl Pts',(5.76491958932306,0.940316321579044,38.8480536129708));
#57856=CARTESIAN_POINT('Ctrl Pts',(2.33681616947948,5.35329644668107,39.0068143752167));
#57857=CARTESIAN_POINT('Ctrl Pts',(-3.23001278765103,4.86677614521149,39.1655751374625));
#57858=CARTESIAN_POINT('Ctrl Pts',(-5.84063537949807,-0.0739663419686063,
39.3243358997085));
#57859=CARTESIAN_POINT('Ctrl Pts',(-3.10573006749788,-4.94701257364771,
39.4830966619543));
#57860=CARTESIAN_POINT('Ctrl Pts',(2.47163426803653,-5.29240178945783,39.6418574242002));
#57861=CARTESIAN_POINT('Ctrl Pts',(5.78688342441216,-0.794023229038551,
39.8006181864461));
#57862=CARTESIAN_POINT('Ctrl Pts',(3.80580010810998,4.43106964435213,39.959378948692));
#57863=CARTESIAN_POINT('Ctrl Pts',(-1.65846771681237,5.60071223044711,40.1181397109378));
#57864=CARTESIAN_POINT('Ctrl Pts',(-5.60485522875205,1.64441190725433,40.2769004731838));
#57865=CARTESIAN_POINT('Ctrl Pts',(-4.4215080328057,-3.81690442267336,40.4356612354296));
#57866=CARTESIAN_POINT('Ctrl Pts',(0.808538371485783,-5.78487323610672,
40.5944219976756));
#57867=CARTESIAN_POINT('Ctrl Pts',(5.29858576106737,-2.45834936260147,40.7531827599214));
#57868=CARTESIAN_POINT('Ctrl Pts',(4.93920561471065,3.1181309388157,40.9119435221673));
#57869=CARTESIAN_POINT('Ctrl Pts',(0.0593136197707885,5.84080256047905,
41.0707042844132));
#57870=CARTESIAN_POINT('Ctrl Pts',(-4.87486401174139,3.21779326915472,41.2294650466591));
#57871=CARTESIAN_POINT('Ctrl Pts',(-5.34741719504777,-2.35023871087517,
41.388225808905));
#57872=CARTESIAN_POINT('Ctrl Pts',(-0.925850822461446,-5.76726043373597,
41.5469865711509));
#57873=CARTESIAN_POINT('Ctrl Pts',(4.34308250332321,-3.90590924437788,41.7057473333967));
#57874=CARTESIAN_POINT('Ctrl Pts',(5.63709406088405,1.53024939298615,41.8645080956427));
#57875=CARTESIAN_POINT('Ctrl Pts',(1.77186494664376,5.56587704381296,42.0232688578886));
#57876=CARTESIAN_POINT('Ctrl Pts',(-3.71502908908446,4.50744401221416,42.1820296201344));
#57877=CARTESIAN_POINT('Ctrl Pts',(-5.80181502544146,-0.676339461033121,
42.3407903823803));
#57878=CARTESIAN_POINT('Ctrl Pts',(-2.57860263176698,-5.24111640048504,
42.4995511446262));
#57879=CARTESIAN_POINT('Ctrl Pts',(3.00462565494359,-5.00906351822809,42.6583119068721));
#57880=CARTESIAN_POINT('Ctrl Pts',(5.83792876476416,-0.192562700251437,
42.817072669118));
#57881=CARTESIAN_POINT('Ctrl Pts',(3.32818114721658,4.80017738289961,42.9758334313639));
#57882=CARTESIAN_POINT('Ctrl Pts',(-2.22761951688042,5.39964850189364,43.1345941936098));
#57883=CARTESIAN_POINT('Ctrl Pts',(-5.74463475560437,1.05719637754358,43.2933549558557));
#57884=CARTESIAN_POINT('Ctrl Pts',(-4.0039847938458,-4.25283416401821,43.4521157181015));
#57885=CARTESIAN_POINT('Ctrl Pts',(1.40123435454846,-5.67054097415953,43.6108764803475));
#57886=CARTESIAN_POINT('Ctrl Pts',(5.5240010203993,-1.89839547582067,43.7696372425933));
#57887=CARTESIAN_POINT('Ctrl Pts',(4.59103321957251,3.61121954923408,43.9283980048393));
#57888=CARTESIAN_POINT('Ctrl Pts',(-0.543788418742688,5.81573613669244,
44.0871587670851));
#57889=CARTESIAN_POINT('Ctrl Pts',(-5.18091828599107,2.69751336787648,44.245919529331));
#57890=CARTESIAN_POINT('Ctrl Pts',(-5.07631348469077,-2.88955603183869,
44.4046802915769));
#57891=CARTESIAN_POINT('Ctrl Pts',(-0.325711524187161,-5.83201548857688,
44.5634410538228));
#57892=CARTESIAN_POINT('Ctrl Pts',(4.7229915722406,-3.43683622893689,44.7222018160687));
#57893=CARTESIAN_POINT('Ctrl Pts',(5.44906851609775,2.1038405269557,44.8809625783145));
#57894=CARTESIAN_POINT('Ctrl Pts',(1.18799151005716,5.71901816993276,45.0397233405605));
#57895=CARTESIAN_POINT('Ctrl Pts',(-4.16037161366087,4.09997569410277,45.1984841028063));
#57896=CARTESIAN_POINT('Ctrl Pts',(-5.70103555635091,-1.27148977235826,
45.3572448650522));
#57897=CARTESIAN_POINT('Ctrl Pts',(-2.02393761747008,-5.47924896099626,
45.5160056272981));
#57898=CARTESIAN_POINT('Ctrl Pts',(3.50552985089882,-4.67223213469171,45.674766389544));
#57899=CARTESIAN_POINT('Ctrl Pts',(5.82662932192163,0.410954256471436,45.8335271517899));
#57900=CARTESIAN_POINT('Ctrl Pts',(2.81501966081174,5.11802275935076,45.9922879140358));
#57901=CARTESIAN_POINT('Ctrl Pts',(-2.77298197976823,5.1409205008315,46.1510486762817));
#57902=CARTESIAN_POINT('Ctrl Pts',(-5.82306581062682,0.458690768489886,
46.3098094385276));
#57903=CARTESIAN_POINT('Ctrl Pts',(-3.54370194373858,-4.64334676606566,
46.4685702007734));
#57904=CARTESIAN_POINT('Ctrl Pts',(1.97896618584451,-5.49565150744413,46.6273309630194));
#57905=CARTESIAN_POINT('Ctrl Pts',(5.69042401383344,-1.31816812234872,46.7860917252652));
#57906=CARTESIAN_POINT('Ctrl Pts',(4.19383196809736,4.0657429922898,46.9448524875111));
#57907=CARTESIAN_POINT('Ctrl Pts',(-1.14108319710691,5.72856193064797,47.103613249757));
#57908=CARTESIAN_POINT('Ctrl Pts',(-5.4316441654788,2.14842600887457,47.2623740120029));
#57909=CARTESIAN_POINT('Ctrl Pts',(-4.75099848187323,-3.39801502074773,
47.4211347742488));
#57910=CARTESIAN_POINT('Ctrl Pts',(0.277906133480956,-5.83448890966147,
47.5798955364947));
#57911=CARTESIAN_POINT('Ctrl Pts',(5.05246256671996,-2.93106033166876,47.7386562987406));
#57912=CARTESIAN_POINT('Ctrl Pts',(5.20285092941832,2.65496419227074,47.8974170609865));
#57913=CARTESIAN_POINT('Ctrl Pts',(0.591431198362095,5.8110843905069,48.0561778232323));
#57914=CARTESIAN_POINT('Ctrl Pts',(-4.56128443093633,3.6487226526672,48.2149385854782));
#57915=CARTESIAN_POINT('Ctrl Pts',(-5.53937322279471,-1.85306150857812,
48.3736993477241));
#57916=CARTESIAN_POINT('Ctrl Pts',(-1.44765843879317,-5.65886717467194,
48.53246010997));
#57917=CARTESIAN_POINT('Ctrl Pts',(3.96899756769466,-4.28550475015754,48.6912208722159));
#57918=CARTESIAN_POINT('Ctrl Pts',(5.75310576561908,1.01008252414809,48.8499816344618));
#57919=CARTESIAN_POINT('Ctrl Pts',(2.27179583594514,5.38121141898098,49.0087423967076));
#57920=CARTESIAN_POINT('Ctrl Pts',(-3.28873103569315,4.8272912519194,49.1675031589537));
#57921=CARTESIAN_POINT('Ctrl Pts',(-5.83931080786754,-0.144713320429998,
49.3262639211994));
#57922=CARTESIAN_POINT('Ctrl Pts',(-3.04557496461057,-4.98427184159595,
49.4850246834454));
#57923=CARTESIAN_POINT('Ctrl Pts',(2.53556411455661,-5.26207252676754,49.6437854456913));
#57924=CARTESIAN_POINT('Ctrl Pts',(5.79607746626723,-0.72386370334331,49.8025462079371));
#57925=CARTESIAN_POINT('Ctrl Pts',(3.75184367735869,4.47684729208542,49.961306970183));
#57926=CARTESIAN_POINT('Ctrl Pts',(-1.72619204662586,5.58021089871651,50.120067732429));
#57927=CARTESIAN_POINT('Ctrl Pts',(-5.62436408231579,1.57639504108098,50.2788284946748));
#57928=CARTESIAN_POINT('Ctrl Pts',(-4.37494631143252,-3.87018570976535,
50.4375892569207));
#57929=CARTESIAN_POINT('Ctrl Pts',(0.878555958148904,-5.77465428267269,
50.5963500191666));
#57930=CARTESIAN_POINT('Ctrl Pts',(5.32797697899131,-2.39398286696617,50.7551107814125));
#57931=CARTESIAN_POINT('Ctrl Pts',(4.90107072348494,3.17773479374659,50.9138715436583));
#57932=CARTESIAN_POINT('Ctrl Pts',(-0.0114451633093337,5.84109250604932,
51.0726323059043));
#57933=CARTESIAN_POINT('Ctrl Pts',(-4.91348608704586,3.15850393832203,51.2313930681501));
#57934=CARTESIAN_POINT('Ctrl Pts',(-5.31855445953128,-2.4148439115166,51.3901538303961));
#57935=CARTESIAN_POINT('Ctrl Pts',(-0.855919333292373,-5.77805285116754,
51.5489145926419));
#57936=CARTESIAN_POINT('Ctrl Pts',(4.39007931117216,-3.85301132850749,51.7076753548878));
#57937=CARTESIAN_POINT('Ctrl Pts',(5.61814327333331,1.59842385376603,51.8664361171337));
#57938=CARTESIAN_POINT('Ctrl Pts',(1.70431090331913,5.58693270058057,52.0251968793796));
#57939=CARTESIAN_POINT('Ctrl Pts',(-3.76935886426715,4.46211008474238,52.1839576416255));
#57940=CARTESIAN_POINT('Ctrl Pts',(-5.79319626271042,-0.746571977579234,
52.3427184038713));
#57941=CARTESIAN_POINT('Ctrl Pts',(-2.51492348603726,-5.27196856168236,
52.5014791661173));
#57942=CARTESIAN_POINT('Ctrl Pts',(3.06508408439537,-4.9722984837573,52.6602399283631));
#57943=CARTESIAN_POINT('Ctrl Pts',(5.83983307657691,-0.121828952662795,
52.8190006906091));
#57944=CARTESIAN_POINT('Ctrl Pts',(3.26978845705136,4.84014215722252,52.9777614528549));
#57945=CARTESIAN_POINT('Ctrl Pts',(-2.29286643535651,5.37226732075056,53.1365222151009));
#57946=CARTESIAN_POINT('Ctrl Pts',(-5.75701992960891,0.98752933428568,53.2952829773466));
#57947=CARTESIAN_POINT('Ctrl Pts',(-3.95217293381976,-4.30102566339373,
53.4540437395927));
#57948=CARTESIAN_POINT('Ctrl Pts',(1.46982345169535,-5.65315059739567,53.6128045018384));
#57949=CARTESIAN_POINT('Ctrl Pts',(5.54659251787697,-1.83133942692776,53.7715652640845));
#57950=CARTESIAN_POINT('Ctrl Pts',(4.54695068882314,3.66656952605562,53.9303260263302));
#57951=CARTESIAN_POINT('Ctrl Pts',(-0.61419929905889,5.80872205196845,54.0890867885762));
#57952=CARTESIAN_POINT('Ctrl Pts',(-5.21321532748033,2.63455472619438,54.2478475508221));
#57953=CARTESIAN_POINT('Ctrl Pts',(-5.04093744845616,-2.95083755851469,
54.4066083130679));
#57954=CARTESIAN_POINT('Ctrl Pts',(-0.255039639165707,-5.8355331751643,
54.5653690753139));
#57955=CARTESIAN_POINT('Ctrl Pts',(4.76427823817645,-3.37937058122179,54.7241298375597));
#57956=CARTESIAN_POINT('Ctrl Pts',(5.42318314516584,2.16969519287334,54.8828905998057));
#57957=CARTESIAN_POINT('Ctrl Pts',(1.11862518441343,5.7329896522482,55.0416513620514));
#57958=CARTESIAN_POINT('Ctrl Pts',(-4.20973271396536,4.04927686543645,55.2004121242976));
#57959=CARTESIAN_POINT('Ctrl Pts',(-5.68521464456297,-1.34045779539507,
55.3591728865431));
#57960=CARTESIAN_POINT('Ctrl Pts',(-1.95741447531414,-5.50336453706454,
55.5179336487893));
#57961=CARTESIAN_POINT('Ctrl Pts',(3.56187121174587,-4.62942395195395,55.676694411035));
#57962=CARTESIAN_POINT('Ctrl Pts',(5.82122356704326,0.481506841580768,55.835455173281));
#57963=CARTESIAN_POINT('Ctrl Pts',(2.75281430219354,5.15174786588276,55.9942159355268));
#57964=CARTESIAN_POINT('Ctrl Pts',(-2.83505469783139,5.10695188114131,56.1529766977728));
#57965=CARTESIAN_POINT('Ctrl Pts',(-5.82819504052776,0.388117540903014,
56.3117374600186));
#57966=CARTESIAN_POINT('Ctrl Pts',(-3.48719325759759,-4.6859338279744,56.4704982222645));
#57967=CARTESIAN_POINT('Ctrl Pts',(2.04539431239091,-5.47127542377716,56.6292589845104));
#57968=CARTESIAN_POINT('Ctrl Pts',(5.70597453029646,-1.24913862945516,56.7880197467563));
#57969=CARTESIAN_POINT('Ctrl Pts',(4.14427256681325,4.11624799398041,56.9467805090021));
#57970=CARTESIAN_POINT('Ctrl Pts',(-1.21039423827122,5.71431872089305,57.1055412712481));
#57971=CARTESIAN_POINT('Ctrl Pts',(-5.4572712645165,2.08247040830632,57.2643020334939));
#57972=CARTESIAN_POINT('Ctrl Pts',(-4.709486934955,-3.45531843184919,57.4230627957399));
#57973=CARTESIAN_POINT('Ctrl Pts',(0.348563690628765,-5.8306942991006,57.5818235579858));
#57974=CARTESIAN_POINT('Ctrl Pts',(5.08759817953255,-2.86964064293877,57.7405843202316));
#57975=CARTESIAN_POINT('Ctrl Pts',(5.17030741181829,2.71779578395536,57.8993450824775));
#57976=CARTESIAN_POINT('Ctrl Pts',(0.520993371711727,5.81782249322041,58.0581058447234));
#57977=CARTESIAN_POINT('Ctrl Pts',(-4.60514971613518,3.59320034898822,58.2168666069693));
#57978=CARTESIAN_POINT('Ctrl Pts',(-5.51651911764551,-1.9200285103718,58.3756273692151));
#57979=CARTESIAN_POINT('Ctrl Pts',(-1.37900171841615,-5.67598862900501,
58.5343881314612));
#57980=CARTESIAN_POINT('Ctrl Pts',(4.02062017566359,-4.23711057904269,58.6931488937069));
#57981=CARTESIAN_POINT('Ctrl Pts',(5.74044767353369,1.07970049708729,58.8519096559529));
#57982=CARTESIAN_POINT('Ctrl Pts',(2.20644211632846,5.40833669840192,59.0106704181987));
#57983=CARTESIAN_POINT('Ctrl Pts',(-3.34696666239261,4.78709795354361,59.1694311804446));
#57984=CARTESIAN_POINT('Ctrl Pts',(-5.83712931726406,-0.215439062208749,
59.3281919426906));
#57985=CARTESIAN_POINT('Ctrl Pts',(-2.98497292353889,-5.02079966755579,
59.4869527049364));
#57986=CARTESIAN_POINT('Ctrl Pts',(2.59912186699419,-5.23097105483309,59.6457134671823));
#57987=CARTESIAN_POINT('Ctrl Pts',(5.80442093364305,-0.653597950635783,
59.8044742294282));
#57988=CARTESIAN_POINT('Ctrl Pts',(3.69733666347582,4.52196796239271,59.9632349916741));
#57989=CARTESIAN_POINT('Ctrl Pts',(-1.79366305772334,5.55889067092954,60.1219957539199));
#57990=CARTESIAN_POINT('Ctrl Pts',(-5.64304756034266,1.5081468389052,60.2807565161659));
#57991=CARTESIAN_POINT('Ctrl Pts',(-4.32774256660426,-3.92289904703017,
60.4395172784117));
#57992=CARTESIAN_POINT('Ctrl Pts',(0.948444616708253,-5.76358789861195,
60.5982780406577));
#57993=CARTESIAN_POINT('Ctrl Pts',(5.35658631619137,-2.32926505429939,60.7570388029035));
#57994=CARTESIAN_POINT('Ctrl Pts',(4.86221660003666,3.23687231603548,60.9157995651494));
#57995=CARTESIAN_POINT('Ctrl Pts',(-0.0822022668114812,5.84052527118238,
61.0745603273953));
#57996=CARTESIAN_POINT('Ctrl Pts',(-4.95138710817278,3.09875109697584,61.2333210896412));
#57997=CARTESIAN_POINT('Ctrl Pts',(-5.28891122604591,-2.47909473376766,
61.3920818518871));
#57998=CARTESIAN_POINT('Ctrl Pts',(-0.785862237944882,-5.78799733923239,
61.5508426141331));
#57999=CARTESIAN_POINT('Ctrl Pts',(4.43643187479794,-3.79954798315087,61.7096033763787));
#58000=CARTESIAN_POINT('Ctrl Pts',(5.59836802314956,1.66636374581465,61.8683641386249));
#58001=CARTESIAN_POINT('Ctrl Pts',(1.63650675233685,5.6071684748672,62.0271249008705));
#58002=CARTESIAN_POINT('Ctrl Pts',(-3.82313548596416,4.41612134253018,62.1858856631167));
#58003=CARTESIAN_POINT('Ctrl Pts',(-5.78372734831682,-0.816694934673283,
62.3446464253623));
#58004=CARTESIAN_POINT('Ctrl Pts',(-2.45087527523776,-5.30204706139213,
62.5034071876083));
#58005=CARTESIAN_POINT('Ctrl Pts',(3.12509271269893,-4.93480376438871,62.6621679498542));
#58006=CARTESIAN_POINT('Ctrl Pts',(5.84088039277376,-0.0510773266730637,
62.8209287121001));
#58007=CARTESIAN_POINT('Ctrl Pts',(3.21091592536738,4.879396640591,62.979689474346));
#58008=CARTESIAN_POINT('Ctrl Pts',(-2.35777687563918,5.34409775927519,63.1384502365919));
#58009=CARTESIAN_POINT('Ctrl Pts',(-5.76856026082839,0.917717371079188,
63.2972109988377));
#58010=CARTESIAN_POINT('Ctrl Pts',(-3.89978109233997,-4.34858598717061,
63.4559717610837));
#58011=CARTESIAN_POINT('Ctrl Pts',(1.53819685222249,-5.63493062067332,63.6147325233296));
#58012=CARTESIAN_POINT('Ctrl Pts',(5.56837005279627,-1.76401462893886,63.7734932855754));
#58013=CARTESIAN_POINT('Ctrl Pts',(4.50220089297303,3.72138143372885,63.9322540478213));
#58014=CARTESIAN_POINT('Ctrl Pts',(-0.684520045616047,5.80085553717197,
64.0910148100672));
#58015=CARTESIAN_POINT('Ctrl Pts',(-5.2447473295203,2.57120946355576,64.2497755723131));
#58016=CARTESIAN_POINT('Ctrl Pts',(-5.00482165455439,-3.01168604972238,
64.408536334559));
#58017=CARTESIAN_POINT('Ctrl Pts',(-0.184330327072359,-5.83819449714635,
64.5672970968048));
#58018=CARTESIAN_POINT('Ctrl Pts',(4.80486574618941,-3.32140901080918,64.7260578590508));
#58019=CARTESIAN_POINT('Ctrl Pts',(5.39650192200348,2.23523145597974,64.8848186212967));
#58020=CARTESIAN_POINT('Ctrl Pts',(1.04909470050257,5.74611981822221,65.0435793835425));
#58021=CARTESIAN_POINT('Ctrl Pts',(-4.25847603591327,3.99798380531258,65.2023401457885));
#58022=CARTESIAN_POINT('Ctrl Pts',(-5.66855942741703,-1.40922910622467,
65.3611009080343));
#58023=CARTESIAN_POINT('Ctrl Pts',(-1.8906040825464,-5.52667249428149,65.5198616702802));
#58024=CARTESIAN_POINT('Ctrl Pts',(3.61768986792422,-4.58593640116248,65.6786224325261));
#58025=CARTESIAN_POINT('Ctrl Pts',(5.8149635474948,0.551988765551636,65.8373831947719));
#58026=CARTESIAN_POINT('Ctrl Pts',(2.6902049680239,5.18471695331663,65.996143957018));
#58027=CARTESIAN_POINT('Ctrl Pts',(-2.89671137156331,5.07223381616474,66.1549047192637));
#58028=CARTESIAN_POINT('Ctrl Pts',(-5.83246898269471,0.317487357059558,
66.3136654815097));
#58029=CARTESIAN_POINT('Ctrl Pts',(-3.4301728257792,-4.72783322900402,66.4724262437555));
#58030=CARTESIAN_POINT('Ctrl Pts',(2.11152227728272,-5.44609643033688,66.6311870060015));
#58031=CARTESIAN_POINT('Ctrl Pts',(5.72068769488774,-1.1799258254438,66.7899477682473));
#58032=CARTESIAN_POINT('Ctrl Pts',(4.0941049934505,4.16614893619904,66.9487085304932));
#58033=CARTESIAN_POINT('Ctrl Pts',(-1.27952765405788,5.69923693475624,67.1074692927391));
#58034=CARTESIAN_POINT('Ctrl Pts',(-5.48209750889141,2.01620920516577,67.266230054985));
#58035=CARTESIAN_POINT('Ctrl Pts',(-4.66728427073886,-3.51211477490457,
67.4249908172309));
#58036=CARTESIAN_POINT('Ctrl Pts',(0.419170096048379,-5.82604403403957,
67.5837515794768));
#58037=CARTESIAN_POINT('Ctrl Pts',(5.12198718721476,-2.80779983438927,67.7425123417226));
#58038=CARTESIAN_POINT('Ctrl Pts',(5.13700515150643,2.78022853905663,67.9012731039686));
#58039=CARTESIAN_POINT('Ctrl Pts',(0.45047908927406,5.82370683037148,68.0600338662144));
#58040=CARTESIAN_POINT('Ctrl Pts',(-4.64833919552487,3.53715074308911,68.2187946284603));
#58041=CARTESIAN_POINT('Ctrl Pts',(-5.49285546321007,-1.98671374794472,
68.3775553907063));
#58042=CARTESIAN_POINT('Ctrl Pts',(-1.31014262951052,-5.69227713189796,
68.5363161529521));
#58043=CARTESIAN_POINT('Ctrl Pts',(4.07165275754471,-4.18809461186912,68.6950769151981));
#58044=CARTESIAN_POINT('Ctrl Pts',(5.72694717064212,1.14916002395785,68.8538376774439));
#58045=CARTESIAN_POINT('Ctrl Pts',(2.14076460128891,5.43466830430864,69.0125984396898));
#58046=CARTESIAN_POINT('Ctrl Pts',(-3.40471112167017,4.74620214845141,69.1713592019357));
#58047=CARTESIAN_POINT('Ctrl Pts',(-5.83409122782134,-0.28613318830099,
69.3301199641816));
#58048=CARTESIAN_POINT('Ctrl Pts',(-2.92393283763341,-5.0565906910682,69.4888807264275));
#58049=CARTESIAN_POINT('Ctrl Pts',(2.66229819824794,-5.19910193779603,69.6476414886733));
#58050=CARTESIAN_POINT('Ctrl Pts',(5.81191260213551,-0.583236282416525,
69.8064022509193));
#58051=CARTESIAN_POINT('Ctrl Pts',(3.64228706536681,4.56642503381477,69.9651630131651));
#58052=CARTESIAN_POINT('Ctrl Pts',(-1.86087084873268,5.53675467583008,70.123923775411));
#58053=CARTESIAN_POINT('Ctrl Pts',(-5.66090292103185,1.43967731615189,70.282684537657));
#58054=CARTESIAN_POINT('Ctrl Pts',(-4.27990372547136,-3.97503669878468,
70.4414452999028));
#58055=CARTESIAN_POINT('Ctrl Pts',(1.01819409100193,-5.75167570791655,70.6002060621487));
#58056=CARTESIAN_POINT('Ctrl Pts',(5.38440957424679,-2.26420542194124,70.7589668243946));
#58057=CARTESIAN_POINT('Ctrl Pts',(4.82264894620915,3.29553482724991,70.9177275866405));
#58058=CARTESIAN_POINT('Ctrl Pts',(-0.152947307129394,5.83910093911992,
71.0764883488863));
#58059=CARTESIAN_POINT('Ctrl Pts',(-4.98856151314671,3.03854351384673,71.2352491111322));
#58060=CARTESIAN_POINT('Ctrl Pts',(-5.25849184473667,-2.542981748819,71.3940098733781));
#58061=CARTESIAN_POINT('Ctrl Pts',(-0.71568981729892,-5.79709243857671,
71.5527706356241));
#58062=CARTESIAN_POINT('Ctrl Pts',(4.48213339196102,-3.74552705405491,71.7115313978699));
#58063=CARTESIAN_POINT('Ctrl Pts',(5.57777121235107,1.73405909895161,71.8702921601158));
#58064=CARTESIAN_POINT('Ctrl Pts',(1.56846244395725,5.62658139707268,72.0290529223617));
#58065=CARTESIAN_POINT('Ctrl Pts',(-3.87635106245531,4.36948453442625,72.1878136846075));
#58066=CARTESIAN_POINT('Ctrl Pts',(-5.77340967182392,-0.88669804176993,
72.3465744468535));
#58067=CARTESIAN_POINT('Ctrl Pts',(-2.38646739844469,-5.33134748559404,
72.5053352090994));
#58068=CARTESIAN_POINT('Ctrl Pts',(3.18464273358708,-4.89658486247307,72.6640959713453));
#58069=CARTESIAN_POINT('Ctrl Pts',(5.84107055966092,0.0196817949154431,
72.8228567335911));
#58070=CARTESIAN_POINT('Ctrl Pts',(3.15157219170978,4.91793507240897,72.9816174958371));
#58071=CARTESIAN_POINT('Ctrl Pts',(-2.42234131212014,5.31514395135115,73.1403782580829));
#58072=CARTESIAN_POINT('Ctrl Pts',(-5.77925405571895,0.847770732830903,
73.2991390203289));
#58073=CARTESIAN_POINT('Ctrl Pts',(-3.84681695791018,-4.39550815587048,
73.4578997825747));
#58074=CARTESIAN_POINT('Ctrl Pts',(1.60634452233207,-5.61588371777435,73.6166605448206));
#58075=CARTESIAN_POINT('Ctrl Pts',(5.58933042930359,-1.6964309617693,73.7754213070665));
#58076=CARTESIAN_POINT('Ctrl Pts',(4.45679039905553,3.77564722860532,73.9341820693123));
#58077=CARTESIAN_POINT('Ctrl Pts',(-0.754740338843374,5.79213774671418,
74.0929428315583));
#58078=CARTESIAN_POINT('Ctrl Pts',(-5.2755096647891,2.50748687587913,74.2517035938041));
#58079=CARTESIAN_POINT('Ctrl Pts',(-4.96797140297887,-3.07209257594453,
74.4104643560501));
#58080=CARTESIAN_POINT('Ctrl Pts',(-0.113593964499922,-5.83999906397405,
74.5692251182959));
#58081=CARTESIAN_POINT('Ctrl Pts',(4.84474814006207,-3.26296002356047,74.7279858805419));
#58082=CARTESIAN_POINT('Ctrl Pts',(5.36902876208054,2.30043969882727,74.8867466427877));
#58083=CARTESIAN_POINT('Ctrl Pts',(0.979410261924092,5.75840674100279,75.0455074050336));
#58084=CARTESIAN_POINT('Ctrl Pts',(-4.30659442642138,3.94610404098849,75.2042681672795));
#58085=CARTESIAN_POINT('Ctrl Pts',(-5.65107234906636,-1.477793612656,75.3630289295254));
#58086=CARTESIAN_POINT('Ctrl Pts',(-1.82351624359326,-5.54916941220397,
75.5217896917713));
#58087=CARTESIAN_POINT('Ctrl Pts',(3.6729776280452,-4.54177586411616,75.6805504540171));
#58088=CARTESIAN_POINT('Ctrl Pts',(5.80785018193428,0.622389685160801,75.8393112162631));
#58089=CARTESIAN_POINT('Ctrl Pts',(2.62720084622344,5.21692518343825,75.9980719785088));
#58090=CARTESIAN_POINT('Ctrl Pts',(-2.95794295284595,5.0367714007783,76.1568327407549));
#58091=CARTESIAN_POINT('Ctrl Pts',(-5.83588700992668,0.246810581940319,
76.3155935030007));
#58092=CARTESIAN_POINT('Ctrl Pts',(-3.37264901603277,-4.76903882041673,
76.4743542652466));
#58093=CARTESIAN_POINT('Ctrl Pts',(2.17734037623983,-5.42011822214095,76.6331150274925));
#58094=CARTESIAN_POINT('Ctrl Pts',(5.73456134845009,-1.110539867295,76.7918757897384));
#58095=CARTESIAN_POINT('Ctrl Pts',(4.04333661010157,4.21543849598137,76.9506365519843));
#58096=CARTESIAN_POINT('Ctrl Pts',(-1.34847329913683,5.68331878549001,77.1093973142302));
#58097=CARTESIAN_POINT('Ctrl Pts',(-5.50611925535187,1.94965212328559,77.2681580764761));
#58098=CARTESIAN_POINT('Ctrl Pts',(-4.62439668246642,-3.56839571504929,
77.4269188387219));
#58099=CARTESIAN_POINT('Ctrl Pts',(0.489714988248199,-5.82053879690483,
77.5856796009679));
#58100=CARTESIAN_POINT('Ctrl Pts',(5.15562454317905,-2.74554698116043,77.7444403632137));
#58101=CARTESIAN_POINT('Ctrl Pts',(5.1029490355901,2.8422532955665,77.9032011254596));
#58102=CARTESIAN_POINT('Ctrl Pts',(0.379898699021361,5.82873653843356,78.0619618877055));
#58103=CARTESIAN_POINT('Ctrl Pts',(-4.69084653104859,3.48058206025056,78.2207226499513));
#58104=CARTESIAN_POINT('Ctrl Pts',(-5.46838573213,-2.05310743523703,78.3794834121973));
#58105=CARTESIAN_POINT('Ctrl Pts',(-1.24109127714898,-5.70773029301263,
78.5382441744431));
#58106=CARTESIAN_POINT('Ctrl Pts',(4.12208782430557,-4.13846404173107,78.6970049366891));
#58107=CARTESIAN_POINT('Ctrl Pts',(5.71260623814347,1.21845091157291,78.8557656989349));
#58108=CARTESIAN_POINT('Ctrl Pts',(2.07477292900298,5.46020237253759,79.0145264611808));
#58109=CARTESIAN_POINT('Ctrl Pts',(-3.46195593952531,4.70460983810283,79.1732872234267));
#58110=CARTESIAN_POINT('Ctrl Pts',(-5.83019698537905,-0.356785324342241,
79.3320479856726));
#58111=CARTESIAN_POINT('Ctrl Pts',(-2.86246366452812,-5.09163965979981,
79.4908087479185));
#58112=CARTESIAN_POINT('Ctrl Pts',(2.72508383719022,-5.16646985244982,79.6495695101644));
#58113=CARTESIAN_POINT('Ctrl Pts',(5.81855137234204,-0.512789024261698,
79.8083302724102));
#58114=CARTESIAN_POINT('Ctrl Pts',(3.58670296156134,4.61021198227599,79.9670910346562));
#58115=CARTESIAN_POINT('Ctrl Pts',(-1.92780555690993,5.51380616187509,80.1258517969019));
#58116=CARTESIAN_POINT('Ctrl Pts',(-5.67792754410753,1.37099652072606,80.2846125591481));
#58117=CARTESIAN_POINT('Ctrl Pts',(-4.23143680838723,-4.02659101382961,
80.4433733213938));
#58118=CARTESIAN_POINT('Ctrl Pts',(1.08779414529793,-5.73891945869655,80.6021340836398));
#58119=CARTESIAN_POINT('Ctrl Pts',(5.41144267008512,-2.19881351740198,80.7608948458856));
#58120=CARTESIAN_POINT('Ctrl Pts',(4.7823735685733,3.3537137186807,80.9196556081314));
#58121=CARTESIAN_POINT('Ctrl Pts',(-0.223669902459649,5.83681971885304,
81.0784163703775));
#58122=CARTESIAN_POINT('Ctrl Pts',(-5.02500384656033,2.97789002445559,81.2371771326232));
#58123=CARTESIAN_POINT('Ctrl Pts',(-5.22730077976831,-2.60649558135874,
81.3959378948693));
#58124=CARTESIAN_POINT('Ctrl Pts',(-0.645412368928784,-5.8053368142863,
81.5546986571149));
#58125=CARTESIAN_POINT('Ctrl Pts',(4.52717715552302,-3.69095646919078,81.713459419361));
#58126=CARTESIAN_POINT('Ctrl Pts',(5.5563558643626,1.80149997964642,81.8722201816067));
#58127=CARTESIAN_POINT('Ctrl Pts',(1.5001879620707,5.64516861688714,82.0309809438528));
#58128=CARTESIAN_POINT('Ctrl Pts',(-3.92899778126385,4.3222065071854,82.1897417060986));
#58129=CARTESIAN_POINT('Ctrl Pts',(-5.76224475326896,-0.956571031279116,
82.3485024683446));
#58130=CARTESIAN_POINT('Ctrl Pts',(-2.32170929618077,-5.35986552417092,
82.5072632305903));
#58131=CARTESIAN_POINT('Ctrl Pts',(3.24372538638481,-4.8576474063222,82.6660239928364));
#58132=CARTESIAN_POINT('Ctrl Pts',(5.8404035909078,0.0904380659057711,82.8247847550821));
#58133=CARTESIAN_POINT('Ctrl Pts',(3.09176588514392,4.95575172494502,82.9835455173283));
#58134=CARTESIAN_POINT('Ctrl Pts',(-2.48655011745873,5.28541028426119,83.1423062795738));
#58135=CARTESIAN_POINT('Ctrl Pts',(-5.78910003705706,0.777699419312094,
83.30106704182));
#58136=CARTESIAN_POINT('Ctrl Pts',(-3.79328774359228,-4.44178477631751,
83.4598278040656));
#58137=CARTESIAN_POINT('Ctrl Pts',(1.67425538991496,-5.59601365552512,83.6185885663117));
#58138=CARTESIAN_POINT('Ctrl Pts',(5.60947262352764,-1.6285964822938,83.7773493285575));
#58139=CARTESIAN_POINT('Ctrl Pts',(4.41072194085603,3.82935538285094,83.9361100908034));
#58140=CARTESIAN_POINT('Ctrl Pts',(-0.8248423466062,5.78257678649102,84.0948708530494));
#58141=CARTESIAN_POINT('Ctrl Pts',(-5.30551223554587,2.44338323992171,84.253631615295));
#58142=CARTESIAN_POINT('Ctrl Pts',(-4.9303644901222,-3.13202323158636,84.4123923775413));
#58143=CARTESIAN_POINT('Ctrl Pts',(-0.0428938145929691,-5.84099457038411,
84.5711531397868));
#58144=CARTESIAN_POINT('Ctrl Pts',(4.88402085037918,-3.20394034224944,84.729913902033));
#58145=CARTESIAN_POINT('Ctrl Pts',(5.3405737125575,2.36513442508082,84.8886746642787));
#58146=CARTESIAN_POINT('Ctrl Pts',(0.90995364228369,5.77018558745976,85.0474354265247));
#58147=CARTESIAN_POINT('Ctrl Pts',(-4.35479260506382,3.89299956501012,85.2061961887705));
#58148=CARTESIAN_POINT('Ctrl Pts',(-5.63139114508318,-1.54490255601334,
85.3649569510165));
#58149=CARTESIAN_POINT('Ctrl Pts',(-1.75878919991609,-5.5732440393258,85.5237177132622));
#58150=CARTESIAN_POINT('Ctrl Pts',(3.73289035077776,-4.49219002151886,85.6824784755083));
#58151=CARTESIAN_POINT('Ctrl Pts',(5.44619302579455,-0.180386406182261,
85.814779110713));
#58152=CARTESIAN_POINT('Ctrl Pts',(4.18934532924144,2.98339184141738,85.9206196188771));
#58153=CARTESIAN_POINT('Ctrl Pts',(2.90742207776985,4.07986902565238,85.973539872959));
#58154=CARTESIAN_POINT('Ctrl Pts',(2.16917135428672,4.4405021828327,86.));
#58155=CARTESIAN_POINT('Ctrl Pts',(2.75898463274055,-3.86904481704483,25.7806068977079));
#58156=CARTESIAN_POINT('Ctrl Pts',(3.40222835107826,-3.41035291299081,25.8070670247489));
#58157=CARTESIAN_POINT('Ctrl Pts',(4.44488144388779,-2.1678284260566,25.8599872788309));
#58158=CARTESIAN_POINT('Ctrl Pts',(5.13713708894935,1.03153993625474,25.9658277869948));
#58159=CARTESIAN_POINT('Ctrl Pts',(2.83087052930385,4.85053885500829,26.0981284221998));
#58160=CARTESIAN_POINT('Ctrl Pts',(-2.54870530784567,5.00827073567408,26.2568891844456));
#58161=CARTESIAN_POINT('Ctrl Pts',(-5.58537388969466,0.575612517731738,
26.4156499466916));
#58162=CARTESIAN_POINT('Ctrl Pts',(-3.51540226351445,-4.38046981539479,
26.5744107089373));
#58163=CARTESIAN_POINT('Ctrl Pts',(1.77471175523205,-5.32917482126994,26.7331714711833));
#58164=CARTESIAN_POINT('Ctrl Pts',(5.43912643226927,-1.39953709723575,26.8919322334291));
#58165=CARTESIAN_POINT('Ctrl Pts',(4.12623242092013,3.81051993270251,27.0506929956751));
#58166=CARTESIAN_POINT('Ctrl Pts',(-0.963505012884285,5.53332322688231,
27.2094537579209));
#58167=CARTESIAN_POINT('Ctrl Pts',(-5.17120987535828,2.19172929477075,27.3682145201668));
#58168=CARTESIAN_POINT('Ctrl Pts',(-4.64617167900849,-3.15573394561846,
27.5269752824127));
#58169=CARTESIAN_POINT('Ctrl Pts',(0.131240194292791,-5.61500874158838,
27.6857360446586));
#58170=CARTESIAN_POINT('Ctrl Pts',(4.78850808778552,-2.93523740776727,27.8444968069045));
#58171=CARTESIAN_POINT('Ctrl Pts',(5.06320222551221,2.43094313930505,28.0032575691504));
#58172=CARTESIAN_POINT('Ctrl Pts',(0.703891137995956,5.57225534640277,28.1620183313963));
#58173=CARTESIAN_POINT('Ctrl Pts',(-4.29963849958627,3.61366660379846,28.3207790936422));
#58174=CARTESIAN_POINT('Ctrl Pts',(-5.36800979937294,-1.65225881189325,
28.4795398558881));
#58175=CARTESIAN_POINT('Ctrl Pts',(-1.52341343958394,-5.40598721644804,
28.638300618134));
#58176=CARTESIAN_POINT('Ctrl Pts',(3.7154568469317,-4.21199061529042,28.7970613803798));
#58177=CARTESIAN_POINT('Ctrl Pts',(5.55382784322941,0.836948256968893,28.9558221426258));
#58178=CARTESIAN_POINT('Ctrl Pts',(2.30916579364752,5.11988662236081,29.1145829048716));
#58179=CARTESIAN_POINT('Ctrl Pts',(-3.04891524119282,4.71694830830577,29.2733436671175));
#58180=CARTESIAN_POINT('Ctrl Pts',(-5.61653596054952,-0.00308515054028371,
29.4321044293634));
#58181=CARTESIAN_POINT('Ctrl Pts',(-3.04373138672984,-4.72029500001125,
29.5908651916093));
#58182=CARTESIAN_POINT('Ctrl Pts',(2.31478911232886,-5.11734667454166,29.7496259538552));
#58183=CARTESIAN_POINT('Ctrl Pts',(5.55474391583396,-0.830846365132238,
29.908386716101));
#58184=CARTESIAN_POINT('Ctrl Pts',(3.71082741246647,4.21606991826224,30.067147478347));
#58185=CARTESIAN_POINT('Ctrl Pts',(-1.52935168579825,5.40431022984286,30.2259082405928));
#58186=CARTESIAN_POINT('Ctrl Pts',(-5.36982140744797,1.64636074283387,30.3846690028388));
#58187=CARTESIAN_POINT('Ctrl Pts',(-4.29566655320965,-3.61838838505691,
30.5434297650846));
#58188=CARTESIAN_POINT('Ctrl Pts',(0.710013543128747,-5.57147793767643,
30.7021905273306));
#58189=CARTESIAN_POINT('Ctrl Pts',(5.06586755727536,-2.42538069880583,30.8609512895764));
#58190=CARTESIAN_POINT('Ctrl Pts',(4.78528484399858,2.94049903987215,31.0197120518223));
#58191=CARTESIAN_POINT('Ctrl Pts',(0.125063273099813,5.61514423852442,31.1784728140682));
#58192=CARTESIAN_POINT('Ctrl Pts',(-4.64962002546522,3.15063791327663,31.3372335763141));
#58193=CARTESIAN_POINT('Ctrl Pts',(-5.16882905222222,-2.19742846769609,
31.49599433856));
#58194=CARTESIAN_POINT('Ctrl Pts',(-0.957367846451143,-5.5343411937037,
31.6547551008058));
#58195=CARTESIAN_POINT('Ctrl Pts',(4.13030565557618,-3.80605581058243,31.8135158630518));
#58196=CARTESIAN_POINT('Ctrl Pts',(5.4377972597899,1.40564810787321,31.9722766252976));
#58197=CARTESIAN_POINT('Ctrl Pts',(1.76845071216457,5.33085994192234,32.1310373875435));
#58198=CARTESIAN_POINT('Ctrl Pts',(-3.51943594526451,4.37710592388724,32.2897981497894));
#58199=CARTESIAN_POINT('Ctrl Pts',(-5.58622732301659,-0.582709136130893,
32.4485589120353));
#58200=CARTESIAN_POINT('Ctrl Pts',(-2.54033282120867,-5.00921099567965,
32.6073196742812));
#58201=CARTESIAN_POINT('Ctrl Pts',(2.83055187404587,-4.8511299436403,32.7660804365271));
#58202=CARTESIAN_POINT('Ctrl Pts',(5.61082903384082,-0.253146587487778,
32.9248411987729));
#58203=CARTESIAN_POINT('Ctrl Pts',(3.25590407686029,4.57652425799672,33.0836019610189));
#58204=CARTESIAN_POINT('Ctrl Pts',(-2.07892374414776,5.217620310809,33.2423627232647));
#58205=CARTESIAN_POINT('Ctrl Pts',(-5.51105705295918,1.08339088088132,33.4011234855107));
#58206=CARTESIAN_POINT('Ctrl Pts',(-3.8993026094728,-4.0423909758343,33.5598842477566));
#58207=CARTESIAN_POINT('Ctrl Pts',(1.28121268795212,-5.46845313502624,33.7186450100024));
#58208=CARTESIAN_POINT('Ctrl Pts',(5.28912299821215,-1.88961994896626,33.8774057722484));
#58209=CARTESIAN_POINT('Ctrl Pts',(4.45626638214284,3.41865113358054,34.0361665344941));
#58210=CARTESIAN_POINT('Ctrl Pts',(-0.455101345292619,5.59806827461589,
34.1949272967401));
#58211=CARTESIAN_POINT('Ctrl Pts',(-4.94994642026466,2.65396233550082,34.353688058986));
#58212=CARTESIAN_POINT('Ctrl Pts',(-4.91444933332838,-2.71913099939964,
34.5124488212319));
#58213=CARTESIAN_POINT('Ctrl Pts',(-0.381098102720512,-5.60359258671175,
34.6712095834778));
#58214=CARTESIAN_POINT('Ctrl Pts',(4.50104575229031,-3.35947507470101,34.8299703457236));
#58215=CARTESIAN_POINT('Ctrl Pts',(5.26369504857235,1.95933664217838,34.9887311079696));
#58216=CARTESIAN_POINT('Ctrl Pts',(1.20884985474224,5.48490361541909,35.1474918702154));
#58217=CARTESIAN_POINT('Ctrl Pts',(-3.95237165094757,3.99051926126589,35.3062526324614));
#58218=CARTESIAN_POINT('Ctrl Pts',(-5.49626189492614,-1.15611021279586,
35.4650133947072));
#58219=CARTESIAN_POINT('Ctrl Pts',(-2.00980536716273,-5.24463230626054,
35.6237741569531));
#58220=CARTESIAN_POINT('Ctrl Pts',(3.31608642293227,-4.53310671365589,35.782534919199));
#58221=CARTESIAN_POINT('Ctrl Pts',(5.60699462758102,0.327256608834102,35.9412956814449));
#58222=CARTESIAN_POINT('Ctrl Pts',(2.76621008118667,4.88810468673588,36.1000564436907));
#58223=CARTESIAN_POINT('Ctrl Pts',(-2.60629442649681,4.97521004623518,36.2588172059367));
#58224=CARTESIAN_POINT('Ctrl Pts',(-5.59343866475058,0.508851201650464,
36.4175779681825));
#58225=CARTESIAN_POINT('Ctrl Pts',(-3.46129698321598,-4.42322380574711,
36.5763387304285));
#58226=CARTESIAN_POINT('Ctrl Pts',(1.83872942405087,-5.30702927699456,36.7350994926743));
#58227=CARTESIAN_POINT('Ctrl Pts',(5.4558944977048,-1.33367944861663,36.8938602549202));
#58228=CARTESIAN_POINT('Ctrl Pts',(4.07965827459196,3.86029454890444,37.0526210171661));
#58229=CARTESIAN_POINT('Ctrl Pts',(-1.03040581621204,5.52120906103586,37.211381779412));
#58230=CARTESIAN_POINT('Ctrl Pts',(-5.1974110298633,2.12894439298054,37.3701425416579));
#58231=CARTESIAN_POINT('Ctrl Pts',(-4.60758691199661,-3.21179521298375,
37.5289033039038));
#58232=CARTESIAN_POINT('Ctrl Pts',(0.199241488304119,-5.61300173446314,
37.6876640661497));
#58233=CARTESIAN_POINT('Ctrl Pts',(4.82371799259843,-2.87701761719148,37.8464248283956));
#58234=CARTESIAN_POINT('Ctrl Pts',(5.03338044768208,2.49210090298119,38.0051855906414));
#58235=CARTESIAN_POINT('Ctrl Pts',(0.636339370439441,5.58037255453223,38.1639463528873));
#58236=CARTESIAN_POINT('Ctrl Pts',(-4.34309893586852,3.56131678947628,38.3227071151332));
#58237=CARTESIAN_POINT('Ctrl Pts',(-5.34760043438529,-1.71716488314614,
38.4814678773791));
#58238=CARTESIAN_POINT('Ctrl Pts',(-1.45781467077047,-5.4240448032289,38.640228639625));
#58239=CARTESIAN_POINT('Ctrl Pts',(3.76620760906239,-4.16667323979076,38.7989894018709));
#58240=CARTESIAN_POINT('Ctrl Pts',(5.54328164477202,0.904164945395139,38.9577501641167));
#58241=CARTESIAN_POINT('Ctrl Pts',(2.2469749974438,5.14748375447756,39.1165109263627));
#58242=CARTESIAN_POINT('Ctrl Pts',(-3.10583180228996,4.67966819952357,39.2752716886085));
#58243=CARTESIAN_POINT('Ctrl Pts',(-5.61608646770029,-0.0711226339607316,
39.4340324508545));
#58244=CARTESIAN_POINT('Ctrl Pts',(-2.98632725227654,-4.75681986037505,
39.5927932131003));
#58245=CARTESIAN_POINT('Ctrl Pts',(2.37660988298438,-5.08893025161958,39.7515539753462));
#58246=CARTESIAN_POINT('Ctrl Pts',(5.56440105884388,-0.763496233183334,
39.9103147375921));
#58247=CARTESIAN_POINT('Ctrl Pts',(3.65948241880601,4.26071285915838,40.069075499838));
#58248=CARTESIAN_POINT('Ctrl Pts',(-1.59470631126904,5.3853873976295,40.2278362620839));
#58249=CARTESIAN_POINT('Ctrl Pts',(-5.38937111433215,1.58119089099016,40.3865970243298));
#58250=CARTESIAN_POINT('Ctrl Pts',(-4.25151885307432,-3.67015981718801,
40.5453577865757));
#58251=CARTESIAN_POINT('Ctrl Pts',(0.777453326851397,-5.56246815418439,
40.7041185488216));
#58252=CARTESIAN_POINT('Ctrl Pts',(5.09487647442165,-2.36383572866916,40.8628793110675));
#58253=CARTESIAN_POINT('Ctrl Pts',(4.74931304757294,2.9982513600266,41.0216400733133));
#58254=CARTESIAN_POINT('Ctrl Pts',(0.0570332499295138,5.61624722124574,
41.1804008355593));
#58255=CARTESIAN_POINT('Ctrl Pts',(-4.6874451201527,3.09408207507567,41.3391615978051));
#58256=CARTESIAN_POINT('Ctrl Pts',(-5.14183053639566,-2.25988149617119,
41.497922360051));
#58257=CARTESIAN_POINT('Ctrl Pts',(-0.89025558647059,-5.5455324931431,41.6566831222969));
#58258=CARTESIAN_POINT('Ctrl Pts',(4.17610846940334,-3.75574276189485,41.8154438845428));
#58259=CARTESIAN_POINT('Ctrl Pts',(5.4203704931852,1.47141746569594,41.9742046467887));
#58260=CARTESIAN_POINT('Ctrl Pts',(1.70374387423147,5.35189148365012,42.1329654090346));
#58261=CARTESIAN_POINT('Ctrl Pts',(-3.57220117995318,4.33415094011377,42.2917261712804));
#58262=CARTESIAN_POINT('Ctrl Pts',(-5.57875859993888,-0.65033693217899,
42.4504869335264));
#58263=CARTESIAN_POINT('Ctrl Pts',(-2.47946574386026,-5.03961657934126,
42.6092476957722));
#58264=CARTESIAN_POINT('Ctrl Pts',(2.88910989726652,-4.81648519599765,42.7680084580182));
#58265=CARTESIAN_POINT('Ctrl Pts',(5.61348391140414,-0.185159439821055,
42.926769220264));
#58266=CARTESIAN_POINT('Ctrl Pts',(3.200225983726,4.61562989144849,43.0855299825099));
#58267=CARTESIAN_POINT('Ctrl Pts',(-2.14197651643363,5.19205375981362,43.2442907447558));
#58268=CARTESIAN_POINT('Ctrl Pts',(-5.52377668122861,1.01655143385025,43.4030515070017));
#58269=CARTESIAN_POINT('Ctrl Pts',(-3.8500477014075,-4.08932981534074,43.5618122692476));
#58270=CARTESIAN_POINT('Ctrl Pts',(1.34736253598006,-5.45253150732624,43.7205730314935));
#58271=CARTESIAN_POINT('Ctrl Pts',(5.31162542471411,-1.82540981406326,43.8793337937394));
#58272=CARTESIAN_POINT('Ctrl Pts',(4.41452647903867,3.47238269889917,44.0380945559852));
#58273=CARTESIAN_POINT('Ctrl Pts',(-0.522881943720034,5.59214450051854,
44.1968553182311));
#58274=CARTESIAN_POINT('Ctrl Pts',(-4.98173283994925,2.59380484098539,44.355616080477));
#58275=CARTESIAN_POINT('Ctrl Pts',(-4.88114967204592,-2.77846423781803,
44.5143768427229));
#58276=CARTESIAN_POINT('Ctrl Pts',(-0.313189227628139,-5.60779797687521,
44.6731376049688));
#58277=CARTESIAN_POINT('Ctrl Pts',(4.54141156440446,-3.30470371507665,44.8318983672147));
#58278=CARTESIAN_POINT('Ctrl Pts',(5.23957377347164,2.02295633024942,44.9906591294605));
#58279=CARTESIAN_POINT('Ctrl Pts',(1.14231802019273,5.49914495012552,45.1494198917065));
#58280=CARTESIAN_POINT('Ctrl Pts',(-4.00042207772478,3.94234813807709,45.3081806539523));
#58281=CARTESIAN_POINT('Ctrl Pts',(-5.48185369562519,-1.22260611053129,
45.4669414161983));
#58282=CARTESIAN_POINT('Ctrl Pts',(-1.94612536588803,-5.26859390179156,
45.6257021784441));
#58283=CARTESIAN_POINT('Ctrl Pts',(3.37075634388315,-4.492603622836,45.7844629406901));
#58284=CARTESIAN_POINT('Ctrl Pts',(5.60261888663935,0.395154720103479,45.9432237029359));
#58285=CARTESIAN_POINT('Ctrl Pts',(2.70679349012103,4.92125539304622,46.1019844651818));
#58286=CARTESIAN_POINT('Ctrl Pts',(-2.66637198863979,4.94327280856975,46.2607452274277));
#58287=CARTESIAN_POINT('Ctrl Pts',(-5.59919237800458,0.441055955456253,
46.4195059896736));
#58288=CARTESIAN_POINT('Ctrl Pts',(-3.40746087346144,-4.46482878032041,
46.5782667519195));
#58289=CARTESIAN_POINT('Ctrl Pts',(1.90288290472123,-5.28436583637694,46.7370275141654));
#58290=CARTESIAN_POINT('Ctrl Pts',(5.47165012418784,-1.26748986592512,46.8957882764113));
#58291=CARTESIAN_POINT('Ctrl Pts',(4.03259601626857,3.90943154580342,47.0545490386571));
#58292=CARTESIAN_POINT('Ctrl Pts',(-1.09721314298891,5.50832179167125,47.2133098009031));
#58293=CARTESIAN_POINT('Ctrl Pts',(-5.22281931897105,2.06582767992164,47.3720705631488));
#58294=CARTESIAN_POINT('Ctrl Pts',(-4.56834172113761,-3.26737502602034,
47.5308313253949));
#58295=CARTESIAN_POINT('Ctrl Pts',(0.267221761695801,-5.61017630487886,
47.6895920876407));
#58296=CARTESIAN_POINT('Ctrl Pts',(4.85821572583019,-2.81837286444571,47.8483528498866));
#58297=CARTESIAN_POINT('Ctrl Pts',(5.00282226155327,2.5528915098482,48.0071136121325));
#58298=CARTESIAN_POINT('Ctrl Pts',(0.568693050307066,5.58767159524255,48.1658743743783));
#58299=CARTESIAN_POINT('Ctrl Pts',(-4.38592141153559,3.50844395901968,48.3246351366243));
#58300=CARTESIAN_POINT('Ctrl Pts',(-5.32640662782695,-1.78181875531413,
48.4833958988701));
#58301=CARTESIAN_POINT('Ctrl Pts',(-1.39200180112221,-5.44130651842186,
48.6421566611161));
#58302=CARTESIAN_POINT('Ctrl Pts',(3.81640559321821,-4.12074434899823,48.8009174233619));
#58303=CARTESIAN_POINT('Ctrl Pts',(5.53192201501862,0.971248918403669,48.9596781856079));
#58304=CARTESIAN_POINT('Ctrl Pts',(2.18445443391585,5.17432550849803,49.1184389478537));
#58305=CARTESIAN_POINT('Ctrl Pts',(-3.16229257013621,4.64170134138436,49.2771997100997));
#58306=CARTESIAN_POINT('Ctrl Pts',(-5.61481282051529,-0.139149675977844,
49.4359604723455));
#58307=CARTESIAN_POINT('Ctrl Pts',(-2.92848487086811,-4.79264665950293,
49.5947212345914));
#58308=CARTESIAN_POINT('Ctrl Pts',(2.43808188433272,-5.05976702695259,49.7534819968373));
#58309=CARTESIAN_POINT('Ctrl Pts',(5.57324162681136,-0.696034058739029,
49.9122427590832));
#58310=CARTESIAN_POINT('Ctrl Pts',(3.60760039555022,4.30473054066965,50.0710035213291));
#58311=CARTESIAN_POINT('Ctrl Pts',(-1.65982691330743,5.36567425955101,50.229764283575));
#58312=CARTESIAN_POINT('Ctrl Pts',(-5.40812993103286,1.515788999437,50.3885250458208));
#58313=CARTESIAN_POINT('Ctrl Pts',(-4.20674724239739,-3.7213926533396,50.5472858080668));
#58314=CARTESIAN_POINT('Ctrl Pts',(0.844779019247828,-5.55264207836113,
50.7060465703126));
#58315=CARTESIAN_POINT('Ctrl Pts',(5.12313771836632,-2.30194386560584,50.8648073325585));
#58316=CARTESIAN_POINT('Ctrl Pts',(4.71264428935673,3.05556368674283,51.0235680948044));
#58317=CARTESIAN_POINT('Ctrl Pts',(-0.0110051428662697,5.61652601957635,
51.1823288570503));
#58318=CARTESIAN_POINT('Ctrl Pts',(-4.7245823321816,3.03707218027256,51.3410896192961));
#58319=CARTESIAN_POINT('Ctrl Pts',(-5.11407745683792,-2.32200288699436,
51.4998503815421));
#58320=CARTESIAN_POINT('Ctrl Pts',(-0.82301268146625,-5.55590998558236,
51.6586111437879));
#58321=CARTESIAN_POINT('Ctrl Pts',(4.22129843923301,-3.70487855788512,51.8173719060339));
#58322=CARTESIAN_POINT('Ctrl Pts',(5.40214828710646,1.53697089297761,51.9761326682797));
#58323=CARTESIAN_POINT('Ctrl Pts',(1.63878701185215,5.37213763520004,52.1348934305256));
#58324=CARTESIAN_POINT('Ctrl Pts',(-3.62444219405034,4.29055991960671,52.2936541927716));
#58325=CARTESIAN_POINT('Ctrl Pts',(-5.57047119392959,-0.717869291269865,
52.4524149550173));
#58326=CARTESIAN_POINT('Ctrl Pts',(-2.41823480486641,-5.06928259917325,
52.6111757172634));
#58327=CARTESIAN_POINT('Ctrl Pts',(2.94724394355444,-4.78113362906013,52.7699364795091));
#58328=CARTESIAN_POINT('Ctrl Pts',(5.6153150100958,-0.117145120002924,52.9286972417552));
#58329=CARTESIAN_POINT('Ctrl Pts',(3.14407825736721,4.65405818112524,53.0874580040009));
#58330=CARTESIAN_POINT('Ctrl Pts',(-2.20471495362471,5.16572527482943,53.2462187662469));
#58331=CARTESIAN_POINT('Ctrl Pts',(-5.53568569516419,0.949562807876645,
53.4049795284926));
#58332=CARTESIAN_POINT('Ctrl Pts',(-3.80022779876814,-4.13566854561846,
53.5637402907387));
#58333=CARTESIAN_POINT('Ctrl Pts',(1.41331465853004,-5.43580972052295,53.7225010529844));
#58334=CARTESIAN_POINT('Ctrl Pts',(5.33334837008319,-1.76093180023503,53.8812618152305));
#58335=CARTESIAN_POINT('Ctrl Pts',(4.37213874408905,3.52560469199021,54.0400225774763));
#58336=CARTESIAN_POINT('Ctrl Pts',(-0.590585809212258,5.58540007910849,
54.1987833397222));
#58337=CARTESIAN_POINT('Ctrl Pts',(-5.01278819024406,2.53326670555979,54.3575441019681));
#58338=CARTESIAN_POINT('Ctrl Pts',(-4.8471337019555,-2.83738973655626,54.516304864214));
#58339=CARTESIAN_POINT('Ctrl Pts',(-0.245234392010581,-5.61118042257805,
54.6750656264598));
#58340=CARTESIAN_POINT('Ctrl Pts',(4.58111092428449,-3.2494473901187,54.8338263887058));
#58341=CARTESIAN_POINT('Ctrl Pts',(5.21468359081919,2.08627914944017,54.9925871509516));
#58342=CARTESIAN_POINT('Ctrl Pts',(1.07561855045193,5.51257928520504,55.1513479131975));
#58343=CARTESIAN_POINT('Ctrl Pts',(-4.04788544248539,3.89359847522351,55.3101086754434));
#58344=CARTESIAN_POINT('Ctrl Pts',(-5.46664103418928,-1.28892259079655,
55.4688694376893));
#58345=CARTESIAN_POINT('Ctrl Pts',(-1.88215977067859,-5.29178233106645,
55.6276301999352));
#58346=CARTESIAN_POINT('Ctrl Pts',(3.42493160627594,-4.45144124234838,55.7863909621811));
#58347=CARTESIAN_POINT('Ctrl Pts',(5.59742096126865,0.46299484241015,55.9451517244269));
#58348=CARTESIAN_POINT('Ctrl Pts',(2.64697967705877,4.95368390503328,56.1039124866729));
#58349=CARTESIAN_POINT('Ctrl Pts',(-2.72605826064226,4.91061014552488,56.2626732489187));
#58350=CARTESIAN_POINT('Ctrl Pts',(-5.60412440966974,0.373195984292183,
56.4214340111647));
#58351=CARTESIAN_POINT('Ctrl Pts',(-3.35312471875849,-4.5057785411845,56.5801947734105));
#58352=CARTESIAN_POINT('Ctrl Pts',(1.96675713728871,-5.26092691497154,56.7389555356564));
#58353=CARTESIAN_POINT('Ctrl Pts',(5.48660278591027,-1.20111427907158,56.8977162979024));
#58354=CARTESIAN_POINT('Ctrl Pts',(3.9849419744025,3.95799483354801,57.0564770601482));
#58355=CARTESIAN_POINT('Ctrl Pts',(-1.1638594537159,5.49462617597814,57.2152378223941));
#58356=CARTESIAN_POINT('Ctrl Pts',(-5.24746115924365,2.00240780661117,57.37399858464));
#58357=CARTESIAN_POINT('Ctrl Pts',(-4.52842612604344,-3.32247535170916,
57.5327593468859));
#58358=CARTESIAN_POINT('Ctrl Pts',(0.335162820288752,-5.60652758181426,
57.6915201091317));
#58359=CARTESIAN_POINT('Ctrl Pts',(4.89200051581106,-2.75931451542811,57.8502808713777));
#58360=CARTESIAN_POINT('Ctrl Pts',(4.97152991116165,2.61330747983713,58.0090416336235));
#58361=CARTESIAN_POINT('Ctrl Pts',(0.500963274458718,5.59415064503912,58.1678023958695));
#58362=CARTESIAN_POINT('Ctrl Pts',(-4.42810025315133,3.45505626434493,58.3265631581152));
#58363=CARTESIAN_POINT('Ctrl Pts',(-5.30443117099388,-1.84621114554552,
58.4853239203613));
#58364=CARTESIAN_POINT('Ctrl Pts',(-1.325984655183,-5.45776972177896,58.644084682607));
#58365=CARTESIAN_POINT('Ctrl Pts',(3.86604351978,-4.07421073889346,58.802845444853));
#58366=CARTESIAN_POINT('Ctrl Pts',(5.51975057560345,1.03819036061473,58.9616062070988));
#58367=CARTESIAN_POINT('Ctrl Pts',(2.12161330165796,5.20040793015086,59.1203669693448));
#58368=CARTESIAN_POINT('Ctrl Pts',(-3.21828927148705,4.60305331348437,59.2791277315906));
#58369=CARTESIAN_POINT('Ctrl Pts',(-5.61271519944128,-0.207156297777243,
59.4378884938366));
#58370=CARTESIAN_POINT('Ctrl Pts',(-2.8702127342488,-4.82777013764157,59.5966492560824));
#58371=CARTESIAN_POINT('Ctrl Pts',(2.49919609711769,-5.02986128137743,59.7554100183283));
#58372=CARTESIAN_POINT('Ctrl Pts',(5.58126432146331,-0.6284697412833,59.9141707805742));
#58373=CARTESIAN_POINT('Ctrl Pts',(3.55518895686721,4.34811650289146,60.0729315428202));
#58374=CARTESIAN_POINT('Ctrl Pts',(-1.72470393571439,5.34517370867209,60.2316923050659));
#58375=CARTESIAN_POINT('Ctrl Pts',(-5.42609510456254,1.45016466581917,60.3904530673119));
#58376=CARTESIAN_POINT('Ctrl Pts',(-4.161358291482,-3.7720793750479,60.5492138295578));
#58377=CARTESIAN_POINT('Ctrl Pts',(0.911980740306919,-5.54200115220642,
60.7079745918037));
#58378=CARTESIAN_POINT('Ctrl Pts',(5.15064714175253,-2.23971419223624,60.8667353540495));
#58379=CARTESIAN_POINT('Ctrl Pts',(4.67528395050075,3.11242760942936,61.0254961162954));
#58380=CARTESIAN_POINT('Ctrl Pts',(-0.0790419206570804,5.61598059260596,
61.1842568785413));
#58381=CARTESIAN_POINT('Ctrl Pts',(-4.76102621166261,2.97961659506878,61.3430176407873));
#58382=CARTESIAN_POINT('Ctrl Pts',(-5.08557388631535,-2.38378352384928,
61.5017784030331));
#58383=CARTESIAN_POINT('Ctrl Pts',(-0.75564899933528,-5.56547214812468,
61.660539165279));
#58384=CARTESIAN_POINT('Ctrl Pts',(4.26586893343571,-3.65347066287608,61.8192999275249));
#58385=CARTESIAN_POINT('Ctrl Pts',(5.38313331566308,1.60229876975119,61.9780606897708));
#58386=CARTESIAN_POINT('Ctrl Pts',(1.5735896574475,5.39159542544895,62.1368214520167));
#58387=CARTESIAN_POINT('Ctrl Pts',(-3.67615132118597,4.24633925934925,62.2955822142625));
#58388=CARTESIAN_POINT('Ctrl Pts',(-5.56136632116585,-0.785296303028447,
62.4543429765086));
#58389=CARTESIAN_POINT('Ctrl Pts',(-2.3566489898686,-5.09820470168657,62.6131037387542));
#58390=CARTESIAN_POINT('Ctrl Pts',(3.00494548173707,-4.7450804306709,62.7718645010003));
#58391=CARTESIAN_POINT('Ctrl Pts',(5.61632206120212,-0.0491136091362308,
62.930625263246));
#58392=CARTESIAN_POINT('Ctrl Pts',(3.08746913746389,4.69180348767462,63.0893860254921));
#58393=CARTESIAN_POINT('Ctrl Pts',(-2.26712984885402,5.13863871956213,63.2481467877378));
#58394=CARTESIAN_POINT('Ctrl Pts',(-5.54678234711784,0.882434833542929,
63.4069075499838));
#58395=CARTESIAN_POINT('Ctrl Pts',(-3.74985021262651,-4.18140036645774,
63.5656683122296));
#58396=CARTESIAN_POINT('Ctrl Pts',(1.47905937712676,-5.41829022853902,63.7244290744757));
#58397=CARTESIAN_POINT('Ctrl Pts',(5.35428864647665,-1.69619536963139,63.8831898367214));
#58398=CARTESIAN_POINT('Ctrl Pts',(4.32910939769494,3.57830930252506,64.0419505989674));
#58399=CARTESIAN_POINT('Ctrl Pts',(-0.658203006225538,5.57783600012977,
64.2007113612132));
#58400=CARTESIAN_POINT('Ctrl Pts',(-5.04310791377582,2.47235681319663,64.3594721234592));
#58401=CARTESIAN_POINT('Ctrl Pts',(-4.81240641490144,-2.89589884829624,
64.518232885705));
#58402=CARTESIAN_POINT('Ctrl Pts',(-0.177243568241342,-5.61373942744627,
64.676993647951));
#58403=CARTESIAN_POINT('Ctrl Pts',(4.62013800604848,-3.19371420869404,64.8357544101967));
#58404=CARTESIAN_POINT('Ctrl Pts',(5.18902815324987,2.14929580712564,64.9945151724427));
#58405=CARTESIAN_POINT('Ctrl Pts',(1.00876123366836,5.52520464916871,65.1532759346885));
#58406=CARTESIAN_POINT('Ctrl Pts',(-4.09475477997962,3.84427742671915,65.3120366969346));
#58407=CARTESIAN_POINT('Ctrl Pts',(-5.45062614307688,-1.35504992164687,
65.4707974591803));
#58408=CARTESIAN_POINT('Ctrl Pts',(-1.81791796848671,-5.31419419118279,
65.6295582214263));
#58409=CARTESIAN_POINT('Ctrl Pts',(3.47860425988976,-4.40962561277309,65.7883189836721));
#58410=CARTESIAN_POINT('Ctrl Pts',(5.59140161426455,0.530767020214592,65.947079745918));
#58411=CARTESIAN_POINT('Ctrl Pts',(2.58677741967834,4.98538546381227,66.1058405081639));
#58412=CARTESIAN_POINT('Ctrl Pts',(-2.78534448354271,4.87722685034708,66.2646012704098));
#58413=CARTESIAN_POINT('Ctrl Pts',(-5.6082340359703,0.305281246610254,66.4233620326558));
#58414=CARTESIAN_POINT('Ctrl Pts',(-3.29829649293878,-4.54606707896127,
66.5821227949015));
#58415=CARTESIAN_POINT('Ctrl Pts',(2.03034274820855,-5.23671595244054,66.7408835571475));
#58416=CARTESIAN_POINT('Ctrl Pts',(5.50075028856868,-1.13456242867458,66.8996443193933));
#58417=CARTESIAN_POINT('Ctrl Pts',(3.93670314222528,4.00597728547496,67.0584050816393));
#58418=CARTESIAN_POINT('Ctrl Pts',(-1.23033496804577,5.48012422378831,67.2171658438851));
#58419=CARTESIAN_POINT('Ctrl Pts',(-5.27133293449043,1.93869407991674,67.375926606131));
#58420=CARTESIAN_POINT('Ctrl Pts',(-4.48784598432852,-3.37708810407645,
67.534687368377));
#58421=CARTESIAN_POINT('Ctrl Pts',(0.403054693731489,-5.60205610071956,
67.6934481306228));
#58422=CARTESIAN_POINT('Ctrl Pts',(4.92506740462245,-2.69985123695237,67.8522088928687));
#58423=CARTESIAN_POINT('Ctrl Pts',(4.93950798866025,2.67333994690335,68.0109696551146));
#58424=CARTESIAN_POINT('Ctrl Pts',(0.433159982240225,5.59980875312125,68.1697304173605));
#58425=CARTESIAN_POINT('Ctrl Pts',(-4.46962927096998,3.40116154009715,68.3284911796064));
#58426=CARTESIAN_POINT('Ctrl Pts',(-5.28167728878481,-1.91033260425587,
68.4872519418522));
#58427=CARTESIAN_POINT('Ctrl Pts',(-1.25977292097022,-5.47343199732475,
68.6460127040982));
#58428=CARTESIAN_POINT('Ctrl Pts',(3.9151141043812,-4.02707923828464,68.804773466344));
#58429=CARTESIAN_POINT('Ctrl Pts',(5.50676911268545,1.10497944837047,68.96353422859));
#58430=CARTESIAN_POINT('Ctrl Pts',(2.05846082260739,5.22572719184021,69.1222949908358));
#58431=CARTESIAN_POINT('Ctrl Pts',(-3.27381368882556,4.56372978742243,69.2810557530818));
#58432=CARTESIAN_POINT('Ctrl Pts',(-5.60979391230414,-0.27513251938597,
69.4398165153275));
#58433=CARTESIAN_POINT('Ctrl Pts',(-2.81151939385567,-4.86218514042,69.5985772775736));
#58434=CARTESIAN_POINT('Ctrl Pts',(2.55994355282749,-4.99921740356275,69.7573380398193));
#58435=CARTESIAN_POINT('Ctrl Pts',(5.58846796546901,-0.560813195881055,
69.9160988020653));
#58436=CARTESIAN_POINT('Ctrl Pts',(3.50225579413674,4.39086437893307,70.074859564311));
#58437=CARTESIAN_POINT('Ctrl Pts',(-1.78932785778569,5.32388875344897,70.2336203265571));
#58438=CARTESIAN_POINT('Ctrl Pts',(-5.4432639985316,1.38432752050883,70.3923810888029));
#58439=CARTESIAN_POINT('Ctrl Pts',(-4.11535866115752,-3.82221254403565,
70.5511418510488));
#58440=CARTESIAN_POINT('Ctrl Pts',(0.979048628174891,-5.53054693727633,
70.7099026132948));
#58441=CARTESIAN_POINT('Ctrl Pts',(5.17740070757192,-2.17715584076599,70.8686633755405));
#58442=CARTESIAN_POINT('Ctrl Pts',(4.63723751363544,3.16883478330451,71.0274241377865));
#58443=CARTESIAN_POINT('Ctrl Pts',(-0.14706709904452,5.61461102037593,71.1861849000324));
#58444=CARTESIAN_POINT('Ctrl Pts',(-4.79677141045583,2.92172375107252,71.3449456622783));
#58445=CARTESIAN_POINT('Ctrl Pts',(-5.05632400772744,-2.44521434042637,
71.5037064245242));
#58446=CARTESIAN_POINT('Ctrl Pts',(-0.688174425699173,-5.57421757752254,
71.6624671867701));
#58447=CARTESIAN_POINT('Ctrl Pts',(4.30981341129062,-3.60152662097726,71.8212279490159));
#58448=CARTESIAN_POINT('Ctrl Pts',(5.36332836930242,1.66739150914959,71.9799887112618));
#58449=CARTESIAN_POINT('Ctrl Pts',(1.50816137873041,5.41026199896583,72.1387494735078));
#58450=CARTESIAN_POINT('Ctrl Pts',(-3.72732097304471,4.20149544872403,72.2975102357535));
#58451=CARTESIAN_POINT('Ctrl Pts',(-5.55144531778782,-0.85260807253943,
72.4562709979996));
#58452=CARTESIAN_POINT('Ctrl Pts',(-2.29471733658639,-5.12637864256223,
72.6150317602453));
#58453=CARTESIAN_POINT('Ctrl Pts',(3.06220604411272,-4.70833089163749,72.7737925224914));
#58454=CARTESIAN_POINT('Ctrl Pts',(5.61650491693822,0.0189251091536447,
72.9325532847371));
#58455=CARTESIAN_POINT('Ctrl Pts',(3.03040693140542,4.72886027197227,73.0913140469831));
#58456=CARTESIAN_POINT('Ctrl Pts',(-2.32921204273454,5.11079806896419,73.2500748092289));
#58457=CARTESIAN_POINT('Ctrl Pts',(-5.55706500865567,0.815177361880478,
73.4088355714748));
#58458=CARTESIAN_POINT('Ctrl Pts',(-3.69892233589434,-4.22651856671307,
73.5675963337208));
#58459=CARTESIAN_POINT('Ctrl Pts',(1.54458704373152,-5.39997560236016,73.7263570959665));
#58460=CARTESIAN_POINT('Ctrl Pts',(5.37444318090863,-1.63121002232468,73.8851178582126));
#58461=CARTESIAN_POINT('Ctrl Pts',(4.28544475441368,3.63048879610115,74.0438786204583));
#58462=CARTESIAN_POINT('Ctrl Pts',(-0.725723611935015,5.56945337361106,
74.2026393827042));
#58463=CARTESIAN_POINT('Ctrl Pts',(-5.07268756112454,2.41108410242379,74.3614001449502));
#58464=CARTESIAN_POINT('Ctrl Pts',(-4.77697290711372,-2.9539829868247,74.5201609071961));
#58465=CARTESIAN_POINT('Ctrl Pts',(-0.109226733975009,-5.61547461594591,
74.6789216694419));
#58466=CARTESIAN_POINT('Ctrl Pts',(4.65848708247156,-3.13751234964793,74.8376824316879));
#58467=CARTESIAN_POINT('Ctrl Pts',(5.16261122569953,2.21199705561036,74.9964431939337));
#58468=CARTESIAN_POINT('Ctrl Pts',(0.94175588115421,5.53701918924425,75.1552039561797));
#58469=CARTESIAN_POINT('Ctrl Pts',(-4.14102321213148,3.79439223042856,75.3139647184255));
#58470=CARTESIAN_POINT('Ctrl Pts',(-5.43381137247341,-1.42097839889528,
75.4727254806715));
#58471=CARTESIAN_POINT('Ctrl Pts',(-1.75340938679805,-5.33582619319972,
75.6314862429172));
#58472=CARTESIAN_POINT('Ctrl Pts',(3.53176642826186,-4.36716287055454,75.7902470051633));
#58473=CARTESIAN_POINT('Ctrl Pts',(5.58456172896637,0.598461307948863,75.949007767409));
#58474=CARTESIAN_POINT('Ctrl Pts',(2.52619555266178,5.0163554171789,76.107768529655));
#58475=CARTESIAN_POINT('Ctrl Pts',(-2.84422195708685,4.8431278220354,76.2665292919008));
#58476=CARTESIAN_POINT('Ctrl Pts',(-5.61152065381861,0.23732170889948,76.4252900541468));
#58477=CARTESIAN_POINT('Ctrl Pts',(-3.24298424204541,-4.58568848130712,
76.5840508163926));
#58478=CARTESIAN_POINT('Ctrl Pts',(2.09363040629115,-5.21173650174305,76.7428115786384));
#58479=CARTESIAN_POINT('Ctrl Pts',(5.51409055601673,-1.06784408121947,76.9015723408844));
#58480=CARTESIAN_POINT('Ctrl Pts',(3.88788659878658,4.05337186015841,77.0603331031303));
#58481=CARTESIAN_POINT('Ctrl Pts',(-1.29662993069554,5.46481806326361,77.2190938653762));
#58482=CARTESIAN_POINT('Ctrl Pts',(-5.29443114152808,1.8746958498288,77.377854627622));
#58483=CARTESIAN_POINT('Ctrl Pts',(-4.44660725112929,-3.43120526869962,
77.5366153898679));
#58484=CARTESIAN_POINT('Ctrl Pts',(0.470887418890042,-5.59676251778467,
77.6953761521139));
#58485=CARTESIAN_POINT('Ctrl Pts',(4.95741153969778,-2.63999175525599,77.8541369143597));
#58486=CARTESIAN_POINT('Ctrl Pts',(4.90676119326682,2.73298010128111,78.0128976766056));
#58487=CARTESIAN_POINT('Ctrl Pts',(0.365293123785983,5.60464508916152,78.1716584388516));
#58488=CARTESIAN_POINT('Ctrl Pts',(-4.51050237060752,3.34676769532807,78.3304192010974));
#58489=CARTESIAN_POINT('Ctrl Pts',(-5.25814832033228,-1.9741737216199,78.4891799633432));
#58490=CARTESIAN_POINT('Ctrl Pts',(-1.19337631505721,-5.48829104661996,
78.6479407255893));
#58491=CARTESIAN_POINT('Ctrl Pts',(3.96361014591247,-3.97935676372049,78.806701487835));
#58492=CARTESIAN_POINT('Ctrl Pts',(5.49297953129461,1.17160638037103,78.9654622500811));
#58493=CARTESIAN_POINT('Ctrl Pts',(1.99500626439154,5.25027957796405,79.1242230123267));
#58494=CARTESIAN_POINT('Ctrl Pts',(-3.32885767394246,4.52373653392658,79.2829837745728));
#58495=CARTESIAN_POINT('Ctrl Pts',(-5.60604938780277,-0.34306836529208,
79.4417445368186));
#58496=CARTESIAN_POINT('Ctrl Pts',(-2.75241346293775,-4.89588661743591,
79.6005052990645));
#58497=CARTESIAN_POINT('Ctrl Pts',(2.62031533677199,-4.96783989049817,79.7592660613105));
#58498=CARTESIAN_POINT('Ctrl Pts',(5.59485150169351,-0.493074351131619,
79.9180268235562));
#58499=CARTESIAN_POINT('Ctrl Pts',(3.44880867530152,4.43296789554331,80.0767875858023));
#58500=CARTESIAN_POINT('Ctrl Pts',(-1.85368919596017,5.30182251744854,80.235548348048));
#58501=CARTESIAN_POINT('Ctrl Pts',(-5.45963409340325,1.31828722510949,80.3943091102941));
#58502=CARTESIAN_POINT('Ctrl Pts',(-4.06875510187306,-3.87178480326137,
80.5530698725397));
#58503=CARTESIAN_POINT('Ctrl Pts',(1.04597284064243,-5.51828111447312,80.7118306347859));
#58504=CARTESIAN_POINT('Ctrl Pts',(5.20339448972971,-2.11427799164205,80.8705913970315));
#58505=CARTESIAN_POINT('Ctrl Pts',(4.59851056209243,3.2247769306293,81.0293521592777));
#58506=CARTESIAN_POINT('Ctrl Pts',(-0.215070695363695,5.6124175038425,81.1881129215234));
#58507=CARTESIAN_POINT('Ctrl Pts',(-4.8318126828924,2.86340214411448,81.3468736837694));
#58508=CARTESIAN_POINT('Ctrl Pts',(-5.02633211360974,-2.50628632185673,
81.5056344460153));
#58509=CARTESIAN_POINT('Ctrl Pts',(-0.62059886223198,-5.58214499018382,
81.664395208261));
#58510=CARTESIAN_POINT('Ctrl Pts',(4.35312542352183,-3.54905405536124,81.823155970507));
#58511=CARTESIAN_POINT('Ctrl Pts',(5.34273635521072,1.73223955954653,81.9819167327528));
#58512=CARTESIAN_POINT('Ctrl Pts',(1.44251177575087,5.42813461502377,82.1406774949988));
#58513=CARTESIAN_POINT('Ctrl Pts',(-3.77794363750813,4.15603507125568,82.2994382572446));
#58514=CARTESIAN_POINT('Ctrl Pts',(-5.54070964539341,-0.919794726960242,
82.4581990194906));
#58515=CARTESIAN_POINT('Ctrl Pts',(-2.23244892259243,-5.15380027738969,
82.6169597817364));
#58516=CARTESIAN_POINT('Ctrl Pts',(3.11901720681907,-4.6708904238858,82.7757205439823));
#58517=CARTESIAN_POINT('Ctrl Pts',(5.61586359044797,0.0869610864393738,
82.9344813062282));
#58518=CARTESIAN_POINT('Ctrl Pts',(2.97289993650437,4.765223026495,83.0932420684742));
#58519=CARTESIAN_POINT('Ctrl Pts',(-2.39095227805809,5.08220754164499,83.2520028307198));
#58520=CARTESIAN_POINT('Ctrl Pts',(-5.56653245165825,0.747800008209614,
83.4107635929661));
#58521=CARTESIAN_POINT('Ctrl Pts',(-3.64745110432035,-4.27101603744643,
83.5695243552116));
#58522=CARTESIAN_POINT('Ctrl Pts',(1.60988701191321,-5.38086946399345,83.7282851174578));
#58523=CARTESIAN_POINT('Ctrl Pts',(5.39381098887153,-1.56598350543525,83.8870458797035));
#58524=CARTESIAN_POINT('Ctrl Pts',(4.24114744292764,3.68213208808317,84.0458066419495));
#58525=CARTESIAN_POINT('Ctrl Pts',(-0.793130479779808,5.56025999380927,
84.2045674041954));
#58526=CARTESIAN_POINT('Ctrl Pts',(-5.10153665384735,2.3494449931422,84.3633281664411));
#58527=CARTESIAN_POINT('Ctrl Pts',(-4.74081182862427,-3.01160955008047,
84.5220889286872));
#58528=CARTESIAN_POINT('Ctrl Pts',(-0.0412447201429887,-5.61643184914312,
84.680849690933));
#58529=CARTESIAN_POINT('Ctrl Pts',(4.6962499152168,-3.08076173742818,84.8396104531789));
#58530=CARTESIAN_POINT('Ctrl Pts',(5.13525015825041,2.27420453014635,84.9983712154247));
#58531=CARTESIAN_POINT('Ctrl Pts',(0.874969588857335,5.54834518648496,85.1571319776707));
#58532=CARTESIAN_POINT('Ctrl Pts',(-4.1873683648852,3.74332940771524,85.3158927399165));
#58533=CARTESIAN_POINT('Ctrl Pts',(-5.41488683153288,-1.48550727360877,
85.4746535021625));
#58534=CARTESIAN_POINT('Ctrl Pts',(-1.69117083731324,-5.35897524785026,
85.6334142644083));
#58535=CARTESIAN_POINT('Ctrl Pts',(3.58937574805651,-4.3194834039373,85.7921750266543));
#58536=CARTESIAN_POINT('Ctrl Pts',(5.23680883419176,-0.173451275228434,
85.9244756618591));
#58537=CARTESIAN_POINT('Ctrl Pts',(4.02828187061023,2.86869243836803,86.0303161700231));
#58538=CARTESIAN_POINT('Ctrl Pts',(2.79564340622479,3.92301449006468,86.083236424105));
#58539=CARTESIAN_POINT('Ctrl Pts',(2.08577545033815,4.26978275451652,86.109696551146));
#58540=CARTESIAN_POINT('Ctrl Pts',(2.64867169498355,-3.71434815979776,25.890303448854));
#58541=CARTESIAN_POINT('Ctrl Pts',(3.26619649360659,-3.27399620981999,25.916763575895));
#58542=CARTESIAN_POINT('Ctrl Pts',(4.26716101578614,-2.08115178444252,25.9696838299769));
#58543=CARTESIAN_POINT('Ctrl Pts',(4.93173808918078,0.990295704796579,26.0755243381408));
#58544=CARTESIAN_POINT('Ctrl Pts',(2.71768336588486,4.65659895971115,26.2078249733458));
#58545=CARTESIAN_POINT('Ctrl Pts',(-2.44680000302844,4.80802422056935,26.3665857355916));
#58546=CARTESIAN_POINT('Ctrl Pts',(-5.36205296397033,0.552597707469077,
26.5253464978375));
#58547=CARTESIAN_POINT('Ctrl Pts',(-3.3748453548303,-4.20532476806197,26.6841072600834));
#58548=CARTESIAN_POINT('Ctrl Pts',(1.70375316232487,-5.11609754516703,26.8428680223293));
#58549=CARTESIAN_POINT('Ctrl Pts',(5.22165294276351,-1.34357917457709,27.0016287845752));
#58550=CARTESIAN_POINT('Ctrl Pts',(3.96125258927572,3.65816328556149,27.1603895468211));
#58551=CARTESIAN_POINT('Ctrl Pts',(-0.924981032991848,5.31208345139673,
27.319150309067));
#58552=CARTESIAN_POINT('Ctrl Pts',(-4.96444853774918,2.10409702077966,27.4779110713129));
#58553=CARTESIAN_POINT('Ctrl Pts',(-4.46040303022669,-3.02955771462767,
27.6366718335588));
#58554=CARTESIAN_POINT('Ctrl Pts',(0.125992795951784,-5.39050292069155,
27.7954325958046));
#58555=CARTESIAN_POINT('Ctrl Pts',(4.59704837888827,-2.8178773262279,27.9541933580506));
#58556=CARTESIAN_POINT('Ctrl Pts',(4.86075937558651,2.33374633870135,28.1129541202964));
#58557=CARTESIAN_POINT('Ctrl Pts',(0.67574734249545,5.34945894155921,28.2717148825423));
#58558=CARTESIAN_POINT('Ctrl Pts',(-4.12772534408922,3.46918077578477,28.4304756447882));
#58559=CARTESIAN_POINT('Ctrl Pts',(-5.15337977793343,-1.58619627522226,
28.5892364070341));
#58560=CARTESIAN_POINT('Ctrl Pts',(-1.46250254869165,-5.18983873767588,
28.74799716928));
#58561=CARTESIAN_POINT('Ctrl Pts',(3.56690112283287,-4.04358189961183,28.9067579315259));
#58562=CARTESIAN_POINT('Ctrl Pts',(5.3317682282855,0.803484416727951,29.0655186937718));
#58563=CARTESIAN_POINT('Ctrl Pts',(2.2168380367468,4.91517735084379,29.2242794560177));
#58564=CARTESIAN_POINT('Ctrl Pts',(-2.92700996008437,4.52834978587781,29.3830402182635));
#58565=CARTESIAN_POINT('Ctrl Pts',(-5.39196907660498,-0.00296179645705061,
29.5418009805095));
#58566=CARTESIAN_POINT('Ctrl Pts',(-2.92203337252994,-4.5315626662565,29.7005617427553));
#58567=CARTESIAN_POINT('Ctrl Pts',(2.22223651734922,-4.91273895817748,29.8593225050013));
#58568=CARTESIAN_POINT('Ctrl Pts',(5.33264767340791,-0.797626497839672,
30.0180832672471));
#58569=CARTESIAN_POINT('Ctrl Pts',(3.56245678780991,4.04749809913968,30.176844029493));
#58570=CARTESIAN_POINT('Ctrl Pts',(-1.46820336502753,5.18822880230289,30.3356047917389));
#58571=CARTESIAN_POINT('Ctrl Pts',(-5.15511895218379,1.58053402963151,30.4943655539848));
#58572=CARTESIAN_POINT('Ctrl Pts',(-4.12391220870013,-3.47371376528387,
30.6531263162307));
#58573=CARTESIAN_POINT('Ctrl Pts',(0.681624954493375,-5.34871261609428,
30.8118870784765));
#58574=CARTESIAN_POINT('Ctrl Pts',(4.86331813894988,-2.32840630217865,30.9706478407225));
#58575=CARTESIAN_POINT('Ctrl Pts',(4.59395401058964,2.82292858162795,31.1294086029683));
#58576=CARTESIAN_POINT('Ctrl Pts',(0.120062847618306,5.39063300003123,31.2881693652142));
#58577=CARTESIAN_POINT('Ctrl Pts',(-4.46371350087791,3.02466543778803,31.4469301274601));
#58578=CARTESIAN_POINT('Ctrl Pts',(-4.96216290745751,-2.10956832273333,
31.605690889706));
#58579=CARTESIAN_POINT('Ctrl Pts',(-0.919089249897086,-5.31306071668268,
31.7644516519519));
#58580=CARTESIAN_POINT('Ctrl Pts',(3.96516296311825,-3.65387765317291,31.9232124141978));
#58581=CARTESIAN_POINT('Ctrl Pts',(5.22037691480677,1.34944584766767,32.0819731764437));
#58582=CARTESIAN_POINT('Ctrl Pts',(1.69774245557567,5.11771528936226,32.2407339386896));
#58583=CARTESIAN_POINT('Ctrl Pts',(-3.37871775721717,4.20209537558378,32.3994947009355));
#58584=CARTESIAN_POINT('Ctrl Pts',(-5.36287227432698,-0.559410580603594,
32.5582554631813));
#58585=CARTESIAN_POINT('Ctrl Pts',(-2.43876227490629,-4.80892688600382,
32.7170162254272));
#58586=CARTESIAN_POINT('Ctrl Pts',(2.71737745147233,-4.65716641474905,32.8757769876731));
#58587=CARTESIAN_POINT('Ctrl Pts',(5.38649033088843,-0.24302498571551,33.034537749919));
#58588=CARTESIAN_POINT('Ctrl Pts',(3.12572272698597,4.39354033353968,33.1932985121649));
#58589=CARTESIAN_POINT('Ctrl Pts',(-1.99580179309791,5.00900333710248,33.3520592744107));
#58590=CARTESIAN_POINT('Ctrl Pts',(-5.29070754957905,1.04007348454996,33.5108200366567));
#58591=CARTESIAN_POINT('Ctrl Pts',(-3.74339614991909,-3.88076339052093,
33.6695807989025));
#58592=CARTESIAN_POINT('Ctrl Pts',(1.22998574967103,-5.24980707112582,33.8283415611485));
#58593=CARTESIAN_POINT('Ctrl Pts',(5.07764712075832,-1.81406696279143,33.9871023233943));
#58594=CARTESIAN_POINT('Ctrl Pts',(4.2780907481768,3.28196264128657,34.1458630856403));
#58595=CARTESIAN_POINT('Ctrl Pts',(-0.436904953119544,5.37423978720491,
34.3046238478861));
#58596=CARTESIAN_POINT('Ctrl Pts',(-4.75203189588531,2.54784852158155,34.463384610132));
#58597=CARTESIAN_POINT('Ctrl Pts',(-4.71795409483259,-2.61041153603965,
34.6221453723779));
#58598=CARTESIAN_POINT('Ctrl Pts',(-0.36586059440485,-5.3795432198188,34.7809061346238));
#58599=CARTESIAN_POINT('Ctrl Pts',(4.32107969737961,-3.22515262853255,34.9396668968697));
#58600=CARTESIAN_POINT('Ctrl Pts',(5.05323586102427,1.88099616195643,35.0984276591155));
#58601=CARTESIAN_POINT('Ctrl Pts',(1.16051621156039,5.265599809247,35.2571884213615));
#58602=CARTESIAN_POINT('Ctrl Pts',(-3.79434332315281,3.83096567127432,35.4159491836074));
#58603=CARTESIAN_POINT('Ctrl Pts',(-5.27650394879067,-1.10988526741874,
35.5747099458532));
#58604=CARTESIAN_POINT('Ctrl Pts',(-1.92944698758358,-5.03493530748322,
35.7334707080991));
#58605=CARTESIAN_POINT('Ctrl Pts',(3.18349879238559,-4.3518587600376,35.892231470345));
#58606=CARTESIAN_POINT('Ctrl Pts',(5.38280923632674,0.314171853851074,36.0509922325909));
#58607=CARTESIAN_POINT('Ctrl Pts',(2.65560824713265,4.69266279059105,36.2097529948368));
#58608=CARTESIAN_POINT('Ctrl Pts',(-2.50208652644733,4.77628540213074,36.3685137570827));
#58609=CARTESIAN_POINT('Ctrl Pts',(-5.36979528379463,0.488505720103176,
36.5272745193286));
#58610=CARTESIAN_POINT('Ctrl Pts',(-3.32290337488047,-4.24636931856435,
36.6860352815745));
#58611=CARTESIAN_POINT('Ctrl Pts',(1.76521120212947,-5.09483744984206,36.8447960438204));
#58612=CARTESIAN_POINT('Ctrl Pts',(5.23775056787229,-1.28035472318811,37.0035568060662));
#58613=CARTESIAN_POINT('Ctrl Pts',(3.91654062472413,3.70594775507185,37.1623175683121));
#58614=CARTESIAN_POINT('Ctrl Pts',(-0.98920693046264,5.30045364824194,37.321078330558));
#58615=CARTESIAN_POINT('Ctrl Pts',(-4.98960208717089,2.04382245807619,37.4798390928039));
#58616=CARTESIAN_POINT('Ctrl Pts',(-4.42336100432008,-3.08337747509074,
37.6385998550498));
#58617=CARTESIAN_POINT('Ctrl Pts',(0.191275183005581,-5.38857616006331,
37.7973606172957));
#58618=CARTESIAN_POINT('Ctrl Pts',(4.63085048026802,-2.761985347144,37.9561213795416));
#58619=CARTESIAN_POINT('Ctrl Pts',(4.83212996681944,2.39245882142244,38.1148821417875));
#58620=CARTESIAN_POINT('Ctrl Pts',(0.610896508406062,5.35725159801683,38.2736429040334));
#58621=CARTESIAN_POINT('Ctrl Pts',(-4.16944809457737,3.41892407272547,38.4324036662793));
#58622=CARTESIAN_POINT('Ctrl Pts',(-5.13378644395327,-1.64850719631984,
38.5911644285251));
#58623=CARTESIAN_POINT('Ctrl Pts',(-1.39952662627435,-5.20717432498527,
38.7499251907711));
#58624=CARTESIAN_POINT('Ctrl Pts',(3.61562270886826,-4.00007645621339,38.9086859530169));
#58625=CARTESIAN_POINT('Ctrl Pts',(5.32164370022099,0.868013569211233,39.0674467152629));
#58626=CARTESIAN_POINT('Ctrl Pts',(2.15713382540813,4.94167106227405,39.2262074775087));
#58627=CARTESIAN_POINT('Ctrl Pts',(-2.98165081692889,4.49256025383564,39.3849682397546));
#58628=CARTESIAN_POINT('Ctrl Pts',(-5.39153755590251,-0.0682789259528612,
39.5437290020005));
#58629=CARTESIAN_POINT('Ctrl Pts',(-2.8669244370552,-4.56662714710238,39.7024897642464));
#58630=CARTESIAN_POINT('Ctrl Pts',(2.28158549793223,-4.88545871378134,39.8612505264922));
#58631=CARTESIAN_POINT('Ctrl Pts',(5.3419186932756,-0.732969237328121,40.0200112887382));
#58632=CARTESIAN_POINT('Ctrl Pts',(3.51316472950203,4.09035607396464,40.1787720509841));
#58633=CARTESIAN_POINT('Ctrl Pts',(-1.53094490572569,5.17006256481187,40.3375328132299));
#58634=CARTESIAN_POINT('Ctrl Pts',(-5.17388699991225,1.517969874726,40.4962935754758));
#58635=CARTESIAN_POINT('Ctrl Pts',(-4.08152967334293,-3.52341521170266,
40.6550543377217));
#58636=CARTESIAN_POINT('Ctrl Pts',(0.746368282217007,-5.34006307226206,
40.8138150999676));
#58637=CARTESIAN_POINT('Ctrl Pts',(4.89116718777592,-2.26932209473684,40.9725758622135));
#58638=CARTESIAN_POINT('Ctrl Pts',(4.55942048043523,2.87837178123751,41.1313366244594));
#58639=CARTESIAN_POINT('Ctrl Pts',(0.054752880088232,5.39169188201243,41.2900973867052));
#58640=CARTESIAN_POINT('Ctrl Pts',(-4.50002622856399,2.97037088099662,41.4488581489512));
#58641=CARTESIAN_POINT('Ctrl Pts',(-4.93624387774355,-2.16952428146721,
41.607618911197));
#58642=CARTESIAN_POINT('Ctrl Pts',(-0.854660350479725,-5.32380455255023,
41.766379673443));
#58643=CARTESIAN_POINT('Ctrl Pts',(4.00913443548347,-3.60557627941182,41.9251404356888));
#58644=CARTESIAN_POINT('Ctrl Pts',(5.20364692548634,1.41258553840574,42.0839011979347));
#58645=CARTESIAN_POINT('Ctrl Pts',(1.63562280181919,5.13790592348729,42.2426619601806));
#58646=CARTESIAN_POINT('Ctrl Pts',(-3.42937327082192,4.16085786801338,42.4014227224264));
#58647=CARTESIAN_POINT('Ctrl Pts',(-5.3557021744363,-0.62433440332485,42.5601834846724));
#58648=CARTESIAN_POINT('Ctrl Pts',(-2.38032885595355,-4.83811675819748,
42.7189442469182));
#58649=CARTESIAN_POINT('Ctrl Pts',(2.77359413958947,-4.62390687376719,42.8777050091642));
#58650=CARTESIAN_POINT('Ctrl Pts',(5.38903905804413,-0.177756179390683,
43.03646577141));
#58651=CARTESIAN_POINT('Ctrl Pts',(3.07227082023542,4.43108239999738,43.195226533656));
#58652=CARTESIAN_POINT('Ctrl Pts',(-2.05633351598682,4.9844590177336,43.3539872959018));
#58653=CARTESIAN_POINT('Ctrl Pts',(-5.30291860685286,0.975906490156919,
43.5127480581477));
#58654=CARTESIAN_POINT('Ctrl Pts',(-3.6961106089692,-3.92582546666328,43.6715088203936));
#58655=CARTESIAN_POINT('Ctrl Pts',(1.29349071741166,-5.23452204049296,43.8302695826395));
#58656=CARTESIAN_POINT('Ctrl Pts',(5.09924982902894,-1.75242415230585,43.9890303448854));
#58657=CARTESIAN_POINT('Ctrl Pts',(4.23801973850483,3.33354584856425,44.1477911071313));
#58658=CARTESIAN_POINT('Ctrl Pts',(-0.501975468697378,5.36855286434462,
44.3065518693772));
#58659=CARTESIAN_POINT('Ctrl Pts',(-4.78254739390742,2.4900963140943,44.4653126316231));
#58660=CARTESIAN_POINT('Ctrl Pts',(-4.68598585940108,-2.66737244379737,
44.624073393869));
#58661=CARTESIAN_POINT('Ctrl Pts',(-0.300666931069113,-5.38358046517354,
44.7828341561148));
#58662=CARTESIAN_POINT('Ctrl Pts',(4.35983155656832,-3.1725712012164,44.9415949183607));
#58663=CARTESIAN_POINT('Ctrl Pts',(5.03007903084552,1.94207213354316,45.1003556806066));
#58664=CARTESIAN_POINT('Ctrl Pts',(1.0966445303283,5.27927173031827,45.2591164428526));
#58665=CARTESIAN_POINT('Ctrl Pts',(-3.84047254178868,3.78472058205141,45.4178772050983));
#58666=CARTESIAN_POINT('Ctrl Pts',(-5.26267183489948,-1.17372244870432,
45.5766379673443));
#58667=CARTESIAN_POINT('Ctrl Pts',(-1.86831311430597,-5.05793884258687,
45.7353987295902));
#58668=CARTESIAN_POINT('Ctrl Pts',(3.23598283686748,-4.3129751109803,45.8941594918361));
#58669=CARTESIAN_POINT('Ctrl Pts',(5.37860845135706,0.379355183735526,46.052920254082));
#58670=CARTESIAN_POINT('Ctrl Pts',(2.59856731943033,4.72448802674167,46.2116810163278));
#58671=CARTESIAN_POINT('Ctrl Pts',(-2.55976199751136,4.745625116308,46.3704417785738));
#58672=CARTESIAN_POINT('Ctrl Pts',(-5.37531894538233,0.423421142422616,
46.5292025408196));
#58673=CARTESIAN_POINT('Ctrl Pts',(-3.27121980318429,-4.28631079457517,
46.6879633030656));
#58674=CARTESIAN_POINT('Ctrl Pts',(1.82679962359794,-5.07308016530974,46.8467240653114));
#58675=CARTESIAN_POINT('Ctrl Pts',(5.25287623454225,-1.21681160950152,47.0054848275573));
#58676=CARTESIAN_POINT('Ctrl Pts',(3.87136006443976,3.75312009931705,47.1642455898032));
#58677=CARTESIAN_POINT('Ctrl Pts',(-1.05334308887091,5.28808165269453,47.3230063520491));
#58678=CARTESIAN_POINT('Ctrl Pts',(-5.01399447246331,1.98322935096872,47.4817671142949));
#58679=CARTESIAN_POINT('Ctrl Pts',(-4.38568496040199,-3.13673503129295,
47.6405278765409));
#58680=CARTESIAN_POINT('Ctrl Pts',(0.256537389910642,-5.38586370009625,
47.7992886387868));
#58681=CARTESIAN_POINT('Ctrl Pts',(4.66396888494043,-2.70568539722266,47.9580494010326));
#58682=CARTESIAN_POINT('Ctrl Pts',(4.80279359368822,2.45081882742566,48.1168101632785));
#58683=CARTESIAN_POINT('Ctrl Pts',(0.545954902252042,5.3642587999782,48.2755709255244));
#58684=CARTESIAN_POINT('Ctrl Pts',(-4.21055839213486,3.36816526537215,48.4343316877703));
#58685=CARTESIAN_POINT('Ctrl Pts',(-5.11344003285917,-1.71057600205014,
48.5930924500163));
#58686=CARTESIAN_POINT('Ctrl Pts',(-1.33634516345125,-5.22374586217178,
48.751853212262));
#58687=CARTESIAN_POINT('Ctrl Pts',(3.66381361874176,-3.9559839478389,48.910613974508));
#58688=CARTESIAN_POINT('Ctrl Pts',(5.31073826441816,0.932415312659234,49.0693747367539));
#58689=CARTESIAN_POINT('Ctrl Pts',(2.09711303188655,4.96743959801509,49.2281354989997));
#58690=CARTESIAN_POINT('Ctrl Pts',(-3.03585410457926,4.45611143084931,49.3868962612457));
#58691=CARTESIAN_POINT('Ctrl Pts',(-5.39031483316305,-0.133586031525688,
49.5456570234915));
#58692=CARTESIAN_POINT('Ctrl Pts',(-2.81139477712564,-4.60102147740992,
49.7044177857375));
#58693=CARTESIAN_POINT('Ctrl Pts',(2.34059965410881,-4.85746152713764,49.8631785479833));
#58694=CARTESIAN_POINT('Ctrl Pts',(5.35040578735549,-0.668204414134744,
50.0219393102293));
#58695=CARTESIAN_POINT('Ctrl Pts',(3.46335711374174,4.13261378925387,50.180700072475));
#58696=CARTESIAN_POINT('Ctrl Pts',(-1.59346177998899,5.15113762038552,50.339460834721));
#58697=CARTESIAN_POINT('Ctrl Pts',(-5.19189577974993,1.45518295779302,50.4982215969668));
#58698=CARTESIAN_POINT('Ctrl Pts',(-4.03854817336226,-3.57259959691384,
50.6569823592128));
#58699=CARTESIAN_POINT('Ctrl Pts',(0.811002080346741,-5.33062987404959,
50.8157431214586));
#58700=CARTESIAN_POINT('Ctrl Pts',(4.91829845774134,-2.2099048642455,50.9745038837045));
#58701=CARTESIAN_POINT('Ctrl Pts',(4.5242178552285,2.93339257973907,51.1332646459504));
#58702=CARTESIAN_POINT('Ctrl Pts',(-0.0105651224232033,5.3919595331034,
51.2920254081963));
#58703=CARTESIAN_POINT('Ctrl Pts',(-4.53567857731733,2.91564042222309,51.4507861704422));
#58704=CARTESIAN_POINT('Ctrl Pts',(-4.90960045414457,-2.22916186247211,
51.6095469326881));
#58705=CARTESIAN_POINT('Ctrl Pts',(-0.790106029640123,-5.33376711999718,
51.7683076949339));
#58706=CARTESIAN_POINT('Ctrl Pts',(4.05251756729386,-3.55674578726275,51.92706845718));
#58707=CARTESIAN_POINT('Ctrl Pts',(5.18615330087962,1.47551793218919,52.0858292194257));
#58708=CARTESIAN_POINT('Ctrl Pts',(1.57326312038517,5.15734256981952,52.2445899816717));
#58709=CARTESIAN_POINT('Ctrl Pts',(-3.47952552383355,4.11900975447104,52.4033507439175));
#58710=CARTESIAN_POINT('Ctrl Pts',(-5.34774612514876,-0.689166604960497,
52.5621115061635));
#58711=CARTESIAN_POINT('Ctrl Pts',(-2.32154612369557,-4.86659663666414,
52.7208722684093));
#58712=CARTESIAN_POINT('Ctrl Pts',(2.82940380271352,-4.58996877436295,52.8796330306552));
#58713=CARTESIAN_POINT('Ctrl Pts',(5.39079694361469,-0.112461287343052,
53.0383937929012));
#58714=CARTESIAN_POINT('Ctrl Pts',(3.01836805768307,4.46797420502795,53.1971545551469));
#58715=CARTESIAN_POINT('Ctrl Pts',(-2.11656347189292,4.95918322890829,53.355915317393));
#58716=CARTESIAN_POINT('Ctrl Pts',(-5.31435146071946,0.911596281467614,
53.5146760796387));
#58717=CARTESIAN_POINT('Ctrl Pts',(-3.64828266371651,-3.97031142784319,
53.6734368418848));
#58718=CARTESIAN_POINT('Ctrl Pts',(1.35680586536473,-5.21846884365023,53.8321976041305));
#58719=CARTESIAN_POINT('Ctrl Pts',(5.1201042222894,-1.69052417354231,53.9909583663765));
#58720=CARTESIAN_POINT('Ctrl Pts',(4.19732679935496,3.38463985792481,54.1497191286223));
#58721=CARTESIAN_POINT('Ctrl Pts',(-0.56697231936563,5.36207810624853,54.3084798908682));
#58722=CARTESIAN_POINT('Ctrl Pts',(-4.81236105300778,2.43197868492519,54.4672406531142));
#58723=CARTESIAN_POINT('Ctrl Pts',(-4.65332995545485,-2.72394191459784,
54.6260014153599));
#58724=CARTESIAN_POINT('Ctrl Pts',(-0.235429144855458,-5.3868276699918,
54.784762177606));
#58725=CARTESIAN_POINT('Ctrl Pts',(4.39794361039255,-3.11952419901562,54.9435229398517));
#58726=CARTESIAN_POINT('Ctrl Pts',(5.00618403647253,2.002863106007,55.1022837020977));
#58727=CARTESIAN_POINT('Ctrl Pts',(1.03261191649043,5.29216891816187,55.2610444643436));
#58728=CARTESIAN_POINT('Ctrl Pts',(-3.88603817100542,3.73792008501059,55.4198052265894));
#58729=CARTESIAN_POINT('Ctrl Pts',(-5.24806742381559,-1.23738738619803,
55.5785659888354));
#58730=CARTESIAN_POINT('Ctrl Pts',(-1.80690506604304,-5.08020012506836,
55.7373267510812));
#58731=CARTESIAN_POINT('Ctrl Pts',(3.287992000806,-4.27345853274282,55.8960875133271));
#58732=CARTESIAN_POINT('Ctrl Pts',(5.37361835549403,0.444482843239534,56.054848275573));
#58733=CARTESIAN_POINT('Ctrl Pts',(2.54114505192401,4.7556199441838,56.2136090378189));
#58734=CARTESIAN_POINT('Ctrl Pts',(-2.61706182345312,4.71426840990844,56.3723698000648));
#58735=CARTESIAN_POINT('Ctrl Pts',(-5.38005377881171,0.358274427681354,
56.5311305623107));
#58736=CARTESIAN_POINT('Ctrl Pts',(-3.21905617991939,-4.32562325439461,
56.6898913245565));
#58737=CARTESIAN_POINT('Ctrl Pts',(1.88811996218651,-5.05057840616592,56.8486520868024));
#58738=CARTESIAN_POINT('Ctrl Pts',(5.26723104152409,-1.15308992868801,57.0074128490484));
#58739=CARTESIAN_POINT('Ctrl Pts',(3.82561138199176,3.79974167311562,57.1661736112942));
#58740=CARTESIAN_POINT('Ctrl Pts',(-1.11732466916059,5.27493363106322,57.3249343735401));
#58741=CARTESIAN_POINT('Ctrl Pts',(-5.03765105397079,1.92234520491603,57.4836951357861));
#58742=CARTESIAN_POINT('Ctrl Pts',(-4.34736531713187,-3.18963227156913,
57.6424558980318));
#58743=CARTESIAN_POINT('Ctrl Pts',(0.321761949948743,-5.38236086452793,
57.8012166602778));
#58744=CARTESIAN_POINT('Ctrl Pts',(4.69640285208957,-2.64898838791747,57.9599774225237));
#58745=CARTESIAN_POINT('Ctrl Pts',(4.77275241050502,2.50881917571891,58.1187381847696));
#58746=CARTESIAN_POINT('Ctrl Pts',(0.480933177205712,5.37047879685782,58.2774989470154));
#58747=CARTESIAN_POINT('Ctrl Pts',(-4.25105079016747,3.31691217970165,58.4362597092614));
#58748=CARTESIAN_POINT('Ctrl Pts',(-5.09234322434225,-1.77239378071924,
58.5950204715072));
#58749=CARTESIAN_POINT('Ctrl Pts',(-1.27296759194985,-5.23955081455291,
58.7537812337532));
#58750=CARTESIAN_POINT('Ctrl Pts',(3.71146686389641,-3.91131089874422,58.912541995999));
#58751=CARTESIAN_POINT('Ctrl Pts',(5.29905347767321,0.996680224142156,59.071302758245));
#58752=CARTESIAN_POINT('Ctrl Pts',(2.03678448698746,4.99247916189982,59.2300635204907));
#58753=CARTESIAN_POINT('Ctrl Pts',(-3.08961188058148,4.41900867342512,59.3888242827367));
#58754=CARTESIAN_POINT('Ctrl Pts',(-5.38830108161851,-0.198873533345728,
59.5475850449826));
#58755=CARTESIAN_POINT('Ctrl Pts',(-2.7554525449587,-4.63474060772737,59.7063458072284));
#58756=CARTESIAN_POINT('Ctrl Pts',(2.39927032724118,-4.82875150792175,59.8651065694744));
#58757=CARTESIAN_POINT('Ctrl Pts',(5.35810770928357,-0.603341531930828,
60.0238673317202));
#58758=CARTESIAN_POINT('Ctrl Pts',(3.4130412502586,4.17426504339022,60.1826280939662));
#58759=CARTESIAN_POINT('Ctrl Pts',(-1.65574481370544,5.13145674641463,60.341388856212));
#58760=CARTESIAN_POINT('Ctrl Pts',(-5.20914264878242,1.39218249273314,60.500149618458));
#58761=CARTESIAN_POINT('Ctrl Pts',(-3.99497401635973,-3.62125970306563,
60.6589103807038));
#58762=CARTESIAN_POINT('Ctrl Pts',(0.875516863905577,-5.32041440580089,
60.8176711429497));
#58763=CARTESIAN_POINT('Ctrl Pts',(4.94470796731371,-2.15016333017309,60.9764319051956));
#58764=CARTESIAN_POINT('Ctrl Pts',(4.48835130096483,2.98798290282324,61.1351926674415));
#58765=CARTESIAN_POINT('Ctrl Pts',(-0.0758815745026817,5.39143591402955,
61.2939534296874));
#58766=CARTESIAN_POINT('Ctrl Pts',(-4.57066531515243,2.86048209316173,61.4527141919332));
#58767=CARTESIAN_POINT('Ctrl Pts',(-4.88223654658481,-2.2884723139309,61.6114749541792));
#58768=CARTESIAN_POINT('Ctrl Pts',(-0.725435760725668,-5.34294695701698,
61.770235716425));
#58769=CARTESIAN_POINT('Ctrl Pts',(4.09530599207347,-3.50739334260129,61.9289964786709));
#58770=CARTESIAN_POINT('Ctrl Pts',(5.16789860817661,1.53823379368774,62.0877572409168));
#58771=CARTESIAN_POINT('Ctrl Pts',(1.51067256255815,5.17602237603069,62.2465180031627));
#58772=CARTESIAN_POINT('Ctrl Pts',(-3.52916715640777,4.07655717616831,62.4052787654086));
#58773=CARTESIAN_POINT('Ctrl Pts',(-5.33900529401489,-0.75389767138361,
62.5640395276545));
#58774=CARTESIAN_POINT('Ctrl Pts',(-2.26242270449944,-4.89436234198102,
62.7228002899004));
#58775=CARTESIAN_POINT('Ctrl Pts',(2.88479825077521,-4.5553570969531,62.8815610521463));
#58776=CARTESIAN_POINT('Ctrl Pts',(5.39176372963048,-0.0471498915993996,
63.0403218143921));
#58777=CARTESIAN_POINT('Ctrl Pts',(2.96402234956039,4.50421033475823,63.1990825766381));
#58778=CARTESIAN_POINT('Ctrl Pts',(-2.17648282206887,4.93317967984907,63.3578433388838));
#58779=CARTESIAN_POINT('Ctrl Pts',(-5.32500443340729,0.847152296006667,
63.5166041011299));
#58780=CARTESIAN_POINT('Ctrl Pts',(-3.59991933291304,-4.01421474574488,
63.6753648633757));
#58781=CARTESIAN_POINT('Ctrl Pts',(1.41992190203103,-5.20164983640472,63.8341256256216));
#58782=CARTESIAN_POINT('Ctrl Pts',(5.14020724015703,-1.62837611032391,63.9928863878675));
#58783=CARTESIAN_POINT('Ctrl Pts',(4.15601790241685,3.43523717132127,64.1516471501133));
#58784=CARTESIAN_POINT('Ctrl Pts',(-0.631885966835028,5.35481646308756,
64.3104079123593));
#58785=CARTESIAN_POINT('Ctrl Pts',(-4.84146849803133,2.3735041628375,64.4691686746051));
#58786=CARTESIAN_POINT('Ctrl Pts',(-4.61999117524849,-2.7801116468701,64.6279294368511));
#58787=CARTESIAN_POINT('Ctrl Pts',(-0.170156809410319,-5.38928435774618,
64.7866901990969));
#58788=CARTESIAN_POINT('Ctrl Pts',(4.43541026590754,-3.06601940657889,64.9454509613428));
#58789=CARTESIAN_POINT('Ctrl Pts',(4.98155438449627,2.06336015827155,65.1042117235887));
#58790=CARTESIAN_POINT('Ctrl Pts',(0.968427766834154,5.30428948011521,65.2629724858346));
#58791=CARTESIAN_POINT('Ctrl Pts',(-3.93103352404596,3.69057104812572,65.4217332480805));
#58792=CARTESIAN_POINT('Ctrl Pts',(-5.23269285873673,-1.30087073706907,
65.5804940103263));
#58793=CARTESIAN_POINT('Ctrl Pts',(-1.74523185442701,-5.10171588808409,
65.7392547725724));
#58794=CARTESIAN_POINT('Ctrl Pts',(3.33951865185531,-4.23331482438371,65.8980155348181));
#58795=CARTESIAN_POINT('Ctrl Pts',(5.36783968103429,0.50954527487755,66.0567762970641));
#58796=CARTESIAN_POINT('Ctrl Pts',(2.48334987133277,4.78605397430791,66.2155370593099));
#58797=CARTESIAN_POINT('Ctrl Pts',(-2.67397759552212,4.68221988452942,66.3742978215559));
#58798=CARTESIAN_POINT('Ctrl Pts',(-5.38399908924589,0.29307513616095,66.5330585838017));
#58799=CARTESIAN_POINT('Ctrl Pts',(-3.16642016009836,-4.36430092891852,
66.6918193460477));
#58800=CARTESIAN_POINT('Ctrl Pts',(1.94916321913439,-5.0273354745442,66.8505801082934));
#58801=CARTESIAN_POINT('Ctrl Pts',(5.2808128822496,-1.08919903190536,67.0093408705395));
#58802=CARTESIAN_POINT('Ctrl Pts',(3.77930129100008,3.84580563475087,67.1681016327852));
#58803=CARTESIAN_POINT('Ctrl Pts',(-1.18114228203367,5.26101151282039,67.3268623950312));
#58804=CARTESIAN_POINT('Ctrl Pts',(-5.06056836008944,1.86117895466771,67.485623157277));
#58805=CARTESIAN_POINT('Ctrl Pts',(-4.30840769791819,-3.24206143324834,
67.644383919523));
#58806=CARTESIAN_POINT('Ctrl Pts',(0.386939291414611,-5.37806816739956,
67.8031446817688));
#58807=CARTESIAN_POINT('Ctrl Pts',(4.72814762203013,-2.59190263951545,67.9619054440148));
#58808=CARTESIAN_POINT('Ctrl Pts',(4.74201082581408,2.56645135475007,68.1206662062606));
#58809=CARTESIAN_POINT('Ctrl Pts',(0.415840875206383,5.37591067587102,68.2794269685066));
#58810=CARTESIAN_POINT('Ctrl Pts',(-4.29091934641509,3.26517233710519,68.4381877307524));
#58811=CARTESIAN_POINT('Ctrl Pts',(-5.07049911435956,-1.83395146056701,
68.5969484929983));
#58812=CARTESIAN_POINT('Ctrl Pts',(-1.20940321242992,-5.25458686275155,
68.7557092552442));
#58813=CARTESIAN_POINT('Ctrl Pts',(3.75857545121767,-3.86606386470014,68.9144700174901));
#58814=CARTESIAN_POINT('Ctrl Pts',(5.28659105472879,1.06079887278309,69.073230779736));
#58815=CARTESIAN_POINT('Ctrl Pts',(1.97615704392586,5.01678607937179,69.2319915419818));
#58816=CARTESIAN_POINT('Ctrl Pts',(-3.14291625598096,4.38125742639343,69.3907523042277));
#58817=CARTESIAN_POINT('Ctrl Pts',(-5.38549659678694,-0.264131850470941,
69.5495130664737));
#58818=CARTESIAN_POINT('Ctrl Pts',(-2.69910595007792,-4.66777958977181,
69.7082738287194));
#58819=CARTESIAN_POINT('Ctrl Pts',(2.45758890740704,-4.79933286932947,69.8670345909655));
#58820=CARTESIAN_POINT('Ctrl Pts',(5.36502332880251,-0.538390109345589,
70.0257953532112));
#58821=CARTESIAN_POINT('Ctrl Pts',(3.36222452290666,4.21530372405138,70.1845561154571));
#58822=CARTESIAN_POINT('Ctrl Pts',(-1.7177848668387,5.11102283106786,70.3433168777031));
#58823=CARTESIAN_POINT('Ctrl Pts',(-5.22562507603134,1.32897772486576,70.5020776399489));
#58824=CARTESIAN_POINT('Ctrl Pts',(-3.95081359684368,-3.66938838928662,
70.6608384021949));
#58825=CARTESIAN_POINT('Ctrl Pts',(0.939903165347853,-5.3094181666361,70.8195991644408));
#58826=CARTESIAN_POINT('Ctrl Pts',(4.97039184089704,-2.09010625959075,70.9783599266866));
#58827=CARTESIAN_POINT('Ctrl Pts',(4.45182608106173,3.0421347393591,71.1371206889325));
#58828=CARTESIAN_POINT('Ctrl Pts',(-0.141186890959645,5.39012110163196,
71.2958814511784));
#58829=CARTESIAN_POINT('Ctrl Pts',(-4.60498130776496,2.80490398829831,71.4546422134243));
#58830=CARTESIAN_POINT('Ctrl Pts',(-4.85415617071822,-2.34744693203373,
71.6134029756702));
#58831=CARTESIAN_POINT('Ctrl Pts',(-0.660659034099426,-5.35134271646838,
71.7721637379161));
#58832=CARTESIAN_POINT('Ctrl Pts',(4.13749343062021,-3.4575261878996,71.9309245001619));
#58833=CARTESIAN_POINT('Ctrl Pts',(5.14888552625377,1.60072391934755,72.0896852624079));
#58834=CARTESIAN_POINT('Ctrl Pts',(1.44786031350356,5.19394260085899,72.2484460246537));
#58835=CARTESIAN_POINT('Ctrl Pts',(-3.57829088363412,4.03350636302179,72.4072067868997));
#58836=CARTESIAN_POINT('Ctrl Pts',(-5.32948096375172,-0.818518103308924,
72.5659675491455));
#58837=CARTESIAN_POINT('Ctrl Pts',(-2.20296727472809,-4.92140979953042,
72.7247283113914));
#58838=CARTESIAN_POINT('Ctrl Pts',(2.93976935463837,-4.52007692080191,72.8834890736374));
#58839=CARTESIAN_POINT('Ctrl Pts',(5.39193927421552,0.0181684233918482,
73.0422498358832));
#58840=CARTESIAN_POINT('Ctrl Pts',(2.90924167110106,4.53978547153557,73.201010598129));
#58841=CARTESIAN_POINT('Ctrl Pts',(-2.23608277334895,4.90645218657722,73.359771360375));
#58842=CARTESIAN_POINT('Ctrl Pts',(-5.33487596159239,0.782583990930051,
73.5185321226207));
#58843=CARTESIAN_POINT('Ctrl Pts',(-3.5510277138785,-4.05752897755565,73.6772928848669));
#58844=CARTESIAN_POINT('Ctrl Pts',(1.48282956513097,-5.18406748694598,73.8360536471125));
#58845=CARTESIAN_POINT('Ctrl Pts',(5.15955593251365,-1.56598908288006,73.9948144093587));
#58846=CARTESIAN_POINT('Ctrl Pts',(4.11409910977184,3.48533036359696,74.1535751716043));
#58847=CARTESIAN_POINT('Ctrl Pts',(-0.696706885026663,5.34676900050795,
74.3123359338504));
#58848=CARTESIAN_POINT('Ctrl Pts',(-4.86986545745996,2.31468132896846,74.4710966960961));
#58849=CARTESIAN_POINT('Ctrl Pts',(-4.58597441124858,-2.83587339770487,
74.6298574583422));
#58850=CARTESIAN_POINT('Ctrl Pts',(-0.104859503450096,-5.39095016791776,
74.7886182205879));
#58851=CARTESIAN_POINT('Ctrl Pts',(4.47222602488106,-3.01206467573539,74.9473789828339));
#58852=CARTESIAN_POINT('Ctrl Pts',(4.95619368931852,2.12355441239345,75.1061397450797));
#58853=CARTESIAN_POINT('Ctrl Pts',(0.904101500384337,5.31563163748572,75.2649005073256));
#58854=CARTESIAN_POINT('Ctrl Pts',(-3.97545199784159,3.64268041986863,75.4236612695716));
#58855=CARTESIAN_POINT('Ctrl Pts',(-5.21655039588045,-1.36416318513457,
75.5824220318174));
#58856=CARTESIAN_POINT('Ctrl Pts',(-1.68330253000285,-5.12248297419546,
75.7411827940633));
#58857=CARTESIAN_POINT('Ctrl Pts',(3.39055522847852,-4.19254987699292,75.8999435563093));
#58858=CARTESIAN_POINT('Ctrl Pts',(5.36127327599845,0.574532930736923,76.058704318555));
#58859=CARTESIAN_POINT('Ctrl Pts',(2.42519025910013,4.81578565091957,76.217465080801));
#58860=CARTESIAN_POINT('Ctrl Pts',(-2.73050096132775,4.64948424329249,76.3762258430469));
#58861=CARTESIAN_POINT('Ctrl Pts',(-5.38715429771053,0.227832835858649,
76.5349866052928));
#58862=CARTESIAN_POINT('Ctrl Pts',(-3.11331946805805,-4.40233814219751,
76.6937473675387));
#58863=CARTESIAN_POINT('Ctrl Pts',(2.00992043634247,-5.00335478134514,76.8525081297845));
#58864=CARTESIAN_POINT('Ctrl Pts',(5.29361976358337,-1.02514829514396,77.0112688920305));
#58865=CARTESIAN_POINT('Ctrl Pts',(3.73243658747159,3.89130522433545,77.1700296542762));
#58866=CARTESIAN_POINT('Ctrl Pts',(-1.24478656225425,5.2463173410372,77.3287904165223));
#58867=CARTESIAN_POINT('Ctrl Pts',(-5.0827430277043,1.79973957637201,77.4875511787681));
#58868=CARTESIAN_POINT('Ctrl Pts',(-4.26881781979216,-3.29401482234996,
77.646311941014));
#58869=CARTESIAN_POINT('Ctrl Pts',(0.452059849531884,-5.3729862386645,77.8050727032599));
#58870=CARTESIAN_POINT('Ctrl Pts',(4.75919853621651,-2.53443652935156,77.9638334655057));
#58871=CARTESIAN_POINT('Ctrl Pts',(4.71057335094352,2.62370690699572,78.1225942277518));
#58872=CARTESIAN_POINT('Ctrl Pts',(0.350687548550617,5.38055363988948,78.2813549899974));
#58873=CARTESIAN_POINT('Ctrl Pts',(-4.33015821016646,3.21295333040559,78.4401157522436));
#58874=CARTESIAN_POINT('Ctrl Pts',(-5.04791090853454,-1.89524000800277,
78.5988765144892));
#58875=CARTESIAN_POINT('Ctrl Pts',(-1.14566135296546,-5.26885180022729,
78.7576372767353));
#58876=CARTESIAN_POINT('Ctrl Pts',(3.80513246751939,-3.82024948570991,78.916398038981));
#58877=CARTESIAN_POINT('Ctrl Pts',(5.27335282444574,1.12476184916915,79.0751588012271));
#58878=CARTESIAN_POINT('Ctrl Pts',(1.91523959978009,5.0403567833905,79.2339195634728));
#58879=CARTESIAN_POINT('Ctrl Pts',(-3.19575940835959,4.34286322975033,79.3926803257188));
#58880=CARTESIAN_POINT('Ctrl Pts',(-5.3819017902265,-0.329351406241924,
79.5514410879647));
#58881=CARTESIAN_POINT('Ctrl Pts',(-2.64236326134738,-4.70013357507201,
79.7102018502106));
#58882=CARTESIAN_POINT('Ctrl Pts',(2.51554683635375,-4.76920992854652,79.8689626124565));
#58883=CARTESIAN_POINT('Ctrl Pts',(5.37115163104497,-0.473359678001532,
80.0277233747023));
#58884=CARTESIAN_POINT('Ctrl Pts',(3.31091438904171,4.25572380881061,80.1864841369483));
#58885=CARTESIAN_POINT('Ctrl Pts',(-1.77957283501041,5.089838873022,80.3452448991941));
#58886=CARTESIAN_POINT('Ctrl Pts',(-5.24134064269895,1.26557792949291,80.50400566144));
#58887=CARTESIAN_POINT('Ctrl Pts',(-3.9060733953589,-3.71697859269313,80.6627664236859));
#58888=CARTESIAN_POINT('Ctrl Pts',(1.00415153598694,-5.29764277024969,80.8215271859318));
#58889=CARTESIAN_POINT('Ctrl Pts',(4.99534630937428,-2.02974246588212,80.9802879481777));
#58890=CARTESIAN_POINT('Ctrl Pts',(4.41464755561157,3.0958401425779,81.1390487104235));
#58891=CARTESIAN_POINT('Ctrl Pts',(-0.206471488267744,5.38801528883197,
81.2978094726694));
#58892=CARTESIAN_POINT('Ctrl Pts',(-4.63862151922447,2.74891426377335,81.4565702349153));
#58893=CARTESIAN_POINT('Ctrl Pts',(-4.82536344745119,-2.40607706235473,
81.6153309971613));
#58894=CARTESIAN_POINT('Ctrl Pts',(-0.595785355535171,-5.35895316608133,
81.7740917594071));
#58895=CARTESIAN_POINT('Ctrl Pts',(4.17907369152063,-3.4071516415317,81.932852521653));
#58896=CARTESIAN_POINT('Ctrl Pts',(5.12911684605883,1.66297913944664,82.0916132838989));
#58897=CARTESIAN_POINT('Ctrl Pts',(1.38483558943104,5.2111006131604,82.2503740461447));
#58898=CARTESIAN_POINT('Ctrl Pts',(-3.62688949375241,3.98986363532597,82.4091348083908));
#58899=CARTESIAN_POINT('Ctrl Pts',(-5.31917453751786,-0.883018422641366,
82.5678955706364));
#58900=CARTESIAN_POINT('Ctrl Pts',(-2.1431885490041,-4.94773503060847,82.7266563328826));
#58901=CARTESIAN_POINT('Ctrl Pts',(2.99430902725335,-4.48413344144938,82.8854170951283));
#58902=CARTESIAN_POINT('Ctrl Pts',(5.39132358998814,0.0834841069729651,
83.0441778573743));
#58903=CARTESIAN_POINT('Ctrl Pts',(2.85403398786483,4.57469432804498,83.20293861962));
#58904=CARTESIAN_POINT('Ctrl Pts',(-2.29535443865746,4.87900479902879,83.3616993818661));
#58905=CARTESIAN_POINT('Ctrl Pts',(-5.34396486625942,0.717900597107141,
83.5204601441119));
#58906=CARTESIAN_POINT('Ctrl Pts',(-3.50161446504842,-4.10024729857536,
83.6792209063577));
#58907=CARTESIAN_POINT('Ctrl Pts',(1.54551863391146,-5.16572527246177,83.8379816686037));
#58908=CARTESIAN_POINT('Ctrl Pts',(5.17814935421542,-1.50337052857669,83.9967424308496));
#58909=CARTESIAN_POINT('Ctrl Pts',(4.07157294499926,3.5349087933154,84.1555031930955));
#58910=CARTESIAN_POINT('Ctrl Pts',(-0.761418612953421,5.33794320112753,
84.3142639553413));
#58911=CARTESIAN_POINT('Ctrl Pts',(-4.89756107214883,2.25550674636269,84.4730247175872));
#58912=CARTESIAN_POINT('Ctrl Pts',(-4.55125916712634,-2.89119586857457,
84.6317854798332));
#58913=CARTESIAN_POINT('Ctrl Pts',(-0.0395956256930076,-5.39186912790212,
84.7905462420789));
#58914=CARTESIAN_POINT('Ctrl Pts',(4.50847898005441,-2.95758313260692,84.949307004325));
#58915=CARTESIAN_POINT('Ctrl Pts',(4.92992660394334,2.18327463521188,85.1080677665708));
#58916=CARTESIAN_POINT('Ctrl Pts',(0.83998553543098,5.32650478551015,85.2668285288166));
#58917=CARTESIAN_POINT('Ctrl Pts',(-4.0199441247066,3.59365925042037,85.4255892910627));
#58918=CARTESIAN_POINT('Ctrl Pts',(-5.19838251798258,-1.4261119912042,85.5843500533084));
#58919=CARTESIAN_POINT('Ctrl Pts',(-1.62355247471041,-5.1447064563747,85.7431108155544));
#58920=CARTESIAN_POINT('Ctrl Pts',(3.44586114533526,-4.14677678635576,85.9018715778002));
#58921=CARTESIAN_POINT('Ctrl Pts',(5.02742464258896,-0.1665161442746,86.0341722130051));
#58922=CARTESIAN_POINT('Ctrl Pts',(3.86721841197903,2.75399303531867,86.1400127211691));
#58923=CARTESIAN_POINT('Ctrl Pts',(2.68386473467973,3.76615995447699,86.192932975251));
#58924=CARTESIAN_POINT('Ctrl Pts',(2.00237954638958,4.09906332620035,86.219393102292));
#58925=CARTESIAN_POINT('Ctrl Pts',(2.53835875722654,-3.55965150255068,26.));
#58926=CARTESIAN_POINT('Ctrl Pts',(3.13016463613492,-3.13763950664917,26.026460127041));
#58927=CARTESIAN_POINT('Ctrl Pts',(4.08944058768451,-1.99447514282845,26.079380381123));
#58928=CARTESIAN_POINT('Ctrl Pts',(4.72633908941221,0.949051473338421,26.1852208892869));
#58929=CARTESIAN_POINT('Ctrl Pts',(2.60449620246589,4.46265906441401,26.3175215244918));
#58930=CARTESIAN_POINT('Ctrl Pts',(-2.34489469821123,4.60777770546463,26.4762822867377));
#58931=CARTESIAN_POINT('Ctrl Pts',(-5.13873203824598,0.529582897206408,
26.6350430489835));
#58932=CARTESIAN_POINT('Ctrl Pts',(-3.23428844614615,-4.03017972072915,
26.7938038112295));
#58933=CARTESIAN_POINT('Ctrl Pts',(1.63279456941769,-4.90302026906412,26.9525645734753));
#58934=CARTESIAN_POINT('Ctrl Pts',(5.00417945325775,-1.28762125191842,27.1113253357213));
#58935=CARTESIAN_POINT('Ctrl Pts',(3.79627275763131,3.50580663842047,27.2700860979671));
#58936=CARTESIAN_POINT('Ctrl Pts',(-0.886457053099411,5.09084367591115,
27.428846860213));
#58937=CARTESIAN_POINT('Ctrl Pts',(-4.75768720014009,2.01646474678857,27.5876076224589));
#58938=CARTESIAN_POINT('Ctrl Pts',(-4.27463438144488,-2.90338148363688,
27.7463683847048));
#58939=CARTESIAN_POINT('Ctrl Pts',(0.12074539761077,-5.16599709979471,27.9051291469506));
#58940=CARTESIAN_POINT('Ctrl Pts',(4.40558866999103,-2.70051724468854,28.0638899091966));
#58941=CARTESIAN_POINT('Ctrl Pts',(4.65831652566081,2.23654953809766,28.2226506714425));
#58942=CARTESIAN_POINT('Ctrl Pts',(0.647603546994949,5.12666253671564,28.3814114336883));
#58943=CARTESIAN_POINT('Ctrl Pts',(-3.95581218859218,3.32469494777108,28.5401721959342));
#58944=CARTESIAN_POINT('Ctrl Pts',(-4.93874975649391,-1.52013373855127,
28.6989329581801));
#58945=CARTESIAN_POINT('Ctrl Pts',(-1.40159165779937,-4.9736902589037,28.857693720426));
#58946=CARTESIAN_POINT('Ctrl Pts',(3.41834539873403,-3.87517318393326,29.0164544826719));
#58947=CARTESIAN_POINT('Ctrl Pts',(5.10970861334159,0.770020576487015,29.1752152449178));
#58948=CARTESIAN_POINT('Ctrl Pts',(2.12451027984608,4.71046807932676,29.3339760071637));
#58949=CARTESIAN_POINT('Ctrl Pts',(-2.80510467897592,4.33975126344986,29.4927367694096));
#58950=CARTESIAN_POINT('Ctrl Pts',(-5.16740219266045,-0.00283844237382118,
29.6514975316555));
#58951=CARTESIAN_POINT('Ctrl Pts',(-2.80033535833003,-4.34283033250174,
29.8102582939013));
#58952=CARTESIAN_POINT('Ctrl Pts',(2.12968392236957,-4.70813124181331,29.9690190561473));
#58953=CARTESIAN_POINT('Ctrl Pts',(5.11055143098187,-0.764406630547101,
30.1277798183931));
#58954=CARTESIAN_POINT('Ctrl Pts',(3.41408616315334,3.87892628001712,30.286540580639));
#58955=CARTESIAN_POINT('Ctrl Pts',(-1.4070550442568,4.97214737476293,30.4453013428849));
#58956=CARTESIAN_POINT('Ctrl Pts',(-4.94041649691963,1.51470731642915,30.6040621051308));
#58957=CARTESIAN_POINT('Ctrl Pts',(-3.95215786419059,-3.32903914551084,
30.7628228673767));
#58958=CARTESIAN_POINT('Ctrl Pts',(0.653236365857992,-5.12594729451212,
30.9215836296226));
#58959=CARTESIAN_POINT('Ctrl Pts',(4.6607687206244,-2.23143190555148,31.0803443918685));
#58960=CARTESIAN_POINT('Ctrl Pts',(4.4026231771807,2.70535812338375,31.2391051541143));
#58961=CARTESIAN_POINT('Ctrl Pts',(0.115062422136807,5.16612176153803,31.3978659163603));
#58962=CARTESIAN_POINT('Ctrl Pts',(-4.27780697629061,2.89869296229943,31.5566266786061));
#58963=CARTESIAN_POINT('Ctrl Pts',(-4.7554967626928,-2.02170817777057,31.715387440852));
#58964=CARTESIAN_POINT('Ctrl Pts',(-0.880810653343035,-5.09178023966167,
31.8741482030979));
#58965=CARTESIAN_POINT('Ctrl Pts',(3.80002027066033,-3.5016994957634,32.0329089653438));
#58966=CARTESIAN_POINT('Ctrl Pts',(5.00295656982363,1.29324358746212,32.1916697275897));
#58967=CARTESIAN_POINT('Ctrl Pts',(1.62703419898677,4.90457063680218,32.3504304898356));
#58968=CARTESIAN_POINT('Ctrl Pts',(-3.23799956916984,4.02708482728032,32.5091912520815));
#58969=CARTESIAN_POINT('Ctrl Pts',(-5.13951722563736,-0.536112025076297,
32.6679520143274));
#58970=CARTESIAN_POINT('Ctrl Pts',(-2.33719172860392,-4.60864277632799,
32.8267127765732));
#58971=CARTESIAN_POINT('Ctrl Pts',(2.60420302889879,-4.4632028858578,32.9854735388192));
#58972=CARTESIAN_POINT('Ctrl Pts',(5.16215162793603,-0.232903383943239,
33.144234301065));
#58973=CARTESIAN_POINT('Ctrl Pts',(2.99554137711165,4.21055640908263,33.302995063311));
#58974=CARTESIAN_POINT('Ctrl Pts',(-1.91267984204806,4.80038636339596,33.4617558255568));
#58975=CARTESIAN_POINT('Ctrl Pts',(-5.07035804619892,0.996756088218607,
33.6205165878027));
#58976=CARTESIAN_POINT('Ctrl Pts',(-3.58748969036538,-3.71913580520757,
33.7792773500486));
#58977=CARTESIAN_POINT('Ctrl Pts',(1.17875881138994,-5.0311610072254,33.9380381122944));
#58978=CARTESIAN_POINT('Ctrl Pts',(4.86617124330449,-1.73851397661661,34.0967988745404));
#58979=CARTESIAN_POINT('Ctrl Pts',(4.09991511421076,3.14527414899259,34.2555596367862));
#58980=CARTESIAN_POINT('Ctrl Pts',(-0.418708560946466,5.15041129979394,
34.4143203990322));
#58981=CARTESIAN_POINT('Ctrl Pts',(-4.55411737150595,2.44173470766227,34.5730811612781));
#58982=CARTESIAN_POINT('Ctrl Pts',(-4.5214588563368,-2.50169207267966,34.7318419235239));
#58983=CARTESIAN_POINT('Ctrl Pts',(-0.350623086089188,-5.15549385292585,
34.8906026857698));
#58984=CARTESIAN_POINT('Ctrl Pts',(4.14111364246891,-3.09083018236409,35.0493634480157));
#58985=CARTESIAN_POINT('Ctrl Pts',(4.84277667347619,1.80265568173448,35.2081242102616));
#58986=CARTESIAN_POINT('Ctrl Pts',(1.11218256837853,5.0462960030749,35.3668849725075));
#58987=CARTESIAN_POINT('Ctrl Pts',(-3.63631499535807,3.67141208128276,35.5256457347534));
#58988=CARTESIAN_POINT('Ctrl Pts',(-5.05674600265519,-1.06366032204162,
35.6844064969993));
#58989=CARTESIAN_POINT('Ctrl Pts',(-1.84908860800444,-4.8252383087059,35.8431672592452));
#58990=CARTESIAN_POINT('Ctrl Pts',(3.05091116183891,-4.17061080641931,36.0019280214911));
#58991=CARTESIAN_POINT('Ctrl Pts',(5.15862384507246,0.301087098868051,36.1606887837369));
#58992=CARTESIAN_POINT('Ctrl Pts',(2.54500641307862,4.49722089444621,36.3194495459828));
#58993=CARTESIAN_POINT('Ctrl Pts',(-2.39787862639785,4.5773607580263,36.4782103082287));
#58994=CARTESIAN_POINT('Ctrl Pts',(-5.14615190283867,0.468160238555881,
36.6369710704746));
#58995=CARTESIAN_POINT('Ctrl Pts',(-3.18450976654496,-4.06951483138158,
36.7957318327205));
#58996=CARTESIAN_POINT('Ctrl Pts',(1.69169298020808,-4.88264562268956,36.9544925949664));
#58997=CARTESIAN_POINT('Ctrl Pts',(5.01960663803976,-1.22702999775959,37.1132533572123));
#58998=CARTESIAN_POINT('Ctrl Pts',(3.75342297485632,3.55160096123927,37.2720141194582));
#58999=CARTESIAN_POINT('Ctrl Pts',(-0.94800804471325,5.07969823544803,37.430774881704));
#59000=CARTESIAN_POINT('Ctrl Pts',(-4.78179314447847,1.95870052317183,37.58953564395));
#59001=CARTESIAN_POINT('Ctrl Pts',(-4.23913509664356,-2.95495973719773,
37.7482964061958));
#59002=CARTESIAN_POINT('Ctrl Pts',(0.183308877707052,-5.16415058566349,
37.9070571684418));
#59003=CARTESIAN_POINT('Ctrl Pts',(4.43798296793759,-2.64695307709652,38.0658179306876));
#59004=CARTESIAN_POINT('Ctrl Pts',(4.63087948595682,2.29281673986369,38.2245786929335));
#59005=CARTESIAN_POINT('Ctrl Pts',(0.585453646372677,5.13413064150142,38.3833394551794));
#59006=CARTESIAN_POINT('Ctrl Pts',(-3.99579725328622,3.27653135597467,38.5421002174253));
#59007=CARTESIAN_POINT('Ctrl Pts',(-4.91997245352125,-1.57984950949354,
38.7008609796712));
#59008=CARTESIAN_POINT('Ctrl Pts',(-1.34123858177823,-4.99030384674165,
38.8596217419171));
#59009=CARTESIAN_POINT('Ctrl Pts',(3.46503780867414,-3.83347967263602,39.0183825041629));
#59010=CARTESIAN_POINT('Ctrl Pts',(5.10000575566994,0.831862193027325,39.1771432664089));
#59011=CARTESIAN_POINT('Ctrl Pts',(2.06729265337245,4.73585837007054,39.3359040286547));
#59012=CARTESIAN_POINT('Ctrl Pts',(-2.85746983156782,4.30545230814772,39.4946647909006));
#59013=CARTESIAN_POINT('Ctrl Pts',(-5.16698864410473,-0.0654352179449955,
39.6534255531465));
#59014=CARTESIAN_POINT('Ctrl Pts',(-2.74752162183386,-4.3764344338297,39.8121863153924));
#59015=CARTESIAN_POINT('Ctrl Pts',(2.18656111288008,-4.68198717594309,39.9709470776383));
#59016=CARTESIAN_POINT('Ctrl Pts',(5.11943632770732,-0.702442241472902,
40.1297078398842));
#59017=CARTESIAN_POINT('Ctrl Pts',(3.36684704019806,3.9199992887709,40.2884686021301));
#59018=CARTESIAN_POINT('Ctrl Pts',(-1.46718350018236,4.95473773199425,40.4472293643759));
#59019=CARTESIAN_POINT('Ctrl Pts',(-4.95840288549236,1.45474885846183,40.6059901266218));
#59020=CARTESIAN_POINT('Ctrl Pts',(-3.91154049361154,-3.37667060621731,
40.7647508888677));
#59021=CARTESIAN_POINT('Ctrl Pts',(0.715283237582617,-5.11765799033974,
40.9235116511136));
#59022=CARTESIAN_POINT('Ctrl Pts',(4.6874579011302,-2.17480846080452,41.0822724133595));
#59023=CARTESIAN_POINT('Ctrl Pts',(4.36952791329752,2.75849220244841,41.2410331756054));
#59024=CARTESIAN_POINT('Ctrl Pts',(0.052472510246957,5.16713654277911,41.3997939378513));
#59025=CARTESIAN_POINT('Ctrl Pts',(-4.3126073369753,2.84665968691757,41.5585547000972));
#59026=CARTESIAN_POINT('Ctrl Pts',(-4.73065721909144,-2.07916706676323,
41.7173154623431));
#59027=CARTESIAN_POINT('Ctrl Pts',(-0.819065114488867,-5.10207661195736,
41.8760762245889));
#59028=CARTESIAN_POINT('Ctrl Pts',(3.8421604015636,-3.45540979692878,42.0348369868349));
#59029=CARTESIAN_POINT('Ctrl Pts',(4.98692335778749,1.35375361111553,42.1935977490807));
#59030=CARTESIAN_POINT('Ctrl Pts',(1.56750172940691,4.92392036332446,42.3523585113267));
#59031=CARTESIAN_POINT('Ctrl Pts',(-3.28654536169065,3.98756479591298,42.5111192735724));
#59032=CARTESIAN_POINT('Ctrl Pts',(-5.13264574893371,-0.59833187447071,
42.6698800358185));
#59033=CARTESIAN_POINT('Ctrl Pts',(-2.28119196804685,-4.63661693705371,
42.8286407980642));
#59034=CARTESIAN_POINT('Ctrl Pts',(2.65807838191241,-4.43132855153674,42.9874015603103));
#59035=CARTESIAN_POINT('Ctrl Pts',(5.1645942046841,-0.170352918960309,43.146162322556));
#59036=CARTESIAN_POINT('Ctrl Pts',(2.94431565674484,4.24653490854626,43.304923084802));
#59037=CARTESIAN_POINT('Ctrl Pts',(-1.97069051554003,4.77686427565358,43.4636838470478));
#59038=CARTESIAN_POINT('Ctrl Pts',(-5.0820605324771,0.935261546463589,43.6224446092938));
#59039=CARTESIAN_POINT('Ctrl Pts',(-3.54217351653091,-3.76232111798581,
43.7812053715396));
#59040=CARTESIAN_POINT('Ctrl Pts',(1.23961889884326,-5.01651257365967,43.9399661337855));
#59041=CARTESIAN_POINT('Ctrl Pts',(4.88687423334376,-1.67943849054845,44.0987268960314));
#59042=CARTESIAN_POINT('Ctrl Pts',(4.06151299797099,3.19470899822934,44.2574876582773));
#59043=CARTESIAN_POINT('Ctrl Pts',(-0.481068993674721,5.1449612281707,44.4162484205232));
#59044=CARTESIAN_POINT('Ctrl Pts',(-4.5833619478656,2.38638778720321,44.5750091827691));
#59045=CARTESIAN_POINT('Ctrl Pts',(-4.49082204675623,-2.55628064977671,
44.733769945015));
#59046=CARTESIAN_POINT('Ctrl Pts',(-0.288144634510089,-5.15936295347187,
44.8925307072609));
#59047=CARTESIAN_POINT('Ctrl Pts',(4.17825154873217,-3.04043868735616,45.0512914695067));
#59048=CARTESIAN_POINT('Ctrl Pts',(4.8205842882194,1.86118793683688,45.2100522317526));
#59049=CARTESIAN_POINT('Ctrl Pts',(1.05097104046387,5.05939851051103,45.3688129939986));
#59050=CARTESIAN_POINT('Ctrl Pts',(-3.68052300585259,3.62709302602572,45.5275737562444));
#59051=CARTESIAN_POINT('Ctrl Pts',(-5.04348997417376,-1.12483878687734,
45.6863345184903));
#59052=CARTESIAN_POINT('Ctrl Pts',(-1.79050086272392,-4.84728378338218,
45.8450952807362));
#59053=CARTESIAN_POINT('Ctrl Pts',(3.1012093298518,-4.13334659912459,46.0038560429821));
#59054=CARTESIAN_POINT('Ctrl Pts',(5.15459801607478,0.363555647367575,46.162616805228));
#59055=CARTESIAN_POINT('Ctrl Pts',(2.49034114873962,4.52772066043712,46.3213775674739));
#59056=CARTESIAN_POINT('Ctrl Pts',(-2.45315200638293,4.54797742404625,46.4801383297198));
#59057=CARTESIAN_POINT('Ctrl Pts',(-5.15144551276008,0.405786329388982,
46.6388990919657));
#59058=CARTESIAN_POINT('Ctrl Pts',(-3.13497873290715,-4.10779280882992,
46.7976598542116));
#59059=CARTESIAN_POINT('Ctrl Pts',(1.75071634247466,-4.86179449424254,46.9564206164574));
#59060=CARTESIAN_POINT('Ctrl Pts',(5.03410234489664,-1.16613335307792,47.1151813787034));
#59061=CARTESIAN_POINT('Ctrl Pts',(3.71012411261097,3.59680865283067,47.2739421409492));
#59062=CARTESIAN_POINT('Ctrl Pts',(-1.00947303475291,5.06784151371782,47.4327029031951));
#59063=CARTESIAN_POINT('Ctrl Pts',(-4.80516962595556,1.90063102201579,47.5914636654409));
#59064=CARTESIAN_POINT('Ctrl Pts',(-4.20302819966638,-3.00609503656556,
47.750224427687));
#59065=CARTESIAN_POINT('Ctrl Pts',(0.245853018125491,-5.16155109531365,
47.9089851899327));
#59066=CARTESIAN_POINT('Ctrl Pts',(4.46972204405066,-2.59299792999961,48.0677459521787));
#59067=CARTESIAN_POINT('Ctrl Pts',(4.60276492582317,2.34874614500311,48.2265067144246));
#59068=CARTESIAN_POINT('Ctrl Pts',(0.523216754197009,5.14084600471386,48.3852674766704));
#59069=CARTESIAN_POINT('Ctrl Pts',(-4.03519537273411,3.22788657172462,48.5440282389163));
#59070=CARTESIAN_POINT('Ctrl Pts',(-4.9004734378914,-1.63933324878614,48.7027890011622));
#59071=CARTESIAN_POINT('Ctrl Pts',(-1.2806885257803,-5.00618520592171,48.8615497634081));
#59072=CARTESIAN_POINT('Ctrl Pts',(3.51122164426531,-3.79122354667958,49.020310525654));
#59073=CARTESIAN_POINT('Ctrl Pts',(5.0895545138177,0.893581706914796,49.1790712878999));
#59074=CARTESIAN_POINT('Ctrl Pts',(2.00977162985725,4.76055368753214,49.3378320501457));
#59075=CARTESIAN_POINT('Ctrl Pts',(-2.90941563902232,4.27052152031426,49.4965928123917));
#59076=CARTESIAN_POINT('Ctrl Pts',(-5.1658168458108,-0.128022387073527,
49.6553535746375));
#59077=CARTESIAN_POINT('Ctrl Pts',(-2.69430468338317,-4.40939629531691,
49.8141143368835));
#59078=CARTESIAN_POINT('Ctrl Pts',(2.2431174238849,-4.6551560273227,49.9728750991294));
#59079=CARTESIAN_POINT('Ctrl Pts',(5.12756994789964,-0.640374769530455,
50.1316358613752));
#59080=CARTESIAN_POINT('Ctrl Pts',(3.31911383193326,3.96049703783808,50.2903966236212));
#59081=CARTESIAN_POINT('Ctrl Pts',(-1.52709664667054,4.93660098122003,50.4491573858669));
#59082=CARTESIAN_POINT('Ctrl Pts',(-4.975661628467,1.39457691614903,50.607918148113));
#59083=CARTESIAN_POINT('Ctrl Pts',(-3.87034910432713,-3.42380654048809,
50.7666789103588));
#59084=CARTESIAN_POINT('Ctrl Pts',(0.777225141445664,-5.10861766973804,
50.9254396726047));
#59085=CARTESIAN_POINT('Ctrl Pts',(4.71345919711634,-2.11786586288516,51.0842004348506));
#59086=CARTESIAN_POINT('Ctrl Pts',(4.33579142110028,2.81122147273531,51.2429611970965));
#59087=CARTESIAN_POINT('Ctrl Pts',(-0.0101251019801382,5.16739304663044,
51.4017219593423));
#59088=CARTESIAN_POINT('Ctrl Pts',(-4.34677482245307,2.79420866417363,51.5604827215882));
#59089=CARTESIAN_POINT('Ctrl Pts',(-4.7051234514512,-2.13632083794987,51.7192434838341));
#59090=CARTESIAN_POINT('Ctrl Pts',(-0.757199377814005,-5.111624254412,51.87800424608));
#59091=CARTESIAN_POINT('Ctrl Pts',(3.88373669535471,-3.40861301664037,52.0367650083259));
#59092=CARTESIAN_POINT('Ctrl Pts',(4.97015831465276,1.41406497140078,52.1955257705718));
#59093=CARTESIAN_POINT('Ctrl Pts',(1.50773922891819,4.94254750443899,52.3542865328176));
#59094=CARTESIAN_POINT('Ctrl Pts',(-3.33460885361675,3.94745958933536,52.5130472950636));
#59095=CARTESIAN_POINT('Ctrl Pts',(-5.12502105636793,-0.660463918651125,
52.6718080573094));
#59096=CARTESIAN_POINT('Ctrl Pts',(-2.22485744252472,-4.66391067415503,
52.8305688195554));
#59097=CARTESIAN_POINT('Ctrl Pts',(2.71156366187259,-4.39880391966578,52.9893295818012));
#59098=CARTESIAN_POINT('Ctrl Pts',(5.16627887713359,-0.107777454683187,
53.1480903440472));
#59099=CARTESIAN_POINT('Ctrl Pts',(2.89265785799892,4.28189022893068,53.306851106293));
#59100=CARTESIAN_POINT('Ctrl Pts',(-2.02841199016113,4.75264118298715,53.4656118685389));
#59101=CARTESIAN_POINT('Ctrl Pts',(-5.09301722627474,0.873629755058583,
53.6243726307848));
#59102=CARTESIAN_POINT('Ctrl Pts',(-3.49633752866489,-3.80495431006791,
53.7831333930307));
#59103=CARTESIAN_POINT('Ctrl Pts',(1.30029707219943,-5.00112796677752,53.9418941552766));
#59104=CARTESIAN_POINT('Ctrl Pts',(4.90686007449561,-1.62011654684958,54.1006549175225));
#59105=CARTESIAN_POINT('Ctrl Pts',(4.02251485462088,3.2436750238594,54.2594156797684));
#59106=CARTESIAN_POINT('Ctrl Pts',(-0.543358829519001,5.13875613338857,
54.4181764420142));
#59107=CARTESIAN_POINT('Ctrl Pts',(-4.61193391577151,2.33069066429059,54.5769372042602));
#59108=CARTESIAN_POINT('Ctrl Pts',(-4.4595262089542,-2.61049409263942,54.735697966506));
#59109=CARTESIAN_POINT('Ctrl Pts',(-0.22562389770033,-5.16247491740555,
54.8944587287519));
#59110=CARTESIAN_POINT('Ctrl Pts',(4.21477629650059,-2.98960100791253,55.0532194909978));
#59111=CARTESIAN_POINT('Ctrl Pts',(4.79768448212587,1.91944706257383,55.2119802532437));
#59112=CARTESIAN_POINT('Ctrl Pts',(0.989605282528937,5.07175855111871,55.3707410154895));
#59113=CARTESIAN_POINT('Ctrl Pts',(-3.72419089952545,3.58224169479765,55.5295017777355));
#59114=CARTESIAN_POINT('Ctrl Pts',(-5.0294938134419,-1.1858521815995,55.6882625399813));
#59115=CARTESIAN_POINT('Ctrl Pts',(-1.7316503614075,-4.86861791907028,55.8470233022273));
#59116=CARTESIAN_POINT('Ctrl Pts',(3.15105239533607,-4.09547582313724,56.0057840644731));
#59117=CARTESIAN_POINT('Ctrl Pts',(5.14981574971942,0.425970844068908,56.1645448267191));
#59118=CARTESIAN_POINT('Ctrl Pts',(2.43531042678924,4.55755598333432,56.3233055889649));
#59119=CARTESIAN_POINT('Ctrl Pts',(-2.50806538626398,4.517926674292,56.4820663512109));
#59120=CARTESIAN_POINT('Ctrl Pts',(-5.1559831479537,0.343352871070528,56.6408271134567));
#59121=CARTESIAN_POINT('Ctrl Pts',(-3.08498764108028,-4.14546796760472,
56.7995878757026));
#59122=CARTESIAN_POINT('Ctrl Pts',(1.8094827870843,-4.8402298973603,56.9583486379485));
#59123=CARTESIAN_POINT('Ctrl Pts',(5.04785929713791,-1.10506557830443,57.1171094001944));
#59124=CARTESIAN_POINT('Ctrl Pts',(3.66628078958101,3.64148851268323,57.2758701624403));
#59125=CARTESIAN_POINT('Ctrl Pts',(-1.07078988460527,5.05524108614831,57.4346309246862));
#59126=CARTESIAN_POINT('Ctrl Pts',(-4.82784094869794,1.84228260322088,57.593391686932));
#59127=CARTESIAN_POINT('Ctrl Pts',(-4.16630450822031,-3.05678919142909,
57.7521524491779));
#59128=CARTESIAN_POINT('Ctrl Pts',(0.308361079608735,-5.1581941472416,57.9109132114238));
#59129=CARTESIAN_POINT('Ctrl Pts',(4.50080518836808,-2.53866226040682,58.0696739736697));
#59130=CARTESIAN_POINT('Ctrl Pts',(4.57397490984839,2.40433087160068,58.2284347359156));
#59131=CARTESIAN_POINT('Ctrl Pts',(0.460903079952699,5.14680694867653,58.3871954981615));
#59132=CARTESIAN_POINT('Ctrl Pts',(-4.07400132718361,3.17876809505837,58.5459562604074));
#59133=CARTESIAN_POINT('Ctrl Pts',(-4.88025527769062,-1.69857641589297,
58.7047170226532));
#59134=CARTESIAN_POINT('Ctrl Pts',(-1.21995052871669,-5.02133190732686,
58.8634777848992));
#59135=CARTESIAN_POINT('Ctrl Pts',(3.55689020801282,-3.74841105859499,59.022238547145));
#59136=CARTESIAN_POINT('Ctrl Pts',(5.07835637974298,0.955170087669591,59.1809993093909));
#59137=CARTESIAN_POINT('Ctrl Pts',(1.95195567231696,4.78455039364876,59.3397600716368));
#59138=CARTESIAN_POINT('Ctrl Pts',(-2.96093448967591,4.23496403336588,59.4985208338827));
#59139=CARTESIAN_POINT('Ctrl Pts',(-5.16388696379574,-0.190590768914221,
59.6572815961286));
#59140=CARTESIAN_POINT('Ctrl Pts',(-2.6406923556686,-4.44171107781315,59.8160423583745));
#59141=CARTESIAN_POINT('Ctrl Pts',(2.29934455736468,-4.62764173446609,59.9748031206204));
#59142=CARTESIAN_POINT('Ctrl Pts',(5.13495109710383,-0.578213322578349,
60.1335638828663));
#59143=CARTESIAN_POINT('Ctrl Pts',(3.27089354364999,4.00041358388897,60.2923246451122));
#59144=CARTESIAN_POINT('Ctrl Pts',(-1.58678569169648,4.91773978415717,60.451085407358));
#59145=CARTESIAN_POINT('Ctrl Pts',(-4.99219019300232,1.33420031964711,60.6098461696039));
#59146=CARTESIAN_POINT('Ctrl Pts',(-3.82858974123746,-3.47044003108337,
60.7686069318499));
#59147=CARTESIAN_POINT('Ctrl Pts',(0.839052987504236,-5.09882765939536,
60.9273676940957));
#59148=CARTESIAN_POINT('Ctrl Pts',(4.73876879287487,-2.06061246810993,61.0861284563416));
#59149=CARTESIAN_POINT('Ctrl Pts',(4.30141865142892,2.86353819621711,61.2448892185875));
#59150=CARTESIAN_POINT('Ctrl Pts',(-0.0727212283482856,5.16689123545314,
61.4036499808334));
#59151=CARTESIAN_POINT('Ctrl Pts',(-4.38030441864225,2.74134759125467,61.5624107430792));
#59152=CARTESIAN_POINT('Ctrl Pts',(-4.67889920685427,-2.19316110401252,
61.7211715053253));
#59153=CARTESIAN_POINT('Ctrl Pts',(-0.695222522116061,-5.12042176590928,
61.879932267571));
#59154=CARTESIAN_POINT('Ctrl Pts',(3.92474305071123,-3.3613160223265,62.038693029817));
#59155=CARTESIAN_POINT('Ctrl Pts',(4.95266390069012,1.47416881762428,62.1974537920629));
#59156=CARTESIAN_POINT('Ctrl Pts',(1.4477554676688,4.96044932661243,62.3562145543087));
#59157=CARTESIAN_POINT('Ctrl Pts',(-3.38218299162958,3.90677509298738,62.5149753165547));
#59158=CARTESIAN_POINT('Ctrl Pts',(-5.11664426686392,-0.722499039738782,
62.6737360788005));
#59159=CARTESIAN_POINT('Ctrl Pts',(-2.16819641913028,-4.69051998227545,
62.8324968410464));
#59160=CARTESIAN_POINT('Ctrl Pts',(2.76465101981334,-4.3656337632353,62.9912576032923));
#59161=CARTESIAN_POINT('Ctrl Pts',(5.16720539805885,-0.0451861740625634,
63.1500183655382));
#59162=CARTESIAN_POINT('Ctrl Pts',(2.8405755616569,4.31661718184185,63.308779127784));
#59163=CARTESIAN_POINT('Ctrl Pts',(-2.08583579528372,4.72772064013601,63.46753989003));
#59164=CARTESIAN_POINT('Ctrl Pts',(-5.10322651969674,0.811869758470405,
63.6263006522758));
#59165=CARTESIAN_POINT('Ctrl Pts',(-3.44998845319957,-3.847029125032,63.7850614145218));
#59166=CARTESIAN_POINT('Ctrl Pts',(1.36078442693529,-4.98500944427043,63.9438221767676));
#59167=CARTESIAN_POINT('Ctrl Pts',(4.92612583383742,-1.56055685101642,64.1025829390136));
#59168=CARTESIAN_POINT('Ctrl Pts',(3.98292640713875,3.29216504011747,64.2613437012594));
#59169=CARTESIAN_POINT('Ctrl Pts',(-0.605568927444514,5.13179692604536,
64.4201044635054));
#59170=CARTESIAN_POINT('Ctrl Pts',(-4.63982908228685,2.27465151247837,64.5788652257511));
#59171=CARTESIAN_POINT('Ctrl Pts',(-4.42757593559553,-2.66432444544396,
64.7376259879972));
#59172=CARTESIAN_POINT('Ctrl Pts',(-0.163070050579303,-5.16482928804609,
64.8963867502428));
#59173=CARTESIAN_POINT('Ctrl Pts',(4.25068252576661,-2.93832460446375,65.0551475124889));
#59174=CARTESIAN_POINT('Ctrl Pts',(4.77408061574266,1.97742450941745,65.2139082747347));
#59175=CARTESIAN_POINT('Ctrl Pts',(0.928094299999949,5.08337431106172,65.3726690369806));
#59176=CARTESIAN_POINT('Ctrl Pts',(-3.76731226811231,3.53686466953228,65.5314297992265));
#59177=CARTESIAN_POINT('Ctrl Pts',(-5.01475957439658,-1.24669155249126,
65.6901905614724));
#59178=CARTESIAN_POINT('Ctrl Pts',(-1.67254574036732,-4.88923758498539,
65.8489513237183));
#59179=CARTESIAN_POINT('Ctrl Pts',(3.20043304382085,-4.05700403599433,66.0077120859643));
#59180=CARTESIAN_POINT('Ctrl Pts',(5.14427774780404,0.488323529540513,66.16647284821));
#59181=CARTESIAN_POINT('Ctrl Pts',(2.3799223229872,4.58672248480354,66.3252336104561));
#59182=CARTESIAN_POINT('Ctrl Pts',(-2.56261070750152,4.48721291871176,66.4839943727018));
#59183=CARTESIAN_POINT('Ctrl Pts',(-5.15976414252148,0.280869025711643,
66.6427551349478));
#59184=CARTESIAN_POINT('Ctrl Pts',(-3.03454382725794,-4.18253477887576,
66.8015158971936));
#59185=CARTESIAN_POINT('Ctrl Pts',(1.86798369006022,-4.81795499664787,66.9602766594396));
#59186=CARTESIAN_POINT('Ctrl Pts',(5.06087547593053,-1.04383563513614,67.1190374216854));
#59187=CARTESIAN_POINT('Ctrl Pts',(3.62189943977487,3.68563398402679,67.2777981839313));
#59188=CARTESIAN_POINT('Ctrl Pts',(-1.13194959602156,5.04189880185246,67.4365589461772));
#59189=CARTESIAN_POINT('Ctrl Pts',(-4.84980378568845,1.78366382941869,67.5953197084231));
#59190=CARTESIAN_POINT('Ctrl Pts',(-4.12896941150786,-3.10703476242022,
67.754080470669));
#59191=CARTESIAN_POINT('Ctrl Pts',(0.370823889097725,-5.15408023407956,
67.9128412329148));
#59192=CARTESIAN_POINT('Ctrl Pts',(4.53122783943781,-2.48395404207855,68.0716019951608));
#59193=CARTESIAN_POINT('Ctrl Pts',(4.5445136629679,2.45956276259679,68.2303627574067));
#59194=CARTESIAN_POINT('Ctrl Pts',(0.398521768172548,5.15201259862078,68.3891235196525));
#59195=CARTESIAN_POINT('Ctrl Pts',(-4.11220942186021,3.12918313411324,68.5478842818985));
#59196=CARTESIAN_POINT('Ctrl Pts',(-4.85932093993431,-1.75757031687816,
68.7066450441443));
#59197=CARTESIAN_POINT('Ctrl Pts',(-1.15903350388962,-5.03574172817834,
68.8654058063903));
#59198=CARTESIAN_POINT('Ctrl Pts',(3.60203679805415,-3.70504849111566,69.0241665686361));
#59199=CARTESIAN_POINT('Ctrl Pts',(5.06641299677213,1.01661829719571,69.182927330882));
#59200=CARTESIAN_POINT('Ctrl Pts',(1.89385326524434,4.80784496690336,69.3416880931279));
#59201=CARTESIAN_POINT('Ctrl Pts',(-3.01201882313635,4.19878506536444,69.5004488553738));
#59202=CARTESIAN_POINT('Ctrl Pts',(-5.16119928126974,-0.25313118155592,
69.6592096176196));
#59203=CARTESIAN_POINT('Ctrl Pts',(-2.58669250630018,-4.47337403912361,
69.8179703798655));
#59204=CARTESIAN_POINT('Ctrl Pts',(2.35523426198658,-4.5994483350962,69.9767311421114));
#59205=CARTESIAN_POINT('Ctrl Pts',(5.14157869213602,-0.51596702281012,70.1354919043573));
#59206=CARTESIAN_POINT('Ctrl Pts',(3.22219325167658,4.03974306916968,70.2942526666032));
#59207=CARTESIAN_POINT('Ctrl Pts',(-1.6462418758917,4.89815690868675,70.4530134288491));
#59208=CARTESIAN_POINT('Ctrl Pts',(-5.00798615353109,1.2736279292227,70.611774191095));
#59209=CARTESIAN_POINT('Ctrl Pts',(-3.78626853252985,-3.51656423453759,
70.7705349533408));
#59210=CARTESIAN_POINT('Ctrl Pts',(0.900757702520816,-5.08828939599587,
70.9292957155868));
#59211=CARTESIAN_POINT('Ctrl Pts',(4.76338297422217,-2.00305667841551,71.0880564778326));
#59212=CARTESIAN_POINT('Ctrl Pts',(4.26641464848803,2.9154346954137,71.2468172400786));
#59213=CARTESIAN_POINT('Ctrl Pts',(-0.135306682874774,5.16563118288797,
71.4055780023244));
#59214=CARTESIAN_POINT('Ctrl Pts',(-4.41319120507407,2.6880842255241,71.5643387645703));
#59215=CARTESIAN_POINT('Ctrl Pts',(-4.65198833370899,-2.24967952364111,
71.7230995268162));
#59216=CARTESIAN_POINT('Ctrl Pts',(-0.63314364249968,-5.12846785541421,
71.8818602890621));
#59217=CARTESIAN_POINT('Ctrl Pts',(3.9651734499498,-3.31352575482195,72.040621051308));
#59218=CARTESIAN_POINT('Ctrl Pts',(4.93444268320512,1.53405632954553,72.1993818135539));
#59219=CARTESIAN_POINT('Ctrl Pts',(1.38755924827672,4.97762320275213,72.3581425757998));
#59220=CARTESIAN_POINT('Ctrl Pts',(-3.42926079422353,3.86551727731956,72.5169033380456));
#59221=CARTESIAN_POINT('Ctrl Pts',(-5.10751660971561,-0.784428134078424,
72.6756641002916));
#59222=CARTESIAN_POINT('Ctrl Pts',(-2.1112172128698,-4.71644095649861,72.8344248625374));
#59223=CARTESIAN_POINT('Ctrl Pts',(2.81733266516402,-4.33182294996633,72.9931856247833));
#59224=CARTESIAN_POINT('Ctrl Pts',(5.16737363149282,0.0174117376300544,
73.1519463870293));
#59225=CARTESIAN_POINT('Ctrl Pts',(2.78807641079671,4.35071067109887,73.3107071492751));
#59226=CARTESIAN_POINT('Ctrl Pts',(-2.14295350396336,4.70210630419026,73.469467911521));
#59227=CARTESIAN_POINT('Ctrl Pts',(-5.11268691452911,0.749990619979619,
73.6282286737669));
#59228=CARTESIAN_POINT('Ctrl Pts',(-3.40313309186266,-3.88853938839824,
73.7869894360128));
#59229=CARTESIAN_POINT('Ctrl Pts',(1.42107208653042,-4.9681593715318,73.9457501982587));
#59230=CARTESIAN_POINT('Ctrl Pts',(4.94466868411869,-1.50076814343543,74.1045109605046));
#59231=CARTESIAN_POINT('Ctrl Pts',(3.94275346512999,3.34017193109278,74.2632717227505));
#59232=CARTESIAN_POINT('Ctrl Pts',(-0.667690158118302,5.12408462740484,
74.4220324849963));
#59233=CARTESIAN_POINT('Ctrl Pts',(-4.6670433537954,2.21827855551313,74.5807932472423));
#59234=CARTESIAN_POINT('Ctrl Pts',(-4.39497591538344,-2.71776380858505,
74.7395540094881));
#59235=CARTESIAN_POINT('Ctrl Pts',(-0.100492272925181,-5.16642571988962,
74.898314771734));
#59236=CARTESIAN_POINT('Ctrl Pts',(4.28596496729055,-2.88661700182285,75.0570755339799));
#59237=CARTESIAN_POINT('Ctrl Pts',(4.74977615293751,2.03511176917654,75.2158362962258));
#59238=CARTESIAN_POINT('Ctrl Pts',(0.866447119614458,5.09424408572719,75.3745970584717));
#59239=CARTESIAN_POINT('Ctrl Pts',(-3.8098807835517,3.4909686093087,75.5333578207175));
#59240=CARTESIAN_POINT('Ctrl Pts',(-4.99928941928749,-1.30734797137385,
75.6921185829635));
#59241=CARTESIAN_POINT('Ctrl Pts',(-1.61319567320764,-4.90913975519121,
75.8508793452094));
#59242=CARTESIAN_POINT('Ctrl Pts',(3.24934402869518,-4.01793688343129,76.0096401074552));
#59243=CARTESIAN_POINT('Ctrl Pts',(5.13798482303055,0.550604553524979,76.1684008697012));
#59244=CARTESIAN_POINT('Ctrl Pts',(2.32418496553848,4.61521588466023,76.3271616319469));
#59245=CARTESIAN_POINT('Ctrl Pts',(-2.61677996556865,4.45584066454958,76.485922394193));
#59246=CARTESIAN_POINT('Ctrl Pts',(-5.16278794160245,0.218343962817818,
76.6446831564387));
#59247=CARTESIAN_POINT('Ctrl Pts',(-2.98365469407069,-4.21898780308791,
76.8034439186847));
#59248=CARTESIAN_POINT('Ctrl Pts',(1.92621046639379,-4.79497306094723,76.9622046809306));
#59249=CARTESIAN_POINT('Ctrl Pts',(5.07314897115,-0.982452509068445,77.1209654431764));
#59250=CARTESIAN_POINT('Ctrl Pts',(3.5769865761566,3.7292385885125,77.2797262054224));
#59251=CARTESIAN_POINT('Ctrl Pts',(-1.19294319381297,5.02781661881079,77.4384869676682));
#59252=CARTESIAN_POINT('Ctrl Pts',(-4.87105491388051,1.72478330291522,77.5972477299142));
#59253=CARTESIAN_POINT('Ctrl Pts',(-4.09102838845504,-3.1568243760003,77.75600849216));
#59254=CARTESIAN_POINT('Ctrl Pts',(0.433232280173729,-5.14920995954434,
77.9147692544059));
#59255=CARTESIAN_POINT('Ctrl Pts',(4.56098553273524,-2.42888130344712,78.0735300166518));
#59256=CARTESIAN_POINT('Ctrl Pts',(4.51438550862023,2.51443371271033,78.2322907788977));
#59257=CARTESIAN_POINT('Ctrl Pts',(0.336081973315249,5.15646219061744,78.3910515411436));
#59258=CARTESIAN_POINT('Ctrl Pts',(-4.1498140497254,3.0791389654831,78.5498123033895));
#59259=CARTESIAN_POINT('Ctrl Pts',(-4.8376734967368,-1.81630629438564,78.7085730656354));
#59260=CARTESIAN_POINT('Ctrl Pts',(-1.0979463908737,-5.04941255383462,78.8673338278812));
#59261=CARTESIAN_POINT('Ctrl Pts',(3.64665478912629,-3.66114220769932,79.0260945901272));
#59262=CARTESIAN_POINT('Ctrl Pts',(5.05372611759689,1.07791731796727,79.184855352373));
#59263=CARTESIAN_POINT('Ctrl Pts',(1.83547293516864,4.83043398881696,79.3436161146189));
#59264=CARTESIAN_POINT('Ctrl Pts',(-3.06266114277673,4.16198992557408,79.5023768768648));
#59265=CARTESIAN_POINT('Ctrl Pts',(-5.15775419265022,-0.315634447191765,
79.6611376391107));
#59266=CARTESIAN_POINT('Ctrl Pts',(-2.53231305975701,-4.50438053270811,
79.8198984013567));
#59267=CARTESIAN_POINT('Ctrl Pts',(2.41077833593552,-4.57057996659486,79.9786591636024));
#59268=CARTESIAN_POINT('Ctrl Pts',(5.14745176039643,-0.453645004871452,
80.1374199258484));
#59269=CARTESIAN_POINT('Ctrl Pts',(3.1730201027819,4.07847972207792,80.2961806880942));
#59270=CARTESIAN_POINT('Ctrl Pts',(-1.70545647406065,4.87785522859546,80.4549414503402));
#59271=CARTESIAN_POINT('Ctrl Pts',(-5.02304719199465,1.21286863387634,80.613702212586));
#59272=CARTESIAN_POINT('Ctrl Pts',(-3.74339168884474,-3.56217238212488,
80.7724629748319));
#59273=CARTESIAN_POINT('Ctrl Pts',(0.962330231331446,-5.07700442602626,
80.9312237370778));
#59274=CARTESIAN_POINT('Ctrl Pts',(4.78729812901886,-1.94520694012218,81.0899844993237));
#59275=CARTESIAN_POINT('Ctrl Pts',(4.2307845491307,2.96690335452649,81.2487452615696));
#59276=CARTESIAN_POINT('Ctrl Pts',(-0.19787228117179,5.16361307382143,81.4075060238155));
#59277=CARTESIAN_POINT('Ctrl Pts',(-4.44543035555655,2.63442638343223,81.5662667860614));
#59278=CARTESIAN_POINT('Ctrl Pts',(-4.62439478129263,-2.30586780285272,
81.7250275483072));
#59279=CARTESIAN_POINT('Ctrl Pts',(-0.57097184883837,-5.13576134197884,
81.8837883105532));
#59280=CARTESIAN_POINT('Ctrl Pts',(4.00502195951943,-3.26524922770216,82.0425490727989));
#59281=CARTESIAN_POINT('Ctrl Pts',(4.91549733690694,1.59371871934676,82.2013098350451));
#59282=CARTESIAN_POINT('Ctrl Pts',(1.32715940311121,4.99406661129702,82.3600705972907));
#59283=CARTESIAN_POINT('Ctrl Pts',(-3.47583534999669,3.82369219939626,82.5188313595369));
#59284=CARTESIAN_POINT('Ctrl Pts',(-5.09763942964231,-0.846242118322492,
82.6775921217824));
#59285=CARTESIAN_POINT('Ctrl Pts',(-2.05392817541576,-4.74166978382725,
82.8363528840287));
#59286=CARTESIAN_POINT('Ctrl Pts',(2.86960084768762,-4.29737645901297,82.9951136462743));
#59287=CARTESIAN_POINT('Ctrl Pts',(5.16678358952832,0.0800071275065655,
83.1538744085204));
#59288=CARTESIAN_POINT('Ctrl Pts',(2.73516803922529,4.38416562959496,83.312635170766));
#59289=CARTESIAN_POINT('Ctrl Pts',(-2.19975659925683,4.67580205641259,83.4713959330121));
#59290=CARTESIAN_POINT('Ctrl Pts',(-5.1213972808606,0.688001186004659,83.6301566952579));
#59291=CARTESIAN_POINT('Ctrl Pts',(-3.35577782577649,-3.92947855970427,
83.7889174575038));
#59292=CARTESIAN_POINT('Ctrl Pts',(1.4811502559097,-4.9505810809301,83.9476782197498));
#59293=CARTESIAN_POINT('Ctrl Pts',(4.96248771955931,-1.44075755171813,84.1064389819956));
#59294=CARTESIAN_POINT('Ctrl Pts',(3.90199844707087,3.38768549854763,84.2651997442416));
#59295=CARTESIAN_POINT('Ctrl Pts',(-0.729706746127024,5.11562640844579,
84.4239605064874));
#59296=CARTESIAN_POINT('Ctrl Pts',(-4.69358549045032,2.16156849958318,84.5827212687333));
#59297=CARTESIAN_POINT('Ctrl Pts',(-4.36170650562841,-2.77078218706868,
84.7414820309791));
#59298=CARTESIAN_POINT('Ctrl Pts',(-0.0379465312430282,-5.16730640666113,
84.9002427932251));
#59299=CARTESIAN_POINT('Ctrl Pts',(4.32070804489202,-2.83440452778566,85.059003555471));
#59300=CARTESIAN_POINT('Ctrl Pts',(4.72460304963626,2.09234474027741,85.2177643177169));
#59301=CARTESIAN_POINT('Ctrl Pts',(0.805001482004623,5.10466438453535,85.3765250799626));
#59302=CARTESIAN_POINT('Ctrl Pts',(-3.85251988452798,3.44398909312549,85.5352858422087));
#59303=CARTESIAN_POINT('Ctrl Pts',(-4.98187820443228,-1.36671670879964,
85.6940466044544));
#59304=CARTESIAN_POINT('Ctrl Pts',(-1.55593411210757,-4.93043766489916,
85.8528073667005));
#59305=CARTESIAN_POINT('Ctrl Pts',(3.302346542614,-3.9740701687742,86.0115681289462));
#59306=CARTESIAN_POINT('Ctrl Pts',(4.81804045098618,-0.159581013320771,
86.1438687641512));
#59307=CARTESIAN_POINT('Ctrl Pts',(3.70615495334781,2.63929363226931,86.2497092723151));
#59308=CARTESIAN_POINT('Ctrl Pts',(2.57208606313468,3.6093054188893,86.3026295263971));
#59309=CARTESIAN_POINT('Ctrl Pts',(1.91898364244101,3.92834389788417,86.329089653438));
#59310=CARTESIAN_POINT('',(2.16917135428672,4.4405021828327,86.));
#59311=CARTESIAN_POINT('Ctrl Pts',(2.54472701347473,-3.56250531650751,85.9999999999999));
#59312=CARTESIAN_POINT('Ctrl Pts',(2.63513329971733,-3.50700228194743,85.9999999999999));
#59313=CARTESIAN_POINT('Ctrl Pts',(2.72315806304114,-3.44815476600379,86.));
#59314=CARTESIAN_POINT('Ctrl Pts',(2.80858471961567,-3.38601400582831,86.));
#59315=CARTESIAN_POINT('Ctrl Pts',(2.91292188753961,-3.31011742753144,86.));
#59316=CARTESIAN_POINT('Ctrl Pts',(3.01338478767473,-3.22930990203852,85.9999999999999));
#59317=CARTESIAN_POINT('Ctrl Pts',(3.1098984160813,-3.14401909712343,85.9999999999999));
#59318=CARTESIAN_POINT('Ctrl Pts',(3.20859981088314,-3.05679492424881,85.9999999999999));
#59319=CARTESIAN_POINT('Ctrl Pts',(3.30317129552995,-2.96488147836652,85.9999999999999));
#59320=CARTESIAN_POINT('Ctrl Pts',(3.39350543356314,-2.86868861821106,85.9999999999999));
#59321=CARTESIAN_POINT('Ctrl Pts',(3.48531110601377,-2.77092878561846,85.9999999999999));
#59322=CARTESIAN_POINT('Ctrl Pts',(3.57274072745551,-2.66874842101355,86.));
#59323=CARTESIAN_POINT('Ctrl Pts',(3.65564683072142,-2.56253686518592,86.));
#59324=CARTESIAN_POINT('Ctrl Pts',(3.68584784338838,-2.52384614862143,86.));
#59325=CARTESIAN_POINT('Ctrl Pts',(3.71544822227817,-2.48462014936941,86.));
#59326=CARTESIAN_POINT('Ctrl Pts',(3.74443952828415,-2.44487660282335,86.));
#59327=CARTESIAN_POINT('Ctrl Pts',(3.75595083040377,-2.42909601082439,86.));
#59328=CARTESIAN_POINT('Ctrl Pts',(3.76736609971463,-2.41323381819194,86.));
#59329=CARTESIAN_POINT('Ctrl Pts',(3.77868477502221,-2.39729111372332,86.));
#59330=CARTESIAN_POINT('Ctrl Pts',(3.78947724093788,-2.38208959146869,86.));
#59331=CARTESIAN_POINT('Ctrl Pts',(3.80017685936615,-2.36682191965604,86.));
#59332=CARTESIAN_POINT('Ctrl Pts',(3.81078105898287,-2.35149266837476,86.));
#59333=CARTESIAN_POINT('Ctrl Pts',(3.88827217096444,-2.23947282995537,86.));
#59334=CARTESIAN_POINT('Ctrl Pts',(3.96071122105411,-2.12411080348259,86.));
#59335=CARTESIAN_POINT('Ctrl Pts',(4.02800505520053,-2.00585829504273,86.));
#59336=CARTESIAN_POINT('Ctrl Pts',(4.09627718657597,-1.88588666771479,86.));
#59337=CARTESIAN_POINT('Ctrl Pts',(4.15925387587574,-1.76293927819734,86.));
#59338=CARTESIAN_POINT('Ctrl Pts',(4.21680206540741,-1.63744665973299,86.));
#59339=CARTESIAN_POINT('Ctrl Pts',(4.27457311504665,-1.5114680607595,86.));
#59340=CARTESIAN_POINT('Ctrl Pts',(4.32687396830893,-1.38292375176368,86.));
#59341=CARTESIAN_POINT('Ctrl Pts',(4.37352758038542,-1.25221847894515,86.));
#59342=CARTESIAN_POINT('Ctrl Pts',(4.41978765417706,-1.1226157473147,86.));
#59343=CARTESIAN_POINT('Ctrl Pts',(4.46049570285582,-0.990887588742712,
86.));
#59344=CARTESIAN_POINT('Ctrl Pts',(4.49543183958698,-0.857409609773572,
86.));
#59345=CARTESIAN_POINT('Ctrl Pts',(4.5001149290464,-0.839517267492425,86.));
#59346=CARTESIAN_POINT('Ctrl Pts',(4.50469423047283,-0.821593465132248,
86.));
#59347=CARTESIAN_POINT('Ctrl Pts',(4.50916914362169,-0.803639092756939,
86.));
#59348=CARTESIAN_POINT('Ctrl Pts',(4.51380380131252,-0.785043788838134,
86.));
#59349=CARTESIAN_POINT('Ctrl Pts',(4.5183245524103,-0.76642335069997,86.));
#59350=CARTESIAN_POINT('Ctrl Pts',(4.52272974339821,-0.747784414927894,
86.));
#59351=CARTESIAN_POINT('Ctrl Pts',(4.55525927718291,-0.610147728443155,
86.));
#59352=CARTESIAN_POINT('Ctrl Pts',(4.58151477805167,-0.471409643850918,
86.));
#59353=CARTESIAN_POINT('Ctrl Pts',(4.60136007125311,-0.332008493005429,
86.));
#59354=CARTESIAN_POINT('Ctrl Pts',(4.6211606972018,-0.19292110252501,86.));
#59355=CARTESIAN_POINT('Ctrl Pts',(4.63458031267456,-0.0531728409362625,
86.));
#59356=CARTESIAN_POINT('Ctrl Pts',(4.64143733545588,0.0868237683291349,
86.));
#59357=CARTESIAN_POINT('Ctrl Pts',(4.64817665416128,0.224417268832664,86.));
#59358=CARTESIAN_POINT('Ctrl Pts',(4.64857698604029,0.362251427033831,86.));
#59359=CARTESIAN_POINT('Ctrl Pts',(4.64241679650986,0.499945184924937,86.));
#59360=CARTESIAN_POINT('Ctrl Pts',(4.64160900570028,0.518001082655194,86.));
#59361=CARTESIAN_POINT('Ctrl Pts',(4.64068833141729,0.536054571915867,86.));
#59362=CARTESIAN_POINT('Ctrl Pts',(4.63965420661563,0.554104796667351,86.));
#59363=CARTESIAN_POINT('Ctrl Pts',(4.63402930249198,0.65228519372856,86.));
#59364=CARTESIAN_POINT('Ctrl Pts',(4.62504894974127,0.750369112179832,86.));
#59365=CARTESIAN_POINT('Ctrl Pts',(4.61279339604946,0.848217515281527,86.));
#59366=CARTESIAN_POINT('Ctrl Pts',(4.6078781705278,0.887460700883271,86.));
#59367=CARTESIAN_POINT('Ctrl Pts',(4.60243597814028,0.926665987486628,86.));
#59368=CARTESIAN_POINT('Ctrl Pts',(4.59647140132863,0.965824309598894,86.));
#59369=CARTESIAN_POINT('Ctrl Pts',(4.59357119157143,0.984864612281179,86.));
#59370=CARTESIAN_POINT('Ctrl Pts',(4.59054712512505,1.00389559177027,86.));
#59371=CARTESIAN_POINT('Ctrl Pts',(4.58740263898465,1.02289935437782,86.));
#59372=CARTESIAN_POINT('Ctrl Pts',(4.56506277525981,1.15791075145704,86.));
#59373=CARTESIAN_POINT('Ctrl Pts',(4.53662319345842,1.29172741325957,86.));
#59374=CARTESIAN_POINT('Ctrl Pts',(4.50239447214487,1.42398414516775,86.));
#59375=CARTESIAN_POINT('Ctrl Pts',(4.46711335178721,1.56030725329147,86.));
#59376=CARTESIAN_POINT('Ctrl Pts',(4.42568158764605,1.6949737254632,86.));
#59377=CARTESIAN_POINT('Ctrl Pts',(4.3783840316949,1.82758749733868,86.));
#59378=CARTESIAN_POINT('Ctrl Pts',(4.33065091250152,1.96142250957807,86.));
#59379=CARTESIAN_POINT('Ctrl Pts',(4.27694321392572,2.09316762674784,86.));
#59380=CARTESIAN_POINT('Ctrl Pts',(4.21750086301315,2.22240829814259,86.));
#59381=CARTESIAN_POINT('Ctrl Pts',(4.17317829962387,2.31877524464499,86.));
#59382=CARTESIAN_POINT('Ctrl Pts',(4.12566627444568,2.41374969077583,86.));
#59383=CARTESIAN_POINT('Ctrl Pts',(4.07504671027994,2.5071531160556,86.));
#59384=CARTESIAN_POINT('Ctrl Pts',(4.04973692819707,2.55385482869548,86.));
#59385=CARTESIAN_POINT('Ctrl Pts',(4.02365003622111,2.60016367547768,86.));
#59386=CARTESIAN_POINT('Ctrl Pts',(3.99679497172134,2.64605655812716,86.));
#59387=CARTESIAN_POINT('Ctrl Pts',(3.98389889010003,2.66809479826952,86.));
#59388=CARTESIAN_POINT('Ctrl Pts',(3.97082565386207,2.69003710756834,86.));
#59389=CARTESIAN_POINT('Ctrl Pts',(3.95757618483902,2.71188087703549,86.));
#59390=CARTESIAN_POINT('Ctrl Pts',(3.94694273066632,2.72941174722991,86.));
#59391=CARTESIAN_POINT('Ctrl Pts',(3.93620106712467,2.74687039690698,86.));
#59392=CARTESIAN_POINT('Ctrl Pts',(3.92535253208302,2.76425480853107,86.));
#59393=CARTESIAN_POINT('Ctrl Pts',(3.92156948774113,2.770317009536,86.));
#59394=CARTESIAN_POINT('Ctrl Pts',(3.91777342701665,2.77637021666335,86.));
#59395=CARTESIAN_POINT('Ctrl Pts',(3.91396438452183,2.78241437972366,86.));
#59396=CARTESIAN_POINT('Ctrl Pts',(3.83729807392157,2.90406796671591,86.));
#59397=CARTESIAN_POINT('Ctrl Pts',(3.7553768005218,3.02205919675202,86.));
#59398=CARTESIAN_POINT('Ctrl Pts',(3.66851542581977,3.13614597147405,86.));
#59399=CARTESIAN_POINT('Ctrl Pts',(3.58104093093735,3.25103803973578,86.));
#59400=CARTESIAN_POINT('Ctrl Pts',(3.48855596305165,3.36197093402805,86.));
#59401=CARTESIAN_POINT('Ctrl Pts',(3.39133507740585,3.46867352459105,86.));
#59402=CARTESIAN_POINT('Ctrl Pts',(3.34733743007933,3.51696215020099,86.));
#59403=CARTESIAN_POINT('Ctrl Pts',(3.30236924503015,3.56438401262811,86.));
#59404=CARTESIAN_POINT('Ctrl Pts',(3.25645316546651,3.61091188198635,86.));
#59405=CARTESIAN_POINT('Ctrl Pts',(3.23459379362241,3.63306250998163,86.));
#59406=CARTESIAN_POINT('Ctrl Pts',(3.21251956234251,3.65501049805194,86.));
#59407=CARTESIAN_POINT('Ctrl Pts',(3.19023278769809,3.67675278772905,86.));
#59408=CARTESIAN_POINT('Ctrl Pts',(3.1754125274436,3.69121097634916,86.));
#59409=CARTESIAN_POINT('Ctrl Pts',(3.16050000228347,3.70557647179484,86.));
#59410=CARTESIAN_POINT('Ctrl Pts',(3.14550229693264,3.71984252397241,86.));
#59411=CARTESIAN_POINT('Ctrl Pts',(3.03965115782958,3.82052978500174,86.));
#59412=CARTESIAN_POINT('Ctrl Pts',(2.92947196960907,3.91635255577481,86.));
#59413=CARTESIAN_POINT('Ctrl Pts',(2.81526020000344,4.00704611824462,86.));
#59414=CARTESIAN_POINT('Ctrl Pts',(2.7017209514917,4.09720564351275,86.));
#59415=CARTESIAN_POINT('Ctrl Pts',(2.58419598194515,4.18229672829323,86.));
#59416=CARTESIAN_POINT('Ctrl Pts',(2.46293629783775,4.26202671871549,86.));
#59417=CARTESIAN_POINT('Ctrl Pts',(2.3673022580591,4.32490747856343,86.));
#59418=CARTESIAN_POINT('Ctrl Pts',(2.26934437440973,4.38445308888104,86.));
#59419=CARTESIAN_POINT('Ctrl Pts',(2.16917135428672,4.4405021828327,86.));
#59420=CARTESIAN_POINT('Ctrl Pts',(2.17574200330365,4.44486699004439,26.));
#59421=CARTESIAN_POINT('Ctrl Pts',(2.28006508424018,4.38720334283182,26.));
#59422=CARTESIAN_POINT('Ctrl Pts',(2.38197081280219,4.32562977310065,26.));
#59423=CARTESIAN_POINT('Ctrl Pts',(2.48120802246663,4.26013719370393,26.));
#59424=CARTESIAN_POINT('Ctrl Pts',(2.60168389996394,4.18062794511602,26.));
#59425=CARTESIAN_POINT('Ctrl Pts',(2.71822805906223,4.09534340135309,26.));
#59426=CARTESIAN_POINT('Ctrl Pts',(2.83065917997165,4.00470474933307,26.));
#59427=CARTESIAN_POINT('Ctrl Pts',(2.90083958424456,3.94812737831637,26.));
#59428=CARTESIAN_POINT('Ctrl Pts',(2.96941670994451,3.88946302886519,26.));
#59429=CARTESIAN_POINT('Ctrl Pts',(3.03633883105725,3.82880744415046,26.));
#59430=CARTESIAN_POINT('Ctrl Pts',(3.07291548330716,3.79565580173034,26.));
#59431=CARTESIAN_POINT('Ctrl Pts',(3.10899764098955,3.76190925146565,26.));
#59432=CARTESIAN_POINT('Ctrl Pts',(3.14457605294962,3.72758291425312,26.));
#59433=CARTESIAN_POINT('Ctrl Pts',(3.16870678245731,3.70430139288574,26.));
#59434=CARTESIAN_POINT('Ctrl Pts',(3.19260993644808,3.68074881011364,26.));
#59435=CARTESIAN_POINT('Ctrl Pts',(3.21625888633569,3.65695400262287,26.));
#59436=CARTESIAN_POINT('Ctrl Pts',(3.31788256697706,3.55470354630845,26.));
#59437=CARTESIAN_POINT('Ctrl Pts',(3.41488652713577,3.44791753206169,26.));
#59438=CARTESIAN_POINT('Ctrl Pts',(3.50709206651038,3.33701451625688,26.));
#59439=CARTESIAN_POINT('Ctrl Pts',(3.59746145912339,3.2283199817939,26.));
#59440=CARTESIAN_POINT('Ctrl Pts',(3.6832218206498,3.11566998580718,26.));
#59441=CARTESIAN_POINT('Ctrl Pts',(3.76416544626806,2.99943221817338,26.));
#59442=CARTESIAN_POINT('Ctrl Pts',(3.79957828247605,2.94857819483358,26.));
#59443=CARTESIAN_POINT('Ctrl Pts',(3.83406863332226,2.89703717531663,26.));
#59444=CARTESIAN_POINT('Ctrl Pts',(3.86761651871398,2.84483889381663,26.));
#59445=CARTESIAN_POINT('Ctrl Pts',(3.89532327236222,2.80172902535561,26.));
#59446=CARTESIAN_POINT('Ctrl Pts',(3.92238715315105,2.75817083249342,26.));
#59447=CARTESIAN_POINT('Ctrl Pts',(3.94879604378199,2.71418084548941,26.));
#59448=CARTESIAN_POINT('Ctrl Pts',(3.95941005243527,2.69650081079038,26.));
#59449=CARTESIAN_POINT('Ctrl Pts',(3.96991386666906,2.6787582983834,26.));
#59450=CARTESIAN_POINT('Ctrl Pts',(3.98030512442337,2.6609577203422,26.));
#59451=CARTESIAN_POINT('Ctrl Pts',(4.05292301831336,2.53656079766556,26.));
#59452=CARTESIAN_POINT('Ctrl Pts',(4.12007774857859,2.40928022608588,26.));
#59453=CARTESIAN_POINT('Ctrl Pts',(4.18159035621228,2.27951928558395,26.));
#59454=CARTESIAN_POINT('Ctrl Pts',(4.24297458767659,2.15002915480893,26.));
#59455=CARTESIAN_POINT('Ctrl Pts',(4.29874053362767,2.01806821927191,26.));
#59456=CARTESIAN_POINT('Ctrl Pts',(4.34866300062458,1.88401668144009,26.));
#59457=CARTESIAN_POINT('Ctrl Pts',(4.39830723531613,1.75071225148679,26.));
#59458=CARTESIAN_POINT('Ctrl Pts',(4.44217322437405,1.61533971306916,26.));
#59459=CARTESIAN_POINT('Ctrl Pts',(4.47998827572883,1.47826395773052,26.));
#59460=CARTESIAN_POINT('Ctrl Pts',(4.50834956424491,1.37545714122654,26.));
#59461=CARTESIAN_POINT('Ctrl Pts',(4.53330618455047,1.27169201598405,26.));
#59462=CARTESIAN_POINT('Ctrl Pts',(4.55472254010161,1.16712293514026,26.));
#59463=CARTESIAN_POINT('Ctrl Pts',(4.5633703360405,1.12489856739035,26.));
#59464=CARTESIAN_POINT('Ctrl Pts',(4.57144068485198,1.0825431363053,26.));
#59465=CARTESIAN_POINT('Ctrl Pts',(4.57892379357549,1.04006693008015,26.));
#59466=CARTESIAN_POINT('Ctrl Pts',(4.58238261217842,1.02043371376567,26.));
#59467=CARTESIAN_POINT('Ctrl Pts',(4.58571635833316,1.00077225530923,26.));
#59468=CARTESIAN_POINT('Ctrl Pts',(4.58892275403614,0.98109144089082,26.));
#59469=CARTESIAN_POINT('Ctrl Pts',(4.6112579051569,0.843998578707096,26.));
#59470=CARTESIAN_POINT('Ctrl Pts',(4.62736483254579,0.706302385469903,26.));
#59471=CARTESIAN_POINT('Ctrl Pts',(4.63704039371253,0.568349643633761,26.));
#59472=CARTESIAN_POINT('Ctrl Pts',(4.64529719664733,0.450625350021645,26.));
#59473=CARTESIAN_POINT('Ctrl Pts',(4.64886975587046,0.332713782967315,26.));
#59474=CARTESIAN_POINT('Ctrl Pts',(4.64760179618238,0.214828774577272,26.));
#59475=CARTESIAN_POINT('Ctrl Pts',(4.64610810169851,0.0759567044171535,
26.));
#59476=CARTESIAN_POINT('Ctrl Pts',(4.63789790766952,-0.0628793196366818,
26.));
#59477=CARTESIAN_POINT('Ctrl Pts',(4.62316922884463,-0.20123695388626,26.));
#59478=CARTESIAN_POINT('Ctrl Pts',(4.60840903270106,-0.339890654178337,
26.));
#59479=CARTESIAN_POINT('Ctrl Pts',(4.58710205140909,-0.478064733297057,
26.));
#59480=CARTESIAN_POINT('Ctrl Pts',(4.55939920087044,-0.615294818730504,
26.));
#59481=CARTESIAN_POINT('Ctrl Pts',(4.54980593455313,-0.66281645389487,26.));
#59482=CARTESIAN_POINT('Ctrl Pts',(4.53944529005038,-0.710224661945217,
26.));
#59483=CARTESIAN_POINT('Ctrl Pts',(4.52832231101321,-0.757499347947085,
26.));
#59484=CARTESIAN_POINT('Ctrl Pts',(4.52204558440698,-0.784176578789409,
26.));
#59485=CARTESIAN_POINT('Ctrl Pts',(4.51552434543633,-0.81081776400017,26.));
#59486=CARTESIAN_POINT('Ctrl Pts',(4.50876854798769,-0.837384466189193,
26.));
#59487=CARTESIAN_POINT('Ctrl Pts',(4.47488762719443,-0.97061882370914,26.));
#59488=CARTESIAN_POINT('Ctrl Pts',(4.43508456291388,-1.10210853291686,26.));
#59489=CARTESIAN_POINT('Ctrl Pts',(4.38958618794437,-1.2314396670372,26.));
#59490=CARTESIAN_POINT('Ctrl Pts',(4.34401166128567,-1.36098726568698,26.));
#59491=CARTESIAN_POINT('Ctrl Pts',(4.29272234355304,-1.48836984485114,26.));
#59492=CARTESIAN_POINT('Ctrl Pts',(4.23589771868779,-1.61315285151403,26.));
#59493=CARTESIAN_POINT('Ctrl Pts',(4.18015009153959,-1.73557084452973,26.));
#59494=CARTESIAN_POINT('Ctrl Pts',(4.11907449353476,-1.85548750502406,26.));
#59495=CARTESIAN_POINT('Ctrl Pts',(4.05280063784894,-1.97246430242313,26.));
#59496=CARTESIAN_POINT('Ctrl Pts',(4.0071971296468,-2.0529568629426,26.));
#59497=CARTESIAN_POINT('Ctrl Pts',(3.95913143391569,-2.13205676654158,26.));
#59498=CARTESIAN_POINT('Ctrl Pts',(3.90866288715487,-2.2096607611529,26.));
#59499=CARTESIAN_POINT('Ctrl Pts',(3.88457170018092,-2.24670506823327,26.));
#59500=CARTESIAN_POINT('Ctrl Pts',(3.85993289144,-2.28340838898037,26.));
#59501=CARTESIAN_POINT('Ctrl Pts',(3.83475240364166,-2.31975877789511,26.));
#59502=CARTESIAN_POINT('Ctrl Pts',(3.81911152043036,-2.34233785548306,26.));
#59503=CARTESIAN_POINT('Ctrl Pts',(3.80326163575805,-2.36478075250477,26.));
#59504=CARTESIAN_POINT('Ctrl Pts',(3.78720411571068,-2.38708450953735,26.));
#59505=CARTESIAN_POINT('Ctrl Pts',(3.77570997324099,-2.40304977442168,26.));
#59506=CARTESIAN_POINT('Ctrl Pts',(3.76411377204687,-2.41893767166227,26.));
#59507=CARTESIAN_POINT('Ctrl Pts',(3.75242084457745,-2.43474120045983,26.));
#59508=CARTESIAN_POINT('Ctrl Pts',(3.66959100122522,-2.54668954001269,26.));
#59509=CARTESIAN_POINT('Ctrl Pts',(3.58184107407233,-2.65450498805187,26.));
#59510=CARTESIAN_POINT('Ctrl Pts',(3.48944434360053,-2.75789800803035,26.));
#59511=CARTESIAN_POINT('Ctrl Pts',(3.40008035358429,-2.85789735603679,26.));
#59512=CARTESIAN_POINT('Ctrl Pts',(3.3063688476751,-2.95376016129811,26.));
#59513=CARTESIAN_POINT('Ctrl Pts',(3.20852006341883,-3.04518760514634,26.));
#59514=CARTESIAN_POINT('Ctrl Pts',(3.11161693078311,-3.13573145589637,26.));
#59515=CARTESIAN_POINT('Ctrl Pts',(3.01065557724222,-3.2219256920299,26.));
#59516=CARTESIAN_POINT('Ctrl Pts',(2.90581240538358,-3.30343749134566,26.));
#59517=CARTESIAN_POINT('Ctrl Pts',(2.80309976478498,-3.38329287915244,26.));
#59518=CARTESIAN_POINT('Ctrl Pts',(2.69666097167601,-3.45865450573126,26.));
#59519=CARTESIAN_POINT('Ctrl Pts',(2.58664264704464,-3.52916309203659,26.));
#59520=CARTESIAN_POINT('Ctrl Pts',(2.57062378681069,-3.53942926535911,26.));
#59521=CARTESIAN_POINT('Ctrl Pts',(2.55452901448013,-3.54959246856517,26.));
#59522=CARTESIAN_POINT('Ctrl Pts',(2.53835875722658,-3.55965150255066,26.));
#59523=CARTESIAN_POINT('Ctrl Pts',(2.16917135428672,4.4405021828327,86.));
#59524=CARTESIAN_POINT('Ctrl Pts',(2.90742207776984,4.07986902565238,85.973539872959));
#59525=CARTESIAN_POINT('Ctrl Pts',(3.54838370350565,3.53163043353487,85.947079745918));
#59526=CARTESIAN_POINT('Ctrl Pts',(4.02597047844268,2.86203885652618,85.9206196188771));
#59527=CARTESIAN_POINT('Ctrl Pts',(4.50355725337971,2.19244727951748,85.894159491836));
#59528=CARTESIAN_POINT('Ctrl Pts',(4.817769177518,1.40150271761755,85.8676993647951));
#59529=CARTESIAN_POINT('Ctrl Pts',(4.91302361527573,0.586752768661848,85.8412392377541));
#59530=CARTESIAN_POINT('Ctrl Pts',(5.10353249079119,-1.04274712924955,85.7883189836721));
#59531=CARTESIAN_POINT('Ctrl Pts',(4.41821142078444,-2.76746857538425,85.7353987295902));
#59532=CARTESIAN_POINT('Ctrl Pts',(3.16027096066549,-3.81000496808603,85.6824784755082));
#59533=CARTESIAN_POINT('Ctrl Pts',(1.90233050054647,-4.85254136078787,85.6295582214263));
#59534=CARTESIAN_POINT('Ctrl Pts',(0.071770650315324,-5.21289270005682,
85.5766379673442));
#59535=CARTESIAN_POINT('Ctrl Pts',(-1.4889429323282,-4.72167812247258,85.5237177132623));
#59536=CARTESIAN_POINT('Ctrl Pts',(-3.04965651497173,-4.23046354488835,
85.4707974591803));
#59537=CARTESIAN_POINT('Ctrl Pts',(-4.34052383002751,-2.88768305045078,
85.4178772050984));
#59538=CARTESIAN_POINT('Ctrl Pts',(-4.77319106421879,-1.30997578306141,
85.3649569510165));
#59539=CARTESIAN_POINT('Ctrl Pts',(-4.88938737554012,-0.886269640491669,
85.3507447855632));
#59540=CARTESIAN_POINT('Ctrl Pts',(-4.94368731125384,-0.445619761719663,
85.33653262011));
#59541=CARTESIAN_POINT('Ctrl Pts',(-4.93983901057914,-0.00407131671605609,
85.3223204546568));
#59542=CARTESIAN_POINT('Origin',(0.,0.,16.));
#59543=CARTESIAN_POINT('Origin',(0.,0.,86.));
#59544=CARTESIAN_POINT('Origin',(0.,0.,26.));
#59545=CARTESIAN_POINT('',(4.61880215351701,-8.,26.));
#59546=CARTESIAN_POINT('',(9.23760430703401,0.,26.));
#59547=CARTESIAN_POINT('',(4.61880215351701,-8.,26.));
#59548=CARTESIAN_POINT('',(4.61880215351701,8.,26.));
#59549=CARTESIAN_POINT('',(9.23760430703401,0.,26.));
#59550=CARTESIAN_POINT('',(-4.61880215351701,8.,26.));
#59551=CARTESIAN_POINT('',(4.61880215351701,8.,26.));
#59552=CARTESIAN_POINT('',(-9.23760430703401,1.11022302462516E-15,26.));
#59553=CARTESIAN_POINT('',(-4.618802153517,8.,26.));
#59554=CARTESIAN_POINT('',(-4.61880215351701,-8.,26.));
#59555=CARTESIAN_POINT('',(-9.23760430703401,1.1312802546399E-15,26.));
#59556=CARTESIAN_POINT('',(-4.61880215351701,-8.,26.));
#59557=CARTESIAN_POINT('Origin',(0.,0.,20.));
#59558=CARTESIAN_POINT('',(4.61880215351701,-8.,20.));
#59559=CARTESIAN_POINT('',(9.23760430703401,0.,20.));
#59560=CARTESIAN_POINT('',(4.61880215351701,-8.,20.));
#59561=CARTESIAN_POINT('',(-4.61880215351701,-8.,20.));
#59562=CARTESIAN_POINT('',(-4.61880215351701,-8.,20.));
#59563=CARTESIAN_POINT('',(-9.23760430703401,1.1312802546399E-15,20.));
#59564=CARTESIAN_POINT('',(-9.23760430703401,1.1312802546399E-15,20.));
#59565=CARTESIAN_POINT('',(-4.618802153517,8.,20.));
#59566=CARTESIAN_POINT('',(-4.618802153517,8.,20.));
#59567=CARTESIAN_POINT('',(4.61880215351701,8.,20.));
#59568=CARTESIAN_POINT('',(4.61880215351701,8.,20.));
#59569=CARTESIAN_POINT('',(9.23760430703401,0.,20.));
#59570=CARTESIAN_POINT('',(-5.,6.12323399573677E-16,20.));
#59571=CARTESIAN_POINT('Origin',(0.,0.,20.));
#59572=CARTESIAN_POINT('Origin',(-4.61880215351701,-8.,20.));
#59573=CARTESIAN_POINT('',(4.61880215351701,-8.,20.));
#59574=CARTESIAN_POINT('',(-4.61880215351701,-8.,20.));
#59575=CARTESIAN_POINT('Origin',(-9.23760430703401,1.1312802546399E-15,
20.));
#59576=CARTESIAN_POINT('',(-9.23760430703401,1.1312802546399E-15,20.));
#59577=CARTESIAN_POINT('Origin',(-4.618802153517,8.,20.));
#59578=CARTESIAN_POINT('',(-4.618802153517,8.,20.));
#59579=CARTESIAN_POINT('Origin',(4.61880215351701,8.,20.));
#59580=CARTESIAN_POINT('',(4.61880215351701,8.,20.));
#59581=CARTESIAN_POINT('Origin',(9.23760430703401,0.,20.));
#59582=CARTESIAN_POINT('',(9.23760430703401,0.,20.));
#59583=CARTESIAN_POINT('Origin',(4.61880215351701,-8.,20.));
#59584=CARTESIAN_POINT('Origin',(0.,0.,16.));
#59585=CARTESIAN_POINT('',(-5.,6.12323399573677E-16,17.3166247903554));
#59586=CARTESIAN_POINT('',(-5.,-6.12323399573677E-16,16.));
#59587=CARTESIAN_POINT('Origin',(0.,0.,17.3166247903554));
#59588=CARTESIAN_POINT('Origin',(0.,0.,86.));
#59589=CARTESIAN_POINT('Origin',(5.55111512312578E-16,0.,14.));
#59590=CARTESIAN_POINT('',(1.87717472568372E-16,-4.49927934798557E-32,8.));
#59591=CARTESIAN_POINT('Origin',(5.55111512312578E-16,0.,14.));
#59592=CARTESIAN_POINT('',(0.,0.,0.));
#59593=CARTESIAN_POINT('Origin',(0.,0.,4.));
#59594=CARTESIAN_POINT('',(-4.51054691465169,-0.000515110389415763,0.38741669750802));
#59595=CARTESIAN_POINT('',(-4.51874859034235,-0.000597354552748235,0.112583302491978));
#59596=CARTESIAN_POINT('',(-4.51775,5.53264807684796E-16,4.));
#59597=CARTESIAN_POINT('',(-3.43378788736191,2.93584158412995,0.));
#59598=CARTESIAN_POINT('Ctrl Pts',(-4.51874859034235,-0.000597354552748235,
0.112583302491978));
#59599=CARTESIAN_POINT('Ctrl Pts',(-4.51722457181931,0.322607764342177,
0.101221950551661));
#59600=CARTESIAN_POINT('Ctrl Pts',(-4.48139903614817,0.645891255334514,
0.0898605986113441));
#59601=CARTESIAN_POINT('Ctrl Pts',(-4.41220310426637,0.961201691623003,
0.0784992466710271));
#59602=CARTESIAN_POINT('Ctrl Pts',(-4.25283743035848,1.68739554150353,0.0523328311140182));
#59603=CARTESIAN_POINT('Ctrl Pts',(-3.91646501574702,2.37129788193745,0.0261664155570086));
#59604=CARTESIAN_POINT('Ctrl Pts',(-3.43378788736191,2.93584158412995,-2.08166817117217E-16));
#59605=CARTESIAN_POINT('',(3.44055068766013,2.93810645203836,-8.32667268468867E-16));
#59606=CARTESIAN_POINT('Origin',(0.,0.,0.));
#59607=CARTESIAN_POINT('Ctrl Pts',(3.44055068766013,2.93810645203836,-8.32667268468867E-16));
#59608=CARTESIAN_POINT('Ctrl Pts',(2.51857754810217,4.00873567447971,0.0500251109657056));
#59609=CARTESIAN_POINT('Ctrl Pts',(1.04980798302248,4.62287274287841,0.10005022193141));
#59610=CARTESIAN_POINT('Ctrl Pts',(-0.359976603224271,4.51112404046721,
0.150075332897117));
#59611=CARTESIAN_POINT('Ctrl Pts',(-1.83479629347494,4.39422023240758,0.202408164011137));
#59612=CARTESIAN_POINT('Ctrl Pts',(-3.24506337966313,3.48291388857057,0.254740995125157));
#59613=CARTESIAN_POINT('Ctrl Pts',(-3.96016577839605,2.18804786800098,0.307073826239177));
#59614=CARTESIAN_POINT('Ctrl Pts',(-4.32611438556047,1.52540931786942,0.333854783328791));
#59615=CARTESIAN_POINT('Ctrl Pts',(-4.5100126795522,0.762323836917479,0.360635740418406));
#59616=CARTESIAN_POINT('Ctrl Pts',(-4.51054691465169,-0.000515110389415763,
0.38741669750802));
#59617=CARTESIAN_POINT('Origin',(0.,0.,4.));
#59618=CARTESIAN_POINT('',(-4.52244050167421,-0.00276900106626683,1.38741669750802));
#59619=CARTESIAN_POINT('',(-4.5233994151039,0.0021134167823725,1.11258330249198));
#59620=CARTESIAN_POINT('',(-4.51775,5.53264807684796E-16,4.));
#59621=CARTESIAN_POINT('Ctrl Pts',(-4.5233994151039,0.0021134167823725,
1.11258330249198));
#59622=CARTESIAN_POINT('Ctrl Pts',(-4.52416026905118,0.130280331830068,
1.10805201945945));
#59623=CARTESIAN_POINT('Ctrl Pts',(-4.51917716893618,0.258387747461467,
1.10352073642693));
#59624=CARTESIAN_POINT('Ctrl Pts',(-4.50825644670978,0.385987082702882,
1.0989894533944));
#59625=CARTESIAN_POINT('Ctrl Pts',(-4.38213051111597,1.85966118637707,1.04665662228038));
#59626=CARTESIAN_POINT('Ctrl Pts',(-3.46401651516602,3.2655651297045,0.994323791166365));
#59627=CARTESIAN_POINT('Ctrl Pts',(-2.16517718342927,3.97324079579977,0.941990960052346));
#59628=CARTESIAN_POINT('Ctrl Pts',(-0.866337851692522,4.68091646189503,
0.889658128938326));
#59629=CARTESIAN_POINT('Ctrl Pts',(0.813226815831038,4.69036385075812,0.837325297824306));
#59630=CARTESIAN_POINT('Ctrl Pts',(2.11977950774785,3.99758999513324,0.784992466710287));
#59631=CARTESIAN_POINT('Ctrl Pts',(3.42633219966466,3.30481613950837,0.732659635596268));
#59632=CARTESIAN_POINT('Ctrl Pts',(4.35987291597477,1.90982103939552,0.680326804482248));
#59633=CARTESIAN_POINT('Ctrl Pts',(4.50321991349222,0.437577595733461,0.627993973368229));
#59634=CARTESIAN_POINT('Ctrl Pts',(4.64656691100967,-1.0346658479286,0.57566114225421));
#59635=CARTESIAN_POINT('Ctrl Pts',(3.99972018973448,-2.58415763513987,0.523328311140192));
#59636=CARTESIAN_POINT('Ctrl Pts',(2.85003205531654,-3.51527160715898,0.470995480026173));
#59637=CARTESIAN_POINT('Ctrl Pts',(1.7003439208986,-4.4463855791781,0.418662648912154));
#59638=CARTESIAN_POINT('Ctrl Pts',(0.0478143733379097,-4.75912173600502,
0.366329817798135));
#59639=CARTESIAN_POINT('Ctrl Pts',(-1.36123648115533,-4.3152078830999,0.313996986684115));
#59640=CARTESIAN_POINT('Ctrl Pts',(-2.77028733564855,-3.87129403019478,
0.261664155570096));
#59641=CARTESIAN_POINT('Ctrl Pts',(-3.93585949707434,-2.67073016755762,
0.209331324456076));
#59642=CARTESIAN_POINT('Ctrl Pts',(-4.34790497327718,-1.24589506757571,
0.156998493342058));
#59643=CARTESIAN_POINT('Ctrl Pts',(-4.46447347068682,-0.842806340108052,
0.142193429725364));
#59644=CARTESIAN_POINT('Ctrl Pts',(-4.52073455040284,-0.421768388741025,
0.127388366108671));
#59645=CARTESIAN_POINT('Ctrl Pts',(-4.51874859034235,-0.000597354552748235,
0.112583302491978));
#59646=CARTESIAN_POINT('Ctrl Pts',(-4.51054691465169,-0.000515110389415763,
0.38741669750802));
#59647=CARTESIAN_POINT('Ctrl Pts',(-4.51105663160901,-0.728344389129203,
0.412968571532425));
#59648=CARTESIAN_POINT('Ctrl Pts',(-4.3446466691941,-1.4559492437521,0.438520445556829));
#59649=CARTESIAN_POINT('Ctrl Pts',(-4.01017598625922,-2.09587333886935,
0.464072319581234));
#59650=CARTESIAN_POINT('Ctrl Pts',(-3.32514608411178,-3.40650282786799,
0.516405150695253));
#59651=CARTESIAN_POINT('Ctrl Pts',(-1.9351485685392,-4.34933610856308,0.568737981809272));
#59652=CARTESIAN_POINT('Ctrl Pts',(-0.463832664911,-4.50105515886306,0.621070812923292));
#59653=CARTESIAN_POINT('Ctrl Pts',(1.00748323871719,-4.65277420916302,0.673403644037311));
#59654=CARTESIAN_POINT('Ctrl Pts',(2.560117530401,-4.01337902906788,0.725736475151331));
#59655=CARTESIAN_POINT('Ctrl Pts',(3.49818631344856,-2.86985357730659,0.77806930626535));
#59656=CARTESIAN_POINT('Ctrl Pts',(4.43625509649613,-1.7263281255453,0.830402137379369));
#59657=CARTESIAN_POINT('Ctrl Pts',(4.75975837090746,-0.0786724021178761,
0.882734968493387));
#59658=CARTESIAN_POINT('Ctrl Pts',(4.32353285348464,1.33455667095541,0.935067799607406));
#59659=CARTESIAN_POINT('Ctrl Pts',(3.88730733606183,2.7477857440287,0.987400630721425));
#59660=CARTESIAN_POINT('Ctrl Pts',(2.69135302680487,3.92658816674785,1.03973346183545));
#59661=CARTESIAN_POINT('Ctrl Pts',(1.27193499135498,4.34236723513978,1.09206629294946));
#59662=CARTESIAN_POINT('Ctrl Pts',(-0.147483044094926,4.7581463035317,1.14439912406348));
#59663=CARTESIAN_POINT('Ctrl Pts',(-1.79036480573777,4.41090201759639,1.1967319551775));
#59664=CARTESIAN_POINT('Ctrl Pts',(-2.92016350112278,3.45636436650575,1.24906478629152));
#59665=CARTESIAN_POINT('Ctrl Pts',(-3.91577693325848,2.61519636835964,1.29518209003036));
#59666=CARTESIAN_POINT('Ctrl Pts',(-4.51294659780824,1.30242392182032,1.34129939376919));
#59667=CARTESIAN_POINT('Ctrl Pts',(-4.52244050167421,-0.00276900106626683,
1.38741669750802));
#59668=CARTESIAN_POINT('Origin',(0.,0.,4.));
#59669=CARTESIAN_POINT('',(-4.51698911071085,0.00388851918503852,2.38741669750802));
#59670=CARTESIAN_POINT('',(-4.51093362149631,0.00101330851266679,2.11258330249198));
#59671=CARTESIAN_POINT('',(-4.51775,5.53264807684796E-16,4.));
#59672=CARTESIAN_POINT('Ctrl Pts',(-4.51093362149631,0.00101330851266679,
2.11258330249198));
#59673=CARTESIAN_POINT('Ctrl Pts',(-4.51232811703185,0.680923530020972,
2.08871567281024));
#59674=CARTESIAN_POINT('Ctrl Pts',(-4.36790019846314,1.36027124256301,2.06484804312849));
#59675=CARTESIAN_POINT('Ctrl Pts',(-4.07455659430891,1.96770381197164,2.04098041344675));
#59676=CARTESIAN_POINT('Ctrl Pts',(-3.43136321904367,3.29957742036487,1.98864758233273));
#59677=CARTESIAN_POINT('Ctrl Pts',(-2.07224023608874,4.28571055146719,1.93631475121871));
#59678=CARTESIAN_POINT('Ctrl Pts',(-0.606537899693793,4.48397159897241,
1.88398192010469));
#59679=CARTESIAN_POINT('Ctrl Pts',(0.859164436701136,4.68223264647763,1.83164908899067));
#59680=CARTESIAN_POINT('Ctrl Pts',(2.43144612653608,4.09262161038578,1.77931625787665));
#59681=CARTESIAN_POINT('Ctrl Pts',(3.40536636602181,2.97949323501332,1.72698342676264));
#59682=CARTESIAN_POINT('Ctrl Pts',(4.37928660550757,1.86636485964083,1.67465059564862));
#59683=CARTESIAN_POINT('Ctrl Pts',(4.75484539464409,0.229719144987712,1.6223177645346));
#59684=CARTESIAN_POINT('Ctrl Pts',(4.36368967023442,-1.19666928711504,1.56998493342058));
#59685=CARTESIAN_POINT('Ctrl Pts',(3.97253394582476,-2.62305771921779,1.51765210230656));
#59686=CARTESIAN_POINT('Ctrl Pts',(2.81466370786892,-3.83918886877017,1.46531927119254));
#59687=CARTESIAN_POINT('Ctrl Pts',(1.40915332177568,-4.29979703199479,1.41298644007852));
#59688=CARTESIAN_POINT('Ctrl Pts',(0.00364293568242802,-4.76040519521942,
1.3606536089645));
#59689=CARTESIAN_POINT('Ctrl Pts',(-1.64950759854823,-4.46549037211628,
1.30832077785048));
#59690=CARTESIAN_POINT('Ctrl Pts',(-2.80901392804473,-3.54731082855424,
1.25598794673646));
#59691=CARTESIAN_POINT('Ctrl Pts',(-3.86812340827646,-2.70863264767388,
1.20818639865497));
#59692=CARTESIAN_POINT('Ctrl Pts',(-4.51537299162016,-1.34994888171753,
1.16038485057347));
#59693=CARTESIAN_POINT('Ctrl Pts',(-4.5233994151039,0.0021134167823725,
1.11258330249198));
#59694=CARTESIAN_POINT('Ctrl Pts',(-4.52244050167421,-0.00276900106626683,
1.38741669750802));
#59695=CARTESIAN_POINT('Ctrl Pts',(-4.52372005651789,-0.178678295071038,
1.39363222488321));
#59696=CARTESIAN_POINT('Ctrl Pts',(-4.51432465941186,-0.35444990932754,
1.39984775225839));
#59697=CARTESIAN_POINT('Ctrl Pts',(-4.49379103756964,-0.528910718243546,
1.40606327963358));
#59698=CARTESIAN_POINT('Ctrl Pts',(-4.32090424950433,-1.99781713565632,
1.4583961107476));
#59699=CARTESIAN_POINT('Ctrl Pts',(-3.3584150442465,-3.37379895423595,1.51072894186162));
#59700=CARTESIAN_POINT('Ctrl Pts',(-2.037860803389,-4.0399278796399,1.56306177297564));
#59701=CARTESIAN_POINT('Ctrl Pts',(-0.717306562531505,-4.70605680504386,
1.61539460408966));
#59702=CARTESIAN_POINT('Ctrl Pts',(0.961312713925656,-4.66233283727215,
1.66772743520368));
#59703=CARTESIAN_POINT('Ctrl Pts',(2.24539906972787,-3.92836571897045,1.72006026631769));
#59704=CARTESIAN_POINT('Ctrl Pts',(3.52948542553009,-3.19439860066874,1.77239309743171));
#59705=CARTESIAN_POINT('Ctrl Pts',(4.41903886067735,-1.77018833183704,1.82472592854573));
#59706=CARTESIAN_POINT('Ctrl Pts',(4.51522900816629,-0.294270957708535,
1.87705875965975));
#59707=CARTESIAN_POINT('Ctrl Pts',(4.61141915565522,1.18164641641996,1.92939159077377));
#59708=CARTESIAN_POINT('Ctrl Pts',(3.91424601548584,2.70927089584527,1.98172442188779));
#59709=CARTESIAN_POINT('Ctrl Pts',(2.73628580760446,3.60369609834798,2.03405725300181));
#59710=CARTESIAN_POINT('Ctrl Pts',(1.55832559972309,4.4981213008507,2.08639008411583));
#59711=CARTESIAN_POINT('Ctrl Pts',(-0.100421675870265,4.75934722643081,
2.13872291522985));
#59712=CARTESIAN_POINT('Ctrl Pts',(-1.49626358664302,4.2702551012346,2.19105574634387));
#59713=CARTESIAN_POINT('Ctrl Pts',(-2.89210549741577,3.78116297603839,2.24338857745789));
#59714=CARTESIAN_POINT('Ctrl Pts',(-4.02504204336792,2.54175280006585,2.29572140857191));
#59715=CARTESIAN_POINT('Ctrl Pts',(-4.38712504707582,1.10770899592287,2.34805423968593));
#59716=CARTESIAN_POINT('Ctrl Pts',(-4.47790602629514,0.748167400624681,
2.36117505895996));
#59717=CARTESIAN_POINT('Ctrl Pts',(-4.52023125554896,0.376391161643011,
2.37429587823399));
#59718=CARTESIAN_POINT('Ctrl Pts',(-4.51698911071085,0.00388851918503852,
2.38741669750802));
#59719=CARTESIAN_POINT('Origin',(0.,0.,4.));
#59720=CARTESIAN_POINT('',(-4.51234492774861,-0.00257476452032779,3.38741669750802));
#59721=CARTESIAN_POINT('',(-4.52027081060448,-0.00355576929457683,3.11258330249198));
#59722=CARTESIAN_POINT('',(-4.51775,5.53264807684796E-16,4.));
#59723=CARTESIAN_POINT('Ctrl Pts',(-4.52027081060448,-0.00355576929457683,
3.11258330249198));
#59724=CARTESIAN_POINT('Ctrl Pts',(-4.50971003274407,1.22072076070225,3.06937932616102));
#59725=CARTESIAN_POINT('Ctrl Pts',(-3.99354051828841,2.45284880293372,3.02617534983006));
#59726=CARTESIAN_POINT('Ctrl Pts',(-3.10547711214626,3.29088013555457,2.9829713734991));
#59727=CARTESIAN_POINT('Ctrl Pts',(-2.02976889732455,4.30598466811756,2.93063854238508));
#59728=CARTESIAN_POINT('Ctrl Pts',(-0.408403261408893,4.74285492731681,
2.87830571127106));
#59729=CARTESIAN_POINT('Ctrl Pts',(1.03168676818161,4.40562172719721,2.82597288015704));
#59730=CARTESIAN_POINT('Ctrl Pts',(2.4717767977721,4.06838852707761,2.77364004904302));
#59731=CARTESIAN_POINT('Ctrl Pts',(3.73059122103745,2.95705186763916,2.721307217929));
#59732=CARTESIAN_POINT('Ctrl Pts',(4.2437450475446,1.56987545160024,2.66897438681498));
#59733=CARTESIAN_POINT('Ctrl Pts',(4.75689887405174,0.182699035561331,2.61664155570096));
#59734=CARTESIAN_POINT('Ctrl Pts',(4.5243921038007,-1.48031713707804,2.56430872458694));
#59735=CARTESIAN_POINT('Ctrl Pts',(3.65046881853353,-2.67356621578173,2.51197589347292));
#59736=CARTESIAN_POINT('Ctrl Pts',(2.77654553326636,-3.86681529448543,2.4596430623589));
#59737=CARTESIAN_POINT('Ctrl Pts',(1.26120573298304,-4.59029727925343,2.40731023124489));
#59738=CARTESIAN_POINT('Ctrl Pts',(-0.216154740062777,-4.51964138893216,
2.35497740013087));
#59739=CARTESIAN_POINT('Ctrl Pts',(-1.69351521310859,-4.44898549861089,
2.30264456901685));
#59740=CARTESIAN_POINT('Ctrl Pts',(-3.1328963589169,-3.58419173320037,2.25031173790283));
#59741=CARTESIAN_POINT('Ctrl Pts',(-3.88895504803329,-2.31298780765304,
2.19797890678881));
#59742=CARTESIAN_POINT('Ctrl Pts',(-4.30019522790109,-1.62154660273587,
2.16951370535653));
#59743=CARTESIAN_POINT('Ctrl Pts',(-4.50927050719276,-0.809866601606811,
2.14104850392425));
#59744=CARTESIAN_POINT('Ctrl Pts',(-4.51093362149631,0.00101330851266679,
2.11258330249198));
#59745=CARTESIAN_POINT('Ctrl Pts',(-4.51698911071085,0.00388851918503852,
2.38741669750802));
#59746=CARTESIAN_POINT('Ctrl Pts',(-4.50729985128856,-1.10934821713655,
2.42662870934801));
#59747=CARTESIAN_POINT('Ctrl Pts',(-4.09063314279102,-2.22907270570801,
2.465840721188));
#59748=CARTESIAN_POINT('Ctrl Pts',(-3.34408434212355,-3.04811166820345,
2.50505273302798));
#59749=CARTESIAN_POINT('Ctrl Pts',(-2.34773117199973,-4.14121109587334,
2.557385564142));
#59750=CARTESIAN_POINT('Ctrl Pts',(-0.763795370288439,-4.69873251889968,
2.60971839525602));
#59751=CARTESIAN_POINT('Ctrl Pts',(0.697571505631126,-4.4707134324377,2.66205122637004));
#59752=CARTESIAN_POINT('Ctrl Pts',(2.15893838155069,-4.24269434597572,2.71438405748406));
#59753=CARTESIAN_POINT('Ctrl Pts',(3.49773633167853,-3.2291347500254,2.76671688859808));
#59754=CARTESIAN_POINT('Ctrl Pts',(4.11372028899329,-1.88446020659954,2.8190497197121));
#59755=CARTESIAN_POINT('Ctrl Pts',(4.72970424630805,-0.539785663173669,
2.87138255082612));
#59756=CARTESIAN_POINT('Ctrl Pts',(4.62287421080972,1.13600382772776,2.92371538194014));
#59757=CARTESIAN_POINT('Ctrl Pts',(3.84112705187867,2.39157432571858,2.97604821305416));
#59758=CARTESIAN_POINT('Ctrl Pts',(3.05937989294762,3.6471448237094,3.02838104416818));
#59759=CARTESIAN_POINT('Ctrl Pts',(1.60271561058387,4.48249632878962,3.08071387528219));
#59760=CARTESIAN_POINT('Ctrl Pts',(0.124224136080841,4.52310215772866,3.13304670639621));
#59761=CARTESIAN_POINT('Ctrl Pts',(-1.35426733842219,4.56370798666771,3.18537953751023));
#59762=CARTESIAN_POINT('Ctrl Pts',(-2.85458600506451,3.80956813946558,3.23771236862425));
#59763=CARTESIAN_POINT('Ctrl Pts',(-3.70406963378462,2.5987983669013,3.29004519973827));
#59764=CARTESIAN_POINT('Ctrl Pts',(-4.2309249653141,1.84787099365534,3.32250236566152));
#59765=CARTESIAN_POINT('Ctrl Pts',(-4.50743256748542,0.921298090727453,
3.35495953158477));
#59766=CARTESIAN_POINT('Ctrl Pts',(-4.51234492774861,-0.00257476452032779,
3.38741669750802));
#59767=CARTESIAN_POINT('Origin',(0.,0.,4.));
#59768=CARTESIAN_POINT('',(-4.52478583629221,-0.000271302356462328,4.38741669750802));
#59769=CARTESIAN_POINT('',(-4.51939464917808,0.00373292266216646,4.11258330249198));
#59770=CARTESIAN_POINT('',(-4.51775,5.53264807684796E-16,4.));
#59771=CARTESIAN_POINT('Ctrl Pts',(-4.51939464917808,0.00373292266216647,
4.11258330249198));
#59772=CARTESIAN_POINT('Ctrl Pts',(-4.52195179175284,0.293129143485266,
4.10237581062582));
#59773=CARTESIAN_POINT('Ctrl Pts',(-4.49647546580418,0.582077227182858,
4.09216831875966));
#59774=CARTESIAN_POINT('Ctrl Pts',(-4.44131034778915,0.865241438283023,
4.0819608268935));
#59775=CARTESIAN_POINT('Ctrl Pts',(-4.15848408230504,2.31699717136045,4.02962799577948));
#59776=CARTESIAN_POINT('Ctrl Pts',(-3.09528361658689,3.61672297535275,3.97729516466546));
#59777=CARTESIAN_POINT('Ctrl Pts',(-1.72839087618034,4.18169168234348,3.92496233355144));
#59778=CARTESIAN_POINT('Ctrl Pts',(-0.361498135773788,4.7466603893342,3.87262950243742));
#59779=CARTESIAN_POINT('Ctrl Pts',(1.30908687932117,4.57687199932334,3.8202966713234));
#59780=CARTESIAN_POINT('Ctrl Pts',(2.5343636726828,3.74845049626232,3.76796384020938));
#59781=CARTESIAN_POINT('Ctrl Pts',(3.75964046604444,2.9200289932013,3.71563100909536));
#59782=CARTESIAN_POINT('Ctrl Pts',(4.53960903767275,1.43297437709012,3.66329817798134));
#59783=CARTESIAN_POINT('Ctrl Pts',(4.52457341059044,-0.0459980138823182,
3.61096534686733));
#59784=CARTESIAN_POINT('Ctrl Pts',(4.50953778350813,-1.52497040485477,3.55863251575331));
#59785=CARTESIAN_POINT('Ctrl Pts',(3.69949795771518,-2.99586057068848,3.50629968463929));
#59786=CARTESIAN_POINT('Ctrl Pts',(2.45763224901275,-3.79920044943065,3.45396685352527));
#59787=CARTESIAN_POINT('Ctrl Pts',(1.21576654031032,-4.60254032817281,3.40163402241125));
#59788=CARTESIAN_POINT('Ctrl Pts',(-0.457925051301578,-4.73832991982345,
3.34930119129723));
#59789=CARTESIAN_POINT('Ctrl Pts',(-1.81304922569253,-4.1456884652134,3.29696836018321));
#59790=CARTESIAN_POINT('Ctrl Pts',(-3.16817340008348,-3.55304701060334,
3.24463552906919));
#59791=CARTESIAN_POINT('Ctrl Pts',(-4.20473015725347,-2.23197450973259,
3.19230269795517));
#59792=CARTESIAN_POINT('Ctrl Pts',(-4.45798313897459,-0.774768856333857,
3.13996986684115));
#59793=CARTESIAN_POINT('Ctrl Pts',(-4.50216018126897,-0.520576248830078,
3.1308410120581));
#59794=CARTESIAN_POINT('Ctrl Pts',(-4.52250226742098,-0.262241279420579,
3.12171215727504));
#59795=CARTESIAN_POINT('Ctrl Pts',(-4.52027081060448,-0.00355576929457683,
3.11258330249198));
#59796=CARTESIAN_POINT('Ctrl Pts',(-4.51234492774861,-0.00257476452032779,
3.38741669750802));
#59797=CARTESIAN_POINT('Ctrl Pts',(-4.51535309020244,-0.568323098591327,
3.40729236269879));
#59798=CARTESIAN_POINT('Ctrl Pts',(-4.41651517435603,-1.13305893603127,
3.42716802788956));
#59799=CARTESIAN_POINT('Ctrl Pts',(-4.21095206217547,-1.65582834772821,
3.44704369308033));
#59800=CARTESIAN_POINT('Ctrl Pts',(-3.66970227104832,-3.032285591867,3.49937652419435));
#59801=CARTESIAN_POINT('Ctrl Pts',(-2.3885540979961,-4.11780038221814,3.55170935530837));
#59802=CARTESIAN_POINT('Ctrl Pts',(-0.941905499312602,-4.42568625369714,
3.60404218642239));
#59803=CARTESIAN_POINT('Ctrl Pts',(0.504743099370899,-4.73357212517614,
3.65637501753641));
#59804=CARTESIAN_POINT('Ctrl Pts',(2.11689212368568,-4.263829077783,3.70870784865043));
#59805=CARTESIAN_POINT('Ctrl Pts',(3.17174063018436,-3.22706463608245,3.76104067976445));
#59806=CARTESIAN_POINT('Ctrl Pts',(4.22658913668306,-2.19030019438189,3.81337351087847));
#59807=CARTESIAN_POINT('Ctrl Pts',(4.72413712536563,-0.586514358373886,
3.86570634199248));
#59808=CARTESIAN_POINT('Ctrl Pts',(4.44131082922502,0.865241532073468,3.9180391731065));
#59809=CARTESIAN_POINT('Ctrl Pts',(4.15848453308441,2.31699742252081,3.97037200422052));
#59810=CARTESIAN_POINT('Ctrl Pts',(3.09528395212065,3.61672336740751,4.02270483533454));
#59811=CARTESIAN_POINT('Ctrl Pts',(1.7283910635404,4.18169213563993,4.07503766644856));
#59812=CARTESIAN_POINT('Ctrl Pts',(0.361498174960155,4.74666090387236,4.12737049756258));
#59813=CARTESIAN_POINT('Ctrl Pts',(-1.30908702123658,4.5768724954505,4.1797033286766));
#59814=CARTESIAN_POINT('Ctrl Pts',(-2.5343639474132,3.74845090259061,4.23203615979062));
#59815=CARTESIAN_POINT('Ctrl Pts',(-3.74701372251171,2.9285666488301,4.28382967236309));
#59816=CARTESIAN_POINT('Ctrl Pts',(-4.52348622608021,1.46355441369542,4.33562318493555));
#59817=CARTESIAN_POINT('Ctrl Pts',(-4.52478583629221,-0.000271302356462328,
4.38741669750802));
#59818=CARTESIAN_POINT('Origin',(0.,0.,4.));
#59819=CARTESIAN_POINT('',(-4.51292607061429,0.0029183530353194,5.38741669750802));
#59820=CARTESIAN_POINT('',(-4.51119223387812,-0.00146992377155156,5.11258330249198));
#59821=CARTESIAN_POINT('',(-4.51775,5.53264807684796E-16,4.));
#59822=CARTESIAN_POINT('Ctrl Pts',(-4.51119223387812,-0.00146992377155156,
5.11258330249198));
#59823=CARTESIAN_POINT('Ctrl Pts',(-4.50867979289825,0.840016500418339,
5.0830394639766));
#59824=CARTESIAN_POINT('Ctrl Pts',(-4.28245206788243,1.68275768437228,5.05349562546122));
#59825=CARTESIAN_POINT('Ctrl Pts',(-3.84112663548136,2.39157406650585,5.02395178694585));
#59826=CARTESIAN_POINT('Ctrl Pts',(-3.05937956127687,3.64714442841863,4.97161895583183));
#59827=CARTESIAN_POINT('Ctrl Pts',(-1.60271543685273,4.48249584288365,4.9192861247178));
#59828=CARTESIAN_POINT('Ctrl Pts',(-0.124224122626221,4.52310166740692,
4.86695329360379));
#59829=CARTESIAN_POINT('Ctrl Pts',(1.3542671916003,4.56370749193019,4.81462046248977));
#59830=CARTESIAN_POINT('Ctrl Pts',(2.85458569562921,3.80956772651169,4.76228763137575));
#59831=CARTESIAN_POINT('Ctrl Pts',(3.70406923227031,2.59879808520239,4.70995480026173));
#59832=CARTESIAN_POINT('Ctrl Pts',(4.5535527689114,1.3880284438931,4.65762196914771));
#59833=CARTESIAN_POINT('Ctrl Pts',(4.7522013381647,-0.279371073306991,4.60528913803369));
#59834=CARTESIAN_POINT('Ctrl Pts',(4.21095160570608,-1.65582816824236,4.55295630691967));
#59835=CARTESIAN_POINT('Ctrl Pts',(3.66970187324747,-3.03228526317774,4.50062347580565));
#59836=CARTESIAN_POINT('Ctrl Pts',(2.38855383907694,-4.11779993584839,4.44829064469163));
#59837=CARTESIAN_POINT('Ctrl Pts',(0.94190539721171,-4.42568577395046,4.39595781357761));
#59838=CARTESIAN_POINT('Ctrl Pts',(-0.50474304465354,-4.73357161205254,
4.34362498246359));
#59839=CARTESIAN_POINT('Ctrl Pts',(-2.11689189421349,-4.263828615586,4.29129215134958));
#59840=CARTESIAN_POINT('Ctrl Pts',(-3.17174028636843,-3.22706428627144,
4.23895932023556));
#59841=CARTESIAN_POINT('Ctrl Pts',(-4.02084104068784,-2.3925203076111,4.1968339809877));
#59842=CARTESIAN_POINT('Ctrl Pts',(-4.50884156719875,-1.19057750531243,
4.15470864173984));
#59843=CARTESIAN_POINT('Ctrl Pts',(-4.51939464917808,0.00373292266216647,
4.11258330249198));
#59844=CARTESIAN_POINT('Ctrl Pts',(-4.52478583629221,-0.000271302356462328,
4.38741669750802));
#59845=CARTESIAN_POINT('Ctrl Pts',(-4.52479936895005,-0.0155139130822968,
4.38795601604957));
#59846=CARTESIAN_POINT('Ctrl Pts',(-4.52472885144687,-0.030756395156677,
4.38849533459112));
#59847=CARTESIAN_POINT('Ctrl Pts',(-4.52457390104248,-0.0459980188636215,
4.38903465313267));
#59848=CARTESIAN_POINT('Ctrl Pts',(-4.50953827233865,-1.52497057016008,
4.44136748424669));
#59849=CARTESIAN_POINT('Ctrl Pts',(-3.69949835877446,-2.99586089545507,
4.49370031536071));
#59850=CARTESIAN_POINT('Ctrl Pts',(-2.45763251543912,-3.79920086127216,
4.54603314647473));
#59851=CARTESIAN_POINT('Ctrl Pts',(-1.21576667210378,-4.60254082708924,
4.59836597758875));
#59852=CARTESIAN_POINT('Ctrl Pts',(0.45792510100271,-4.73833043342844,4.65069880870277));
#59853=CARTESIAN_POINT('Ctrl Pts',(1.81304942226226,-4.14568891458885,4.70303163981679));
#59854=CARTESIAN_POINT('Ctrl Pts',(3.16817374352182,-3.55304739574926,4.75536447093081));
#59855=CARTESIAN_POINT('Ctrl Pts',(4.20473061293445,-2.23197475173087,4.80769730204483));
#59856=CARTESIAN_POINT('Ctrl Pts',(4.45798362215519,-0.774768940348221,
4.86003013315885));
#59857=CARTESIAN_POINT('Ctrl Pts',(4.71123663137592,0.682436871034428,4.91236296427287));
#59858=CARTESIAN_POINT('Ctrl Pts',(4.18118578040478,2.27577584978132,4.96469579538688));
#59859=CARTESIAN_POINT('Ctrl Pts',(3.10547744889356,3.29088049233953,5.0170286265009));
#59860=CARTESIAN_POINT('Ctrl Pts',(2.02976911738235,4.30598513489774,5.06936145761492));
#59861=CARTESIAN_POINT('Ctrl Pts',(0.408403305331062,4.74285544126724,5.12169428872895));
#59862=CARTESIAN_POINT('Ctrl Pts',(-1.03168688021991,4.40562220466712,5.17402711984297));
#59863=CARTESIAN_POINT('Ctrl Pts',(-2.47177706577088,4.068388968067,5.22635995095699));
#59864=CARTESIAN_POINT('Ctrl Pts',(-3.73059162482154,2.95705218849725,5.278692782071));
#59865=CARTESIAN_POINT('Ctrl Pts',(-4.2437455072054,1.56987562195304,5.33102561318502));
#59866=CARTESIAN_POINT('Ctrl Pts',(-4.42806131327582,1.07162631350615,5.34982264129268));
#59867=CARTESIAN_POINT('Ctrl Pts',(-4.51617798535533,0.537790377713164,
5.36861966940035));
#59868=CARTESIAN_POINT('Ctrl Pts',(-4.51292607061429,0.0029183530353194,
5.38741669750802));
#59869=CARTESIAN_POINT('Origin',(0.,0.,4.));
#59870=CARTESIAN_POINT('',(-4.51611343680291,-0.0038242599945422,6.38741669750802));
#59871=CARTESIAN_POINT('',(-4.52399690261043,-0.00167256832429505,6.11258330249198));
#59872=CARTESIAN_POINT('',(-4.51775,5.53264807684796E-16,4.));
#59873=CARTESIAN_POINT('Ctrl Pts',(-4.52399690261043,-0.00167256832429505,
6.11258330249198));
#59874=CARTESIAN_POINT('Ctrl Pts',(-4.5173342997898,1.3804594726294,6.06370311732738));
#59875=CARTESIAN_POINT('Ctrl Pts',(-3.83652995787924,2.76828008382611,6.01482293216279));
#59876=CARTESIAN_POINT('Ctrl Pts',(-2.73628551041168,3.60369570881218,5.96594274699819));
#59877=CARTESIAN_POINT('Ctrl Pts',(-1.55832542986843,4.49812081512447,5.91360991588417));
#59878=CARTESIAN_POINT('Ctrl Pts',(0.100421664862097,4.75934671033683,5.86127708477015));
#59879=CARTESIAN_POINT('Ctrl Pts',(1.49626342410919,4.27025463771519,5.80894425365613));
#59880=CARTESIAN_POINT('Ctrl Pts',(2.89210518335629,3.78116256509354,5.75661142254211));
#59881=CARTESIAN_POINT('Ctrl Pts',(4.02504160711995,2.54175252463788,5.7042785914281));
#59882=CARTESIAN_POINT('Ctrl Pts',(4.3871245717083,1.10770887619882,5.65194576031408));
#59883=CARTESIAN_POINT('Ctrl Pts',(4.74920753629665,-0.326334772240243,
5.59961292920006));
#59884=CARTESIAN_POINT('Ctrl Pts',(4.34043704170966,-1.95501202866272,5.54728009808604));
#59885=CARTESIAN_POINT('Ctrl Pts',(3.34408397951354,-3.04811133798521,5.49494726697202));
#59886=CARTESIAN_POINT('Ctrl Pts',(2.34773091731743,-4.14121064730769,5.442614435858));
#59887=CARTESIAN_POINT('Ctrl Pts',(0.763795287512193,-4.6987320095302,5.39028160474398));
#59888=CARTESIAN_POINT('Ctrl Pts',(-0.697571429950846,-4.47071294770401,
5.33794877362996));
#59889=CARTESIAN_POINT('Ctrl Pts',(-2.15893814741389,-4.24269388587781,
5.28561594251594));
#59890=CARTESIAN_POINT('Ctrl Pts',(-3.49773595253472,-3.22913440000291,
5.23328311140192));
#59891=CARTESIAN_POINT('Ctrl Pts',(-4.11371984310272,-1.88446000238519,
5.1809502802879));
#59892=CARTESIAN_POINT('Ctrl Pts',(-4.3819578119688,-1.29890454431857,5.15816128768926));
#59893=CARTESIAN_POINT('Ctrl Pts',(-4.51313023522704,-0.650560524599824,
5.13537229509062));
#59894=CARTESIAN_POINT('Ctrl Pts',(-4.51119223387812,-0.00146992377155156,
5.11258330249198));
#59895=CARTESIAN_POINT('Ctrl Pts',(-4.51292607061429,0.0029183530353194,
5.38741669750802));
#59896=CARTESIAN_POINT('Ctrl Pts',(-4.50712432517217,-0.95134754210846,
5.42095250051437));
#59897=CARTESIAN_POINT('Ctrl Pts',(-4.21049476107502,-1.90891132639337,
5.45448830352073));
#59898=CARTESIAN_POINT('Ctrl Pts',(-3.65046921487666,-2.67356650591896,
5.48802410652708));
#59899=CARTESIAN_POINT('Ctrl Pts',(-2.776545834447,-3.86681571372806,5.5403569376411));
#59900=CARTESIAN_POINT('Ctrl Pts',(-1.26120586787061,-4.5902977758276,5.59268976875511));
#59901=CARTESIAN_POINT('Ctrl Pts',(0.216154764597121,-4.51964187827841,
5.64502259986913));
#59902=CARTESIAN_POINT('Ctrl Pts',(1.69351539706486,-4.44898598072923,5.69735543098315));
#59903=CARTESIAN_POINT('Ctrl Pts',(3.13289669542393,-3.58419212353131,5.74968826209718));
#59904=CARTESIAN_POINT('Ctrl Pts',(3.88895546769304,-2.31298805942388,5.8020210932112));
#59905=CARTESIAN_POINT('Ctrl Pts',(4.64501423996215,-1.04178399531645,5.85435392432522));
#59906=CARTESIAN_POINT('Ctrl Pts',(4.71775048614129,0.635830275700497,5.90668675543923));
#59907=CARTESIAN_POINT('Ctrl Pts',(4.07455703922814,1.96770402713248,5.95901958655325));
#59908=CARTESIAN_POINT('Ctrl Pts',(3.43136359231499,3.29957777856446,6.01135241766727));
#59909=CARTESIAN_POINT('Ctrl Pts',(2.07224045230956,4.28571101041149,6.0636852487813));
#59910=CARTESIAN_POINT('Ctrl Pts',(0.606537960019231,4.4839720817303,6.11601807989532));
#59911=CARTESIAN_POINT('Ctrl Pts',(-0.859164532271093,4.68223315304911,
6.16835091100933));
#59912=CARTESIAN_POINT('Ctrl Pts',(-2.43144637684631,4.0926220638397,6.22068374212335));
#59913=CARTESIAN_POINT('Ctrl Pts',(-3.4053667262744,2.97949356381203,6.27301657323736));
#59914=CARTESIAN_POINT('Ctrl Pts',(-4.11503346658856,2.16838999191388,6.31114994799425));
#59915=CARTESIAN_POINT('Ctrl Pts',(-4.506994027605,1.07931947572563,6.34928332275114));
#59916=CARTESIAN_POINT('Ctrl Pts',(-4.51611343680291,-0.0038242599945422,
6.38741669750802));
#59917=CARTESIAN_POINT('Origin',(0.,0.,4.));
#59918=CARTESIAN_POINT('',(-4.52286359173795,0.00246468782935438,7.38741669750802));
#59919=CARTESIAN_POINT('',(-4.51483246697105,0.00361950456559231,7.11258330249198));
#59920=CARTESIAN_POINT('',(-4.51775,5.53264807684796E-16,4.));
#59921=CARTESIAN_POINT('',(3.43378788736184,2.93584158413003,8.));
#59922=CARTESIAN_POINT('Ctrl Pts',(-4.52286359173795,0.00246468782935438,
7.38741669750802));
#59923=CARTESIAN_POINT('Ctrl Pts',(-4.514736621556,-1.33289820095304,7.43461263832996));
#59924=CARTESIAN_POINT('Ctrl Pts',(-3.88687106704568,-2.67555385687553,
7.48180857915189));
#59925=CARTESIAN_POINT('Ctrl Pts',(-2.85003294005483,-3.51527175392636,
7.52900451997383));
#59926=CARTESIAN_POINT('Ctrl Pts',(-1.70034350389957,-4.44638604308903,
7.58133735108785));
#59927=CARTESIAN_POINT('Ctrl Pts',(-0.0478099810187527,-4.759123220785,
7.63367018220187));
#59928=CARTESIAN_POINT('Ctrl Pts',(1.3612375474742,-4.31520832020808,7.68600301331589));
#59929=CARTESIAN_POINT('Ctrl Pts',(2.77028507596716,-3.87129341963115,7.73833584442991));
#59930=CARTESIAN_POINT('Ctrl Pts',(3.93584661007225,-2.67072644078133,7.79066867554392));
#59931=CARTESIAN_POINT('Ctrl Pts',(4.34789968202776,-1.24589357093064,7.84300150665794));
#59932=CARTESIAN_POINT('Ctrl Pts',(4.55392621800552,-0.533477136005289,
7.86916792221495));
#59933=CARTESIAN_POINT('Ctrl Pts',(4.57157563844588,0.235005771670285,7.89533433777196));
#59934=CARTESIAN_POINT('Ctrl Pts',(4.41221033788124,0.961199526155991,7.92150075332897));
#59935=CARTESIAN_POINT('Ctrl Pts',(4.2528450373166,1.6873932806417,7.94766716888598));
#59936=CARTESIAN_POINT('Ctrl Pts',(3.91646501574697,2.37129788193754,7.97383358444299));
#59937=CARTESIAN_POINT('Ctrl Pts',(3.43378788736183,2.93584158413004,8.));
#59938=CARTESIAN_POINT('',(-3.44054916109511,2.9381068161154,8.));
#59939=CARTESIAN_POINT('Origin',(0.,0.,8.));
#59940=CARTESIAN_POINT('Ctrl Pts',(-3.44054916109511,2.9381068161154,8.));
#59941=CARTESIAN_POINT('Ctrl Pts',(-2.51857342159112,4.00873681403696,7.94997488903429));
#59942=CARTESIAN_POINT('Ctrl Pts',(-1.04980743191293,4.62287257548397,7.89994977806859));
#59943=CARTESIAN_POINT('Ctrl Pts',(0.359975956906261,4.51112341871505,7.84992466710289));
#59944=CARTESIAN_POINT('Ctrl Pts',(1.83479439449057,4.39421913533762,7.79759183598887));
#59945=CARTESIAN_POINT('Ctrl Pts',(3.24506283044465,3.48291324925361,7.74525900487485));
#59946=CARTESIAN_POINT('Ctrl Pts',(3.96016560277148,2.18804756351099,7.69292617376083));
#59947=CARTESIAN_POINT('Ctrl Pts',(4.67526837509831,0.893181877768381,7.64059334264681));
#59948=CARTESIAN_POINT('Ctrl Pts',(4.69520548379788,-0.785243607632836,
7.58826051153279));
#59949=CARTESIAN_POINT('Ctrl Pts',(4.01017546547555,-2.09587300826054,7.53592768041877));
#59950=CARTESIAN_POINT('Ctrl Pts',(3.32514544715321,-3.40650240888826,7.48359484930475));
#59951=CARTESIAN_POINT('Ctrl Pts',(1.93514830180898,-4.34933572474246,7.43126201819073));
#59952=CARTESIAN_POINT('Ctrl Pts',(0.463832634566904,-4.50105475907159,
7.37892918707671));
#59953=CARTESIAN_POINT('Ctrl Pts',(-1.00748303267517,-4.65277379340072,
7.32659635596269));
#59954=CARTESIAN_POINT('Ctrl Pts',(-2.56011722181508,-4.01337854620477,
7.27426352484867));
#59955=CARTESIAN_POINT('Ctrl Pts',(-3.49818593160913,-2.86985320272758,
7.22193069373465));
#59956=CARTESIAN_POINT('Ctrl Pts',(-4.15153848320893,-2.0734028007694,7.18548156332043));
#59957=CARTESIAN_POINT('Ctrl Pts',(-4.50676902168756,-1.0324019249735,7.14903243290621));
#59958=CARTESIAN_POINT('Ctrl Pts',(-4.51483246697105,0.00361950456559231,
7.11258330249198));
#59959=CARTESIAN_POINT('Origin',(0.,0.,10.2083368446371));
#59960=CARTESIAN_POINT('',(-5.0799445016814,0.00237344505285342,0.791663155362921));
#59961=CARTESIAN_POINT('',(-5.06551066928822,-0.000578487979983568,0.708336844637072));
#59962=CARTESIAN_POINT('',(-5.0736,1.10600941455115E-13,10.2083368446371));
#59963=CARTESIAN_POINT('',(1.31303618635654,-4.9007502418832,0.));
#59964=CARTESIAN_POINT('Ctrl Pts',(-5.06551066928822,-0.000578487979984235,
0.708336844637072));
#59965=CARTESIAN_POINT('Ctrl Pts',(-5.06491070355288,0.856117806205452,
0.681555887547458));
#59966=CARTESIAN_POINT('Ctrl Pts',(-4.45481520994778,3.38770743142078,0.602442099343825));
#59967=CARTESIAN_POINT('Ctrl Pts',(-0.476761969141785,5.95830217192949,
0.470995480026171));
#59968=CARTESIAN_POINT('Ctrl Pts',(4.70955374493753,3.67573393888292,0.313996986684114));
#59969=CARTESIAN_POINT('Ctrl Pts',(5.49957691269067,-0.955274817987675,
0.183164908899066));
#59970=CARTESIAN_POINT('Ctrl Pts',(3.61105296193539,-3.84612671226304,0.0784992466710263));
#59971=CARTESIAN_POINT('Ctrl Pts',(2.11876087752236,-4.68487601374969,0.0261664155570096));
#59972=CARTESIAN_POINT('Ctrl Pts',(1.31303618635654,-4.90075024188321,0.));
#59973=CARTESIAN_POINT('',(-1.31785621200034,-4.9071451662202,1.75207071073658E-15));
#59974=CARTESIAN_POINT('Origin',(0.,0.,0.));
#59975=CARTESIAN_POINT('Ctrl Pts',(-5.0799445016814,0.00237344505285278,
0.791663155362921));
#59976=CARTESIAN_POINT('Ctrl Pts',(-5.08079896874729,0.146309621287887,
0.787131872330397));
#59977=CARTESIAN_POINT('Ctrl Pts',(-5.01057089916491,1.95175929947146,0.730267758183854));
#59978=CARTESIAN_POINT('Ctrl Pts',(-2.85914249825567,5.24623219278067,0.621070812923292));
#59979=CARTESIAN_POINT('Ctrl Pts',(2.79949684465664,5.27806149196883,0.464072319581235));
#59980=CARTESIAN_POINT('Ctrl Pts',(5.94469888877439,0.578168532022547,0.307073826239177));
#59981=CARTESIAN_POINT('Ctrl Pts',(3.79743415440745,-4.56550609975241,0.152383053045432));
#59982=CARTESIAN_POINT('Ctrl Pts',(0.216274136307286,-5.31234397836678,
0.0500251109657079));
#59983=CARTESIAN_POINT('Ctrl Pts',(-1.31785621200034,-4.9071451662202,1.74231289118421E-15));
#59984=CARTESIAN_POINT('Origin',(0.,0.,10.2083368446371));
#59985=CARTESIAN_POINT('',(-5.06594495534805,0.00113798286105304,1.79166315536292));
#59986=CARTESIAN_POINT('',(-5.0788676065064,-0.0031096904011537,1.70833684463707));
#59987=CARTESIAN_POINT('',(-5.0736,1.10600941455115E-13,10.2083368446371));
#59988=CARTESIAN_POINT('Ctrl Pts',(-5.0788676065064,-0.00310969040115398,
1.70833684463707));
#59989=CARTESIAN_POINT('Ctrl Pts',(-5.06820560204524,1.46267013662722,1.66221954089824));
#59990=CARTESIAN_POINT('Ctrl Pts',(-3.63653147921883,4.60995381904077,1.56376940604539));
#59991=CARTESIAN_POINT('Ctrl Pts',(1.67938795492248,5.73354207176578,1.41298644007852));
#59992=CARTESIAN_POINT('Ctrl Pts',(5.70869045070874,1.76202618095205,1.25598794673646));
#59993=CARTESIAN_POINT('Ctrl Pts',(4.61877209773216,-3.78910839602635,1.0989894533944));
#59994=CARTESIAN_POINT('Ctrl Pts',(-0.612224753988487,-5.94330155793046,
0.941990960052346));
#59995=CARTESIAN_POINT('Ctrl Pts',(-4.49644008704084,-3.30864398166895,
0.811773423799902));
#59996=CARTESIAN_POINT('Ctrl Pts',(-5.06608310024492,-0.817957632158887,
0.733888718661477));
#59997=CARTESIAN_POINT('Ctrl Pts',(-5.06551066928822,-0.000578487979984235,
0.708336844637072));
#59998=CARTESIAN_POINT('Ctrl Pts',(-5.06594495534805,0.00113798286105242,
1.79166315536292));
#59999=CARTESIAN_POINT('Ctrl Pts',(-5.06751102530523,0.764702257078156,
1.76779552568118));
#60000=CARTESIAN_POINT('Ctrl Pts',(-4.54967353500429,3.20046203254748,1.69159506488542));
#60001=CARTESIAN_POINT('Ctrl Pts',(-0.800856996403053,5.92047503909791,
1.56306177297564));
#60002=CARTESIAN_POINT('Ctrl Pts',(4.49633411524324,3.93401017093414,1.40606327963358));
#60003=CARTESIAN_POINT('Ctrl Pts',(5.76163326143087,-1.58003046734643,1.24906478629152));
#60004=CARTESIAN_POINT('Ctrl Pts',(1.86064021890344,-5.67731097226746,1.09206629294947));
#60005=CARTESIAN_POINT('Ctrl Pts',(-3.54825609197855,-4.71238753324782,
0.939599082639932));
#60006=CARTESIAN_POINT('Ctrl Pts',(-5.07093053185417,-1.51604242073639,
0.839464703444417));
#60007=CARTESIAN_POINT('Ctrl Pts',(-5.0799445016814,0.00237344505285278,
0.791663155362921));
#60008=CARTESIAN_POINT('Origin',(0.,0.,10.2083368446371));
#60009=CARTESIAN_POINT('',(-5.07643096335186,-0.00399326016102722,2.79166315536292));
#60010=CARTESIAN_POINT('',(-5.07274549324388,0.00436695056987321,2.70833684463708));
#60011=CARTESIAN_POINT('',(-5.0736,1.10600941455115E-13,10.2083368446371));
#60012=CARTESIAN_POINT('Ctrl Pts',(-5.07274549324388,0.00436695056987284,
2.70833684463708));
#60013=CARTESIAN_POINT('Ctrl Pts',(-5.07638654156454,0.422701167110148,
2.69521602536304));
#60014=CARTESIAN_POINT('Ctrl Pts',(-4.83926758888069,2.50550600890858,2.62976237497499));
#60015=CARTESIAN_POINT('Ctrl Pts',(-1.97561166336026,5.63828895889383,2.51197589347292));
#60016=CARTESIAN_POINT('Ctrl Pts',(3.6128915810316,4.75818989009414,2.35497740013087));
#60017=CARTESIAN_POINT('Ctrl Pts',(5.96174508817349,-0.388546134793637,
2.19797890678881));
#60018=CARTESIAN_POINT('Ctrl Pts',(2.96474106500057,-5.18686823314646,2.04098041344675));
#60019=CARTESIAN_POINT('Ctrl Pts',(-2.69071315072611,-5.33417912211988,
1.88398192010469));
#60020=CARTESIAN_POINT('Ctrl Pts',(-4.98091385691211,-2.06009093973243,
1.77310073050147));
#60021=CARTESIAN_POINT('Ctrl Pts',(-5.08030459382418,-0.200662320374615,
1.71455237201226));
#60022=CARTESIAN_POINT('Ctrl Pts',(-5.0788676065064,-0.00310969040115398,
1.70833684463707));
#60023=CARTESIAN_POINT('Ctrl Pts',(-5.07643096335186,-0.00399326016102722,
2.79166315536292));
#60024=CARTESIAN_POINT('Ctrl Pts',(-5.06457082001664,1.37091447103077,2.74845917903196));
#60025=CARTESIAN_POINT('Ctrl Pts',(-3.7827320999117,4.43074150154599,2.65292237158698));
#60026=CARTESIAN_POINT('Ctrl Pts',(1.36220151697138,5.81702256793933,2.50505273302799));
#60027=CARTESIAN_POINT('Ctrl Pts',(5.60328669734595,2.07280630409542,2.34805423968593));
#60028=CARTESIAN_POINT('Ctrl Pts',(4.81994564291905,-3.53007932713903,2.19105574634387));
#60029=CARTESIAN_POINT('Ctrl Pts',(-0.285401937658034,-5.96757024490932,
2.03405725300181));
#60030=CARTESIAN_POINT('Ctrl Pts',(-4.39760317314566,-3.49692096558582,
1.90092638934149));
#60031=CARTESIAN_POINT('Ctrl Pts',(-5.0640772165997,-0.90951008575328,1.8201283567952));
#60032=CARTESIAN_POINT('Ctrl Pts',(-5.06594495534805,0.00113798286105242,
1.79166315536292));
#60033=CARTESIAN_POINT('Origin',(0.,0.,10.2083368446371));
#60034=CARTESIAN_POINT('',(-5.07544700173093,0.00419220993169878,3.79166315536292));
#60035=CARTESIAN_POINT('',(-5.06752990436066,-0.00289155559083432,3.70833684463708));
#60036=CARTESIAN_POINT('',(-5.0736,1.10600941455115E-13,10.2083368446371));
#60037=CARTESIAN_POINT('Ctrl Pts',(-5.06752990436066,-0.00289155559083445,
3.70833684463708));
#60038=CARTESIAN_POINT('Ctrl Pts',(-5.06201314247005,1.03465176096834,3.67587967871383));
#60039=CARTESIAN_POINT('Ctrl Pts',(-4.25079971500112,3.75301601020252,3.59108968167655));
#60040=CARTESIAN_POINT('Ctrl Pts',(0.164021032340792,5.97213939901987,3.45396685352527));
#60041=CARTESIAN_POINT('Ctrl Pts',(5.07168429591276,3.15774768001703,3.29696836018321));
#60042=CARTESIAN_POINT('Ctrl Pts',(5.43160651478565,-2.48817267483047,3.13996986684115));
#60043=CARTESIAN_POINT('Ctrl Pts',(0.921047975843499,-5.90296718493849,
2.9829713734991));
#60044=CARTESIAN_POINT('Ctrl Pts',(-3.96942410407231,-4.18159504957827,
2.83909369943107));
#60045=CARTESIAN_POINT('Ctrl Pts',(-5.06186409728241,-1.24583899384963,
2.74754885647706));
#60046=CARTESIAN_POINT('Ctrl Pts',(-5.07274549324388,0.00436695056987284,
2.70833684463708));
#60047=CARTESIAN_POINT('Ctrl Pts',(-5.07544700173093,0.00419220993169878,
3.79166315536292));
#60048=CARTESIAN_POINT('Ctrl Pts',(-5.07831876722643,0.329194847520769,
3.78145566349676));
#60049=CARTESIAN_POINT('Ctrl Pts',(-4.90302280847942,2.31737130051307,3.71891534051658));
#60050=CARTESIAN_POINT('Ctrl Pts',(-2.2821043825461,5.52135344516299,3.60404218642239));
#60051=CARTESIAN_POINT('Ctrl Pts',(3.34628151701835,4.94931755856517,3.44704369308033));
#60052=CARTESIAN_POINT('Ctrl Pts',(5.9740820006751,-0.0607341045204584,
3.29004519973827));
#60053=CARTESIAN_POINT('Ctrl Pts',(3.24496813195078,-5.01632594473331,3.13304670639622));
#60054=CARTESIAN_POINT('Ctrl Pts',(-2.39388416789017,-5.47381611497205,
2.97604821305415));
#60055=CARTESIAN_POINT('Ctrl Pts',(-4.9251294092353,-2.24779066275208,2.86225369604306));
#60056=CARTESIAN_POINT('Ctrl Pts',(-5.0789369717198,-0.294506636106011,
2.80079201014598));
#60057=CARTESIAN_POINT('Ctrl Pts',(-5.07643096335186,-0.00399326016102722,
2.79166315536292));
#60058=CARTESIAN_POINT('Origin',(0.,0.,10.2083368446371));
#60059=CARTESIAN_POINT('',(-5.06623538659821,-0.00165077865025204,4.79166315536292));
#60060=CARTESIAN_POINT('',(-5.08150150384863,-0.000304682560140652,4.70833684463708));
#60061=CARTESIAN_POINT('',(-5.0736,1.10600941455115E-13,10.2083368446371));
#60062=CARTESIAN_POINT('Ctrl Pts',(-5.08150150384863,-0.000304682560140828,
4.70833684463708));
#60063=CARTESIAN_POINT('Ctrl Pts',(-5.08004199361202,1.64362562632391,4.65654333206461));
#60064=CARTESIAN_POINT('Ctrl Pts',(-3.32694734261784,4.95128314317388,4.55241698837811));
#60065=CARTESIAN_POINT('Ctrl Pts',(2.28210462993784,5.52135404368456,4.39595781357762));
#60066=CARTESIAN_POINT('Ctrl Pts',(5.86414511529741,1.14243341683897,4.23895932023555));
#60067=CARTESIAN_POINT('Ctrl Pts',(4.18785084798745,-4.2608986517151,4.0819608268935));
#60068=CARTESIAN_POINT('Ctrl Pts',(-1.24365772802729,-5.8435149929827,3.92496233355144));
#60069=CARTESIAN_POINT('Ctrl Pts',(-4.66764902476596,-2.94237266391977,
3.80042100613263));
#60070=CARTESIAN_POINT('Ctrl Pts',(-5.07090818182747,-0.638247816504467,
3.72821250982785));
#60071=CARTESIAN_POINT('Ctrl Pts',(-5.06752990436066,-0.00289155559083445,
3.70833684463708));
#60072=CARTESIAN_POINT('Ctrl Pts',(-5.06623538659821,-0.00165077865025218,
4.79166315536292));
#60073=CARTESIAN_POINT('Ctrl Pts',(-5.06341382264369,0.943369534950495,
4.76211931684755));
#60074=CARTESIAN_POINT('Ctrl Pts',(-4.35931582912874,3.56626810599387,4.68024264721815));
#60075=CARTESIAN_POINT('Ctrl Pts',(-0.164021014606317,5.97213875156532,
4.54603314647473));
#60076=CARTESIAN_POINT('Ctrl Pts',(4.89071815558305,3.43135837605058,4.38903465313268));
#60077=CARTESIAN_POINT('Ctrl Pts',(5.55998718173337,-2.18629522837624,4.23203615979062));
#60078=CARTESIAN_POINT('Ctrl Pts',(1.24365759322077,-5.84351435953346,4.07503766644856));
#60079=CARTESIAN_POINT('Ctrl Pts',(-3.83471277836695,-4.36379434722342,
3.92824666497267));
#60080=CARTESIAN_POINT('Ctrl Pts',(-5.06359550115425,-1.33706248264138,
3.83378849461079));
#60081=CARTESIAN_POINT('Ctrl Pts',(-5.07544700173093,0.00419220993169878,
3.79166315536292));
#60082=CARTESIAN_POINT('Origin',(0.,0.,10.2083368446371));
#60083=CARTESIAN_POINT('',(-5.08061550220448,-0.00187835596255306,5.79166315536292));
#60084=CARTESIAN_POINT('',(-5.06818254924878,0.00327741817492065,5.70833684463708));
#60085=CARTESIAN_POINT('',(-5.0736,1.10600941455115E-13,10.2083368446371));
#60086=CARTESIAN_POINT('Ctrl Pts',(-5.06818254924878,0.00327741817492046,
5.70833684463708));
#60087=CARTESIAN_POINT('Ctrl Pts',(-5.07183456953104,0.603958443996534,
5.68953981652941));
#60088=CARTESIAN_POINT('Ctrl Pts',(-4.69736642816282,2.87259326592426,5.61840995730772));
#60089=CARTESIAN_POINT('Ctrl Pts',(-1.36220166545199,5.81702319809857,5.49494726697201));
#60090=CARTESIAN_POINT('Ctrl Pts',(4.10035928902097,4.34515876133492,5.33794877362997));
#60091=CARTESIAN_POINT('Ctrl Pts',(5.88615929841981,-1.02297668832719,5.1809502802879));
#60092=CARTESIAN_POINT('Ctrl Pts',(2.3938844275315,-5.47381670826519,5.02395178694585));
#60093=CARTESIAN_POINT('Ctrl Pts',(-3.24496848378481,-5.01632648853908,
4.86695329360378));
#60094=CARTESIAN_POINT('Ctrl Pts',(-5.07375293308448,-1.69557487064781,
4.7617483128342));
#60095=CARTESIAN_POINT('Ctrl Pts',(-5.08151670152288,-0.0174226970094883,
4.70887616317863));
#60096=CARTESIAN_POINT('Ctrl Pts',(-5.08150150384863,-0.000304682560140828,
4.70833684463708));
#60097=CARTESIAN_POINT('Ctrl Pts',(-5.08061550220448,-0.00187835596255308,
5.79166315536293));
#60098=CARTESIAN_POINT('Ctrl Pts',(-5.07313315332044,1.5503069404754,5.74278297019833));
#60099=CARTESIAN_POINT('Ctrl Pts',(-3.48999114796195,4.77754415127511,5.64156995391971));
#60100=CARTESIAN_POINT('Ctrl Pts',(1.97561144788205,5.63828834519714,5.48802410652708));
#60101=CARTESIAN_POINT('Ctrl Pts',(5.79259970947732,1.46257867915377,5.33102561318502));
#60102=CARTESIAN_POINT('Ctrl Pts',(4.41540665009831,-4.0246153410012,5.17402711984296));
#60103=CARTESIAN_POINT('Ctrl Pts',(-0.92104787574744,-5.90296654461282,
5.01702862650091));
#60104=CARTESIAN_POINT('Ctrl Pts',(-4.58281307585404,-3.13076536575022,
4.88957397167423));
#60105=CARTESIAN_POINT('Ctrl Pts',(-5.0684118336446,-0.730603481292581,
4.81445214796157));
#60106=CARTESIAN_POINT('Ctrl Pts',(-5.06623538659821,-0.00165077865025218,
4.79166315536292));
#60107=CARTESIAN_POINT('Origin',(0.,0.,10.2083368446371));
#60108=CARTESIAN_POINT('',(-5.07032350272244,0.00406483722298734,6.79166315536293));
#60109=CARTESIAN_POINT('',(-5.07176207912418,-0.00429478512726797,6.70833684463708));
#60110=CARTESIAN_POINT('',(-5.0736,1.10600941455115E-13,10.2083368446371));
#60111=CARTESIAN_POINT('Ctrl Pts',(-5.07176207912418,-0.00429478512726802,
6.70833684463708));
#60112=CARTESIAN_POINT('Ctrl Pts',(-5.06152064599786,1.21211560888524,6.67020346988019));
#60113=CARTESIAN_POINT('Ctrl Pts',(-4.01723926286446,4.11367300543969,6.57973726400929));
#60114=CARTESIAN_POINT('Ctrl Pts',(0.800857062853464,5.92047566764934,6.43693822702436));
#60115=CARTESIAN_POINT('Ctrl Pts',(5.37989341709942,2.59808361512381,6.27993973368231));
#60116=CARTESIAN_POINT('Ctrl Pts',(5.13483694964473,-3.0539846259906,6.12294124034024));
#60117=CARTESIAN_POINT('Ctrl Pts',(0.285401972927619,-5.96757088942664,
5.96594274699819));
#60118=CARTESIAN_POINT('Ctrl Pts',(-4.20869589117159,-3.8219142963774,5.8277412817638));
#60119=CARTESIAN_POINT('Ctrl Pts',(-5.06166697497504,-1.0683984039935,5.74187264764343));
#60120=CARTESIAN_POINT('Ctrl Pts',(-5.06818254924878,0.00327741817492046,
5.70833684463708));
#60121=CARTESIAN_POINT('Ctrl Pts',(-5.07032350272244,0.00406483722298713,
6.79166315536293));
#60122=CARTESIAN_POINT('Ctrl Pts',(-5.07426970367213,0.511087407033013,
6.77577945466313));
#60123=CARTESIAN_POINT('Ctrl Pts',(-4.77323782375589,2.68406204063008,6.70756292284932));
#60124=CARTESIAN_POINT('Ctrl Pts',(-1.67938775292856,5.73354154736347,6.58701355992148));
#60125=CARTESIAN_POINT('Ctrl Pts',(3.85566217988192,4.56363706615652,6.43001506657943));
#60126=CARTESIAN_POINT('Ctrl Pts',(5.93344523009267,-0.69834389981148,6.27301657323736));
#60127=CARTESIAN_POINT('Ctrl Pts',(2.69071284975304,-5.33417856632519,6.11601807989532));
#60128=CARTESIAN_POINT('Ctrl Pts',(-2.96474073765194,-5.18686765769478,
5.95901958655325));
#60129=CARTESIAN_POINT('Ctrl Pts',(-5.0286520759667,-1.88246391579033,5.85090127837579));
#60130=CARTESIAN_POINT('Ctrl Pts',(-5.08114401701022,-0.111516776080137,
5.79511580131235));
#60131=CARTESIAN_POINT('Ctrl Pts',(-5.08061550220448,-0.00187835596255308,
5.79166315536293));
#60132=CARTESIAN_POINT('Origin',(0.,0.,10.2083368446371));
#60133=CARTESIAN_POINT('',(-5.0667809979009,-0.000656412822606089,7.79166315536293));
#60134=CARTESIAN_POINT('',(-5.07934275226421,0.00276793540382957,7.70833684463708));
#60135=CARTESIAN_POINT('',(-5.0736,1.10600941455115E-13,10.2083368446371));
#60136=CARTESIAN_POINT('',(-1.31303618635646,-4.90075024188322,8.));
#60137=CARTESIAN_POINT('Ctrl Pts',(-1.31303618635644,-4.90075024188323,
8.));
#60138=CARTESIAN_POINT('Ctrl Pts',(-2.11876087752226,-4.68487601374973,
7.97383358444299));
#60139=CARTESIAN_POINT('Ctrl Pts',(-3.61103600209076,-3.84612122823184,
7.92150075332897));
#60140=CARTESIAN_POINT('Ctrl Pts',(-4.8640953672922,-1.92805050100101,7.85205513844995));
#60141=CARTESIAN_POINT('Ctrl Pts',(-5.07037793642002,-0.54712311490011,
7.80877593912793));
#60142=CARTESIAN_POINT('Ctrl Pts',(-5.0667809979009,-0.000656412822605951,
7.79166315536293));
#60143=CARTESIAN_POINT('',(1.31785785677863,-4.90714579947409,8.00000000000001));
#60144=CARTESIAN_POINT('Origin',(0.,0.,8.));
#60145=CARTESIAN_POINT('Ctrl Pts',(1.31785785677863,-4.90714579947409,8.00000000000001));
#60146=CARTESIAN_POINT('Ctrl Pts',(-0.216269591468087,-5.31234554625424,
7.9499748890343));
#60147=CARTESIAN_POINT('Ctrl Pts',(-3.61771514871704,-4.60298607712906,
7.85275383724664));
#60148=CARTESIAN_POINT('Ctrl Pts',(-5.07021586478366,-1.49689387689792,
7.75553278545901));
#60149=CARTESIAN_POINT('Ctrl Pts',(-5.07934275226421,0.00276793540382986,
7.70833684463708));
#60150=CARTESIAN_POINT('Origin',(0.,0.,10.2083368446371));
#60151=CARTESIAN_POINT('Ctrl Pts',(-5.07934275226421,0.00276793540383012,
7.70833684463708));
#60152=CARTESIAN_POINT('Ctrl Pts',(-5.08033613895975,0.165993799129837,
7.70319995434499));
#60153=CARTESIAN_POINT('Ctrl Pts',(-4.99920696262547,1.99102187228673,7.64573023293889));
#60154=CARTESIAN_POINT('Ctrl Pts',(-2.799497488489,5.27806255262917,7.53592768041876));
#60155=CARTESIAN_POINT('Ctrl Pts',(2.8591428156985,5.24623244979999,7.37892918707671));
#60156=CARTESIAN_POINT('Ctrl Pts',(5.95237094349663,0.509586379962791,7.22193069373465));
#60157=CARTESIAN_POINT('Ctrl Pts',(3.70900729550924,-4.68371090122276,7.06493220039259));
#60158=CARTESIAN_POINT('Ctrl Pts',(-1.86064034918539,-5.67731151891722,
6.90793370705054));
#60159=CARTESIAN_POINT('Ctrl Pts',(-4.81412133745352,-2.5752195014975,6.78906858846536));
#60160=CARTESIAN_POINT('Ctrl Pts',(-5.07557560949328,-0.457240961862529,
6.72253630099421));
#60161=CARTESIAN_POINT('Ctrl Pts',(-5.07176207912418,-0.00429478512726802,
6.70833684463708));
#60162=CARTESIAN_POINT('Ctrl Pts',(-5.0667809979009,-0.000656412822605951,
7.79166315536293));
#60163=CARTESIAN_POINT('Ctrl Pts',(-5.05937809100424,1.12403395819613,7.75644310801391));
#60164=CARTESIAN_POINT('Ctrl Pts',(-4.14423912611421,3.92453560182124,7.66889022955088));
#60165=CARTESIAN_POINT('Ctrl Pts',(0.476758320675261,5.95830042580594,7.52900451997384));
#60166=CARTESIAN_POINT('Ctrl Pts',(5.22810884028568,2.88800998678043,7.37200602663177));
#60167=CARTESIAN_POINT('Ctrl Pts',(5.29527916712856,-2.76679132542031,7.21500753328971));
#60168=CARTESIAN_POINT('Ctrl Pts',(0.612224870220684,-5.9433011663707,7.05800903994766));
#60169=CARTESIAN_POINT('Ctrl Pts',(-4.08954628424525,-4.00704976176015,
6.91689424730539));
#60170=CARTESIAN_POINT('Ctrl Pts',(-5.0612679560476,-1.15942546766541,6.82811228577715));
#60171=CARTESIAN_POINT('Ctrl Pts',(-5.07032350272244,0.00406483722298713,
6.79166315536293));
#60172=CARTESIAN_POINT('Ctrl Pts',(3.43378788736183,2.93584158413004,8.));
#60173=CARTESIAN_POINT('Ctrl Pts',(3.91646501574697,2.37129788193754,7.97383358444299));
#60174=CARTESIAN_POINT('Ctrl Pts',(4.58922505888624,1.00348867934585,7.92150075332897));
#60175=CARTESIAN_POINT('Ctrl Pts',(4.5186273771248,-2.07044295135642,7.81683509110093));
#60176=CARTESIAN_POINT('Ctrl Pts',(1.60472354186206,-5.07186039848098,7.68600301331589));
#60177=CARTESIAN_POINT('Ctrl Pts',(-3.35287702678038,-4.13364886539305,
7.52900451997383));
#60178=CARTESIAN_POINT('Ctrl Pts',(-5.29341307506948,0.514825336495039,
7.37200602663177));
#60179=CARTESIAN_POINT('Ctrl Pts',(-2.49279205665034,4.69981218407846,7.21500753328972));
#60180=CARTESIAN_POINT('Ctrl Pts',(2.5459028018807,4.67146930189292,7.05800903994766));
#60181=CARTESIAN_POINT('Ctrl Pts',(5.3002451572812,0.453757463748993,6.90101054660559));
#60182=CARTESIAN_POINT('Ctrl Pts',(3.30265841006127,-4.17057610454098,6.74401205326355));
#60183=CARTESIAN_POINT('Ctrl Pts',(-1.6567935859217,-5.05532050508283,6.58701355992147));
#60184=CARTESIAN_POINT('Ctrl Pts',(-5.13040478426442,-1.40692675790748,
6.43001506657944));
#60185=CARTESIAN_POINT('Ctrl Pts',(-4.00372822142153,3.50301097463029,6.27301657323735));
#60186=CARTESIAN_POINT('Ctrl Pts',(0.713117312304132,5.27184424225852,6.11601807989532));
#60187=CARTESIAN_POINT('Ctrl Pts',(4.79048673232043,2.31344454671744,5.95901958655324));
#60188=CARTESIAN_POINT('Ctrl Pts',(4.57227799378301,-2.71939826633338,5.8020210932112));
#60189=CARTESIAN_POINT('Ctrl Pts',(0.254134098705802,-5.31377983792714,
5.64502259986913));
#60190=CARTESIAN_POINT('Ctrl Pts',(-4.2918858010234,-3.14333365162852,5.48802410652709));
#60191=CARTESIAN_POINT('Ctrl Pts',(-4.98940618387219,1.8457154089275,5.33102561318501));
#60192=CARTESIAN_POINT('Ctrl Pts',(-1.21296250672023,5.17972574763675,5.17402711984298));
#60193=CARTESIAN_POINT('Ctrl Pts',(3.65113492943364,3.86911482852823,5.0170286265009));
#60194=CARTESIAN_POINT('Ctrl Pts',(5.24128748234707,-0.910902107712505,
4.86003013315885));
#60195=CARTESIAN_POINT('Ctrl Pts',(2.13161687410921,-4.87412003976763,4.70303163981679));
#60196=CARTESIAN_POINT('Ctrl Pts',(-2.88945844521027,-4.46675122075005,
4.54603314647474));
#60197=CARTESIAN_POINT('Ctrl Pts',(-5.31957818590282,-0.0540802448651307,
4.38903465313267));
#60198=CARTESIAN_POINT('Ctrl Pts',(-2.97967221743332,4.40708408702865,4.23203615979062));
#60199=CARTESIAN_POINT('Ctrl Pts',(2.0320833711569,4.91644931229421,4.07503766644856));
#60200=CARTESIAN_POINT('Ctrl Pts',(5.22168511404818,1.01727147763408,3.9180391731065));
#60201=CARTESIAN_POINT('Ctrl Pts',(3.7290411480005,-3.79408603038985,3.76104067976445));
#60202=CARTESIAN_POINT('Ctrl Pts',(-1.10740592494388,-5.20331517256929,
3.60404218642238));
#60203=CARTESIAN_POINT('Ctrl Pts',(-4.95085044410053,-1.94677080151586,
3.44704369308033));
#60204=CARTESIAN_POINT('Ctrl Pts',(-4.35490467170682,3.05542829226346,3.29004519973827));
#60205=CARTESIAN_POINT('Ctrl Pts',(0.146051328220124,5.31784783386984,3.13304670639621));
#60206=CARTESIAN_POINT('Ctrl Pts',(4.51604417531138,2.81179331862917,2.97604821305416));
#60207=CARTESIAN_POINT('Ctrl Pts',(4.83653428180639,-2.21557515407508,2.8190497197121));
#60208=CARTESIAN_POINT('Ctrl Pts',(0.820140431422849,-5.25625394192603,
2.66205122637004));
#60209=CARTESIAN_POINT('Ctrl Pts',(-3.93166697371103,-3.58368967284698,
2.50505273302798));
#60210=CARTESIAN_POINT('Ctrl Pts',(-5.15797858932007,1.30234262409331,2.34805423968593));
#60211=CARTESIAN_POINT('Ctrl Pts',(-1.75916895146362,5.02057315201092,2.19105574634387));
#60212=CARTESIAN_POINT('Ctrl Pts',(3.21707287531645,4.23689537527058,2.03405725300181));
#60213=CARTESIAN_POINT('Ctrl Pts',(5.30859229582462,-0.345978063005356,
1.87705875965975));
#60214=CARTESIAN_POINT('Ctrl Pts',(2.63993199038283,-4.61860886950043,1.7200602663177));
#60215=CARTESIAN_POINT('Ctrl Pts',(-2.39592583898866,-4.74978077281557,
1.56306177297564));
#60216=CARTESIAN_POINT('Ctrl Pts',(-5.28339345476216,-0.621835317076693,
1.40606327963358));
#60217=CARTESIAN_POINT('Ctrl Pts',(-3.43324656738056,4.06365773166108,1.24906478629152));
#60218=CARTESIAN_POINT('Ctrl Pts',(1.4953987175479,5.10539058946701,1.09206629294947));
#60219=CARTESIAN_POINT('Ctrl Pts',(5.08326164531879,1.56898332130955,0.935067799607405));
#60220=CARTESIAN_POINT('Ctrl Pts',(4.1127518220848,-3.37398384897273,0.778069306265351));
#60221=CARTESIAN_POINT('Ctrl Pts',(-0.545151052966628,-5.29216938925817,
0.621070812923291));
#60222=CARTESIAN_POINT('Ctrl Pts',(-4.71514359968435,-2.4636695471729,0.464072319581234));
#60223=CARTESIAN_POINT('Ctrl Pts',(-4.65533046585126,2.57160754473359,0.307073826239176));
#60224=CARTESIAN_POINT('Ctrl Pts',(-0.424529207286798,5.30552657624457,
0.150075332897118));
#60225=CARTESIAN_POINT('Ctrl Pts',(4.1935876756527,3.27303039309136,-0.00692316044493899));
#60226=CARTESIAN_POINT('Ctrl Pts',(4.89705802532881,-0.850617472596149,
-0.137755238229987));
#60227=CARTESIAN_POINT('Ctrl Pts',(3.21543569039412,-3.42475539150235,-0.242420900458027));
#60228=CARTESIAN_POINT('Ctrl Pts',(1.88663512189109,-4.17161357046627,-0.294753731572044));
#60229=CARTESIAN_POINT('Ctrl Pts',(1.16918346556927,-4.36383719750628,-0.320920147129053));
#60230=CARTESIAN_POINT('Ctrl Pts',(3.574615437742,3.05624720968396,8.10697338237635));
#60231=CARTESIAN_POINT('Ctrl Pts',(4.0770882669231,2.46855026993857,8.08080696681934));
#60232=CARTESIAN_POINT('Ctrl Pts',(4.77743974901458,1.04464406144345,8.02847413570532));
#60233=CARTESIAN_POINT('Ctrl Pts',(4.7039466937149,-2.15535658568851,7.92380847347729));
#60234=CARTESIAN_POINT('Ctrl Pts',(1.67053695050899,-5.27986907555073,7.79297639569223));
#60235=CARTESIAN_POINT('Ctrl Pts',(-3.49038623640434,-4.30317932648753,
7.63597790235018));
#60236=CARTESIAN_POINT('Ctrl Pts',(-5.51050813771329,0.535939509353267,
7.47897940900812));
#60237=CARTESIAN_POINT('Ctrl Pts',(-2.59502720059656,4.8925623069287,7.32198091566607));
#60238=CARTESIAN_POINT('Ctrl Pts',(2.65031613981997,4.86305701786194,7.16498242232401));
#60239=CARTESIAN_POINT('Ctrl Pts',(5.51762041935301,0.472367102486928,7.00798392898195));
#60240=CARTESIAN_POINT('Ctrl Pts',(3.43810803854393,-4.34162103676824,6.85098543563989));
#60241=CARTESIAN_POINT('Ctrl Pts',(-1.72474250700959,-5.26265084302763,
6.69398694229783));
#60242=CARTESIAN_POINT('Ctrl Pts',(-5.34081450144173,-1.46462806485474,
6.53698844895577));
#60243=CARTESIAN_POINT('Ctrl Pts',(-4.16793033765764,3.64667752326241,6.37998995561372));
#60244=CARTESIAN_POINT('Ctrl Pts',(0.742363895820577,5.48805471738879,6.22299146227166));
#60245=CARTESIAN_POINT('Ctrl Pts',(4.98695562724675,2.40832423618623,6.0659929689296));
#60246=CARTESIAN_POINT('Ctrl Pts',(4.75979764573692,-2.83092705288579,5.90899447558755));
#60247=CARTESIAN_POINT('Ctrl Pts',(0.264556723446406,-5.53171018842698,
5.75199598224549));
#60248=CARTESIAN_POINT('Ctrl Pts',(-4.4679059233187,-3.27224900479161,5.59499748890343));
#60249=CARTESIAN_POINT('Ctrl Pts',(-5.19403322368223,1.92141244912467,5.43799899556137));
#60250=CARTESIAN_POINT('Ctrl Pts',(-1.26270889296415,5.39215823112403,5.28100050221931));
#60251=CARTESIAN_POINT('Ctrl Pts',(3.80087638262942,4.02779613946379,5.12400200887726));
#60252=CARTESIAN_POINT('Ctrl Pts',(5.45624475437132,-0.948260301250735,
4.96700351553519));
#60253=CARTESIAN_POINT('Ctrl Pts',(2.21903939191664,-5.07401892926682,4.81000502219315));
#60254=CARTESIAN_POINT('Ctrl Pts',(-3.00796179140179,-4.64994297667973,
4.65300652885108));
#60255=CARTESIAN_POINT('Ctrl Pts',(-5.53774634000859,-0.05629820027127,
4.49600803550903));
#60256=CARTESIAN_POINT('Ctrl Pts',(-3.10187543821507,4.58782875637178,4.33900954216697));
#60257=CARTESIAN_POINT('Ctrl Pts',(2.11542379075055,5.11808422275766,4.18201104882491));
#60258=CARTESIAN_POINT('Ctrl Pts',(5.43583844779792,1.05899212403571,4.02501255548285));
#60259=CARTESIAN_POINT('Ctrl Pts',(3.88197771466281,-3.94969023749826,3.8680140621408));
#60260=CARTESIAN_POINT('Ctrl Pts',(-1.15282319263835,-5.4167151127071,3.71101556879874));
#60261=CARTESIAN_POINT('Ctrl Pts',(-5.15389622421624,-2.0266123561262,3.55401707545668));
#60262=CARTESIAN_POINT('Ctrl Pts',(-4.53350934304161,3.18073844416463,3.39701858211462));
#60263=CARTESIAN_POINT('Ctrl Pts',(0.152041229593681,5.53594502225318,3.24002008877256));
#60264=CARTESIAN_POINT('Ctrl Pts',(4.70125754884517,2.92711143909179,3.08302159543051));
#60265=CARTESIAN_POINT('Ctrl Pts',(5.03489169279947,-2.30644099432688,2.92602310208845));
#60266=CARTESIAN_POINT('Ctrl Pts',(0.853776279563064,-5.47182502293018,
2.7690246087464));
#60267=CARTESIAN_POINT('Ctrl Pts',(-4.09291369219827,-3.730665040722,2.61202611540433));
#60268=CARTESIAN_POINT('Ctrl Pts',(-5.36951917175407,1.3557546948219,2.45502762206228));
#60269=CARTESIAN_POINT('Ctrl Pts',(-1.83131652209583,5.22647842097189,2.29802912872022));
#60270=CARTESIAN_POINT('Ctrl Pts',(3.34901244388816,4.41066021354511,2.14103063537816));
#60271=CARTESIAN_POINT('Ctrl Pts',(5.52630989327424,-0.360167420268118,
1.9840321420361));
#60272=CARTESIAN_POINT('Ctrl Pts',(2.74820168192207,-4.80802865738244,1.82703364869405));
#60273=CARTESIAN_POINT('Ctrl Pts',(-2.49418827623448,-4.94458022258368,
1.67003515535199));
#60274=CARTESIAN_POINT('Ctrl Pts',(-5.50007758969876,-0.647338215717022,
1.51303666200993));
#60275=CARTESIAN_POINT('Ctrl Pts',(-3.57405191698147,4.23031769514908,1.35603816866787));
#60276=CARTESIAN_POINT('Ctrl Pts',(1.55672846333943,5.31477441689994,1.19903967532582));
#60277=CARTESIAN_POINT('Ctrl Pts',(5.2917379137821,1.63333094119038,1.04204118198376));
#60278=CARTESIAN_POINT('Ctrl Pts',(4.28142524730059,-3.5123586979906,0.885042688641701));
#60279=CARTESIAN_POINT('Ctrl Pts',(-0.567508953307252,-5.50921344548227,
0.728044195299643));
#60280=CARTESIAN_POINT('Ctrl Pts',(-4.90852249920177,-2.56471030992692,
0.571045701957585));
#60281=CARTESIAN_POINT('Ctrl Pts',(-4.84625629098129,2.67707509338356,0.414047208615528));
#60282=CARTESIAN_POINT('Ctrl Pts',(-0.441940127905122,5.52311844147288,
0.257048715273468));
#60283=CARTESIAN_POINT('Ctrl Pts',(4.3655763654143,3.40726490835521,0.100050221931412));
#60284=CARTESIAN_POINT('Ctrl Pts',(5.09789765444943,-0.885503254393324,
-0.0307818558536364));
#60285=CARTESIAN_POINT('Ctrl Pts',(3.3473081142412,-3.56521249842258,-0.135447518081676));
#60286=CARTESIAN_POINT('Ctrl Pts',(1.96401037376818,-4.34270105156074,-0.187780349195693));
#60287=CARTESIAN_POINT('Ctrl Pts',(1.21713437249836,-4.54280821229859,-0.213946764752702));
#60288=CARTESIAN_POINT('Ctrl Pts',(3.71544298812217,3.17665283523789,8.21394676475271));
#60289=CARTESIAN_POINT('Ctrl Pts',(4.23771151809924,2.5658026579396,8.1877803491957));
#60290=CARTESIAN_POINT('Ctrl Pts',(4.96565443914292,1.08579944354106,8.13544751808168));
#60291=CARTESIAN_POINT('Ctrl Pts',(4.889266010305,-2.24027022002061,8.03078185585363));
#60292=CARTESIAN_POINT('Ctrl Pts',(1.73635035915592,-5.48787775262049,7.89994977806859));
#60293=CARTESIAN_POINT('Ctrl Pts',(-3.62789544602829,-4.472709787582,7.74295128472654));
#60294=CARTESIAN_POINT('Ctrl Pts',(-5.72760320035712,0.557053682211493,
7.58595279138447));
#60295=CARTESIAN_POINT('Ctrl Pts',(-2.69726234454278,5.08531242977894,7.42895429804241));
#60296=CARTESIAN_POINT('Ctrl Pts',(2.75472947775923,5.05464473383097,7.27195580470038));
#60297=CARTESIAN_POINT('Ctrl Pts',(5.73499568142482,0.490976741224864,7.11495731135828));
#60298=CARTESIAN_POINT('Ctrl Pts',(3.57355766702658,-4.5126659689955,6.95795881801627));
#60299=CARTESIAN_POINT('Ctrl Pts',(-1.7926914280975,-5.46998118097242,6.80096032467417));
#60300=CARTESIAN_POINT('Ctrl Pts',(-5.55122421861904,-1.522329371802,6.64396183133214));
#60301=CARTESIAN_POINT('Ctrl Pts',(-4.33213245389376,3.79034407189453,6.48696333799006));
#60302=CARTESIAN_POINT('Ctrl Pts',(0.771610479337022,5.70426519251906,6.32996484464802));
#60303=CARTESIAN_POINT('Ctrl Pts',(5.18342452217309,2.50320392565502,6.17296635130595));
#60304=CARTESIAN_POINT('Ctrl Pts',(4.94731729769082,-2.9424558394382,6.01596785796391));
#60305=CARTESIAN_POINT('Ctrl Pts',(0.274979348187014,-5.7496405389268,5.85896936462183));
#60306=CARTESIAN_POINT('Ctrl Pts',(-4.64392604561401,-3.40116435795471,
5.70197087127979));
#60307=CARTESIAN_POINT('Ctrl Pts',(-5.39866026349227,1.99710948932185,5.54497237793772));
#60308=CARTESIAN_POINT('Ctrl Pts',(-1.31245527920807,5.6045907146113,5.38797388459567));
#60309=CARTESIAN_POINT('Ctrl Pts',(3.95061783582519,4.18647745039935,5.23097539125361));
#60310=CARTESIAN_POINT('Ctrl Pts',(5.67120202639557,-0.985618494788963,
5.07397689791155));
#60311=CARTESIAN_POINT('Ctrl Pts',(2.30646190972407,-5.273917818766,4.9169784045695));
#60312=CARTESIAN_POINT('Ctrl Pts',(-3.1264651375933,-4.83313473260941,4.75997991122743));
#60313=CARTESIAN_POINT('Ctrl Pts',(-5.75591449411437,-0.058516155677411,
4.60298141788538));
#60314=CARTESIAN_POINT('Ctrl Pts',(-3.22407865899683,4.76857342571492,4.44598292454332));
#60315=CARTESIAN_POINT('Ctrl Pts',(2.19876421034419,5.31971913322111,4.28898443120126));
#60316=CARTESIAN_POINT('Ctrl Pts',(5.64999178154766,1.10071277043733,4.1319859378592));
#60317=CARTESIAN_POINT('Ctrl Pts',(4.03491428132513,-4.10529444460668,3.97498744451715));
#60318=CARTESIAN_POINT('Ctrl Pts',(-1.19824046033282,-5.6301150528449,3.81798895117509));
#60319=CARTESIAN_POINT('Ctrl Pts',(-5.35694200433196,-2.10645391073654,
3.66099045783303));
#60320=CARTESIAN_POINT('Ctrl Pts',(-4.7121140143764,3.30604859606581,3.50399196449097));
#60321=CARTESIAN_POINT('Ctrl Pts',(0.158031130967237,5.75404221063653,3.34699347114891));
#60322=CARTESIAN_POINT('Ctrl Pts',(4.88647092237896,3.04242955955441,3.18999497780686));
#60323=CARTESIAN_POINT('Ctrl Pts',(5.23324910379256,-2.39730683457867,3.0329964844648));
#60324=CARTESIAN_POINT('Ctrl Pts',(0.887412127703281,-5.68739610393434,
2.87599799112275));
#60325=CARTESIAN_POINT('Ctrl Pts',(-4.25416041068552,-3.87764040859701,
2.71899949778068));
#60326=CARTESIAN_POINT('Ctrl Pts',(-5.58105975418807,1.40916676555049,2.56200100443863));
#60327=CARTESIAN_POINT('Ctrl Pts',(-1.90346409272805,5.43238368993286,2.40500251109657));
#60328=CARTESIAN_POINT('Ctrl Pts',(3.48095201245988,4.58442505181962,2.24800401775452));
#60329=CARTESIAN_POINT('Ctrl Pts',(5.74402749072386,-0.374356777530876,
2.09100552441245));
#60330=CARTESIAN_POINT('Ctrl Pts',(2.85647137346132,-4.99744844526445,1.9340070310704));
#60331=CARTESIAN_POINT('Ctrl Pts',(-2.5924507134803,-5.13937967235178,1.77700853772834));
#60332=CARTESIAN_POINT('Ctrl Pts',(-5.71676172463537,-0.672841114357358,
1.62001004438628));
#60333=CARTESIAN_POINT('Ctrl Pts',(-3.71485726658238,4.39697765863709,1.46301155104423));
#60334=CARTESIAN_POINT('Ctrl Pts',(1.61805820913096,5.52415824433286,1.30601305770217));
#60335=CARTESIAN_POINT('Ctrl Pts',(5.50021418224542,1.69767856107122,1.14901456436011));
#60336=CARTESIAN_POINT('Ctrl Pts',(4.45009867251637,-3.65073354700848,0.992016071018051));
#60337=CARTESIAN_POINT('Ctrl Pts',(-0.589866853647869,-5.72625750170636,
0.835017577675995));
#60338=CARTESIAN_POINT('Ctrl Pts',(-5.1019013987192,-2.66575107268096,0.678019084333936));
#60339=CARTESIAN_POINT('Ctrl Pts',(-5.0371821161113,2.78254264203352,0.521020590991878));
#60340=CARTESIAN_POINT('Ctrl Pts',(-0.459351048523452,5.74071030670118,
0.36402209764982));
#60341=CARTESIAN_POINT('Ctrl Pts',(4.53756505517591,3.54149942361907,0.207023604307763));
#60342=CARTESIAN_POINT('Ctrl Pts',(5.29873728357006,-0.920389036190499,
0.076191526522715));
#60343=CARTESIAN_POINT('Ctrl Pts',(3.47918053808829,-3.70566960534281,-0.0284741357053249));
#60344=CARTESIAN_POINT('Ctrl Pts',(2.04138562564527,-4.51378853265522,-0.0808069668193416));
#60345=CARTESIAN_POINT('Ctrl Pts',(1.26508527942745,-4.7217792270909,-0.106973382376351));
#60346=CARTESIAN_POINT('Ctrl Pts',(3.85627053850235,3.29705846079181,8.32092014712906));
#60347=CARTESIAN_POINT('Ctrl Pts',(4.39833476927537,2.66305504594064,8.29475373157205));
#60348=CARTESIAN_POINT('Ctrl Pts',(5.15386912927126,1.12695482563867,8.24242090045804));
#60349=CARTESIAN_POINT('Ctrl Pts',(5.0745853268951,-2.3251838543527,8.13775523822997));
#60350=CARTESIAN_POINT('Ctrl Pts',(1.80216376780286,-5.69588642969024,8.00692316044496));
#60351=CARTESIAN_POINT('Ctrl Pts',(-3.76540465565226,-4.64224024867649,
7.84992466710287));
#60352=CARTESIAN_POINT('Ctrl Pts',(-5.94469826300093,0.578167855069724,
7.69292617376083));
#60353=CARTESIAN_POINT('Ctrl Pts',(-2.799497488489,5.27806255262917,7.53592768041876));
#60354=CARTESIAN_POINT('Ctrl Pts',(2.8591428156985,5.24623244979999,7.37892918707671));
#60355=CARTESIAN_POINT('Ctrl Pts',(5.95237094349663,0.509586379962791,7.22193069373465));
#60356=CARTESIAN_POINT('Ctrl Pts',(3.70900729550924,-4.68371090122276,7.06493220039259));
#60357=CARTESIAN_POINT('Ctrl Pts',(-1.86064034918539,-5.67731151891722,
6.90793370705054));
#60358=CARTESIAN_POINT('Ctrl Pts',(-5.76163393579635,-1.58003067874924,
6.75093521370848));
#60359=CARTESIAN_POINT('Ctrl Pts',(-4.49633457012987,3.93401062052664,6.59393672036642));
#60360=CARTESIAN_POINT('Ctrl Pts',(0.800857062853464,5.92047566764934,6.43693822702436));
#60361=CARTESIAN_POINT('Ctrl Pts',(5.37989341709942,2.59808361512381,6.27993973368231));
#60362=CARTESIAN_POINT('Ctrl Pts',(5.13483694964473,-3.0539846259906,6.12294124034024));
#60363=CARTESIAN_POINT('Ctrl Pts',(0.285401972927619,-5.96757088942664,
5.96594274699819));
#60364=CARTESIAN_POINT('Ctrl Pts',(-4.81994616790931,-3.5300797111178,5.80894425365613));
#60365=CARTESIAN_POINT('Ctrl Pts',(-5.6032873033023,2.07280652951902,5.65194576031408));
#60366=CARTESIAN_POINT('Ctrl Pts',(-1.36220166545199,5.81702319809857,5.49494726697201));
#60367=CARTESIAN_POINT('Ctrl Pts',(4.10035928902097,4.34515876133492,5.33794877362997));
#60368=CARTESIAN_POINT('Ctrl Pts',(5.88615929841981,-1.02297668832719,5.1809502802879));
#60369=CARTESIAN_POINT('Ctrl Pts',(2.3938844275315,-5.47381670826519,5.02395178694585));
#60370=CARTESIAN_POINT('Ctrl Pts',(-3.24496848378481,-5.01632648853908,
4.86695329360378));
#60371=CARTESIAN_POINT('Ctrl Pts',(-5.97408264822014,-0.0607341110835563,
4.70995480026174));
#60372=CARTESIAN_POINT('Ctrl Pts',(-3.34628187977858,4.94931809505806,4.55295630691966));
#60373=CARTESIAN_POINT('Ctrl Pts',(2.28210462993784,5.52135404368456,4.39595781357762));
#60374=CARTESIAN_POINT('Ctrl Pts',(5.86414511529741,1.14243341683897,4.23895932023555));
#60375=CARTESIAN_POINT('Ctrl Pts',(4.18785084798745,-4.2608986517151,4.0819608268935));
#60376=CARTESIAN_POINT('Ctrl Pts',(-1.24365772802729,-5.8435149929827,3.92496233355144));
#60377=CARTESIAN_POINT('Ctrl Pts',(-5.55998778444767,-2.18629546534688,
3.76796384020939));
#60378=CARTESIAN_POINT('Ctrl Pts',(-4.89071868571119,3.43135874796699,3.61096534686732));
#60379=CARTESIAN_POINT('Ctrl Pts',(0.164021032340792,5.97213939901987,3.45396685352527));
#60380=CARTESIAN_POINT('Ctrl Pts',(5.07168429591276,3.15774768001703,3.29696836018321));
#60381=CARTESIAN_POINT('Ctrl Pts',(5.43160651478565,-2.48817267483047,3.13996986684115));
#60382=CARTESIAN_POINT('Ctrl Pts',(0.921047975843499,-5.90296718493849,
2.9829713734991));
#60383=CARTESIAN_POINT('Ctrl Pts',(-4.41540712917277,-4.02461577647203,
2.82597288015704));
#60384=CARTESIAN_POINT('Ctrl Pts',(-5.79260033662206,1.46257883627908,2.66897438681498));
#60385=CARTESIAN_POINT('Ctrl Pts',(-1.97561166336026,5.63828895889383,2.51197589347292));
#60386=CARTESIAN_POINT('Ctrl Pts',(3.6128915810316,4.75818989009414,2.35497740013087));
#60387=CARTESIAN_POINT('Ctrl Pts',(5.96174508817349,-0.388546134793637,
2.19797890678881));
#60388=CARTESIAN_POINT('Ctrl Pts',(2.96474106500057,-5.18686823314646,2.04098041344675));
#60389=CARTESIAN_POINT('Ctrl Pts',(-2.69071315072611,-5.33417912211988,
1.88398192010469));
#60390=CARTESIAN_POINT('Ctrl Pts',(-5.93344585957197,-0.698344012997689,
1.72698342676263));
#60391=CARTESIAN_POINT('Ctrl Pts',(-3.85566261618328,4.5636376221251,1.56998493342058));
#60392=CARTESIAN_POINT('Ctrl Pts',(1.67938795492248,5.73354207176578,1.41298644007852));
#60393=CARTESIAN_POINT('Ctrl Pts',(5.70869045070874,1.76202618095205,1.25598794673646));
#60394=CARTESIAN_POINT('Ctrl Pts',(4.61877209773216,-3.78910839602635,1.0989894533944));
#60395=CARTESIAN_POINT('Ctrl Pts',(-0.612224753988487,-5.94330155793046,
0.941990960052346));
#60396=CARTESIAN_POINT('Ctrl Pts',(-5.29528029823663,-2.76679183543498,
0.784992466710288));
#60397=CARTESIAN_POINT('Ctrl Pts',(-5.22810794124132,2.88801019068349,0.62799397336823));
#60398=CARTESIAN_POINT('Ctrl Pts',(-0.476761969141785,5.95830217192949,
0.470995480026171));
#60399=CARTESIAN_POINT('Ctrl Pts',(4.70955374493753,3.67573393888292,0.313996986684114));
#60400=CARTESIAN_POINT('Ctrl Pts',(5.49957691269067,-0.955274817987675,
0.183164908899066));
#60401=CARTESIAN_POINT('Ctrl Pts',(3.61105296193539,-3.84612671226304,0.0784992466710263));
#60402=CARTESIAN_POINT('Ctrl Pts',(2.11876087752236,-4.68487601374969,0.0261664155570096));
#60403=CARTESIAN_POINT('Ctrl Pts',(1.31303618635654,-4.90075024188321,0.));
#60404=CARTESIAN_POINT('Ctrl Pts',(1.31303618635654,-4.90075024188321,0.));
#60405=CARTESIAN_POINT('Ctrl Pts',(1.45239813196613,-4.85517621763986,-2.47434559251786E-16));
#60406=CARTESIAN_POINT('Ctrl Pts',(1.58927692318379,-4.80351009978137,-1.74819720228364E-15));
#60407=CARTESIAN_POINT('Ctrl Pts',(1.72341090925204,-4.74604460400692,-1.88737914186277E-15));
#60408=CARTESIAN_POINT('Ctrl Pts',(1.85925417986306,-4.68784681892573,-2.02833469262672E-15));
#60409=CARTESIAN_POINT('Ctrl Pts',(1.99228283138741,-4.62370052461763,2.98138735348004E-16));
#60410=CARTESIAN_POINT('Ctrl Pts',(2.12220346118141,-4.55386096654418,1.11022302462516E-16));
#60411=CARTESIAN_POINT('Ctrl Pts',(2.25247560296862,-4.48383245124121,-7.66003908251115E-17));
#60412=CARTESIAN_POINT('Ctrl Pts',(2.37962344910693,-4.40807936214696,-4.32517766211178E-16));
#60413=CARTESIAN_POINT('Ctrl Pts',(2.50332095055395,-4.32681677710386,-4.44089209850063E-16));
#60414=CARTESIAN_POINT('Ctrl Pts',(2.62609735089877,-4.24615930579203,-4.55574487888469E-16));
#60415=CARTESIAN_POINT('Ctrl Pts',(2.74547509807873,-4.16007358686041,1.08564249317406E-16));
#60416=CARTESIAN_POINT('Ctrl Pts',(2.86109774307792,-4.06873562676994,-5.55111512312578E-17));
#60417=CARTESIAN_POINT('Ctrl Pts',(2.90211866182286,-4.03633049506564,-1.13722271327984E-16));
#60418=CARTESIAN_POINT('Ctrl Pts',(2.94266654026491,-4.00326397860027,-2.92134559916121E-15));
#60419=CARTESIAN_POINT('Ctrl Pts',(2.98272412781597,-3.96954306736407,-2.99760216648792E-15));
#60420=CARTESIAN_POINT('Ctrl Pts',(2.99979215651063,-3.95517501587181,-3.03009412016909E-15));
#60421=CARTESIAN_POINT('Ctrl Pts',(3.01677225892353,-3.94068710954429,-2.12566972362838E-15));
#60422=CARTESIAN_POINT('Ctrl Pts',(3.03364729547102,-3.92609378878367,-2.1094237467878E-15));
#60423=CARTESIAN_POINT('Ctrl Pts',(3.14433957478624,-3.83036848867988,-2.00285780240447E-15));
#60424=CARTESIAN_POINT('Ctrl Pts',(3.25067225380611,-3.72997908311154,-3.12896148123733E-15));
#60425=CARTESIAN_POINT('Ctrl Pts',(3.35235973413124,-3.62516300488518,-3.10862446895044E-15));
#60426=CARTESIAN_POINT('Ctrl Pts',(3.36192986162372,-3.61529843523825,-3.10671048898182E-15));
#60427=CARTESIAN_POINT('Ctrl Pts',(3.37145882014037,-3.60539462864919,-2.66105468162811E-15));
#60428=CARTESIAN_POINT('Ctrl Pts',(3.38094635546186,-3.59545176562119,-2.692290834716E-15));
#60429=CARTESIAN_POINT('Ctrl Pts',(3.48180408426425,-3.48975365237926,-3.02597608841997E-15));
#60430=CARTESIAN_POINT('Ctrl Pts',(3.57798405787049,-3.37964444416285,-3.04382432431275E-15));
#60431=CARTESIAN_POINT('Ctrl Pts',(3.66918347167548,-3.26550314479251,-2.94209101525666E-15));
#60432=CARTESIAN_POINT('Ctrl Pts',(3.75971565071324,-3.15219692801907,-2.84110200923889E-15));
#60433=CARTESIAN_POINT('Ctrl Pts',(3.84534031026112,-3.03491668112307,-1.42999735083781E-15));
#60434=CARTESIAN_POINT('Ctrl Pts',(3.92571655230007,-2.91400844798661,-1.72084568816899E-15));
#60435=CARTESIAN_POINT('Ctrl Pts',(3.99657720672258,-2.80741430638731,-1.97726105417974E-15));
#60436=CARTESIAN_POINT('Ctrl Pts',(4.06335815473368,-2.69799970084542,-4.7182430533371E-15));
#60437=CARTESIAN_POINT('Ctrl Pts',(4.12579259176727,-2.58599222827228,-4.96824803519758E-15));
#60438=CARTESIAN_POINT('Ctrl Pts',(4.14218217787996,-2.55658928649489,-5.03387653084013E-15));
#60439=CARTESIAN_POINT('Ctrl Pts',(4.15827206325859,-2.52700763769101,-2.22246092678142E-15));
#60440=CARTESIAN_POINT('Ctrl Pts',(4.17405702945515,-2.49725134739943,-2.08166817117217E-15));
#60441=CARTESIAN_POINT('Ctrl Pts',(4.18546582852437,-2.47574458376403,-1.97990829160411E-15));
#60442=CARTESIAN_POINT('Ctrl Pts',(4.1967169159508,-2.45414332829404,-3.10559938199478E-15));
#60443=CARTESIAN_POINT('Ctrl Pts',(4.20779634099434,-2.4324729617879,-3.08086889333481E-15));
#60444=CARTESIAN_POINT('Ctrl Pts',(4.27314972651924,-2.30464757272886,-2.93499298792804E-15));
#60445=CARTESIAN_POINT('Ctrl Pts',(4.3326198595779,-2.17426195525281,-5.03888835755339E-15));
#60446=CARTESIAN_POINT('Ctrl Pts',(4.38592260758549,-2.04167340157391,-4.413136522885E-15));
#60447=CARTESIAN_POINT('Ctrl Pts',(4.43841100193019,-1.9111105215869,-3.79694485758248E-15));
#60448=CARTESIAN_POINT('Ctrl Pts',(4.48491932736646,-1.77841080748911,-3.47246432590996E-15));
#60449=CARTESIAN_POINT('Ctrl Pts',(4.52512906800885,-1.64389810614591,-3.30291349825984E-15));
#60450=CARTESIAN_POINT('Ctrl Pts',(4.53704337373435,-1.60404145892158,-3.25267491516128E-15));
#60451=CARTESIAN_POINT('Ctrl Pts',(4.54840435272953,-1.56402555907027,-1.86047514559207E-15));
#60452=CARTESIAN_POINT('Ctrl Pts',(4.55920284487768,-1.52385866802948,-1.74860126378462E-15));
#60453=CARTESIAN_POINT('Ctrl Pts',(4.59648625924208,-1.38517645000696,-1.33619040184573E-15));
#60454=CARTESIAN_POINT('Ctrl Pts',(4.62706837090021,-1.24469418107576,-3.1405520603229E-15));
#60455=CARTESIAN_POINT('Ctrl Pts',(4.6510479415724,-1.1028549274787,-3.44169137633799E-15));
#60456=CARTESIAN_POINT('Ctrl Pts',(4.66553556506662,-1.0171605782801,-3.62362928879583E-15));
#60457=CARTESIAN_POINT('Ctrl Pts',(4.67761212738266,-0.93097088404131,-3.48256637849421E-15));
#60458=CARTESIAN_POINT('Ctrl Pts',(4.68729033896278,-0.844384764732073,
-3.60822483003176E-15));
#60459=CARTESIAN_POINT('Ctrl Pts',(4.69282045363923,-0.794909594117687,
-3.68002586902689E-15));
#60460=CARTESIAN_POINT('Ctrl Pts',(4.6975673931995,-0.74530501799734,-2.90670583210387E-15));
#60461=CARTESIAN_POINT('Ctrl Pts',(4.70153256693874,-0.695589781678817,
-3.02535774210355E-15));
#60462=CARTESIAN_POINT('Ctrl Pts',(4.70300273002319,-0.67715691846114,-3.06935017962366E-15));
#60463=CARTESIAN_POINT('Ctrl Pts',(4.70436508297707,-0.658712562708346,
-1.39035176949888E-15));
#60464=CARTESIAN_POINT('Ctrl Pts',(4.70561925922056,-0.640267374588028,
-1.41553435639707E-15));
#60465=CARTESIAN_POINT('Ctrl Pts',(4.71515008316959,-0.500097409167311,
-1.60690363448191E-15));
#60466=CARTESIAN_POINT('Ctrl Pts',(4.71845154780466,-0.359714693128242,
-6.98970443009747E-16));
#60467=CARTESIAN_POINT('Ctrl Pts',(4.71567835888356,-0.219533504962576,
-9.0205620750794E-16));
#60468=CARTESIAN_POINT('Ctrl Pts',(4.71285964179518,-0.0770509255950372,
-1.1084760840775E-15));
#60469=CARTESIAN_POINT('Ctrl Pts',(4.70376507114378,0.065224279671225,-2.40577940367026E-15));
#60470=CARTESIAN_POINT('Ctrl Pts',(4.68850374693714,0.206855299208619,-2.26207941267376E-15));
#60471=CARTESIAN_POINT('Ctrl Pts',(4.67332604169022,0.347710302303635,-2.11916677430768E-15));
#60472=CARTESIAN_POINT('Ctrl Pts',(4.65204869880232,0.487928957857132,-3.70693630030531E-15));
#60473=CARTESIAN_POINT('Ctrl Pts',(4.62472984685344,0.627067645312151,-4.06619182768964E-15));
#60474=CARTESIAN_POINT('Ctrl Pts',(4.60512526025429,0.72691651350792,-4.32400120090221E-15));
#60475=CARTESIAN_POINT('Ctrl Pts',(4.58240838869996,0.826208961746935,-2.80327058352682E-15));
#60476=CARTESIAN_POINT('Ctrl Pts',(4.55658611607818,0.924773126569175,-2.94209101525666E-15));
#60477=CARTESIAN_POINT('Ctrl Pts',(4.54451163215688,0.970861688981747,-3.00700339130591E-15));
#60478=CARTESIAN_POINT('Ctrl Pts',(4.53175798542344,1.01679090044476,-4.8702446610021E-15));
#60479=CARTESIAN_POINT('Ctrl Pts',(4.51832500803005,1.062542528366,-4.8988590961585E-15));
#60480=CARTESIAN_POINT('Ctrl Pts',(4.51266846717592,1.08180824622589,-4.91090845176596E-15));
#60481=CARTESIAN_POINT('Ctrl Pts',(4.50689146090876,1.10104246936981,-1.58247074004002E-15));
#60482=CARTESIAN_POINT('Ctrl Pts',(4.50099394804091,1.12024381085806,-1.56819002228303E-15));
#60483=CARTESIAN_POINT('Ctrl Pts',(4.49471177106765,1.14069755603102,-1.55297784754686E-15));
#60484=CARTESIAN_POINT('Ctrl Pts',(4.48829554526876,1.1611051847425,-3.02768046308214E-15));
#60485=CARTESIAN_POINT('Ctrl Pts',(4.48174652480305,1.18146221251882,-3.05311331771918E-15));
#60486=CARTESIAN_POINT('Ctrl Pts',(4.4388367801027,1.31484320732769,-3.21975156617037E-15));
#60487=CARTESIAN_POINT('Ctrl Pts',(4.3902172033679,1.44609540153194,-2.42101694317024E-15));
#60488=CARTESIAN_POINT('Ctrl Pts',(4.33595560037894,1.57478564497199,-2.33146835171283E-15));
#60489=CARTESIAN_POINT('Ctrl Pts',(4.28905400984558,1.68602041819998,-2.25406607942409E-15));
#60490=CARTESIAN_POINT('Ctrl Pts',(4.23793630897375,1.79534112442678,-2.09120843630436E-15));
#60491=CARTESIAN_POINT('Ctrl Pts',(4.18261934387559,1.90245063170277,-1.54737334057131E-15));
#60492=CARTESIAN_POINT('Ctrl Pts',(4.15876651886949,1.94863654101668,-1.31287017598733E-15));
#60493=CARTESIAN_POINT('Ctrl Pts',(4.13413259613109,1.99441106904023,-3.34114378130206E-15));
#60494=CARTESIAN_POINT('Ctrl Pts',(4.1087175751394,2.03974918362091,-3.32373017997156E-15));
#60495=CARTESIAN_POINT('Ctrl Pts',(4.09757084929567,2.05963394128716,-3.31609278159812E-15));
#60496=CARTESIAN_POINT('Ctrl Pts',(4.08627386148571,2.07943474030452,-3.10826804513356E-15));
#60497=CARTESIAN_POINT('Ctrl Pts',(4.07482656400744,2.09914941832117,-3.21964677141295E-15));
#60498=CARTESIAN_POINT('Ctrl Pts',(4.06286705490573,2.11974623356295,-3.33600916115644E-15));
#60499=CARTESIAN_POINT('Ctrl Pts',(4.05074796307183,2.14024130439856,-5.56609850953026E-16));
#60500=CARTESIAN_POINT('Ctrl Pts',(4.03847105489573,2.16062996612303,-7.21644966006352E-16));
#60501=CARTESIAN_POINT('Ctrl Pts',(3.96920184151707,2.27566760746066,-1.65281203475204E-15));
#60502=CARTESIAN_POINT('Ctrl Pts',(3.89489673126452,2.38734604756407,-5.44084181235126E-15));
#60503=CARTESIAN_POINT('Ctrl Pts',(3.81559015152877,2.49525778868992,-3.92741394961149E-15));
#60504=CARTESIAN_POINT('Ctrl Pts',(3.73966418517796,2.5985695599563,-2.47849920176032E-15));
#60505=CARTESIAN_POINT('Ctrl Pts',(3.65915364949516,2.69842924853399,9.77632756533034E-16));
#60506=CARTESIAN_POINT('Ctrl Pts',(3.57405694815596,2.79444772885285,1.90646110009851E-15));
#60507=CARTESIAN_POINT('Ctrl Pts',(3.53072890723773,2.84333672899846,2.33391700333807E-15));
#60508=CARTESIAN_POINT('Ctrl Pts',(3.48621138925297,2.89122932971802,2.44271821993007E-16));
#60509=CARTESIAN_POINT('Ctrl Pts',(3.44055068766011,2.93810645203839,2.77555756156289E-16));
#60510=CARTESIAN_POINT('Ctrl Pts',(3.43378788736183,2.93584158413004,8.));
#60511=CARTESIAN_POINT('Ctrl Pts',(3.52723828091404,2.83914431545175,8.));
#60512=CARTESIAN_POINT('Ctrl Pts',(3.61594081851665,2.73846055769803,8.));
#60513=CARTESIAN_POINT('Ctrl Pts',(3.69984090589852,2.63418809372837,8.));
#60514=CARTESIAN_POINT('Ctrl Pts',(3.78516287227981,2.52814849421259,8.));
#60515=CARTESIAN_POINT('Ctrl Pts',(3.86551863442571,2.41839706286655,8.));
#60516=CARTESIAN_POINT('Ctrl Pts',(3.94081955158113,2.30530820215193,8.));
#60517=CARTESIAN_POINT('Ctrl Pts',(4.01714046916727,2.19068747846675,8.));
#60518=CARTESIAN_POINT('Ctrl Pts',(4.08826910733635,2.07263776324572,8.));
#60519=CARTESIAN_POINT('Ctrl Pts',(4.15407500660322,1.95151170764482,8.));
#60520=CARTESIAN_POINT('Ctrl Pts',(4.2198164513151,1.83050429073889,8.));
#60521=CARTESIAN_POINT('Ctrl Pts',(4.28024594506117,1.70642592249187,8.));
#60522=CARTESIAN_POINT('Ctrl Pts',(4.33518967485951,1.57960030623271,8.));
#60523=CARTESIAN_POINT('Ctrl Pts',(4.35307625782352,1.53831303076909,8.));
#60524=CARTESIAN_POINT('Ctrl Pts',(4.37038109771682,1.49673442540794,8.));
#60525=CARTESIAN_POINT('Ctrl Pts',(4.3870970941841,1.45487519313349,8.));
#60526=CARTESIAN_POINT('Ctrl Pts',(4.39376575085273,1.43817592851012,8.));
#60527=CARTESIAN_POINT('Ctrl Pts',(4.40033736934907,1.42144028204873,8.));
#60528=CARTESIAN_POINT('Ctrl Pts',(4.40681102745828,1.40467100393547,8.));
#60529=CARTESIAN_POINT('Ctrl Pts',(4.45934053196233,1.26859927210788,8.));
#60530=CARTESIAN_POINT('Ctrl Pts',(4.50544025366947,1.13027539792009,8.));
#60531=CARTESIAN_POINT('Ctrl Pts',(4.54499873531868,0.990127463611741,8.));
#60532=CARTESIAN_POINT('Ctrl Pts',(4.58299050839006,0.855530070216331,8.));
#60533=CARTESIAN_POINT('Ctrl Pts',(4.61494911931547,0.719249512352558,8.));
#60534=CARTESIAN_POINT('Ctrl Pts',(4.64085249468742,0.581767615475945,8.));
#60535=CARTESIAN_POINT('Ctrl Pts',(4.66691769963291,0.443426809811538,8.));
#60536=CARTESIAN_POINT('Ctrl Pts',(4.68685201899535,0.303868786404607,8.));
#60537=CARTESIAN_POINT('Ctrl Pts',(4.70058414747143,0.163565049614876,8.));
#60538=CARTESIAN_POINT('Ctrl Pts',(4.71271762019861,0.0395950789853681,
8.));
#60539=CARTESIAN_POINT('Ctrl Pts',(4.72000832561645,-0.0849577470138994,
8.));
#60540=CARTESIAN_POINT('Ctrl Pts',(4.7223733384523,-0.209772800136726,8.));
#60541=CARTESIAN_POINT('Ctrl Pts',(4.72292943816615,-0.239121315406544,
8.));
#60542=CARTESIAN_POINT('Ctrl Pts',(4.7232130590816,-0.268484329285888,8.));
#60543=CARTESIAN_POINT('Ctrl Pts',(4.72322285747563,-0.297857662780827,
8.));
#60544=CARTESIAN_POINT('Ctrl Pts',(4.72323033779459,-0.320281939952091,
8.));
#60545=CARTESIAN_POINT('Ctrl Pts',(4.72307812055779,-0.342714494826838,
8.));
#60546=CARTESIAN_POINT('Ctrl Pts',(4.72276611337907,-0.365130653249834,
8.));
#60547=CARTESIAN_POINT('Ctrl Pts',(4.72077139214363,-0.508441417465993,
8.));
#60548=CARTESIAN_POINT('Ctrl Pts',(4.71225120797944,-0.651280085007766,
8.));
#60549=CARTESIAN_POINT('Ctrl Pts',(4.69718547532262,-0.793154607131843,
8.));
#60550=CARTESIAN_POINT('Ctrl Pts',(4.68212772666397,-0.934953943670782,
8.));
#60551=CARTESIAN_POINT('Ctrl Pts',(4.66053153776914,-1.07579102267899,8.));
#60552=CARTESIAN_POINT('Ctrl Pts',(4.63232650453452,-1.21518583219434,8.));
#60553=CARTESIAN_POINT('Ctrl Pts',(4.62517817164043,-1.25051429622537,8.));
#60554=CARTESIAN_POINT('Ctrl Pts',(4.6176050749471,-1.28575013896589,8.));
#60555=CARTESIAN_POINT('Ctrl Pts',(4.60960553319191,-1.32088555816255,8.));
#60556=CARTESIAN_POINT('Ctrl Pts',(4.57835655312357,-1.45813667176012,8.));
#60557=CARTESIAN_POINT('Ctrl Pts',(4.54060431924761,-1.59385616146054,8.));
#60558=CARTESIAN_POINT('Ctrl Pts',(4.49667031501799,-1.72776662727194,8.));
#60559=CARTESIAN_POINT('Ctrl Pts',(4.46792000249182,-1.81539733178229,8.));
#60560=CARTESIAN_POINT('Ctrl Pts',(4.43652132007444,-1.90225320075805,8.));
#60561=CARTESIAN_POINT('Ctrl Pts',(4.4025528899726,-1.98825323145006,8.));
#60562=CARTESIAN_POINT('Ctrl Pts',(4.39064088821649,-2.01841160243036,8.));
#60563=CARTESIAN_POINT('Ctrl Pts',(4.37841279355623,-2.04846469658551,8.));
#60564=CARTESIAN_POINT('Ctrl Pts',(4.36587175340618,-2.07840891566329,8.));
#60565=CARTESIAN_POINT('Ctrl Pts',(4.35885849939885,-2.09515444968045,8.));
#60566=CARTESIAN_POINT('Ctrl Pts',(4.35174737519127,-2.11186593393486,8.));
#60567=CARTESIAN_POINT('Ctrl Pts',(4.34453891478344,-2.12854273059161,8.));
#60568=CARTESIAN_POINT('Ctrl Pts',(4.33664233992457,-2.14681148227446,8.));
#60569=CARTESIAN_POINT('Ctrl Pts',(4.32863248368416,-2.16503040522278,8.));
#60570=CARTESIAN_POINT('Ctrl Pts',(4.32051229345552,-2.18319454758947,8.));
#60571=CARTESIAN_POINT('Ctrl Pts',(4.26271734267779,-2.31247670532764,8.));
#60572=CARTESIAN_POINT('Ctrl Pts',(4.19930769062008,-2.43905306787665,8.));
#60573=CARTESIAN_POINT('Ctrl Pts',(4.1306563766664,-2.56266246904431,8.));
#60574=CARTESIAN_POINT('Ctrl Pts',(4.05932719227651,-2.69109348165625,8.));
#60575=CARTESIAN_POINT('Ctrl Pts',(3.98233931388035,-2.81632224208436,8.));
#60576=CARTESIAN_POINT('Ctrl Pts',(3.90005514682149,-2.93804448640157,8.));
#60577=CARTESIAN_POINT('Ctrl Pts',(3.81788412514087,-3.05959935575629,8.));
#60578=CARTESIAN_POINT('Ctrl Pts',(3.73043085662906,-3.17765799919859,8.));
#60579=CARTESIAN_POINT('Ctrl Pts',(3.63800695579095,-3.29189623321801,8.));
#60580=CARTESIAN_POINT('Ctrl Pts',(3.56857767496828,-3.37771254651463,8.));
#60581=CARTESIAN_POINT('Ctrl Pts',(3.49634236728105,-3.46137260211582,8.));
#60582=CARTESIAN_POINT('Ctrl Pts',(3.42141741611953,-3.54272769601374,8.));
#60583=CARTESIAN_POINT('Ctrl Pts',(3.38628453897598,-3.58087571579362,8.));
#60584=CARTESIAN_POINT('Ctrl Pts',(3.35056009922657,-3.61851677693959,8.));
#60585=CARTESIAN_POINT('Ctrl Pts',(3.3142552023334,-3.65563464117867,8.));
#60586=CARTESIAN_POINT('Ctrl Pts',(3.299200603776,-3.67102635395701,8.));
#60587=CARTESIAN_POINT('Ctrl Pts',(3.28404454782071,-3.68632972667595,8.));
#60588=CARTESIAN_POINT('Ctrl Pts',(3.26879310797022,-3.70153828550149,8.));
#60589=CARTESIAN_POINT('Ctrl Pts',(3.16313496534899,-3.80689935915782,8.));
#60590=CARTESIAN_POINT('Ctrl Pts',(3.05310906400962,-3.90750842604698,8.));
#60591=CARTESIAN_POINT('Ctrl Pts',(2.93905349297435,-4.00304219163214,8.));
#60592=CARTESIAN_POINT('Ctrl Pts',(2.83343523748027,-4.09150880111292,8.));
#60593=CARTESIAN_POINT('Ctrl Pts',(2.72436063892977,-4.17562341526862,8.));
#60594=CARTESIAN_POINT('Ctrl Pts',(2.61206707761722,-4.25510461849443,8.));
#60595=CARTESIAN_POINT('Ctrl Pts',(2.56057116079448,-4.29155334611912,8.));
#60596=CARTESIAN_POINT('Ctrl Pts',(2.50839792228814,-4.3270273021059,8.));
#60597=CARTESIAN_POINT('Ctrl Pts',(2.45556847535629,-4.3614972584752,8.));
#60598=CARTESIAN_POINT('Ctrl Pts',(2.42827791858812,-4.37930369703788,8.));
#60599=CARTESIAN_POINT('Ctrl Pts',(2.40081223344856,-4.39684219182932,8.));
#60600=CARTESIAN_POINT('Ctrl Pts',(2.37317422709578,-4.41410855841438,8.));
#60601=CARTESIAN_POINT('Ctrl Pts',(2.35241127848289,-4.42707985155184,8.));
#60602=CARTESIAN_POINT('Ctrl Pts',(2.33155925321721,-4.43989244410762,8.));
#60603=CARTESIAN_POINT('Ctrl Pts',(2.31062069154639,-4.45254421740167,8.));
#60604=CARTESIAN_POINT('Ctrl Pts',(2.18359867140573,-4.52929513408044,8.));
#60605=CARTESIAN_POINT('Ctrl Pts',(2.05338150515115,-4.60013897577206,8.00000000000001));
#60606=CARTESIAN_POINT('Ctrl Pts',(1.9202708514578,-4.66473499429566,8.00000000000001));
#60607=CARTESIAN_POINT('Ctrl Pts',(1.79118849882964,-4.72737615644222,8.00000000000001));
#60608=CARTESIAN_POINT('Ctrl Pts',(1.65938453798209,-4.78414231274042,8.00000000000001));
#60609=CARTESIAN_POINT('Ctrl Pts',(1.52510693593821,-4.83468454964306,8.00000000000001));
#60610=CARTESIAN_POINT('Ctrl Pts',(1.45664940136588,-4.86045204085127,8.00000000000001));
#60611=CARTESIAN_POINT('Ctrl Pts',(1.38754853402863,-4.88460115986285,8.00000000000001));
#60612=CARTESIAN_POINT('Ctrl Pts',(1.31785785677859,-4.9071457994741,8.00000000000001));
#60613=CARTESIAN_POINT('Ctrl Pts',(-4.51611343680291,-0.0038242599945422,
6.38741669750802));
#60614=CARTESIAN_POINT('Ctrl Pts',(-4.51950916701914,-0.407146869176555,
6.40161615386516));
#60615=CARTESIAN_POINT('Ctrl Pts',(-4.46982237313174,-0.809647705501708,
6.41581561022229));
#60616=CARTESIAN_POINT('Ctrl Pts',(-4.36369015740015,-1.19666942701374,
6.43001506657943));
#60617=CARTESIAN_POINT('Ctrl Pts',(-3.97253438481685,-2.62305800696593,
6.48234789769345));
#60618=CARTESIAN_POINT('Ctrl Pts',(-2.81466398536927,-3.83918925602438,
6.53468072880746));
#60619=CARTESIAN_POINT('Ctrl Pts',(-1.40915345298166,-4.2997974804633,6.58701355992148));
#60620=CARTESIAN_POINT('Ctrl Pts',(-0.0036429205940397,-4.76040570490222,
6.6393463910355));
#60621=CARTESIAN_POINT('Ctrl Pts',(1.64950774473362,-4.4654909047216,6.69167922214952));
#60622=CARTESIAN_POINT('Ctrl Pts',(2.8090142019341,-3.54731124324962,6.74401205326355));
#60623=CARTESIAN_POINT('Ctrl Pts',(3.96852065913458,-2.62913158177766,6.79634488437757));
#60624=CARTESIAN_POINT('Ctrl Pts',(4.63438290820789,-1.08768705901433,6.84867771549158));
#60625=CARTESIAN_POINT('Ctrl Pts',(4.50825697351113,0.385987175391315,6.9010105466056));
#60626=CARTESIAN_POINT('Ctrl Pts',(4.38213103881437,1.85966140979697,6.95334337771962));
#60627=CARTESIAN_POINT('Ctrl Pts',(3.46401692034753,3.26556535584495,7.00567620883364));
#60628=CARTESIAN_POINT('Ctrl Pts',(2.16517738469227,3.97324114256653,7.05800903994766));
#60629=CARTESIAN_POINT('Ctrl Pts',(0.866337849037014,4.6809169292881,7.11034187106168));
#60630=CARTESIAN_POINT('Ctrl Pts',(-0.81322710380666,4.69036455668328,7.1626747021757));
#60631=CARTESIAN_POINT('Ctrl Pts',(-2.11977974996502,3.9975905624503,7.21500753328971));
#60632=CARTESIAN_POINT('Ctrl Pts',(-3.42633239612339,3.30481656821732,7.26734036440373));
#60633=CARTESIAN_POINT('Ctrl Pts',(-4.35987273559643,1.90982095235617,7.31967319551775));
#60634=CARTESIAN_POINT('Ctrl Pts',(-4.50322023061811,0.437577444110917,
7.37200602663177));
#60635=CARTESIAN_POINT('Ctrl Pts',(-4.51729094569115,0.293064846108908,
7.37714291692385));
#60636=CARTESIAN_POINT('Ctrl Pts',(-4.52374814565307,0.14780796397411,7.38227980721594));
#60637=CARTESIAN_POINT('Ctrl Pts',(-4.52286359173795,0.00246468782935438,
7.38741669750802));
#60638=CARTESIAN_POINT('Ctrl Pts',(-1.31303618635644,-4.90075024188323,
8.));
#60639=CARTESIAN_POINT('Ctrl Pts',(-2.11876087752226,-4.68487601374973,
7.97383358444299));
#60640=CARTESIAN_POINT('Ctrl Pts',(-3.61103600209076,-3.84612122823184,
7.92150075332897));
#60641=CARTESIAN_POINT('Ctrl Pts',(-5.49959712288033,-0.955281493922513,
7.81683509110094));
#60642=CARTESIAN_POINT('Ctrl Pts',(-4.70954440514987,3.67573693777646,7.68600301331588));
#60643=CARTESIAN_POINT('Ctrl Pts',(0.476758320675261,5.95830042580594,7.52900451997384));
#60644=CARTESIAN_POINT('Ctrl Pts',(5.22810884028568,2.88800998678043,7.37200602663177));
#60645=CARTESIAN_POINT('Ctrl Pts',(5.29527916712856,-2.76679132542031,7.21500753328971));
#60646=CARTESIAN_POINT('Ctrl Pts',(0.612224870220684,-5.9433011663707,7.05800903994766));
#60647=CARTESIAN_POINT('Ctrl Pts',(-4.61877163601819,-3.7891077783966,6.90101054660559));
#60648=CARTESIAN_POINT('Ctrl Pts',(-5.70868984087812,1.76202584286959,6.74401205326355));
#60649=CARTESIAN_POINT('Ctrl Pts',(-1.67938775292856,5.73354154736347,6.58701355992148));
#60650=CARTESIAN_POINT('Ctrl Pts',(3.85566217988192,4.56363706615652,6.43001506657943));
#60651=CARTESIAN_POINT('Ctrl Pts',(5.93344523009267,-0.69834389981148,6.27301657323736));
#60652=CARTESIAN_POINT('Ctrl Pts',(2.69071284975304,-5.33417856632519,6.11601807989532));
#60653=CARTESIAN_POINT('Ctrl Pts',(-2.96474073765194,-5.18686765769478,
5.95901958655325));
#60654=CARTESIAN_POINT('Ctrl Pts',(-5.96174444561926,-0.38854610033802,
5.8020210932112));
#60655=CARTESIAN_POINT('Ctrl Pts',(-3.61289118716291,4.75818937870979,5.64502259986913));
#60656=CARTESIAN_POINT('Ctrl Pts',(1.97561144788205,5.63828834519714,5.48802410652708));
#60657=CARTESIAN_POINT('Ctrl Pts',(5.79259970947732,1.46257867915377,5.33102561318502));
#60658=CARTESIAN_POINT('Ctrl Pts',(4.41540665009831,-4.0246153410012,5.17402711984296));
#60659=CARTESIAN_POINT('Ctrl Pts',(-0.92104787574744,-5.90296654461282,
5.01702862650091));
#60660=CARTESIAN_POINT('Ctrl Pts',(-5.43160592614493,-2.48817240536104,
4.86003013315885));
#60661=CARTESIAN_POINT('Ctrl Pts',(-5.07168374606222,3.15774733785514,4.70303163981679));
#60662=CARTESIAN_POINT('Ctrl Pts',(-0.164021014606317,5.97213875156532,
4.54603314647473));
#60663=CARTESIAN_POINT('Ctrl Pts',(4.89071815558305,3.43135837605058,4.38903465313268));
#60664=CARTESIAN_POINT('Ctrl Pts',(5.55998718173337,-2.18629522837624,4.23203615979062));
#60665=CARTESIAN_POINT('Ctrl Pts',(1.24365759322077,-5.84351435953346,4.07503766644856));
#60666=CARTESIAN_POINT('Ctrl Pts',(-4.1878503940255,-4.26089818984331,3.91803917310651));
#60667=CARTESIAN_POINT('Ctrl Pts',(-5.86414447963045,1.14243329300625,3.76104067976444));
#60668=CARTESIAN_POINT('Ctrl Pts',(-2.2821043825461,5.52135344516299,3.60404218642239));
#60669=CARTESIAN_POINT('Ctrl Pts',(3.34628151701835,4.94931755856517,3.44704369308033));
#60670=CARTESIAN_POINT('Ctrl Pts',(5.9740820006751,-0.0607341045204584,
3.29004519973827));
#60671=CARTESIAN_POINT('Ctrl Pts',(3.24496813195078,-5.01632594473331,3.13304670639622));
#60672=CARTESIAN_POINT('Ctrl Pts',(-2.39388416789017,-5.47381611497205,
2.97604821305415));
#60673=CARTESIAN_POINT('Ctrl Pts',(-5.88615866062065,-1.02297657731424,
2.8190497197121));
#60674=CARTESIAN_POINT('Ctrl Pts',(-4.10035884408111,4.34515829009749,2.66205122637004));
#60675=CARTESIAN_POINT('Ctrl Pts',(1.36220151697138,5.81702256793933,2.50505273302799));
#60676=CARTESIAN_POINT('Ctrl Pts',(5.60328669734595,2.07280630409542,2.34805423968593));
#60677=CARTESIAN_POINT('Ctrl Pts',(4.81994564291905,-3.53007932713903,2.19105574634387));
#60678=CARTESIAN_POINT('Ctrl Pts',(-0.285401937658034,-5.96757024490932,
2.03405725300181));
#60679=CARTESIAN_POINT('Ctrl Pts',(-5.13483640041478,-3.05398429071519,
1.87705875965975));
#60680=CARTESIAN_POINT('Ctrl Pts',(-5.37989282152843,2.59808332599247,1.7200602663177));
#60681=CARTESIAN_POINT('Ctrl Pts',(-0.800856996403053,5.92047503909791,
1.56306177297564));
#60682=CARTESIAN_POINT('Ctrl Pts',(4.49633411524324,3.93401017093414,1.40606327963358));
#60683=CARTESIAN_POINT('Ctrl Pts',(5.76163326143087,-1.58003046734643,1.24906478629152));
#60684=CARTESIAN_POINT('Ctrl Pts',(1.86064021890344,-5.67731097226746,1.09206629294947));
#60685=CARTESIAN_POINT('Ctrl Pts',(-3.70900698411085,-4.68371027734449,
0.935067799607409));
#60686=CARTESIAN_POINT('Ctrl Pts',(-5.9523702132809,0.509586132109229,0.77806930626535));
#60687=CARTESIAN_POINT('Ctrl Pts',(-2.85914249825567,5.24623219278067,0.621070812923292));
#60688=CARTESIAN_POINT('Ctrl Pts',(2.79949684465664,5.27806149196883,0.464072319581235));
#60689=CARTESIAN_POINT('Ctrl Pts',(5.94469888877439,0.578168532022547,0.307073826239177));
#60690=CARTESIAN_POINT('Ctrl Pts',(3.76540065952631,-4.64224087416102,0.150075332897119));
#60691=CARTESIAN_POINT('Ctrl Pts',(-1.80215437063507,-5.69588361575389,
-0.00692316044493745));
#60692=CARTESIAN_POINT('Ctrl Pts',(-5.07460576691081,-2.32518978947096,
-0.137755238229986));
#60693=CARTESIAN_POINT('Ctrl Pts',(-5.15385204348173,1.12695990370127,-0.242420900458024));
#60694=CARTESIAN_POINT('Ctrl Pts',(-4.39833476927544,2.66305504594052,-0.294753731572044));
#60695=CARTESIAN_POINT('Ctrl Pts',(-3.85627053850243,3.2970584607917,-0.320920147129053));
#60696=CARTESIAN_POINT('Ctrl Pts',(-1.26508527942735,-4.72177922709092,
8.10697338237635));
#60697=CARTESIAN_POINT('Ctrl Pts',(-2.04138562564518,-4.51378853265526,
8.08080696681934));
#60698=CARTESIAN_POINT('Ctrl Pts',(-3.47916419760203,-3.70566432158352,
8.02847413570533));
#60699=CARTESIAN_POINT('Ctrl Pts',(-5.29875675570167,-0.920395468326166,
7.92380847347728));
#60700=CARTESIAN_POINT('Ctrl Pts',(-4.53755605646894,3.54150231299569,7.79297639569223));
#60701=CARTESIAN_POINT('Ctrl Pts',(0.459347533295664,5.74070862434451,7.63597790235019));
#60702=CARTESIAN_POINT('Ctrl Pts',(5.03718298232336,2.78254244557681,7.47897940900812));
#60703=CARTESIAN_POINT('Ctrl Pts',(5.10190030891819,-2.66575058129155,7.32198091566607));
#60704=CARTESIAN_POINT('Ctrl Pts',(0.589866965635366,-5.72625712444602,
7.16498242232401));
#60705=CARTESIAN_POINT('Ctrl Pts',(-4.45009822766378,-3.650732951934,7.00798392898195));
#60706=CARTESIAN_POINT('Ctrl Pts',(-5.50021359468528,1.69767823533522,6.8509854356399));
#60707=CARTESIAN_POINT('Ctrl Pts',(-1.61805801451367,5.52415773908126,6.69398694229783));
#60708=CARTESIAN_POINT('Ctrl Pts',(3.71485684621434,4.39697712297199,6.53698844895578));
#60709=CARTESIAN_POINT('Ctrl Pts',(5.71676111814409,-0.672841005304612,
6.37998995561372));
#60710=CARTESIAN_POINT('Ctrl Pts',(2.5924504234985,-5.13937913685421,6.22299146227166));
#60711=CARTESIAN_POINT('Ctrl Pts',(-2.85647105806718,-4.99744789082776,
6.0659929689296));
#60712=CARTESIAN_POINT('Ctrl Pts',(-5.74402687163513,-0.374356744333544,
5.90899447558755));
#60713=CARTESIAN_POINT('Ctrl Pts',(-3.48095163297493,4.58442455911056,5.75199598224549));
#60714=CARTESIAN_POINT('Ctrl Pts',(1.90346388511891,5.43238309864782,5.59499748890343));
#60715=CARTESIAN_POINT('Ctrl Pts',(5.58105914994609,1.40916661416325,5.43799899556138));
#60716=CARTESIAN_POINT('Ctrl Pts',(4.25415994910644,-3.8776399890292,5.28100050221931));
#60717=CARTESIAN_POINT('Ctrl Pts',(-0.887412031262641,-5.68739548699278,
5.12400200887726));
#60718=CARTESIAN_POINT('Ctrl Pts',(-5.23324853664848,-2.39730657495003,
4.9670035155352));
#60719=CARTESIAN_POINT('Ctrl Pts',(-4.88647039260848,3.04242922988797,4.81000502219315));
#60720=CARTESIAN_POINT('Ctrl Pts',(-0.15803111388041,5.75404158682643,4.65300652885108));
#60721=CARTESIAN_POINT('Ctrl Pts',(4.71211350360807,3.30604823773145,4.49600803550903));
#60722=CARTESIAN_POINT('Ctrl Pts',(5.35694142362824,-2.10645368241985,4.33900954216697));
#60723=CARTESIAN_POINT('Ctrl Pts',(1.19824033044931,-5.63011444252866,4.18201104882491));
#60724=CARTESIAN_POINT('Ctrl Pts',(-4.03491384394147,-4.10529399960203,
4.02501255548286));
#60725=CARTESIAN_POINT('Ctrl Pts',(-5.6499911690947,1.10071265112688,3.86801406214079));
#60726=CARTESIAN_POINT('Ctrl Pts',(-2.19876397198699,5.31971855655701,3.71101556879874));
#60727=CARTESIAN_POINT('Ctrl Pts',(3.22407830948427,4.76857290881427,3.55401707545668));
#60728=CARTESIAN_POINT('Ctrl Pts',(5.75591387021709,-0.0585161493539971,
3.39701858211462));
#60729=CARTESIAN_POINT('Ctrl Pts',(3.12646479860794,-4.83313420866293,3.24002008877257));
#60730=CARTESIAN_POINT('Ctrl Pts',(-2.30646165956461,-5.27391724713939,
3.08302159543051));
#60731=CARTESIAN_POINT('Ctrl Pts',(-5.67120141188825,-0.985618387830106,
2.92602310208845));
#60732=CARTESIAN_POINT('Ctrl Pts',(-3.95061740713414,4.18647699637109,2.76902460874639));
#60733=CARTESIAN_POINT('Ctrl Pts',(1.31245513614984,5.60459010746491,2.61202611540434));
#60734=CARTESIAN_POINT('Ctrl Pts',(5.39865967966489,1.99710927213052,2.45502762206228));
#60735=CARTESIAN_POINT('Ctrl Pts',(4.64392553979592,-3.4011639879985,2.29802912872022));
#60736=CARTESIAN_POINT('Ctrl Pts',(-0.274979314205441,-5.74963991794669,
2.14103063537816));
#60737=CARTESIAN_POINT('Ctrl Pts',(-4.94731676851826,-2.94245551640673,
1.9840321420361));
#60738=CARTESIAN_POINT('Ctrl Pts',(-5.18342394835182,2.50320364708249,1.82703364869405));
#60739=CARTESIAN_POINT('Ctrl Pts',(-0.771610415313318,5.70426458692177,
1.67003515535199));
#60740=CARTESIAN_POINT('Ctrl Pts',(4.33213201561917,3.79034363872074,1.51303666200993));
#60741=CARTESIAN_POINT('Ctrl Pts',(5.55122356888078,-1.52232916811941,1.35603816866787));
#60742=CARTESIAN_POINT('Ctrl Pts',(1.79269130257332,-5.46998065428583,1.19903967532582));
#60743=CARTESIAN_POINT('Ctrl Pts',(-3.57355736700018,-4.5126653679007,1.04204118198376));
#60744=CARTESIAN_POINT('Ctrl Pts',(-5.73499497787591,0.490976502422684,
0.885042688641701));
#60745=CARTESIAN_POINT('Ctrl Pts',(-2.75472917190912,5.05464448619777,0.728044195299644));
#60746=CARTESIAN_POINT('Ctrl Pts',(2.6972617242226,5.08531140785296,0.571045701957586));
#60747=CARTESIAN_POINT('Ctrl Pts',(5.72760380327789,0.557054334442611,0.414047208615528));
#60748=CARTESIAN_POINT('Ctrl Pts',(3.62789159583729,-4.47271039022441,0.25704871527347));
#60749=CARTESIAN_POINT('Ctrl Pts',(-1.7363413051643,-5.48787504144657,0.100050221931414));
#60750=CARTESIAN_POINT('Ctrl Pts',(-4.88928570386961,-2.24027593839366,
-0.0307818558536355));
#60751=CARTESIAN_POINT('Ctrl Pts',(-4.96563797731115,1.08580433615736,-0.135447518081672));
#60752=CARTESIAN_POINT('Ctrl Pts',(-4.2377115180993,2.56580265793949,-0.187780349195693));
#60753=CARTESIAN_POINT('Ctrl Pts',(-3.71544298812226,3.17665283523778,-0.213946764752702));
#60754=CARTESIAN_POINT('Ctrl Pts',(-1.21713437249827,-4.54280821229861,
8.21394676475271));
#60755=CARTESIAN_POINT('Ctrl Pts',(-1.96401037376809,-4.34270105156078,
8.1877803491957));
#60756=CARTESIAN_POINT('Ctrl Pts',(-3.34729239311329,-3.56520741493521,
8.13544751808168));
#60757=CARTESIAN_POINT('Ctrl Pts',(-5.097916388523,-0.88550944272982,8.03078185585364));
#60758=CARTESIAN_POINT('Ctrl Pts',(-4.36556770778803,3.40726768821492,7.89994977806859));
#60759=CARTESIAN_POINT('Ctrl Pts',(0.441936745916073,5.52311682288307,7.74295128472654));
#60760=CARTESIAN_POINT('Ctrl Pts',(4.84625712436104,2.6770749043732,7.58595279138447));
#60761=CARTESIAN_POINT('Ctrl Pts',(4.90852145070782,-2.56470983716281,7.42895429804242));
#60762=CARTESIAN_POINT('Ctrl Pts',(0.567509061050049,-5.50921308252134,
7.27195580470035));
#60763=CARTESIAN_POINT('Ctrl Pts',(-4.28142481930937,-3.51235812547142,
7.11495731135831));
#60764=CARTESIAN_POINT('Ctrl Pts',(-5.29173734849243,1.63333062780086,6.95795881801624));
#60765=CARTESIAN_POINT('Ctrl Pts',(-1.55672827609878,5.31477393079903,6.80096032467419));
#60766=CARTESIAN_POINT('Ctrl Pts',(3.57405151254677,4.23031717978746,6.64396183133213));
#60767=CARTESIAN_POINT('Ctrl Pts',(5.50007700619551,-0.647338110797742,
6.48696333799007));
#60768=CARTESIAN_POINT('Ctrl Pts',(2.49418799724395,-4.94457970738323,6.32996484464802));
#60769=CARTESIAN_POINT('Ctrl Pts',(-2.74820137848241,-4.80802812396074,
6.17296635130595));
#60770=CARTESIAN_POINT('Ctrl Pts',(-5.52630929765102,-0.360167388329068,
6.0159678579639));
#60771=CARTESIAN_POINT('Ctrl Pts',(-3.34901207878694,4.41065973951134,5.85896936462184));
#60772=CARTESIAN_POINT('Ctrl Pts',(1.83131632235576,5.22647785209851,5.70197087127978));
#60773=CARTESIAN_POINT('Ctrl Pts',(5.36951859041486,1.35575454917273,5.54497237793772));
#60774=CARTESIAN_POINT('Ctrl Pts',(4.09291324811456,-3.73066463705719,5.38797388459567));
#60775=CARTESIAN_POINT('Ctrl Pts',(-0.853776186777843,-5.47182442937275,
5.23097539125361));
#60776=CARTESIAN_POINT('Ctrl Pts',(-5.03489114715202,-2.30644074453902,
5.07397689791155));
#60777=CARTESIAN_POINT('Ctrl Pts',(-4.70125703915474,2.92711112192079,4.91697840456949));
#60778=CARTESIAN_POINT('Ctrl Pts',(-0.1520412131545,5.53594442208755,4.75997991122743));
#60779=CARTESIAN_POINT('Ctrl Pts',(4.53350885163308,3.18073809941233,4.60298141788538));
#60780=CARTESIAN_POINT('Ctrl Pts',(5.15389566552312,-2.02661213646347,4.44598292454332));
#60781=CARTESIAN_POINT('Ctrl Pts',(1.15282306767785,-5.41671452552386,4.28898443120126));
#60782=CARTESIAN_POINT('Ctrl Pts',(-3.88197729385743,-3.94968980936076,
4.13198593785921));
#60783=CARTESIAN_POINT('Ctrl Pts',(-5.43583785855895,1.05899200924751,3.97498744451714));
#60784=CARTESIAN_POINT('Ctrl Pts',(-2.11542356142786,5.11808366795104,3.81798895117509));
#60785=CARTESIAN_POINT('Ctrl Pts',(3.1018751019502,4.58782825906337,3.66099045783304));
#60786=CARTESIAN_POINT('Ctrl Pts',(5.53774573975908,-0.0562981941875292,
3.50399196449097));
#60787=CARTESIAN_POINT('Ctrl Pts',(3.00796146526509,-4.64994247259256,3.34699347114892));
#60788=CARTESIAN_POINT('Ctrl Pts',(-2.21903915123905,-5.07401837930674,
3.18999497780685));
#60789=CARTESIAN_POINT('Ctrl Pts',(-5.45624416315586,-0.948260198345973,
3.03299648446481));
#60790=CARTESIAN_POINT('Ctrl Pts',(-3.80087597018717,4.0277957026447,2.87599799112274));
#60791=CARTESIAN_POINT('Ctrl Pts',(1.26270875532829,5.39215764699048,2.71899949778069));
#60792=CARTESIAN_POINT('Ctrl Pts',(5.19403266198385,1.92141224016561,2.56200100443863));
#60793=CARTESIAN_POINT('Ctrl Pts',(4.46790543667278,-3.27224864885797,2.40500251109657));
#60794=CARTESIAN_POINT('Ctrl Pts',(-0.264556690752847,-5.53170959098406,
2.24800401775451));
#60795=CARTESIAN_POINT('Ctrl Pts',(-4.75979713662174,-2.83092674209829,
2.09100552441246));
#60796=CARTESIAN_POINT('Ctrl Pts',(-4.9869550751752,2.40832396817252,1.9340070310704));
#60797=CARTESIAN_POINT('Ctrl Pts',(-0.742363834223583,5.48805413474563,
1.77700853772834));
#60798=CARTESIAN_POINT('Ctrl Pts',(4.16792991599511,3.64667710650734,1.62001004438628));
#60799=CARTESIAN_POINT('Ctrl Pts',(5.3408138763307,-1.4646278688924,1.46301155104423));
#60800=CARTESIAN_POINT('Ctrl Pts',(1.7247423862432,-5.26265033630419,1.30601305770217));
#60801=CARTESIAN_POINT('Ctrl Pts',(-3.43810774988952,-4.34162045845692,
1.14901456436011));
#60802=CARTESIAN_POINT('Ctrl Pts',(-5.51761974247093,0.472366872736146,
0.992016071018053));
#60803=CARTESIAN_POINT('Ctrl Pts',(-2.65031584556259,4.86305677961485,0.835017577675994));
#60804=CARTESIAN_POINT('Ctrl Pts',(2.59502660378856,4.89256132373709,0.678019084333937));
#60805=CARTESIAN_POINT('Ctrl Pts',(5.51050871778138,0.535940136862668,0.521020590991879));
#60806=CARTESIAN_POINT('Ctrl Pts',(3.49038253214829,-4.30317990628779,0.364022097649821));
#60807=CARTESIAN_POINT('Ctrl Pts',(-1.67052823969354,-5.27986646713926,
0.207023604307765));
#60808=CARTESIAN_POINT('Ctrl Pts',(-4.70396564082841,-2.15536208731635,
0.0761915265227156));
#60809=CARTESIAN_POINT('Ctrl Pts',(-4.77742391114056,1.04464876861345,-0.0284741357053212));
#60810=CARTESIAN_POINT('Ctrl Pts',(-4.07708826692317,2.46855026993846,-0.0808069668193416));
#60811=CARTESIAN_POINT('Ctrl Pts',(-3.57461543774208,3.05624720968387,-0.106973382376351));
#60812=CARTESIAN_POINT('Ctrl Pts',(-1.16918346556918,-4.3638371975063,8.32092014712906));
#60813=CARTESIAN_POINT('Ctrl Pts',(-1.886635121891,-4.17161357046631,8.29475373157205));
#60814=CARTESIAN_POINT('Ctrl Pts',(-3.21542058862456,-3.4247505082869,8.24242090045803));
#60815=CARTESIAN_POINT('Ctrl Pts',(-4.89707602134433,-0.850623417133479,
8.13775523822999));
#60816=CARTESIAN_POINT('Ctrl Pts',(-4.19357935910711,3.27303306343417,8.00692316044493));
#60817=CARTESIAN_POINT('Ctrl Pts',(0.424525958536476,5.30552502142163,7.84992466710289));
#60818=CARTESIAN_POINT('Ctrl Pts',(4.65533126639873,2.5716073631696,7.69292617376082));
#60819=CARTESIAN_POINT('Ctrl Pts',(4.71514259249745,-2.46366909303406,7.53592768041877));
#60820=CARTESIAN_POINT('Ctrl Pts',(0.545151156464739,-5.29216904059666,
7.3789291870767));
#60821=CARTESIAN_POINT('Ctrl Pts',(-4.11275141095498,-3.37398329900883,
7.22193069373466));
#60822=CARTESIAN_POINT('Ctrl Pts',(-5.08326110229957,1.56898302026649,7.06493220039259));
#60823=CARTESIAN_POINT('Ctrl Pts',(-1.4953985376839,5.10539012251682,6.90793370705054));
#60824=CARTESIAN_POINT('Ctrl Pts',(3.4332461788792,4.06365723660293,6.75093521370847));
#60825=CARTESIAN_POINT('Ctrl Pts',(5.28339289424692,-0.621835216290863,
6.59393672036643));
#60826=CARTESIAN_POINT('Ctrl Pts',(2.3959255709894,-4.74978027791225,6.43693822702436));
#60827=CARTESIAN_POINT('Ctrl Pts',(-2.63993169889764,-4.61860835709371,
6.27993973368231));
#60828=CARTESIAN_POINT('Ctrl Pts',(-5.3085917236669,-0.345978032324596,
6.12294124034025));
#60829=CARTESIAN_POINT('Ctrl Pts',(-3.21707252459896,4.23689491991211,5.96594274699819));
#60830=CARTESIAN_POINT('Ctrl Pts',(1.75916875959262,5.0205726055492,5.80894425365613));
#60831=CARTESIAN_POINT('Ctrl Pts',(5.15797803088363,1.30234248418222,5.65194576031408));
#60832=CARTESIAN_POINT('Ctrl Pts',(3.93166654712268,-3.58368928508518,5.49494726697202));
#60833=CARTESIAN_POINT('Ctrl Pts',(-0.820140342293046,-5.25625337175271,
5.33794877362996));
#60834=CARTESIAN_POINT('Ctrl Pts',(-4.83653375765556,-2.215574914128,5.1809502802879));
#60835=CARTESIAN_POINT('Ctrl Pts',(-4.516043685701,2.81179301395361,5.02395178694585));
#60836=CARTESIAN_POINT('Ctrl Pts',(-0.14605131242859,5.31784725734868,4.86695329360378));
#60837=CARTESIAN_POINT('Ctrl Pts',(4.3549041996581,3.0554279610932,4.70995480026174));
#60838=CARTESIAN_POINT('Ctrl Pts',(4.95084990741799,-1.94677059050708,4.55295630691967));
#60839=CARTESIAN_POINT('Ctrl Pts',(1.1074058049064,-5.20331460851906,4.39595781357761));
#60840=CARTESIAN_POINT('Ctrl Pts',(-3.7290407437734,-3.79408561911948,4.23895932023556));
#60841=CARTESIAN_POINT('Ctrl Pts',(-5.22168454802319,1.01727136736814,4.08196082689349));
#60842=CARTESIAN_POINT('Ctrl Pts',(-2.03208315086874,4.91644877934506,3.92496233355144));
#60843=CARTESIAN_POINT('Ctrl Pts',(2.97967189441612,4.40708360931248,3.76796384020938));
#60844=CARTESIAN_POINT('Ctrl Pts',(5.31957760930108,-0.0540802390210696,
3.61096534686732));
#60845=CARTESIAN_POINT('Ctrl Pts',(2.88945813192224,-4.46675073652217,3.45396685352527));
#60846=CARTESIAN_POINT('Ctrl Pts',(-2.13161664291348,-4.87411951147409,
3.29696836018321));
#60847=CARTESIAN_POINT('Ctrl Pts',(-5.24128691442347,-0.910902008861835,
3.13996986684115));
#60848=CARTESIAN_POINT('Ctrl Pts',(-3.6511345332402,3.86911440891831,2.9829713734991));
#60849=CARTESIAN_POINT('Ctrl Pts',(1.21296237450675,5.17972518651607,2.82597288015703));
#60850=CARTESIAN_POINT('Ctrl Pts',(4.98940564430279,1.8457152082007,2.66897438681498));
#60851=CARTESIAN_POINT('Ctrl Pts',(4.29188533354966,-3.14333330971743,2.51197589347292));
#60852=CARTESIAN_POINT('Ctrl Pts',(-0.254134067300259,-5.31377926402143,
2.35497740013087));
#60853=CARTESIAN_POINT('Ctrl Pts',(-4.57227750472522,-2.71939796778984,
2.1979789067888));
#60854=CARTESIAN_POINT('Ctrl Pts',(-4.79048620199859,2.31344428926255,2.04098041344675));
#60855=CARTESIAN_POINT('Ctrl Pts',(-0.713117253133846,5.27184368256949,
1.88398192010469));
#60856=CARTESIAN_POINT('Ctrl Pts',(4.00372781637104,3.50301057429394,1.72698342676264));
#60857=CARTESIAN_POINT('Ctrl Pts',(5.13040418378061,-1.40692656966539,1.56998493342058));
#60858=CARTESIAN_POINT('Ctrl Pts',(1.65679346991308,-5.05532001832255,1.41298644007852));
#60859=CARTESIAN_POINT('Ctrl Pts',(-3.30265813277885,-4.17057554901314,
1.25598794673646));
#60860=CARTESIAN_POINT('Ctrl Pts',(-5.30024450706594,0.453757243049607,
1.0989894533944));
#60861=CARTESIAN_POINT('Ctrl Pts',(-2.54590251921605,4.67146907303194,0.941990960052346));
#60862=CARTESIAN_POINT('Ctrl Pts',(2.49279148335452,4.69981123962122,0.784992466710289));
#60863=CARTESIAN_POINT('Ctrl Pts',(5.29341363228488,0.514825939282724,0.62799397336823));
#60864=CARTESIAN_POINT('Ctrl Pts',(3.35287346845927,-4.13364942235117,0.470995480026172));
#60865=CARTESIAN_POINT('Ctrl Pts',(-1.60471517422276,-5.07185789283195,
0.313996986684116));
#60866=CARTESIAN_POINT('Ctrl Pts',(-4.51864557778723,-2.07044823623904,
0.183164908899067));
#60867=CARTESIAN_POINT('Ctrl Pts',(-4.58920984496997,1.00349320106954,0.07849924667103));
#60868=CARTESIAN_POINT('Ctrl Pts',(-3.91646501574703,2.37129788193743,0.0261664155570096));
#60869=CARTESIAN_POINT('Ctrl Pts',(-3.43378788736191,2.93584158412995,0.));
#60870=CARTESIAN_POINT('Ctrl Pts',(-3.43378788736191,2.93584158412995,0.));
#60871=CARTESIAN_POINT('Ctrl Pts',(-3.52723777670969,2.83914483717434,2.20957577510153E-16));
#60872=CARTESIAN_POINT('Ctrl Pts',(-3.61593961326928,2.73846171784274,-1.95102593779902E-16));
#60873=CARTESIAN_POINT('Ctrl Pts',(-3.69983889649088,2.63418997519716,-5.55111512312578E-17));
#60874=CARTESIAN_POINT('Ctrl Pts',(-3.78516004991503,2.5281511032253,8.64459958272222E-17));
#60875=CARTESIAN_POINT('Ctrl Pts',(-3.86551489177621,2.41840048478536,3.57207213678775E-15));
#60876=CARTESIAN_POINT('Ctrl Pts',(-3.9408148769991,2.30531248881791,3.33066907387547E-15));
#60877=CARTESIAN_POINT('Ctrl Pts',(-4.01713525064214,2.19069203993958,3.08599476344226E-15));
#60878=CARTESIAN_POINT('Ctrl Pts',(-4.08826327828892,2.07264261686327,1.15541512747695E-15));
#60879=CARTESIAN_POINT('Ctrl Pts',(-4.15406859699169,1.95151684254046,1.38777878078145E-15));
#60880=CARTESIAN_POINT('Ctrl Pts',(-4.21980984783224,1.8305089959106,1.61991620552547E-15));
#60881=CARTESIAN_POINT('Ctrl Pts',(-4.28023911511666,1.70643015108279,2.039107624704E-15));
#60882=CARTESIAN_POINT('Ctrl Pts',(-4.33518267922297,1.57960398874639,2.4980018054066E-15));
#60883=CARTESIAN_POINT('Ctrl Pts',(-4.35306946209471,1.53831594955441,2.64739401730341E-15));
#60884=CARTESIAN_POINT('Ctrl Pts',(-4.37037449182742,1.49673656482301,-1.24977233183131E-15));
#60885=CARTESIAN_POINT('Ctrl Pts',(-4.38709067099901,1.45487653718474,-1.55431223447522E-15));
#60886=CARTESIAN_POINT('Ctrl Pts',(-4.39375920070266,1.43817745572383,-1.67580132393046E-15));
#60887=CARTESIAN_POINT('Ctrl Pts',(-4.40033069663165,1.42144199284245,2.13318250051857E-15));
#60888=CARTESIAN_POINT('Ctrl Pts',(-4.40680423707264,1.40467289792598,2.1094237467878E-15));
#60889=CARTESIAN_POINT('Ctrl Pts',(-4.45933329243635,1.26860134275516,1.91663513266347E-15));
#60890=CARTESIAN_POINT('Ctrl Pts',(-4.50543275765374,1.13027759164836,2.92434253228364E-15));
#60891=CARTESIAN_POINT('Ctrl Pts',(-4.54499128400339,0.990129694249863,
2.63677968348475E-15));
#60892=CARTESIAN_POINT('Ctrl Pts',(-4.58298351161253,0.855530878059325,
2.35904680574097E-15));
#60893=CARTESIAN_POINT('Ctrl Pts',(-4.61494272389214,0.719248781594657,
4.48491542532579E-15));
#60894=CARTESIAN_POINT('Ctrl Pts',(-4.64084676847695,0.58176526830246,3.3584246494911E-15));
#60895=CARTESIAN_POINT('Ctrl Pts',(-4.66691254514768,0.44342337572085,2.22490062051545E-15));
#60896=CARTESIAN_POINT('Ctrl Pts',(-4.68684755285248,0.303864196021266,
1.79312284184644E-16));
#60897=CARTESIAN_POINT('Ctrl Pts',(-4.70058040711193,0.163559265384357,
-6.66133814775094E-16));
#60898=CARTESIAN_POINT('Ctrl Pts',(-4.71271438319262,0.0395896491496948,
-1.41314696648225E-15));
#60899=CARTESIAN_POINT('Ctrl Pts',(-4.72000573130037,-0.0849628385647041,
1.44014651394631E-16));
#60900=CARTESIAN_POINT('Ctrl Pts',(-4.7223714742082,-0.209777558646538,
-3.88578058618805E-16));
#60901=CARTESIAN_POINT('Ctrl Pts',(-4.72292774412613,-0.239125918464476,
-5.13809461450429E-16));
#60902=CARTESIAN_POINT('Ctrl Pts',(-4.72321154151185,-0.268488777105225,
3.0010215925102E-15));
#60903=CARTESIAN_POINT('Ctrl Pts',(-4.72322152198113,-0.297861955465308,
2.91433543964104E-15));
#60904=CARTESIAN_POINT('Ctrl Pts',(-4.72322914092456,-0.320285007726138,
2.84816050575247E-15));
#60905=CARTESIAN_POINT('Ctrl Pts',(-4.72307708136321,-0.342716335801155,
3.67219762837691E-17));
#60906=CARTESIAN_POINT('Ctrl Pts',(-4.72276525050185,-0.365131269043745,
1.38777878078145E-16));
#60907=CARTESIAN_POINT('Ctrl Pts',(-4.72077152616445,-0.508443568958217,
7.91283323787342E-16));
#60908=CARTESIAN_POINT('Ctrl Pts',(-4.71225224775121,-0.651283769357607,
4.69641391259678E-15));
#60909=CARTESIAN_POINT('Ctrl Pts',(-4.69718724960338,-0.793159785562181,
4.52415882534751E-15));
#60910=CARTESIAN_POINT('Ctrl Pts',(-4.68213033873543,-0.934959639059055,
4.35199620907545E-15));
#60911=CARTESIAN_POINT('Ctrl Pts',(-4.66053490666648,-1.07579720961356,
2.29755459169068E-15));
#60912=CARTESIAN_POINT('Ctrl Pts',(-4.63233047059339,-1.21519245994795,
1.88737914186277E-15));
#60913=CARTESIAN_POINT('Ctrl Pts',(-4.62518265294206,-1.25051923720629,
1.78342885146082E-15));
#60914=CARTESIAN_POINT('Ctrl Pts',(-4.61761010448178,-1.28575339934606,
3.86113148383421E-16));
#60915=CARTESIAN_POINT('Ctrl Pts',(-4.60961114292865,-1.32088714489269,
2.22044604925031E-16));
#60916=CARTESIAN_POINT('Ctrl Pts',(-4.57836306126197,-1.45813772958496,
-4.20462921062943E-16));
#60917=CARTESIAN_POINT('Ctrl Pts',(-4.54061164386395,-1.59385666227503,
-3.37562086541692E-16));
#60918=CARTESIAN_POINT('Ctrl Pts',(-4.49667838831439,-1.72776655308613,
-8.04911692853238E-16));
#60919=CARTESIAN_POINT('Ctrl Pts',(-4.46792839524171,-1.81539740094895,
-1.11074602668306E-15));
#60920=CARTESIAN_POINT('Ctrl Pts',(-4.43652997184098,-1.90225339638272,
9.54490265544014E-16));
#60921=CARTESIAN_POINT('Ctrl Pts',(-4.40256174565587,-1.98825353803286,
7.21644966006352E-16));
#60922=CARTESIAN_POINT('Ctrl Pts',(-4.39065014752274,-2.01841110708421,
6.3999337724903E-16));
#60923=CARTESIAN_POINT('Ctrl Pts',(-4.37842246733328,-2.04846340327406,
1.30054899424822E-15));
#60924=CARTESIAN_POINT('Ctrl Pts',(-4.3658818524655,-2.07840682871088,1.27675647831893E-15));
#60925=CARTESIAN_POINT('Ctrl Pts',(-4.35886905063707,-2.09515140709612,
1.26345153267066E-15));
#60926=CARTESIAN_POINT('Ctrl Pts',(-4.35175838797214,-2.11186193915223,
-4.29181623021427E-15));
#60927=CARTESIAN_POINT('Ctrl Pts',(-4.34455039841696,-2.12853778716716,
-4.44089209850063E-15));
#60928=CARTESIAN_POINT('Ctrl Pts',(-4.33665307152192,-2.14680843281913,
-4.60422486348398E-15));
#60929=CARTESIAN_POINT('Ctrl Pts',(-4.3286424353965,-2.16502924396809,5.30168465333661E-15));
#60930=CARTESIAN_POINT('Ctrl Pts',(-4.32052144132994,-2.18319526042712,
5.16253706450698E-15));
#60931=CARTESIAN_POINT('Ctrl Pts',(-4.26272706163057,-2.31247668142725,
4.17227053836974E-15));
#60932=CARTESIAN_POINT('Ctrl Pts',(-4.19931793630604,-2.4390523089761,-3.17224447424671E-16));
#60933=CARTESIAN_POINT('Ctrl Pts',(-4.1306671181063,-2.56266098762457,-5.55111512312578E-17));
#60934=CARTESIAN_POINT('Ctrl Pts',(-4.0593379123478,-2.69109221545352,2.16412797287518E-16));
#60935=CARTESIAN_POINT('Ctrl Pts',(-3.9823498940757,-2.81632115639891,3.16344549884833E-15));
#60936=CARTESIAN_POINT('Ctrl Pts',(-3.90006549167258,-2.93804355166681,
2.74780198594726E-15));
#60937=CARTESIAN_POINT('Ctrl Pts',(-3.81789453604086,-3.05959812639587,
2.33273152715138E-15));
#60938=CARTESIAN_POINT('Ctrl Pts',(-3.73044127702168,-3.17765647132671,
1.52792430062925E-15));
#60939=CARTESIAN_POINT('Ctrl Pts',(-3.63801734753769,-3.29189441139934,
2.04003480774873E-15));
#60940=CARTESIAN_POINT('Ctrl Pts',(-3.56858774848175,-3.37771087062696,
2.42473633883647E-15));
#60941=CARTESIAN_POINT('Ctrl Pts',(-3.49635207705255,-3.46137105631218,
2.6380387160668E-15));
#60942=CARTESIAN_POINT('Ctrl Pts',(-3.42142672585507,-3.54272626619495,
2.95596880306448E-15));
#60943=CARTESIAN_POINT('Ctrl Pts',(-3.38629422705786,-3.58087372586878,
3.10504622773483E-15));
#60944=CARTESIAN_POINT('Ctrl Pts',(-3.3505701767281,-3.61851424013804,2.76570113010457E-15));
#60945=CARTESIAN_POINT('Ctrl Pts',(-3.31426568073248,-3.6556315716941,2.76167977375508E-15));
#60946=CARTESIAN_POINT('Ctrl Pts',(-3.29921135129803,-3.67102295839838,
2.76001224411176E-15));
#60947=CARTESIAN_POINT('Ctrl Pts',(-3.2840555690535,-3.68632600746954,3.617329513469E-16));
#60948=CARTESIAN_POINT('Ctrl Pts',(-3.26880440302003,-3.70153424964867,
5.13478148889135E-16));
#60949=CARTESIAN_POINT('Ctrl Pts',(-3.16314622619418,-3.8068950553632,1.56474995848081E-15));
#60950=CARTESIAN_POINT('Ctrl Pts',(-3.05312027550677,-3.90750387615403,
1.50739186887073E-15));
#60951=CARTESIAN_POINT('Ctrl Pts',(-2.93906465882528,-4.00303742675364,
1.35308431126191E-15));
#60952=CARTESIAN_POINT('Ctrl Pts',(-2.83344548104308,-4.09150457426047,
1.21019053860593E-15));
#60953=CARTESIAN_POINT('Ctrl Pts',(-2.72436990580127,-4.17561968062982,
2.13759783489021E-15));
#60954=CARTESIAN_POINT('Ctrl Pts',(-2.61207533410326,-4.25510133080791,
2.0122792321331E-15));
#60955=CARTESIAN_POINT('Ctrl Pts',(-2.56057702495619,-4.29155162872077,
1.95480810018898E-15));
#60956=CARTESIAN_POINT('Ctrl Pts',(-2.50840133628958,-4.32702707245024,
2.36751160669112E-15));
#60957=CARTESIAN_POINT('Ctrl Pts',(-2.45556938566372,-4.36149843071932,
2.75474087985117E-15));
#60958=CARTESIAN_POINT('Ctrl Pts',(-2.42827777589571,-4.37930543664865,
2.95477343758642E-15));
#60959=CARTESIAN_POINT('Ctrl Pts',(-2.40081102655259,-4.39684448061502,
1.19861602340893E-15));
#60960=CARTESIAN_POINT('Ctrl Pts',(-2.3731719452944,-4.41411137781326,1.24206200879939E-15));
#60961=CARTESIAN_POINT('Ctrl Pts',(-2.35240993886931,-4.42708197648195,
1.27469789200386E-15));
#60962=CARTESIAN_POINT('Ctrl Pts',(-2.3315588675056,-4.43989388919032,-2.42681870829991E-15));
#60963=CARTESIAN_POINT('Ctrl Pts',(-2.310621268056,-4.45254499954709,-2.38004060904018E-15));
#60964=CARTESIAN_POINT('Ctrl Pts',(-2.18359867883944,-4.52929576545271,
-2.09625089852901E-15));
#60965=CARTESIAN_POINT('Ctrl Pts',(-2.0533809663479,-4.60013945799199,1.86447051626453E-17));
#60966=CARTESIAN_POINT('Ctrl Pts',(-1.92026980955225,-4.66473533433833,
-1.2490009027033E-16));
#60967=CARTESIAN_POINT('Ctrl Pts',(-1.7911873441691,-4.72737617657195,-2.64100413770296E-16));
#60968=CARTESIAN_POINT('Ctrl Pts',(-1.65938332691157,-4.78414205363558,
1.04097051092433E-15));
#60969=CARTESIAN_POINT('Ctrl Pts',(-1.52510574125302,-4.83468405991464,
1.71217207078911E-15));
#60970=CARTESIAN_POINT('Ctrl Pts',(-1.45664804130053,-4.8604514989394,2.07094871730909E-15));
#60971=CARTESIAN_POINT('Ctrl Pts',(-1.38754702424773,-4.88460057019718,
-4.86141022577448E-16));
#60972=CARTESIAN_POINT('Ctrl Pts',(-1.31785621200041,-4.90714516622019,
-4.9960036108132E-16));
#60973=CARTESIAN_POINT('Ctrl Pts',(-4.51483246697105,0.00361950456559231,
7.11258330249198));
#60974=CARTESIAN_POINT('Ctrl Pts',(-4.5183463327351,0.455094042321683,7.09669960179219));
#60975=CARTESIAN_POINT('Ctrl Pts',(-4.45593254783999,0.905622974345749,
7.08081590109239));
#60976=CARTESIAN_POINT('Ctrl Pts',(-4.32353239297286,1.33455648409566,7.0649322003926));
#60977=CARTESIAN_POINT('Ctrl Pts',(-3.88730691409435,2.74778538768327,7.01259936927858));
#60978=CARTESIAN_POINT('Ctrl Pts',(-2.69135272588913,3.92658775510004,6.96026653816456));
#60979=CARTESIAN_POINT('Ctrl Pts',(-1.27193484569267,4.34236679115612,6.90793370705054));
#60980=CARTESIAN_POINT('Ctrl Pts',(0.147483034503799,4.75814582721219,6.85560087593652));
#60981=CARTESIAN_POINT('Ctrl Pts',(1.7903646066915,4.41090153190756,6.8032680448225));
#60982=CARTESIAN_POINT('Ctrl Pts',(2.92016317867997,3.45636397543961,6.75093521370848));
#60983=CARTESIAN_POINT('Ctrl Pts',(4.04996175066844,2.50182641897166,6.69860238259446));
#60984=CARTESIAN_POINT('Ctrl Pts',(4.66667732245768,0.939995601340394,6.64626955148044));
#60985=CARTESIAN_POINT('Ctrl Pts',(4.49379055447605,-0.528910651078803,
6.59393672036643));
#60986=CARTESIAN_POINT('Ctrl Pts',(4.32090378649441,-1.997816903498,6.54160388925241));
#60987=CARTESIAN_POINT('Ctrl Pts',(3.35841467874189,-3.37379859070514,6.48927105813838));
#60988=CARTESIAN_POINT('Ctrl Pts',(2.03786057988447,-4.03992744750561,6.43693822702436));
#60989=CARTESIAN_POINT('Ctrl Pts',(0.717306481027035,-4.70605630430607,
6.38460539591034));
#60990=CARTESIAN_POINT('Ctrl Pts',(-0.961312608935302,-4.66233233069989,
6.33227256479632));
#60991=CARTESIAN_POINT('Ctrl Pts',(-2.24539882471135,-3.92836528976861,
6.27993973368231));
#60992=CARTESIAN_POINT('Ctrl Pts',(-3.5294850404874,-3.19439824883733,6.22760690256829));
#60993=CARTESIAN_POINT('Ctrl Pts',(-4.41903838207715,-1.77018814058096,
6.17527407145427));
#60994=CARTESIAN_POINT('Ctrl Pts',(-4.51522851969403,-0.294270927746662,
6.12294124034025));
#60995=CARTESIAN_POINT('Ctrl Pts',(-4.52157464089458,-0.196897644511263,
6.11948859439083));
#60996=CARTESIAN_POINT('Ctrl Pts',(-4.52446751475242,-0.0992992973699645,
6.1160359484414));
#60997=CARTESIAN_POINT('Ctrl Pts',(-4.52399690261043,-0.00167256832429505,
6.11258330249198));
#60998=CARTESIAN_POINT('Ctrl Pts',(-1.31303618635644,-4.90075024188323,
8.));
#60999=CARTESIAN_POINT('Ctrl Pts',(-1.45239709211802,-4.85517655769009,
8.));
#61000=CARTESIAN_POINT('Ctrl Pts',(-1.58927461952972,-4.80351078633936,
8.));
#61001=CARTESIAN_POINT('Ctrl Pts',(-1.72340721958534,-4.74604566824414,
8.));
#61002=CARTESIAN_POINT('Ctrl Pts',(-1.85924970425712,-4.68784800100459,
8.));
#61003=CARTESIAN_POINT('Ctrl Pts',(-1.99227741877149,-4.62370180241543,
8.));
#61004=CARTESIAN_POINT('Ctrl Pts',(-2.1221970609313,-4.55386234778148,8.));
#61005=CARTESIAN_POINT('Ctrl Pts',(-2.25246970806005,-4.48383313219911,
8.));
#61006=CARTESIAN_POINT('Ctrl Pts',(-2.37961793682551,-4.40807921917534,
8.));
#61007=CARTESIAN_POINT('Ctrl Pts',(-2.50331578855033,-4.32681572428032,
8.));
#61008=CARTESIAN_POINT('Ctrl Pts',(-2.62609342189428,-4.24615676827303,
8.));
#61009=CARTESIAN_POINT('Ctrl Pts',(-2.74547232113475,-4.16006940168606,
8.));
#61010=CARTESIAN_POINT('Ctrl Pts',(-2.86109611850811,-4.06872967104376,
8.));
#61011=CARTESIAN_POINT('Ctrl Pts',(-2.9021226048247,-4.0363198359191,8.));
#61012=CARTESIAN_POINT('Ctrl Pts',(-2.94267593191283,-4.00324843420239,
8.));
#61013=CARTESIAN_POINT('Ctrl Pts',(-2.98273884627905,-3.96952246026761,
8.));
#61014=CARTESIAN_POINT('Ctrl Pts',(-2.99980179304064,-3.95515844040447,
8.));
#61015=CARTESIAN_POINT('Ctrl Pts',(-3.01677686159523,-3.94067464141144,
8.));
#61016=CARTESIAN_POINT('Ctrl Pts',(-3.03364692784275,-3.92608549145045,
8.));
#61017=CARTESIAN_POINT('Ctrl Pts',(-3.14433906287484,-3.83035947983968,
8.));
#61018=CARTESIAN_POINT('Ctrl Pts',(-3.25067173076357,-3.72996938710921,
8.));
#61019=CARTESIAN_POINT('Ctrl Pts',(-3.35235942406226,-3.62515267891276,
8.));
#61020=CARTESIAN_POINT('Ctrl Pts',(-3.36192701172294,-3.61529068862227,
8.));
#61021=CARTESIAN_POINT('Ctrl Pts',(-3.37145345441303,-3.60538948288356,
8.));
#61022=CARTESIAN_POINT('Ctrl Pts',(-3.38093849819353,-3.5954492420827,8.));
#61023=CARTESIAN_POINT('Ctrl Pts',(-3.48179697338609,-3.48975046478426,
8.));
#61024=CARTESIAN_POINT('Ctrl Pts',(-3.57797791034191,-3.37964062514819,
8.));
#61025=CARTESIAN_POINT('Ctrl Pts',(-3.6691784190789,-3.26549870852508,8.));
#61026=CARTESIAN_POINT('Ctrl Pts',(-3.75971104108468,-3.1521926849539,8.));
#61027=CARTESIAN_POINT('Ctrl Pts',(-3.84533634314077,-3.03491270174392,
8.));
#61028=CARTESIAN_POINT('Ctrl Pts',(-3.92571335075401,-2.91400477707446,
8.));
#61029=CARTESIAN_POINT('Ctrl Pts',(-3.99657459670685,-2.80741103289235,
8.));
#61030=CARTESIAN_POINT('Ctrl Pts',(-4.06335624155544,-2.69799686623316,
8.));
#61031=CARTESIAN_POINT('Ctrl Pts',(-4.12579142887319,-2.5859898555039,8.));
#61032=CARTESIAN_POINT('Ctrl Pts',(-4.14218052019666,-2.55658827593677,
8.));
#61033=CARTESIAN_POINT('Ctrl Pts',(-4.15826993976141,-2.52700800600865,
8.));
#61034=CARTESIAN_POINT('Ctrl Pts',(-4.17405446883537,-2.49725311040552,
8.));
#61035=CARTESIAN_POINT('Ctrl Pts',(-4.18546373911311,-2.47574587097943,
8.));
#61036=CARTESIAN_POINT('Ctrl Pts',(-4.19671529109329,-2.45414413479639,
8.));
#61037=CARTESIAN_POINT('Ctrl Pts',(-4.20779517261687,-2.4324732839539,8.));
#61038=CARTESIAN_POINT('Ctrl Pts',(-4.27314976421176,-2.30464794545096,
8.));
#61039=CARTESIAN_POINT('Ctrl Pts',(-4.33262109126524,-2.17426237076666,
8.));
#61040=CARTESIAN_POINT('Ctrl Pts',(-4.38592494350939,-2.0416738299269,8.));
#61041=CARTESIAN_POINT('Ctrl Pts',(-4.43841400089354,-1.91111201805743,
8.));
#61042=CARTESIAN_POINT('Ctrl Pts',(-4.48492299905459,-1.7784133775905,8.));
#61043=CARTESIAN_POINT('Ctrl Pts',(-4.52513335521759,-1.64390172617838,
8.));
#61044=CARTESIAN_POINT('Ctrl Pts',(-4.537048107786,-1.60404450537571,8.));
#61045=CARTESIAN_POINT('Ctrl Pts',(-4.54840950403996,-1.5640280227951,8.));
#61046=CARTESIAN_POINT('Ctrl Pts',(-4.55920838150573,-1.52386053965931,
8.));
#61047=CARTESIAN_POINT('Ctrl Pts',(-4.59649237875198,-1.385179057684,8.));
#61048=CARTESIAN_POINT('Ctrl Pts',(-4.62707496138222,-1.24469748534875,
8.));
#61049=CARTESIAN_POINT('Ctrl Pts',(-4.65105491040296,-1.10285889077504,
8.));
#61050=CARTESIAN_POINT('Ctrl Pts',(-4.66554282028716,-1.017164597826,8.));
#61051=CARTESIAN_POINT('Ctrl Pts',(-4.67761961594462,-0.930974942162248,
8.));
#61052=CARTESIAN_POINT('Ctrl Pts',(-4.68729801221865,-0.844388845291519,
8.));
#61053=CARTESIAN_POINT('Ctrl Pts',(-4.69282817886049,-0.794914166739051,
8.));
#61054=CARTESIAN_POINT('Ctrl Pts',(-4.69757516967293,-0.745310079919106,
8.));
#61055=CARTESIAN_POINT('Ctrl Pts',(-4.70154039472519,-0.695595329877529,
8.));
#61056=CARTESIAN_POINT('Ctrl Pts',(-4.70301053775668,-0.677163136906814,
8.));
#61057=CARTESIAN_POINT('Ctrl Pts',(-4.70437287652954,-0.658719449757616,
8.));
#61058=CARTESIAN_POINT('Ctrl Pts',(-4.70562704431493,-0.64027493011297,
8.));
#61059=CARTESIAN_POINT('Ctrl Pts',(-4.71515809633756,-0.500105745165328,
8.));
#61060=CARTESIAN_POINT('Ctrl Pts',(-4.71845973908213,-0.359723770205855,
8.));
#61061=CARTESIAN_POINT('Ctrl Pts',(-4.71568669686701,-0.219543283976319,
8.));
#61062=CARTESIAN_POINT('Ctrl Pts',(-4.71286811953556,-0.0770609450327588,
8.));
#61063=CARTESIAN_POINT('Ctrl Pts',(-4.70377361453064,0.0652140588645918,
8.));
#61064=CARTESIAN_POINT('Ctrl Pts',(-4.68851230252744,0.206844911988138,
8.));
#61065=CARTESIAN_POINT('Ctrl Pts',(-4.67333458060724,0.347700016947462,
8.));
#61066=CARTESIAN_POINT('Ctrl Pts',(-4.65205714501789,0.487918806531984,
8.));
#61067=CARTESIAN_POINT('Ctrl Pts',(-4.62473814484182,0.627057654071025,
8.));
#61068=CARTESIAN_POINT('Ctrl Pts',(-4.605133388788,0.726906958439074,8.));
#61069=CARTESIAN_POINT('Ctrl Pts',(-4.5824162991499,0.826199852698566,8.));
#61070=CARTESIAN_POINT('Ctrl Pts',(-4.55659376741278,0.92476446952987,8.));
#61071=CARTESIAN_POINT('Ctrl Pts',(-4.54451944953447,0.97085214703918,8.));
#61072=CARTESIAN_POINT('Ctrl Pts',(-4.53176599217756,1.01678048248609,8.));
#61073=CARTESIAN_POINT('Ctrl Pts',(-4.5183332282825,1.06253124418397,8.));
#61074=CARTESIAN_POINT('Ctrl Pts',(-4.51267692512135,1.08179609392292,8.));
#61075=CARTESIAN_POINT('Ctrl Pts',(-4.50690016711964,1.10102945232834,8.));
#61076=CARTESIAN_POINT('Ctrl Pts',(-4.50100291315461,1.12022993263941,8.));
#61077=CARTESIAN_POINT('Ctrl Pts',(-4.49471977615854,1.14068678406554,8.));
#61078=CARTESIAN_POINT('Ctrl Pts',(-4.48830254703555,1.16109751332069,8.));
#61079=CARTESIAN_POINT('Ctrl Pts',(-4.48175248385615,1.18145762320509,8.));
#61080=CARTESIAN_POINT('Ctrl Pts',(-4.43884234970562,1.31483878649018,8.));
#61081=CARTESIAN_POINT('Ctrl Pts',(-4.39022235830023,1.4460911608231,8.));
#61082=CARTESIAN_POINT('Ctrl Pts',(-4.33596033524399,1.57478158992507,8.));
#61083=CARTESIAN_POINT('Ctrl Pts',(-4.28905827705606,1.68601677162324,8.));
#61084=CARTESIAN_POINT('Ctrl Pts',(-4.23794008569217,1.79533788193322,8.));
#61085=CARTESIAN_POINT('Ctrl Pts',(-4.18262262022186,1.90244778297798,8.));
#61086=CARTESIAN_POINT('Ctrl Pts',(-4.15876953368252,1.94863395071215,8.));
#61087=CARTESIAN_POINT('Ctrl Pts',(-4.13413534457581,1.9944087336574,8.));
#61088=CARTESIAN_POINT('Ctrl Pts',(-4.10872005342092,2.03974709902823,8.));
#61089=CARTESIAN_POINT('Ctrl Pts',(-4.09757333138634,2.05963174851782,8.));
#61090=CARTESIAN_POINT('Ctrl Pts',(-4.08627634995272,2.07943244040586,8.));
#61091=CARTESIAN_POINT('Ctrl Pts',(-4.0748290615074,2.09914701235749,8.));
#61092=CARTESIAN_POINT('Ctrl Pts',(-4.06286920268517,2.11974433533126,8.));
#61093=CARTESIAN_POINT('Ctrl Pts',(-4.05074975381766,2.1402399100487,8.));
#61094=CARTESIAN_POINT('Ctrl Pts',(-4.0384724823486,2.16062907002492,8.));
#61095=CARTESIAN_POINT('Ctrl Pts',(-3.96920273979072,2.27566699731059,8.));
#61096=CARTESIAN_POINT('Ctrl Pts',(-3.89489711290362,2.38734570786034,8.));
#61097=CARTESIAN_POINT('Ctrl Pts',(-3.81559004701476,2.49525769668179,8.));
#61098=CARTESIAN_POINT('Ctrl Pts',(-3.739663695997,2.59856959519238,8.));
#61099=CARTESIAN_POINT('Ctrl Pts',(-3.65915281331369,2.69842939750744,8.));
#61100=CARTESIAN_POINT('Ctrl Pts',(-3.57405581868196,2.79444797267076,8.));
#61101=CARTESIAN_POINT('Ctrl Pts',(-3.53072763156913,2.8433370175658,8.));
#61102=CARTESIAN_POINT('Ctrl Pts',(-3.48620998149697,2.89122965827726,8.));
#61103=CARTESIAN_POINT('Ctrl Pts',(-3.44054916109509,2.93810681611542,8.));
#61104=CARTESIAN_POINT('Origin',(-1.11022302462516E-15,0.,8.));
#61105=CARTESIAN_POINT('',(4.90747728811182,-8.5,8.));
#61106=CARTESIAN_POINT('',(9.81495457622364,0.,8.));
#61107=CARTESIAN_POINT('',(4.90747728811182,-8.5,8.));
#61108=CARTESIAN_POINT('',(4.90747728811182,8.5,8.));
#61109=CARTESIAN_POINT('',(9.81495457622364,0.,8.));
#61110=CARTESIAN_POINT('',(-4.90747728811182,8.5,8.));
#61111=CARTESIAN_POINT('',(4.90747728811182,8.5,8.));
#61112=CARTESIAN_POINT('',(-9.81495457622364,1.11022302462516E-15,8.));
#61113=CARTESIAN_POINT('',(-4.90747728811182,8.5,8.));
#61114=CARTESIAN_POINT('',(-4.90747728811182,-8.5,8.));
#61115=CARTESIAN_POINT('',(-9.81495457622364,1.20198527055489E-15,8.));
#61116=CARTESIAN_POINT('',(-4.90747728811182,-8.5,8.));
#61117=CARTESIAN_POINT('Origin',(0.,0.,4.));
#61118=CARTESIAN_POINT('Origin',(-4.90747728811182,-8.5,0.));
#61119=CARTESIAN_POINT('',(-4.90747728811182,-8.5,0.));
#61120=CARTESIAN_POINT('',(4.90747728811182,-8.5,0.));
#61121=CARTESIAN_POINT('',(-4.90747728811182,-8.5,0.));
#61122=CARTESIAN_POINT('',(4.90747728811182,-8.5,0.));
#61123=CARTESIAN_POINT('',(-4.90747728811182,-8.5,0.));
#61124=CARTESIAN_POINT('Origin',(-9.81495457622364,1.20198527055489E-15,
0.));
#61125=CARTESIAN_POINT('',(-9.81495457622364,1.20198527055489E-15,0.));
#61126=CARTESIAN_POINT('',(-9.81495457622364,1.20198527055489E-15,0.));
#61127=CARTESIAN_POINT('',(-9.81495457622364,1.20198527055489E-15,0.));
#61128=CARTESIAN_POINT('Origin',(-4.90747728811182,8.5,0.));
#61129=CARTESIAN_POINT('',(-4.90747728811182,8.5,0.));
#61130=CARTESIAN_POINT('',(-4.90747728811182,8.5,0.));
#61131=CARTESIAN_POINT('',(-4.90747728811182,8.5,0.));
#61132=CARTESIAN_POINT('Origin',(4.90747728811182,8.5,0.));
#61133=CARTESIAN_POINT('',(4.90747728811182,8.5,0.));
#61134=CARTESIAN_POINT('',(4.90747728811182,8.5,0.));
#61135=CARTESIAN_POINT('',(4.90747728811182,8.5,0.));
#61136=CARTESIAN_POINT('Origin',(9.81495457622364,0.,0.));
#61137=CARTESIAN_POINT('',(9.81495457622364,0.,0.));
#61138=CARTESIAN_POINT('',(9.81495457622364,0.,0.));
#61139=CARTESIAN_POINT('',(9.81495457622364,0.,0.));
#61140=CARTESIAN_POINT('Origin',(4.90747728811182,-8.5,0.));
#61141=CARTESIAN_POINT('',(4.90747728811182,-8.5,0.));
#61142=CARTESIAN_POINT('Origin',(-1.11022302462516E-15,0.,0.));
#61143=CARTESIAN_POINT('',(0.,0.,0.));
#61144=CARTESIAN_POINT('Origin',(0.,0.,0.));
#61145=CARTESIAN_POINT('',(-5.5,-6.73555739531044E-16,2.));
#61146=CARTESIAN_POINT('Origin',(0.,0.,2.));
#61147=CARTESIAN_POINT('',(-5.5,-6.73555739531044E-16,0.));
#61148=CARTESIAN_POINT('',(-5.5,-6.73555739531044E-16,0.));
#61149=CARTESIAN_POINT('Origin',(0.,0.,0.));
#61150=CARTESIAN_POINT('Origin',(0.,0.,0.));
#61151=CARTESIAN_POINT('',(-11.,-1.34711147906209E-15,2.));
#61152=CARTESIAN_POINT('Origin',(0.,0.,2.));
#61153=CARTESIAN_POINT('',(-11.,-1.34711147906209E-15,0.));
#61154=CARTESIAN_POINT('',(-11.,-1.34711147906209E-15,0.));
#61155=CARTESIAN_POINT('Origin',(0.,0.,0.));
#61156=CARTESIAN_POINT('Origin',(0.,0.,2.));
#61157=CARTESIAN_POINT('Origin',(0.,0.,0.));
#61158=CARTESIAN_POINT('',(0.,0.,0.));
#61159=CARTESIAN_POINT('Origin',(0.,0.,0.));
#61160=CARTESIAN_POINT('',(-2.94490570994055,0.00214417779480537,0.322176117089595));
#61161=CARTESIAN_POINT('',(-2.94453111094736,0.00313617179185542,0.177823882910391));
#61162=CARTESIAN_POINT('',(-2.942,-3.60291088309151E-16,0.));
#61163=CARTESIAN_POINT('',(1.28892185405323,2.64462557919718,0.));
#61164=CARTESIAN_POINT('Ctrl Pts',(-2.94490570994055,0.00214417779480537,
0.322176117089595));
#61165=CARTESIAN_POINT('Ctrl Pts',(-2.94584715833611,0.124808428590093,
0.315520895872749));
#61166=CARTESIAN_POINT('Ctrl Pts',(-2.93884007386573,0.247358426874668,
0.308865674655903));
#61167=CARTESIAN_POINT('Ctrl Pts',(-2.92351947045398,0.368852411761562,
0.302210453439057));
#61168=CARTESIAN_POINT('Ctrl Pts',(-2.80238513102988,1.32946037267173,0.249590083068687));
#61169=CARTESIAN_POINT('Ctrl Pts',(-2.16153286152783,2.22405187279705,0.196969712698316));
#61170=CARTESIAN_POINT('Ctrl Pts',(-1.29099252632988,2.64857098947325,0.144349342327946));
#61171=CARTESIAN_POINT('Ctrl Pts',(-0.494964144347145,3.03675434170317,
0.0962328948852971));
#61172=CARTESIAN_POINT('Ctrl Pts',(0.493115753268411,3.03189109212113,0.0481164474426485));
#61173=CARTESIAN_POINT('Ctrl Pts',(1.29200104020318,2.64812001020929,-1.63834222883338E-16));
#61174=CARTESIAN_POINT('',(-1.28892185405328,2.64462557919715,0.));
#61175=CARTESIAN_POINT('Origin',(0.,0.,0.));
#61176=CARTESIAN_POINT('Ctrl Pts',(-1.28892185405328,2.64462557919715,2.08166817117217E-15));
#61177=CARTESIAN_POINT('Ctrl Pts',(-2.16403831185616,2.21811653527939,0.0526649636666859));
#61178=CARTESIAN_POINT('Ctrl Pts',(-2.80357657272064,1.32706756586464,0.10532992733337));
#61179=CARTESIAN_POINT('Ctrl Pts',(-2.92355402589586,0.366959843828546,
0.157994891000053));
#61180=CARTESIAN_POINT('Ctrl Pts',(-2.93861167702227,0.246462477535227,
0.164604554970166));
#61181=CARTESIAN_POINT('Ctrl Pts',(-2.94548559297357,0.124877349165528,
0.171214218940278));
#61182=CARTESIAN_POINT('Ctrl Pts',(-2.94453111094736,0.00313617179185542,
0.177823882910391));
#61183=CARTESIAN_POINT('Origin',(0.,0.,0.));
#61184=CARTESIAN_POINT('',(-2.93741501075088,0.000605053430647595,1.3221761170896));
#61185=CARTESIAN_POINT('',(-2.93743260967528,0.000720687897601403,1.17782388291039));
#61186=CARTESIAN_POINT('',(-2.942,-3.60291088309151E-16,0.));
#61187=CARTESIAN_POINT('Ctrl Pts',(-2.93741501075088,0.000605053430647595,
1.3221761170896));
#61188=CARTESIAN_POINT('Ctrl Pts',(-2.9382479568139,0.450815163107398,1.29790978476164));
#61189=CARTESIAN_POINT('Ctrl Pts',(-2.84099804532476,0.900683451883265,
1.27364345243368));
#61190=CARTESIAN_POINT('Ctrl Pts',(-2.64378204823906,1.30134356458571,1.24937712010572));
#61191=CARTESIAN_POINT('Ctrl Pts',(-2.21612867774369,2.17015567999336,1.19675674973535));
#61192=CARTESIAN_POINT('Ctrl Pts',(-1.31841648749453,2.80758195059898,1.14413637936498));
#61193=CARTESIAN_POINT('Ctrl Pts',(-0.357192829781819,2.92497002089294,
1.09151600899461));
#61194=CARTESIAN_POINT('Ctrl Pts',(0.604030827930888,3.04235809118689,1.03889563862424));
#61195=CARTESIAN_POINT('Ctrl Pts',(1.62876595310715,2.63970796116917,0.986275268253872));
#61196=CARTESIAN_POINT('Ctrl Pts',(2.25292793158662,1.89932766827126,0.933654897883501));
#61197=CARTESIAN_POINT('Ctrl Pts',(2.8770899100661,1.15894737537334,0.881034527513131));
#61198=CARTESIAN_POINT('Ctrl Pts',(3.1006787418488,0.0808369195952267,0.828414157142761));
#61199=CARTESIAN_POINT('Ctrl Pts',(2.82245137682484,-0.846673957408537,
0.775793786772391));
#61200=CARTESIAN_POINT('Ctrl Pts',(2.54422401180089,-1.7741848344123,0.72317341640202));
#61201=CARTESIAN_POINT('Ctrl Pts',(1.76418044997028,-2.55109613264171,0.67055304603165));
#61202=CARTESIAN_POINT('Ctrl Pts',(0.835554749603298,-2.82571794203434,
0.617932675661279));
#61203=CARTESIAN_POINT('Ctrl Pts',(-0.0930709507636752,-3.10033975142697,
0.565312305290909));
#61204=CARTESIAN_POINT('Ctrl Pts',(-1.17027878966702,-2.87267207198282,
0.512691934920538));
#61205=CARTESIAN_POINT('Ctrl Pts',(-1.90817450444562,-2.24552602141323,
0.460071564550168));
#61206=CARTESIAN_POINT('Ctrl Pts',(-2.55274401908064,-1.69769898118953,
0.414106415396644));
#61207=CARTESIAN_POINT('Ctrl Pts',(-2.93840347440061,-0.845052391620324,
0.368141266243119));
#61208=CARTESIAN_POINT('Ctrl Pts',(-2.94490570994055,0.00214417779480537,
0.322176117089595));
#61209=CARTESIAN_POINT('Ctrl Pts',(-2.94453111094736,0.00313617179185542,
0.177823882910391));
#61210=CARTESIAN_POINT('Ctrl Pts',(-2.93788040132423,-0.845140901703999,
0.223879182606963));
#61211=CARTESIAN_POINT('Ctrl Pts',(-2.55115114237882,-1.7009943502416,0.269934482303535));
#61212=CARTESIAN_POINT('Ctrl Pts',(-1.90455354763271,-2.24922658650796,
0.315989782000107));
#61213=CARTESIAN_POINT('Ctrl Pts',(-1.16515897070839,-2.87613882015091,
0.368654745666792));
#61214=CARTESIAN_POINT('Ctrl Pts',(-0.0859531713737992,-3.10079681277935,
0.421319709333476));
#61215=CARTESIAN_POINT('Ctrl Pts',(0.842833952810694,-2.82335342322726,
0.473984673000161));
#61216=CARTESIAN_POINT('Ctrl Pts',(1.77162107699519,-2.54591003367518,0.526649636666845));
#61217=CARTESIAN_POINT('Ctrl Pts',(2.54998952602959,-1.76636526194256,0.57931460033353));
#61218=CARTESIAN_POINT('Ctrl Pts',(2.82526196809064,-0.837265996441287,
0.631979564000215));
#61219=CARTESIAN_POINT('Ctrl Pts',(3.1005344101517,0.0918332690599885,0.684644527666899));
#61220=CARTESIAN_POINT('Ctrl Pts',(2.87271084523941,1.17048702832993,0.737309491333584));
#61221=CARTESIAN_POINT('Ctrl Pts',(2.2449320231631,1.90890163868963,0.789974455000268));
#61222=CARTESIAN_POINT('Ctrl Pts',(1.61715320108678,2.64731624904933,0.842639418666953));
#61223=CARTESIAN_POINT('Ctrl Pts',(0.589419121846451,3.0454917104988,0.895304382333637));
#61224=CARTESIAN_POINT('Ctrl Pts',(-0.37200976733393,2.9231058378395,0.947969346000322));
#61225=CARTESIAN_POINT('Ctrl Pts',(-1.33343865651431,2.8007199651802,1.00063430966701));
#61226=CARTESIAN_POINT('Ctrl Pts',(-2.22856235563474,2.15777275841214,1.05329927333369));
#61227=CARTESIAN_POINT('Ctrl Pts',(-2.6514251854394,1.28574400496261,1.10596423700038));
#61228=CARTESIAN_POINT('Ctrl Pts',(-2.8437527539192,0.889125626674557,1.12991745230371));
#61229=CARTESIAN_POINT('Ctrl Pts',(-2.93838674329414,0.445118617110292,
1.15387066760705));
#61230=CARTESIAN_POINT('Ctrl Pts',(-2.93743260967528,0.000720687897601403,
1.17782388291039));
#61231=CARTESIAN_POINT('Origin',(0.,0.,0.));
#61232=CARTESIAN_POINT('',(-2.94283216929169,-0.00254059509496668,2.3221761170896));
#61233=CARTESIAN_POINT('',(-2.94249560619114,-0.00258942729680482,2.17782388291039));
#61234=CARTESIAN_POINT('',(-2.942,-3.60291088309151E-16,0.));
#61235=CARTESIAN_POINT('Ctrl Pts',(-2.94283216929169,-0.00254059509496668,
2.3221761170896));
#61236=CARTESIAN_POINT('Ctrl Pts',(-2.93583836831966,0.770783310741536,
2.28029867365053));
#61237=CARTESIAN_POINT('Ctrl Pts',(-2.62244249954969,1.54912568223824,2.23842123021146));
#61238=CARTESIAN_POINT('Ctrl Pts',(-2.07534059520784,2.09189740289201,2.19654378677239));
#61239=CARTESIAN_POINT('Ctrl Pts',(-1.38788924974329,2.77390773164861,2.14392341640202));
#61240=CARTESIAN_POINT('Ctrl Pts',(-0.331445515483537,3.08398167899393,
2.09130304603165));
#61241=CARTESIAN_POINT('Ctrl Pts',(0.615553755286461,2.88169496582278,2.03868267566128));
#61242=CARTESIAN_POINT('Ctrl Pts',(1.56255302605646,2.67940825265162,1.98606230529091));
#61243=CARTESIAN_POINT('Ctrl Pts',(2.40010783333669,1.96476087896396,1.93344193492054));
#61244=CARTESIAN_POINT('Ctrl Pts',(2.74891040156469,1.06139789331815,1.88082156455017));
#61245=CARTESIAN_POINT('Ctrl Pts',(3.09771296979268,0.158034907672333,1.8282011941798));
#61246=CARTESIAN_POINT('Ctrl Pts',(2.95776329896845,-0.934043689931643,
1.77558082380943));
#61247=CARTESIAN_POINT('Ctrl Pts',(2.39244139669332,-1.72026117030417,1.72296045343906));
#61248=CARTESIAN_POINT('Ctrl Pts',(1.82711949441818,-2.50647865067671,1.67034008306869));
#61249=CARTESIAN_POINT('Ctrl Pts',(0.836425360692154,-2.9868350138178,1.61771971269832));
#61250=CARTESIAN_POINT('Ctrl Pts',(-0.130980997368149,-2.9437920444354,
1.56509934232795));
#61251=CARTESIAN_POINT('Ctrl Pts',(-1.09838735542844,-2.90074907505299,
1.51247897195758));
#61252=CARTESIAN_POINT('Ctrl Pts',(-2.04250593782301,-2.33430677314711,
1.45985860158721));
#61253=CARTESIAN_POINT('Ctrl Pts',(-2.5357679536495,-1.50098664208934,1.40723823121684));
#61254=CARTESIAN_POINT('Ctrl Pts',(-2.80155798635321,-1.05195919262036,
1.37888419317442));
#61255=CARTESIAN_POINT('Ctrl Pts',(-2.93644175348072,-0.525443729069001,
1.35053015513201));
#61256=CARTESIAN_POINT('Ctrl Pts',(-2.93741501075088,0.000605053430647595,
1.3221761170896));
#61257=CARTESIAN_POINT('Ctrl Pts',(-2.93743260967528,0.000720687897601403,
1.17782388291039));
#61258=CARTESIAN_POINT('Ctrl Pts',(-2.93628892837727,-0.53196109845813,
1.20653563127374));
#61259=CARTESIAN_POINT('Ctrl Pts',(-2.79780571115684,-1.06520455211536,
1.23524737963708));
#61260=CARTESIAN_POINT('Ctrl Pts',(-2.52560900690579,-1.51806949138664,
1.26395912800043));
#61261=CARTESIAN_POINT('Ctrl Pts',(-2.02632803807862,-2.34874393415536,
1.31662409166711));
#61262=CARTESIAN_POINT('Ctrl Pts',(-1.07716413993538,-2.9089825195618,1.3692890553338));
#61263=CARTESIAN_POINT('Ctrl Pts',(-0.108652539320438,-2.94471329972367,
1.42195401900048));
#61264=CARTESIAN_POINT('Ctrl Pts',(0.85985906129451,-2.98044407988555,1.47461898266717));
#61265=CARTESIAN_POINT('Ctrl Pts',(1.84771836438116,-2.49166705480286,1.52728394633385));
#61266=CARTESIAN_POINT('Ctrl Pts',(2.40686102399513,-1.70005997098112,1.57994891000054));
#61267=CARTESIAN_POINT('Ctrl Pts',(2.9660036836091,-0.908452887159384,1.63261387366722));
#61268=CARTESIAN_POINT('Ctrl Pts',(3.09642969975039,0.185984255401396,1.68527883733391));
#61269=CARTESIAN_POINT('Ctrl Pts',(2.73897659148843,1.08682694396802,1.73794380100059));
#61270=CARTESIAN_POINT('Ctrl Pts',(2.38152348322647,1.98766963253464,1.79060876466727));
#61271=CARTESIAN_POINT('Ctrl Pts',(1.53619125056127,2.69491786710711,1.84327372833396));
#61272=CARTESIAN_POINT('Ctrl Pts',(0.586406744725485,2.88778465426983,1.89593869200064));
#61273=CARTESIAN_POINT('Ctrl Pts',(-0.363377761110303,3.08065144143255,
1.94860365566733));
#61274=CARTESIAN_POINT('Ctrl Pts',(-1.41761454011667,2.75913678118554,2.00126861933401));
#61275=CARTESIAN_POINT('Ctrl Pts',(-2.09812527093809,2.0690698668059,2.0539335830007));
#61276=CARTESIAN_POINT('Ctrl Pts',(-2.63174175688638,1.52795998382732,2.09523034963726));
#61277=CARTESIAN_POINT('Ctrl Pts',(-2.93556254699721,0.76023565397735,2.13652711627383));
#61278=CARTESIAN_POINT('Ctrl Pts',(-2.94249560619114,-0.00258942729680482,
2.17782388291039));
#61279=CARTESIAN_POINT('Origin',(0.,0.,0.));
#61280=CARTESIAN_POINT('',(-2.94484294150901,0.00199174253909633,3.3221761170896));
#61281=CARTESIAN_POINT('',(-2.94526037616607,0.00180040430511289,3.17782388291039));
#61282=CARTESIAN_POINT('',(-2.942,-3.60291088309151E-16,0.));
#61283=CARTESIAN_POINT('Ctrl Pts',(-2.94484294150901,0.00199174253909633,
3.3221761170896));
#61284=CARTESIAN_POINT('Ctrl Pts',(-2.94583002736539,0.128597483532049,
3.31530793290979));
#61285=CARTESIAN_POINT('Ctrl Pts',(-2.93836342958051,0.255086036799256,
3.30843974872998));
#61286=CARTESIAN_POINT('Ctrl Pts',(-2.92204585589404,0.380422278131109,
3.30157156455017));
#61287=CARTESIAN_POINT('Ctrl Pts',(-2.79702929424561,1.34068182665933,3.2489511941798));
#61288=CARTESIAN_POINT('Ctrl Pts',(-2.15247739366928,2.23330287085301,3.19633082380943));
#61289=CARTESIAN_POINT('Ctrl Pts',(-1.28029158434589,2.65403966800756,3.14371045343906));
#61290=CARTESIAN_POINT('Ctrl Pts',(-0.4081057750225,3.0747764651621,3.09109008306869));
#61291=CARTESIAN_POINT('Ctrl Pts',(0.69171394304795,3.0236290152775,3.03846971269832));
#61292=CARTESIAN_POINT('Ctrl Pts',(1.5210867384019,2.5237607280468,2.98584934232795));
#61293=CARTESIAN_POINT('Ctrl Pts',(2.35045953375586,2.0238924408161,2.93322897195758));
#61294=CARTESIAN_POINT('Ctrl Pts',(2.90938540639331,1.07530331623929,2.8806086015872));
#61295=CARTESIAN_POINT('Ctrl Pts',(2.94474080948057,0.107585617606989,2.82798823121683));
#61296=CARTESIAN_POINT('Ctrl Pts',(2.98009621256783,-0.860132081025304,
2.77536786084646));
#61297=CARTESIAN_POINT('Ctrl Pts',(2.49188114610491,-1.84697835371309,2.7227474904761));
#61298=CARTESIAN_POINT('Ctrl Pts',(1.70119600494326,-2.40603518007504,2.67012712010573));
#61299=CARTESIAN_POINT('Ctrl Pts',(0.91051086378161,-2.965092006437,2.61750674973535));
#61300=CARTESIAN_POINT('Ctrl Pts',(-0.182644352078765,-3.09635938647313,
2.56488637936498));
#61301=CARTESIAN_POINT('Ctrl Pts',(-1.08320700768761,-2.74038967310636,
2.51226600899461));
#61302=CARTESIAN_POINT('Ctrl Pts',(-1.98376966329644,-2.3844199597396,2.45964563862424));
#61303=CARTESIAN_POINT('Ctrl Pts',(-2.69173975865374,-1.54121315296996,
2.40702526825387));
#61304=CARTESIAN_POINT('Ctrl Pts',(-2.88649532799773,-0.59263639450121,
2.3544048978835));
#61305=CARTESIAN_POINT('Ctrl Pts',(-2.92625644781122,-0.398975826678611,
2.3436619709522));
#61306=CARTESIAN_POINT('Ctrl Pts',(-2.94462630681883,-0.200923340849699,
2.3329190440209));
#61307=CARTESIAN_POINT('Ctrl Pts',(-2.94283216929169,-0.00254059509496668,
2.3221761170896));
#61308=CARTESIAN_POINT('Ctrl Pts',(-2.94249560619114,-0.00258942729680482,
2.17782388291039));
#61309=CARTESIAN_POINT('Ctrl Pts',(-2.94440414260591,-0.212580342560449,
2.18919207994051));
#61310=CARTESIAN_POINT('Ctrl Pts',(-2.92381470891138,-0.422199995772688,
2.20056027697063));
#61311=CARTESIAN_POINT('Ctrl Pts',(-2.87932772554241,-0.626618874207943,
2.21192847400075));
#61312=CARTESIAN_POINT('Ctrl Pts',(-2.67323476668884,-1.57362153232989,
2.26459343766743));
#61313=CARTESIAN_POINT('Ctrl Pts',(-1.95426416634525,-2.40900768006153,
2.31725840133412));
#61314=CARTESIAN_POINT('Ctrl Pts',(-1.04852602468143,-2.75386472764491,
2.3699233650008));
#61315=CARTESIAN_POINT('Ctrl Pts',(-0.142787883017607,-3.09872177522829,
2.42258832866749));
#61316=CARTESIAN_POINT('Ctrl Pts',(0.949717799966449,-2.95304972266342,
2.47525329233417));
#61317=CARTESIAN_POINT('Ctrl Pts',(1.7334537997702,-2.38292188563198,2.52791825600086));
#61318=CARTESIAN_POINT('Ctrl Pts',(2.51718979957395,-1.81279404860055,2.58058321966754));
#61319=CARTESIAN_POINT('Ctrl Pts',(2.99215611619739,-0.818210427102559,
2.63324818333423));
#61320=CARTESIAN_POINT('Ctrl Pts',(2.94291803037279,0.149706737509724,2.68591314700091));
#61321=CARTESIAN_POINT('Ctrl Pts',(2.89367994454819,1.11762390212201,2.7385781106676));
#61322=CARTESIAN_POINT('Ctrl Pts',(2.32023745627556,2.05887460984858,2.79124307433428));
#61323=CARTESIAN_POINT('Ctrl Pts',(1.4826919461771,2.54652764310569,2.84390803800096));
#61324=CARTESIAN_POINT('Ctrl Pts',(0.645146436078633,3.03418067636279,2.89657300166765));
#61325=CARTESIAN_POINT('Ctrl Pts',(-0.456502095845658,3.06823603515044,
2.94923796533433));
#61326=CARTESIAN_POINT('Ctrl Pts',(-1.32256928803916,2.63324686948073,3.00190292900102));
#61327=CARTESIAN_POINT('Ctrl Pts',(-2.18863648023266,2.19825770381101,3.0545678926677));
#61328=CARTESIAN_POINT('Ctrl Pts',(-2.81912233269536,1.29422401368392,3.10723285633439));
#61329=CARTESIAN_POINT('Ctrl Pts',(-2.92805183726137,0.331196319314338,
3.15989782000107));
#61330=CARTESIAN_POINT('Ctrl Pts',(-2.94041095304778,0.221931425219236,
3.16587317430418));
#61331=CARTESIAN_POINT('Ctrl Pts',(-2.94605601250203,0.111907094355046,
3.17184852860728));
#61332=CARTESIAN_POINT('Ctrl Pts',(-2.94526037616607,0.00180040430511289,
3.17782388291039));
#61333=CARTESIAN_POINT('Origin',(0.,0.,0.));
#61334=CARTESIAN_POINT('',(-2.93739242931988,0.000540407572186541,4.3221761170896));
#61335=CARTESIAN_POINT('',(-2.93753500859377,0.000882026442511373,4.17782388291039));
#61336=CARTESIAN_POINT('',(-2.942,-3.60291088309151E-16,0.));
#61337=CARTESIAN_POINT('Ctrl Pts',(-2.93739242931988,0.000540407572186541,
4.3221761170896));
#61338=CARTESIAN_POINT('Ctrl Pts',(-2.93814630501522,0.454709257120266,
4.29769682179868));
#61339=CARTESIAN_POINT('Ctrl Pts',(-2.83910536028106,0.908566671316128,
4.27321752650776));
#61340=CARTESIAN_POINT('Ctrl Pts',(-2.6385374625564,1.31194251096478,4.24873823121684));
#61341=CARTESIAN_POINT('Ctrl Pts',(-2.20739935432037,2.17903389691023,4.19611786084646));
#61342=CARTESIAN_POINT('Ctrl Pts',(-1.30713327152341,2.8128638865229,4.14349749047609));
#61343=CARTESIAN_POINT('Ctrl Pts',(-0.345447198709921,2.92638673563265,
4.09087712010572));
#61344=CARTESIAN_POINT('Ctrl Pts',(0.616238874103564,3.0399095847424,4.03825674973536));
#61345=CARTESIAN_POINT('Ctrl Pts',(1.63934493693357,2.63312529334921,3.98563637936499));
#61346=CARTESIAN_POINT('Ctrl Pts',(2.26053185174972,1.89025628960273,3.93301600899462));
#61347=CARTESIAN_POINT('Ctrl Pts',(2.88171876656588,1.14738728585625,3.88039563862425));
#61348=CARTESIAN_POINT('Ctrl Pts',(3.10098653336818,0.0684335697564567,
3.82777526825387));
#61349=CARTESIAN_POINT('Ctrl Pts',(2.8190342665149,-0.857973716122647,3.7751548978835));
#61350=CARTESIAN_POINT('Ctrl Pts',(2.53708199966161,-1.78438100200175,3.72253452751313));
#61351=CARTESIAN_POINT('Ctrl Pts',(1.75390969915275,-2.55824185766015,3.66991415714276));
#61352=CARTESIAN_POINT('Ctrl Pts',(0.824196505293748,-2.82909406262337,
3.61729378677239));
#61353=CARTESIAN_POINT('Ctrl Pts',(-0.105516688565254,-3.09994626758658,
3.56467341640202));
#61354=CARTESIAN_POINT('Ctrl Pts',(-1.18177077577439,-2.86778982185459,
3.51205304603165));
#61355=CARTESIAN_POINT('Ctrl Pts',(-1.91715720801869,-2.23776257255722,
3.45943267566128));
#61356=CARTESIAN_POINT('Ctrl Pts',(-2.55655857926025,-1.68996855643583,
3.41368048947072));
#61357=CARTESIAN_POINT('Ctrl Pts',(-2.93826750108625,-0.841388295482023,
3.36792830328016));
#61358=CARTESIAN_POINT('Ctrl Pts',(-2.94484294150901,0.00199174253909633,
3.3221761170896));
#61359=CARTESIAN_POINT('Ctrl Pts',(-2.94526037616607,0.00180040430511289,
3.17782388291039));
#61360=CARTESIAN_POINT('Ctrl Pts',(-2.93904351473207,-0.858539934689441,
3.22451349227397));
#61361=CARTESIAN_POINT('Ctrl Pts',(-2.53959728591596,-1.72390862024193,
3.27120310163755));
#61362=CARTESIAN_POINT('Ctrl Pts',(-1.87733008879233,-2.27130145042432,
3.31789271100113));
#61363=CARTESIAN_POINT('Ctrl Pts',(-1.13030567908798,-2.88874982718133,
3.37055767466781));
#61364=CARTESIAN_POINT('Ctrl Pts',(-0.0488837030099704,-3.10162488208327,
3.4232226383345));
#61365=CARTESIAN_POINT('Ctrl Pts',(0.876425794829888,-2.81337100100799,
3.47588760200118));
#61366=CARTESIAN_POINT('Ctrl Pts',(1.80173529266975,-2.5251171199327,3.52855256566786));
#61367=CARTESIAN_POINT('Ctrl Pts',(2.57093231227146,-1.73573430288019,3.58121752933455));
#61368=CARTESIAN_POINT('Ctrl Pts',(2.83512541526138,-0.803269840348294,
3.63388249300123));
#61369=CARTESIAN_POINT('Ctrl Pts',(3.0993185182513,0.129194622183599,3.68654745666792));
#61370=CARTESIAN_POINT('Ctrl Pts',(2.85850770462944,1.20474073019488,3.7392124203346));
#61371=CARTESIAN_POINT('Ctrl Pts',(2.22191964750238,1.93552360728328,3.79187738400129));
#61372=CARTESIAN_POINT('Ctrl Pts',(1.58533159037532,2.66630648437168,3.84454234766797));
#61373=CARTESIAN_POINT('Ctrl Pts',(0.552966289743035,3.05232613053722,3.89720731133465));
#61374=CARTESIAN_POINT('Ctrl Pts',(-0.406917273431679,2.91849222887777,
3.94987227500134));
#61375=CARTESIAN_POINT('Ctrl Pts',(-1.36680083660641,2.78465832721833,4.00253723866802));
#61376=CARTESIAN_POINT('Ctrl Pts',(-2.25420266232356,2.13097087773392,4.05520220233471));
#61377=CARTESIAN_POINT('Ctrl Pts',(-2.666616123304,1.25392862924115,4.10786716600139));
#61378=CARTESIAN_POINT('Ctrl Pts',(-2.84922387445754,0.865593310885713,
4.13118607163773));
#61379=CARTESIAN_POINT('Ctrl Pts',(-2.9387088904313,0.433468688742346,4.15450497727406));
#61380=CARTESIAN_POINT('Ctrl Pts',(-2.93753500859377,0.000882026442511374,
4.17782388291039));
#61381=CARTESIAN_POINT('Origin',(0.,0.,0.));
#61382=CARTESIAN_POINT('',(-2.94294893056736,-0.00252441656932667,5.3221761170896));
#61383=CARTESIAN_POINT('',(-2.94214529852914,-0.00261326515612426,5.1778238829104));
#61384=CARTESIAN_POINT('',(-2.942,-3.60291088309151E-16,0.));
#61385=CARTESIAN_POINT('Ctrl Pts',(-2.94294893056736,-0.00252441656932667,
5.3221761170896));
#61386=CARTESIAN_POINT('Ctrl Pts',(-2.93593381851913,0.774652637504292,
5.28008571068756));
#61387=CARTESIAN_POINT('Ctrl Pts',(-2.61899610205614,1.55689120032164,5.23799530428553));
#61388=CARTESIAN_POINT('Ctrl Pts',(-2.06692649506365,2.10021140779169,5.1959048978835));
#61389=CARTESIAN_POINT('Ctrl Pts',(-1.37674291943613,2.77945670358908,5.14328452751313));
#61390=CARTESIAN_POINT('Ctrl Pts',(-0.31906293568821,3.08528758407071,5.09066415714276));
#61391=CARTESIAN_POINT('Ctrl Pts',(0.627116654359043,2.8792008952563,5.03804378677239));
#61392=CARTESIAN_POINT('Ctrl Pts',(1.5732962444063,2.67311420644189,4.98542341640202));
#61393=CARTESIAN_POINT('Ctrl Pts',(2.4079754407529,1.95510994833143,4.93280304603165));
#61394=CARTESIAN_POINT('Ctrl Pts',(2.75314891878373,1.05035428518759,4.88018267566128));
#61395=CARTESIAN_POINT('Ctrl Pts',(3.09832239681456,0.145598622043775,4.82756230529091));
#61396=CARTESIAN_POINT('Ctrl Pts',(2.95399015652965,-0.945908446133409,
4.77494193492054));
#61397=CARTESIAN_POINT('Ctrl Pts',(2.38551665840565,-1.72985067733577,4.72232156455017));
#61398=CARTESIAN_POINT('Ctrl Pts',(1.81704316028163,-2.51379290853814,4.6697011941798));
#61399=CARTESIAN_POINT('Ctrl Pts',(0.824428404318513,-2.99017030276568,
4.61708082380943));
#61400=CARTESIAN_POINT('Ctrl Pts',(-0.142797221412707,-2.9432434569701,
4.56446045343906));
#61401=CARTESIAN_POINT('Ctrl Pts',(-1.11002284714393,-2.89631661117452,
4.51184008306869));
#61402=CARTESIAN_POINT('Ctrl Pts',(-2.05185934264326,-2.32608552535581,
4.45921971269832));
#61403=CARTESIAN_POINT('Ctrl Pts',(-2.54177252355539,-1.49079359130735,
4.40659934232795));
#61404=CARTESIAN_POINT('Ctrl Pts',(-2.80377530896762,-1.04408421119714,
4.3784582672485));
#61405=CARTESIAN_POINT('Ctrl Pts',(-2.93652578376122,-0.52156611314212,
4.35031719216905));
#61406=CARTESIAN_POINT('Ctrl Pts',(-2.93739242931988,0.000540407572186541,
4.3221761170896));
#61407=CARTESIAN_POINT('Ctrl Pts',(-2.93753500859377,0.000882026442511374,
4.17782388291039));
#61408=CARTESIAN_POINT('Ctrl Pts',(-2.93605771780397,-0.543513730930775,
4.20716994094074));
#61409=CARTESIAN_POINT('Ctrl Pts',(-2.79100052624987,-1.08864123864977,
4.23651599897109));
#61410=CARTESIAN_POINT('Ctrl Pts',(-2.50727405993036,-1.54814577624058,
4.26586205700145));
#61411=CARTESIAN_POINT('Ctrl Pts',(-1.99809343933257,-2.37278088572845,
4.31852702066813));
#61412=CARTESIAN_POINT('Ctrl Pts',(-1.04230710189327,-2.92165405720309,
4.37119198433482));
#61413=CARTESIAN_POINT('Ctrl Pts',(-0.0734394371752462,-2.94580807344744,
4.4238569480015));
#61414=CARTESIAN_POINT('Ctrl Pts',(0.895428227542791,-2.9699620896918,4.47652191166818));
#61415=CARTESIAN_POINT('Ctrl Pts',(1.87737721953956,-2.46939695070584,4.52918687533487));
#61416=CARTESIAN_POINT('Ctrl Pts',(2.427016324523,-1.67115837574717,4.58185183900155));
#61417=CARTESIAN_POINT('Ctrl Pts',(2.97665542950643,-0.872919800788501,
4.63451680266824));
#61418=CARTESIAN_POINT('Ctrl Pts',(3.09398464747655,0.22299221014288,4.68718176633492));
#61419=CARTESIAN_POINT('Ctrl Pts',(2.725785936287,1.11949523708763,4.73984673000161));
#61420=CARTESIAN_POINT('Ctrl Pts',(2.35758722509745,2.01599826403239,4.79251169366829));
#61421=CARTESIAN_POINT('Ctrl Pts',(1.50386058474821,2.71309230699052,4.84517665733498));
#61422=CARTESIAN_POINT('Ctrl Pts',(0.551838293166775,2.8945903085884,4.89784162100166));
#61423=CARTESIAN_POINT('Ctrl Pts',(-0.400183998414646,3.07608831018627,
4.95050658466835));
#61424=CARTESIAN_POINT('Ctrl Pts',(-1.45050194122825,2.74199027042391,5.00317154833503));
#61425=CARTESIAN_POINT('Ctrl Pts',(-2.12271361651498,2.04383596665945,5.05583651200172));
#61426=CARTESIAN_POINT('Ctrl Pts',(-2.64172618991724,1.50479316935294,5.09649896897128));
#61427=CARTESIAN_POINT('Ctrl Pts',(-2.93533688440644,0.748724173372516,
5.13716142594084));
#61428=CARTESIAN_POINT('Ctrl Pts',(-2.94214529852914,-0.00261326515612426,
5.1778238829104));
#61429=CARTESIAN_POINT('Origin',(0.,0.,0.));
#61430=CARTESIAN_POINT('',(-2.94474230559933,0.0020353165097306,6.3221761170896));
#61431=CARTESIAN_POINT('',(-2.94552589459255,0.00164462538419303,6.1778238829104));
#61432=CARTESIAN_POINT('',(-2.942,-3.60291088309151E-16,0.));
#61433=CARTESIAN_POINT('Ctrl Pts',(-2.94474230559933,0.0020353165097306,
6.3221761170896));
#61434=CARTESIAN_POINT('Ctrl Pts',(-2.94577608567865,0.132578411608025,
6.31509496994683));
#61435=CARTESIAN_POINT('Ctrl Pts',(-2.93783733482844,0.262995037552802,
6.30801382280405));
#61436=CARTESIAN_POINT('Ctrl Pts',(-2.92049520368276,0.39214902611321,6.30093267566128));
#61437=CARTESIAN_POINT('Ctrl Pts',(-2.79162493090094,1.35189898976081,6.24831230529091));
#61438=CARTESIAN_POINT('Ctrl Pts',(-2.1434950231737,2.24192544902223,6.19569193492054));
#61439=CARTESIAN_POINT('Ctrl Pts',(-1.26962729970534,2.65915768867859,6.14307156455017));
#61440=CARTESIAN_POINT('Ctrl Pts',(-0.395759576236975,3.07638992833495,
6.0904511941798));
#61441=CARTESIAN_POINT('Ctrl Pts',(0.70384596297251,3.02082794838624,6.03783082380943));
#61442=CARTESIAN_POINT('Ctrl Pts',(1.53120548099802,2.51763437940803,5.98521045343906));
#61443=CARTESIAN_POINT('Ctrl Pts',(2.35856499902354,2.0144408104298,5.93259008306869));
#61444=CARTESIAN_POINT('Ctrl Pts',(2.91367849586509,1.06361565242206,5.87996971269832));
#61445=CARTESIAN_POINT('Ctrl Pts',(2.9451489575673,0.0957638301017936,5.82734934232795));
#61446=CARTESIAN_POINT('Ctrl Pts',(2.97661941926951,-0.872087992218468,
5.77472897195758));
#61447=CARTESIAN_POINT('Ctrl Pts',(2.48444684583239,-1.85696647885126,5.72210860158721));
#61448=CARTESIAN_POINT('Ctrl Pts',(1.69152388176343,-2.41284480454905,5.66948823121684));
#61449=CARTESIAN_POINT('Ctrl Pts',(0.898600917694462,-2.96872313024685,
5.61686786084646));
#61450=CARTESIAN_POINT('Ctrl Pts',(-0.19507243700635,-3.09560129500965,
5.56424749047609));
#61451=CARTESIAN_POINT('Ctrl Pts',(-1.09419888335647,-2.73601935246765,
5.51162712010572));
#61452=CARTESIAN_POINT('Ctrl Pts',(-1.9933253297066,-2.37643740992565,5.45900674973535));
#61453=CARTESIAN_POINT('Ctrl Pts',(-2.69790486770603,-1.53039536007885,
5.40638637936499));
#61454=CARTESIAN_POINT('Ctrl Pts',(-2.88885105295217,-0.581044479598858,
5.35376600899461));
#61455=CARTESIAN_POINT('Ctrl Pts',(-2.92706166295704,-0.391068040923041,
5.34323604502627));
#61456=CARTESIAN_POINT('Ctrl Pts',(-2.94470393564848,-0.196954622309047,
5.33270608105794));
#61457=CARTESIAN_POINT('Ctrl Pts',(-2.94294893056736,-0.00252441656932667,
5.3221761170896));
#61458=CARTESIAN_POINT('Ctrl Pts',(-2.94214529852914,-0.00261326515612426,
5.1778238829104));
#61459=CARTESIAN_POINT('Ctrl Pts',(-2.94415496646843,-0.224388664623296,
5.18982638960752));
#61460=CARTESIAN_POINT('Ctrl Pts',(-2.92117618657372,-0.445751813963285,
5.20182889630465));
#61461=CARTESIAN_POINT('Ctrl Pts',(-2.87162987121487,-0.660999575716158,
5.21383140300177));
#61462=CARTESIAN_POINT('Ctrl Pts',(-2.65422904286817,-1.60547024656074,
5.26649636666845));
#61463=CARTESIAN_POINT('Ctrl Pts',(-1.92532197841492,-2.43220102048334,
5.31916133033513));
#61464=CARTESIAN_POINT('Ctrl Pts',(-1.01552544630456,-2.76620437138433,
5.37182629400182));
#61465=CARTESIAN_POINT('Ctrl Pts',(-0.105728914194198,-3.10020772228531,
5.4244912576685));
#61466=CARTESIAN_POINT('Ctrl Pts',(0.984957085573281,-2.94148365016469,
5.47715622133519));
#61467=CARTESIAN_POINT('Ctrl Pts',(1.761820540694,-2.36202602414577,5.52982118500188));
#61468=CARTESIAN_POINT('Ctrl Pts',(2.53868399581473,-1.78256839812686,5.58248614866856));
#61469=CARTESIAN_POINT('Ctrl Pts',(3.0017249062887,-0.782377218209647,5.63515111233524));
#61470=CARTESIAN_POINT('Ctrl Pts',(2.94091774630216,0.184882032222853,5.68781607600193));
#61471=CARTESIAN_POINT('Ctrl Pts',(2.88011058631563,1.15214128265535,5.74048103966861));
#61472=CARTESIAN_POINT('Ctrl Pts',(2.2954553558686,2.08646860360313,5.7931460033353));
#61473=CARTESIAN_POINT('Ctrl Pts',(1.45213925422783,2.56407295970403,5.84581096700198));
#61474=CARTESIAN_POINT('Ctrl Pts',(0.60882315258705,3.04167731580494,5.89847593066867));
#61475=CARTESIAN_POINT('Ctrl Pts',(-0.493153820247473,3.06255870705896,
5.95114089433535));
#61476=CARTESIAN_POINT('Ctrl Pts',(-1.35395830631657,2.6172457777424,6.00380585800203));
#61477=CARTESIAN_POINT('Ctrl Pts',(-2.21476279238567,2.17193284842583,6.05647082166872));
#61478=CARTESIAN_POINT('Ctrl Pts',(-2.83439479168936,1.26042559853868,6.10913578533541));
#61479=CARTESIAN_POINT('Ctrl Pts',(-2.93180238522596,0.296164363719765,
6.16180074900209));
#61480=CARTESIAN_POINT('Ctrl Pts',(-2.94168102690256,0.198373309905978,
6.1671417936382));
#61481=CARTESIAN_POINT('Ctrl Pts',(-2.94618853440423,0.100039675683843,
6.1724828382743));
#61482=CARTESIAN_POINT('Ctrl Pts',(-2.94552589459255,0.00164462538419303,
6.1778238829104));
#61483=CARTESIAN_POINT('Origin',(0.,0.,0.));
#61484=CARTESIAN_POINT('',(-2.93737184280031,0.000478285809368539,7.32217611708959));
#61485=CARTESIAN_POINT('',(-2.93765213932985,0.00105817779144944,7.17782388291039));
#61486=CARTESIAN_POINT('',(-2.942,-3.60291088309151E-16,0.));
#61487=CARTESIAN_POINT('Ctrl Pts',(-2.93737184280031,0.000478285809368539,
7.32217611708959));
#61488=CARTESIAN_POINT('Ctrl Pts',(-2.93804459091945,0.458606303769958,
7.29748385883571));
#61489=CARTESIAN_POINT('Ctrl Pts',(-2.83719423177179,0.916453996322869,
7.27279160058183));
#61490=CARTESIAN_POINT('Ctrl Pts',(-2.63324974290992,1.32252368027208,7.24809934232795));
#61491=CARTESIAN_POINT('Ctrl Pts',(-2.198634389848,2.18787738530332,7.19547897195758));
#61492=CARTESIAN_POINT('Ctrl Pts',(-1.29583121079705,2.81808837804428,7.14285860158721));
#61493=CARTESIAN_POINT('Ctrl Pts',(-0.333697177699206,2.92774986756231,
7.09023823121684));
#61494=CARTESIAN_POINT('Ctrl Pts',(0.628436855398639,3.03741135708034,7.03761786084647));
#61495=CARTESIAN_POINT('Ctrl Pts',(1.64990174254338,2.62652334337548,6.9849974904761));
#61496=CARTESIAN_POINT('Ctrl Pts',(2.26810159307568,1.88116672756646,6.93237712010573));
#61497=CARTESIAN_POINT('Ctrl Pts',(2.886301443608,1.13581011175742,6.87975674973536));
#61498=CARTESIAN_POINT('Ctrl Pts',(3.10123625752784,0.055984893844227,6.82713637936498));
#61499=CARTESIAN_POINT('Ctrl Pts',(2.81556743521199,-0.869283101865742,
6.77451600899461));
#61500=CARTESIAN_POINT('Ctrl Pts',(2.52989861289615,-1.7945510975757,6.72189563862424));
#61501=CARTESIAN_POINT('Ctrl Pts',(1.74362615434463,-2.56526187108243,6.66927526825387));
#61502=CARTESIAN_POINT('Ctrl Pts',(0.812833183747132,-2.8323797960046,6.6166548978835));
#61503=CARTESIAN_POINT('Ctrl Pts',(-0.117959786850361,-3.09949772092676,
6.56403452751313));
#61504=CARTESIAN_POINT('Ctrl Pts',(-1.19327326949384,-2.86302279726437,
6.51141415714276));
#61505=CARTESIAN_POINT('Ctrl Pts',(-1.92612469189739,-2.23004860141629,
6.45879378677239));
#61506=CARTESIAN_POINT('Ctrl Pts',(-2.56035596550109,-1.68225403062272,
6.41325456354479));
#61507=CARTESIAN_POINT('Ctrl Pts',(-2.93809401248361,-0.83749407451141,
6.3677153403172));
#61508=CARTESIAN_POINT('Ctrl Pts',(-2.94474230559933,0.0020353165097306,
6.3221761170896));
#61509=CARTESIAN_POINT('Ctrl Pts',(-2.94552589459255,0.00164462538419303,
6.1778238829104));
#61510=CARTESIAN_POINT('Ctrl Pts',(-2.93965462503178,-0.87017722046166,
6.22514780194098));
#61511=CARTESIAN_POINT('Ctrl Pts',(-2.52789003171806,-1.74682066505967,
6.27247172097156));
#61512=CARTESIAN_POINT('Ctrl Pts',(-1.85003983495055,-2.2935847848838,6.31979564000214));
#61513=CARTESIAN_POINT('Ctrl Pts',(-1.095686503369,-2.90205747891776,6.37246060366883));
#61514=CARTESIAN_POINT('Ctrl Pts',(-0.0117966524363787,-3.10198764723502,
6.42512556733551));
#61515=CARTESIAN_POINT('Ctrl Pts',(0.910000294361383,-2.80269121035772,
6.4777905310022));
#61516=CARTESIAN_POINT('Ctrl Pts',(1.83179724115916,-2.50339477348041,6.53045549466888));
#61517=CARTESIAN_POINT('Ctrl Pts',(2.59150128382206,-1.70487173140855,6.58312045833556));
#61518=CARTESIAN_POINT('Ctrl Pts',(2.8445267984577,-0.769315181970455,6.63578542200225));
#61519=CARTESIAN_POINT('Ctrl Pts',(3.09755231309333,0.166241367467632,6.68845038566893));
#61520=CARTESIAN_POINT('Ctrl Pts',(2.84389929970168,1.23883142427194,6.74111534933562));
#61521=CARTESIAN_POINT('Ctrl Pts',(2.19861937965545,1.96195091165853,6.79378031300231));
#61522=CARTESIAN_POINT('Ctrl Pts',(1.55333945960922,2.68507039904512,6.84644527666899));
#61523=CARTESIAN_POINT('Ctrl Pts',(0.51643263290838,3.05871931701401,6.89911024033567));
#61524=CARTESIAN_POINT('Ctrl Pts',(-0.441782179220013,2.91341844960141,
6.95177520400236));
#61525=CARTESIAN_POINT('Ctrl Pts',(-1.39999699134843,2.76811758218879,7.00444016766904));
#61526=CARTESIAN_POINT('Ctrl Pts',(-2.2795197889044,2.10386692939468,7.05710513133573));
#61527=CARTESIAN_POINT('Ctrl Pts',(-2.68141770473996,1.22195648411116,7.10977009500241));
#61528=CARTESIAN_POINT('Ctrl Pts',(-2.85452884366231,0.842087578115104,
7.13245469097174));
#61529=CARTESIAN_POINT('Ctrl Pts',(-2.93902534565796,0.421835844039577,
7.15513928694107));
#61530=CARTESIAN_POINT('Ctrl Pts',(-2.93765213932985,0.00105817779144944,
7.17782388291039));
#61531=CARTESIAN_POINT('Origin',(0.,0.,0.));
#61532=CARTESIAN_POINT('',(-2.94306537549688,-0.00250657139928612,8.3221761170896));
#61533=CARTESIAN_POINT('',(-2.94179645842688,-0.00262223567938445,8.17782388291039));
#61534=CARTESIAN_POINT('',(-2.942,-3.60291088309151E-16,0.));
#61535=CARTESIAN_POINT('Ctrl Pts',(-2.94306537549688,-0.00250657139928612,
8.3221761170896));
#61536=CARTESIAN_POINT('Ctrl Pts',(-2.93603346312234,0.778523040326291,
8.2798727477246));
#61537=CARTESIAN_POINT('Ctrl Pts',(-2.6155295502631,1.5646541741046,8.23756937835961));
#61538=CARTESIAN_POINT('Ctrl Pts',(-2.0584790752992,2.10849163858216,8.19526600899462));
#61539=CARTESIAN_POINT('Ctrl Pts',(-1.36557440251332,2.78496089461673,8.14264563862425));
#61540=CARTESIAN_POINT('Ctrl Pts',(-0.306675260078988,3.08654352280986,
8.09002526825387));
#61541=CARTESIAN_POINT('Ctrl Pts',(0.638669423716989,2.87666029635488,8.0374048978835));
#61542=CARTESIAN_POINT('Ctrl Pts',(1.58401410751295,2.66677706989991,7.98478452751313));
#61543=CARTESIAN_POINT('Ctrl Pts',(2.41580433267058,1.94542798879682,7.93216415714276));
#61544=CARTESIAN_POINT('Ctrl Pts',(2.75734311734437,1.03929400395132,7.87954378677239));
#61545=CARTESIAN_POINT('Ctrl Pts',(3.09888190201817,0.133160019105817,7.82692341640202));
#61546=CARTESIAN_POINT('Ctrl Pts',(2.95016924620815,-0.957758869482093,
7.77430304603165));
#61547=CARTESIAN_POINT('Ctrl Pts',(2.37855339098706,-1.73941279161662,7.72168267566128));
#61548=CARTESIAN_POINT('Ctrl Pts',(1.80693753576595,-2.52106671375116,7.66906230529091));
#61549=CARTESIAN_POINT('Ctrl Pts',(0.812418481133763,-2.99345566943229,
7.61644193492054));
#61550=CARTESIAN_POINT('Ctrl Pts',(-0.154610975618871,-2.94264651965433,
7.56382156455017));
#61551=CARTESIAN_POINT('Ctrl Pts',(-1.1216404323715,-2.89183736987637,7.5112011941798));
#61552=CARTESIAN_POINT('Ctrl Pts',(-2.06118029124457,-2.31783011463932,
7.45858082380943));
#61553=CARTESIAN_POINT('Ctrl Pts',(-2.54773645714466,-1.48057827836003,
7.40596045343906));
#61554=CARTESIAN_POINT('Ctrl Pts',(-2.80597476023112,-1.03620924430037,
7.37803234132257));
#61555=CARTESIAN_POINT('Ctrl Pts',(-2.93661093285418,-0.517686173583286,
7.35010422920608));
#61556=CARTESIAN_POINT('Ctrl Pts',(-2.93737184280031,0.000478285809368539,
7.32217611708959));
#61557=CARTESIAN_POINT('Ctrl Pts',(-2.93765213932985,0.00105817779144944,
7.17782388291039));
#61558=CARTESIAN_POINT('Ctrl Pts',(-2.93583728528984,-0.555049110608679,
7.20780425060775));
#61559=CARTESIAN_POINT('Ctrl Pts',(-2.78403605908896,-1.11207503097007,
7.23778461830511));
#61560=CARTESIAN_POINT('Ctrl Pts',(-2.48858495099342,-1.57801251517323,
7.26776498600247));
#61561=CARTESIAN_POINT('Ctrl Pts',(-1.96958124729618,-2.39650083140119,
7.32042994966915));
#61562=CARTESIAN_POINT('Ctrl Pts',(-1.00730080578659,-2.93390722608419,
7.37309491333584));
#61563=CARTESIAN_POINT('Ctrl Pts',(-0.0382136038189444,-2.94647556868157,
7.42575987700252));
#61564=CARTESIAN_POINT('Ctrl Pts',(0.930873598148709,-2.95904391127895,
7.47842484066921));
#61565=CARTESIAN_POINT('Ctrl Pts',(1.90676756057442,-2.44677420179069,7.53108980433588));
#61566=CARTESIAN_POINT('Ctrl Pts',(2.44682350205541,-1.64202110404938,7.58375476800257));
#61567=CARTESIAN_POINT('Ctrl Pts',(2.98687944353639,-0.837268006308086,
7.63641973166925));
#61568=CARTESIAN_POINT('Ctrl Pts',(3.09109736407267,0.25996847968624,7.68908469533594));
#61569=CARTESIAN_POINT('Ctrl Pts',(2.71220622763963,1.15200518015635,7.74174965900263));
#61570=CARTESIAN_POINT('Ctrl Pts',(2.33331509120659,2.04404188062646,7.79441462266931));
#61571=CARTESIAN_POINT('Ctrl Pts',(1.47131489780423,2.73087879557235,7.84707958633599));
#61572=CARTESIAN_POINT('Ctrl Pts',(0.517190633372317,2.90098128313613,7.89974455000268));
#61573=CARTESIAN_POINT('Ctrl Pts',(-0.436933631059594,3.07108377069992,
7.95240951366936));
#61574=CARTESIAN_POINT('Ctrl Pts',(-1.48318196652107,2.72445183088159,8.00507447733605));
#61575=CARTESIAN_POINT('Ctrl Pts',(-2.14699834174799,2.01831035197405,8.05773944100273));
#61576=CARTESIAN_POINT('Ctrl Pts',(-2.65153376339188,1.48160562142403,8.09776758830529));
#61577=CARTESIAN_POINT('Ctrl Pts',(-2.93514585523751,0.737219387421443,
8.13779573560784));
#61578=CARTESIAN_POINT('Ctrl Pts',(-2.94179645842688,-0.00262223567938445,
8.17782388291039));
#61579=CARTESIAN_POINT('Origin',(0.,0.,0.));
#61580=CARTESIAN_POINT('',(-2.94464008512449,0.00207742171232136,9.3221761170896));
#61581=CARTESIAN_POINT('',(-2.94577110767244,0.00147777103002609,9.1778238829104));
#61582=CARTESIAN_POINT('',(-2.942,-3.60291088309151E-16,0.));
#61583=CARTESIAN_POINT('Ctrl Pts',(-2.94464008512449,0.00207742171232136,
9.3221761170896));
#61584=CARTESIAN_POINT('Ctrl Pts',(-2.94572064417758,0.136558752036829,
9.31488200698387));
#61585=CARTESIAN_POINT('Ctrl Pts',(-2.93729508396668,0.270903986837675,
9.30758789687813));
#61586=CARTESIAN_POINT('Ctrl Pts',(-2.91889749004766,0.4038694541666,9.3002937867724));
#61587=CARTESIAN_POINT('Ctrl Pts',(-2.7861755826581,1.3630943679524,9.24767341640203));
#61588=CARTESIAN_POINT('Ctrl Pts',(-2.1344781113937,2.25051190295123,9.19505304603165));
#61589=CARTESIAN_POINT('Ctrl Pts',(-1.25894255572533,2.66423286046833,9.14243267566128));
#61590=CARTESIAN_POINT('Ctrl Pts',(-0.383407000056953,3.07795381798544,
9.08981230529091));
#61591=CARTESIAN_POINT('Ctrl Pts',(0.715966640015389,3.01797819802083,9.03719193492054));
#61592=CARTESIAN_POINT('Ctrl Pts',(1.54129954888374,2.51146745828537,8.98457156455017));
#61593=CARTESIAN_POINT('Ctrl Pts',(2.3666324577521,2.00495671854991,8.9319511941798));
#61594=CARTESIAN_POINT('Ctrl Pts',(2.91792463541645,1.05191085904358,8.87933082380943));
#61595=CARTESIAN_POINT('Ctrl Pts',(2.94550964776859,0.0839405046308018,
8.82671045343906));
#61596=CARTESIAN_POINT('Ctrl Pts',(2.97309466012074,-0.884029849781979,
8.77409008306869));
#61597=CARTESIAN_POINT('Ctrl Pts',(2.47697250716068,-1.86692469910122,8.72146971269832));
#61598=CARTESIAN_POINT('Ctrl Pts',(1.68182449914462,-2.41961555778857,8.66884934232795));
#61599=CARTESIAN_POINT('Ctrl Pts',(0.886676491128584,-2.97230641647591,
8.61622897195757));
#61600=CARTESIAN_POINT('Ctrl Pts',(-0.207497371943416,-3.09479328453138,
8.56360860158721));
#61601=CARTESIAN_POINT('Ctrl Pts',(-1.10517312337017,-2.73160492399537,
8.51098823121684));
#61602=CARTESIAN_POINT('Ctrl Pts',(-2.00284887479693,-2.36841656345936,
8.45836786084647));
#61603=CARTESIAN_POINT('Ctrl Pts',(-2.70402651457844,-1.51955297433185,
8.4057474904761));
#61604=CARTESIAN_POINT('Ctrl Pts',(-2.89116023290047,-0.56944323783011,
8.35312712010573));
#61605=CARTESIAN_POINT('Ctrl Pts',(-2.92785056302318,-0.383160187412328,
8.34281011910035));
#61606=CARTESIAN_POINT('Ctrl Pts',(-2.94478032747652,-0.192985093804385,
8.33249311809497));
#61607=CARTESIAN_POINT('Ctrl Pts',(-2.94306537549688,-0.00250657139928612,
8.3221761170896));
#61608=CARTESIAN_POINT('Ctrl Pts',(-2.94179645842688,-0.00262223567938445,
8.17782388291039));
#61609=CARTESIAN_POINT('Ctrl Pts',(-2.94389604226671,-0.236188947098698,
8.19046069927452));
#61610=CARTESIAN_POINT('Ctrl Pts',(-2.91839215134056,-0.469302718100354,
8.20309751563865));
#61611=CARTESIAN_POINT('Ctrl Pts',(-2.86352159037298,-0.695286025907358,
8.21573433200279));
#61612=CARTESIAN_POINT('Ctrl Pts',(-2.63484404877868,-1.63708990688444,
8.26839929566947));
#61613=CARTESIAN_POINT('Ctrl Pts',(-1.89610455059774,-2.45504665084187,
8.32106425933616));
#61614=CARTESIAN_POINT('Ctrl Pts',(-0.982379647459882,-2.77814844538783,
8.37372922300284));
#61615=CARTESIAN_POINT('Ctrl Pts',(-0.068654744322021,-3.1012502399338,
8.42639418666953));
#61616=CARTESIAN_POINT('Ctrl Pts',(1.02005556377276,-2.92949708506828,8.47905915033621));
#61617=CARTESIAN_POINT('Ctrl Pts',(1.78993539631662,-2.34079256521527,8.53172411400289));
#61618=CARTESIAN_POINT('Ctrl Pts',(2.55981522886048,-1.75208804536226,8.58438907766958));
#61619=CARTESIAN_POINT('Ctrl Pts',(3.01086458585342,-0.746432160521719,
8.63705404133626));
#61620=CARTESIAN_POINT('Ctrl Pts',(2.93849705553841,0.220030931794408,8.68971900500295));
#61621=CARTESIAN_POINT('Ctrl Pts',(2.86612952522341,1.18649402411053,8.74238396866963));
#61622=CARTESIAN_POINT('Ctrl Pts',(2.27034510760049,2.11376432390223,8.79504893233632));
#61623=CARTESIAN_POINT('Ctrl Pts',(1.42137896494728,2.58125171077128,8.847713896003));
#61624=CARTESIAN_POINT('Ctrl Pts',(0.572412822294062,3.04873909764032,8.90037885966968));
#61625=CARTESIAN_POINT('Ctrl Pts',(-0.529735045389435,3.05644357158669,
8.95304382333637));
#61626=CARTESIAN_POINT('Ctrl Pts',(-1.38515376586909,2.60087054680792,9.00570878700305));
#61627=CARTESIAN_POINT('Ctrl Pts',(-2.24057248634875,2.14529752202914,9.05837375066974));
#61628=CARTESIAN_POINT('Ctrl Pts',(-2.84926205962455,1.2264469985252,9.11103871433643));
#61629=CARTESIAN_POINT('Ctrl Pts',(-2.93513381881397,0.261090064936974,
9.16370367800311));
#61630=CARTESIAN_POINT('Ctrl Pts',(-2.94280828744918,0.174814884615283,
9.16841041297221));
#61631=CARTESIAN_POINT('Ctrl Pts',(-2.94630689264378,0.0881682471389342,
9.1731171479413));
#61632=CARTESIAN_POINT('Ctrl Pts',(-2.94577110767244,0.00147777103002609,
9.1778238829104));
#61633=CARTESIAN_POINT('Origin',(0.,0.,0.));
#61634=CARTESIAN_POINT('',(-2.93735377875815,0.0004158914717875,10.3221761170896));
#61635=CARTESIAN_POINT('',(-2.93779053274574,0.00122895754932335,10.1778238829104));
#61636=CARTESIAN_POINT('',(-2.942,-3.60291088309151E-16,0.));
#61637=CARTESIAN_POINT('Ctrl Pts',(-2.93735377875815,0.0004158914717875,
10.3221761170896));
#61638=CARTESIAN_POINT('Ctrl Pts',(-2.93794360094505,0.462502223744089,
10.2972708958728));
#61639=CARTESIAN_POINT('Ctrl Pts',(-2.83526550161259,0.924340675123848,
10.2723656746559));
#61640=CARTESIAN_POINT('Ctrl Pts',(-2.6279195904465,1.33308353810155,10.2474604534391));
#61641=CARTESIAN_POINT('Ctrl Pts',(-2.18983399605069,2.19668561771623,10.1948400830687));
#61642=CARTESIAN_POINT('Ctrl Pts',(-1.28450826872579,2.82326745826868,10.1422197126983));
#61643=CARTESIAN_POINT('Ctrl Pts',(-0.321941779407734,2.9290658210569,10.0895993423279));
#61644=CARTESIAN_POINT('Ctrl Pts',(0.640624709910309,3.03486418384512,10.0369789719576));
#61645=CARTESIAN_POINT('Ctrl Pts',(1.66043196122149,2.61987906886913,9.98435860158721));
#61646=CARTESIAN_POINT('Ctrl Pts',(2.27563478565877,1.87204685190273,9.93173823121684));
#61647=CARTESIAN_POINT('Ctrl Pts',(2.89083761009605,1.12421463493634,9.87911786084647));
#61648=CARTESIAN_POINT('Ctrl Pts',(3.10143600765941,0.0435353159795382,
9.82649749047609));
#61649=CARTESIAN_POINT('Ctrl Pts',(2.8120552331994,-0.880578479665677,9.77387712010572));
#61650=CARTESIAN_POINT('Ctrl Pts',(2.52267445873939,-1.8046922753109,9.72125674973535));
#61651=CARTESIAN_POINT('Ctrl Pts',(1.733314512256,-2.57224054764455,9.66863637936499));
#61652=CARTESIAN_POINT('Ctrl Pts',(0.801456763974427,-2.83561988794246,
9.61601600899462));
#61653=CARTESIAN_POINT('Ctrl Pts',(-0.130400984307143,-3.09899922824038,
9.56339563862425));
#61654=CARTESIAN_POINT('Ctrl Pts',(-1.20475653438691,-2.85820963650256,
9.51077526825387));
#61655=CARTESIAN_POINT('Ctrl Pts',(-1.93506113766943,-2.22229869434726,
9.4581548978835));
#61656=CARTESIAN_POINT('Ctrl Pts',(-2.5641326605009,-1.67453620870937,9.41282863761886));
#61657=CARTESIAN_POINT('Ctrl Pts',(-2.93792539338528,-0.833601734574448,
9.36750237735423));
#61658=CARTESIAN_POINT('Ctrl Pts',(-2.94464008512449,0.00207742171232136,
9.3221761170896));
#61659=CARTESIAN_POINT('Ctrl Pts',(-2.94577110767244,0.00147777103002609,
9.1778238829104));
#61660=CARTESIAN_POINT('Ctrl Pts',(-2.94031184592155,-0.881835546255158,
9.22578211160798));
#61661=CARTESIAN_POINT('Ctrl Pts',(-2.51599664630944,-1.76970025068938,
9.27374034030557));
#61662=CARTESIAN_POINT('Ctrl Pts',(-1.82248510748737,-2.31554023703778,
9.32169856900316));
#61663=CARTESIAN_POINT('Ctrl Pts',(-1.06091069186834,-2.91495026175178,
9.37436353266984));
#61664=CARTESIAN_POINT('Ctrl Pts',(0.0252920844727601,-3.1019069675073,
9.42702849633653));
#61665=CARTESIAN_POINT('Ctrl Pts',(0.943444704192239,-2.79161076199491,
9.47969346000322));
#61666=CARTESIAN_POINT('Ctrl Pts',(1.86159732391172,-2.48131455648253,9.5323584236699));
#61667=CARTESIAN_POINT('Ctrl Pts',(2.61169978700958,-1.67376543970224,9.58502338733658));
#61668=CARTESIAN_POINT('Ctrl Pts',(2.85352154222556,-0.735250545330611,
9.63768835100327));
#61669=CARTESIAN_POINT('Ctrl Pts',(3.09534329744155,0.203264349041017,9.69035331466995));
#61670=CARTESIAN_POINT('Ctrl Pts',(2.82888434477565,1.27274502100399,9.74301827833664));
#61671=CARTESIAN_POINT('Ctrl Pts',(2.17500480776272,1.98809774472063,9.79568324200333));
#61672=CARTESIAN_POINT('Ctrl Pts',(1.52112527074978,2.70345046843728,9.84834820567001));
#61673=CARTESIAN_POINT('Ctrl Pts',(0.479825149389799,3.06467524390761,9.90101316933669));
#61674=CARTESIAN_POINT('Ctrl Pts',(-0.476583929910364,2.90792818241875,
9.95367813300337));
#61675=CARTESIAN_POINT('Ctrl Pts',(-1.43299300921054,2.75118112092989,10.0063430966701));
#61676=CARTESIAN_POINT('Ctrl Pts',(-2.3045110464509,2.07646222248183,10.0590080603367));
#61677=CARTESIAN_POINT('Ctrl Pts',(-2.69583596380714,1.18980965393578,10.1116730240034));
#61678=CARTESIAN_POINT('Ctrl Pts',(-2.85967973895049,0.818577213506006,
10.1337233103058));
#61679=CARTESIAN_POINT('Ctrl Pts',(-2.93934508420187,0.410192546500391,
10.1557735966081));
#61680=CARTESIAN_POINT('Ctrl Pts',(-2.93779053274574,0.00122895754932335,
10.1778238829104));
#61681=CARTESIAN_POINT('Origin',(0.,0.,0.));
#61682=CARTESIAN_POINT('',(-2.94318142996902,-0.00248705772575741,11.3221761170896));
#61683=CARTESIAN_POINT('',(-2.94145083142593,-0.00261642954227547,11.1778238829104));
#61684=CARTESIAN_POINT('',(-2.942,-3.60291088309151E-16,0.));
#61685=CARTESIAN_POINT('Ctrl Pts',(-2.94318142996902,-0.00248705772575741,
11.3221761170896));
#61686=CARTESIAN_POINT('Ctrl Pts',(-2.93613735245544,0.782394524444463,
11.2796597847616));
#61687=CARTESIAN_POINT('Ctrl Pts',(-2.61204283140731,1.57241444895454,11.2371434524337));
#61688=CARTESIAN_POINT('Ctrl Pts',(-2.04999848462302,2.11673789269853,11.1946271201057));
#61689=CARTESIAN_POINT('Ctrl Pts',(-1.35438388023453,2.79042020824128,11.1420067497354));
#61690=CARTESIAN_POINT('Ctrl Pts',(-0.294282642636005,3.08774972424349,
11.089386379365));
#61691=CARTESIAN_POINT('Ctrl Pts',(0.65021190135765,2.87407334222539,11.0367660089946));
#61692=CARTESIAN_POINT('Ctrl Pts',(1.59470644535131,2.66039696020728,10.9841456386242));
#61693=CARTESIAN_POINT('Ctrl Pts',(2.42359429574009,1.93571468016887,10.9315252682539));
#61694=CARTESIAN_POINT('Ctrl Pts',(2.76149288344003,1.02821697529914,10.8789048978835));
#61695=CARTESIAN_POINT('Ctrl Pts',(3.09939147113997,0.120719270429434,10.8262845275131));
#61696=CARTESIAN_POINT('Ctrl Pts',(2.9463007961511,-0.969593859271576,10.7736641571428));
#61697=CARTESIAN_POINT('Ctrl Pts',(2.37155179497663,-1.74894687658982,10.7210437867724));
#61698=CARTESIAN_POINT('Ctrl Pts',(1.79680279380215,-2.52829989390807,10.668423416402));
#61699=CARTESIAN_POINT('Ctrl Pts',(0.800395466442055,-2.99669279884355,
10.6158030460317));
#61700=CARTESIAN_POINT('Ctrl Pts',(-0.166422238380945,-2.94200216382593,
10.5631826756613));
#61701=CARTESIAN_POINT('Ctrl Pts',(-1.13323994320395,-2.8873115288083,10.5105623052909));
#61702=CARTESIAN_POINT('Ctrl Pts',(-2.07046802548985,-2.30953735383759,
10.4579419349205));
#61703=CARTESIAN_POINT('Ctrl Pts',(-2.55365933589945,-1.47033910701379,
10.4053215645502));
#61704=CARTESIAN_POINT('Ctrl Pts',(-2.80815619982173,-1.02833338914462,
10.3776064153966));
#61705=CARTESIAN_POINT('Ctrl Pts',(-2.93669740996939,-0.513805263571333,
10.3498912662431));
#61706=CARTESIAN_POINT('Ctrl Pts',(-2.93735377875815,0.0004158914717875,
10.3221761170896));
#61707=CARTESIAN_POINT('Ctrl Pts',(-2.93779053274574,0.00122895754932335,
10.1778238829104));
#61708=CARTESIAN_POINT('Ctrl Pts',(-2.93563218928374,-0.566577199606596,
10.2084385602748));
#61709=CARTESIAN_POINT('Ctrl Pts',(-2.77690932929649,-1.13549932265473,
10.2390532376391));
#61710=CARTESIAN_POINT('Ctrl Pts',(-2.46954008606165,-1.60765366907442,
10.2696679150035));
#61711=CARTESIAN_POINT('Ctrl Pts',(-1.94078749348779,-2.41987818489459,
10.3223328786702));
#61712=CARTESIAN_POINT('Ctrl Pts',(-0.972150510867944,-2.9457409778909,
10.3749978423368));
#61713=CARTESIAN_POINT('Ctrl Pts',(-0.00298230764251388,-2.94672185015728,
10.4276628060035));
#61714=CARTESIAN_POINT('Ctrl Pts',(0.966185895582889,-2.94770272242366,
10.4803277696702));
#61715=CARTESIAN_POINT('Ctrl Pts',(1.93588531941386,-2.42380167396015,10.5329927333369));
#61716=CARTESIAN_POINT('Ctrl Pts',(2.46628089363149,-1.61264909700348,10.5856576970036));
#61717=CARTESIAN_POINT('Ctrl Pts',(2.99667646784912,-0.801496520046785,
10.6383226606703));
#61718=CARTESIAN_POINT('Ctrl Pts',(3.08776819245338,0.296907585403119,10.690987624337));
#61719=CARTESIAN_POINT('Ctrl Pts',(2.69823879520542,1.18435043817229,10.7436525880036));
#61720=CARTESIAN_POINT('Ctrl Pts',(2.30870939795745,2.07179329094149,10.7963175516703));
#61721=CARTESIAN_POINT('Ctrl Pts',(1.43855887885726,2.74827489102996,10.848982515337));
#61722=CARTESIAN_POINT('Ctrl Pts',(0.482469038528927,2.90695754754173,10.9016474790037));
#61723=CARTESIAN_POINT('Ctrl Pts',(-0.473620801799363,3.0656402040535,10.9543124426704));
#61724=CARTESIAN_POINT('Ctrl Pts',(-1.51564996335577,2.70652391698861,11.0069774063371));
#61725=CARTESIAN_POINT('Ctrl Pts',(-2.17097614256679,1.99249620947818,11.0596423700038));
#61726=CARTESIAN_POINT('Ctrl Pts',(-2.66116565955863,1.45839745352016,11.0990362076393));
#61727=CARTESIAN_POINT('Ctrl Pts',(-2.93498842496261,0.725719853723158,
11.1384300452748));
#61728=CARTESIAN_POINT('Ctrl Pts',(-2.94145083142593,-0.00261642954227547,
11.1778238829104));
#61729=CARTESIAN_POINT('Origin',(0.,0.,0.));
#61730=CARTESIAN_POINT('',(-2.9445363666432,0.00211803469319205,12.3221761170896));
#61731=CARTESIAN_POINT('',(-2.94599368555865,0.00130075687149912,12.1778238829104));
#61732=CARTESIAN_POINT('',(-2.942,-3.60291088309151E-16,0.));
#61733=CARTESIAN_POINT('Ctrl Pts',(-2.9445363666432,0.00211803469319205,
12.3221761170896));
#61734=CARTESIAN_POINT('Ctrl Pts',(-2.9456637214079,0.140538485345201,12.3146690440209));
#61735=CARTESIAN_POINT('Ctrl Pts',(-2.93673667551181,0.278812877817704,
12.3071619709522));
#61736=CARTESIAN_POINT('Ctrl Pts',(-2.91725274860024,0.415583368023806,
12.2996548978835));
#61737=CARTESIAN_POINT('Ctrl Pts',(-2.78068135240184,1.37426776932391,12.2470345275131));
#61738=CARTESIAN_POINT('Ctrl Pts',(-2.12542680364205,2.25906209195984,12.1944141571428));
#61739=CARTESIAN_POINT('Ctrl Pts',(-1.24823752065428,2.66926510338839,12.1417937867724));
#61740=CARTESIAN_POINT('Ctrl Pts',(-0.371048237666502,3.07946811481694,
12.089173416402));
#61741=CARTESIAN_POINT('Ctrl Pts',(0.728075779549269,3.01507981503809,12.0365530460316));
#61742=CARTESIAN_POINT('Ctrl Pts',(1.55136877770631,2.50526006508935,11.9839326756613));
#61743=CARTESIAN_POINT('Ctrl Pts',(2.37466177586334,1.99544031514062,11.9313123052909));
#61744=CARTESIAN_POINT('Ctrl Pts',(2.92212375496165,1.04018911502201,11.8786919349205));
#61745=CARTESIAN_POINT('Ctrl Pts',(2.9458228744686,0.0721158274039949,11.8260715645502));
#61746=CARTESIAN_POINT('Ctrl Pts',(2.96952199397554,-0.895957460214037,
11.7734511941798));
#61747=CARTESIAN_POINT('Ctrl Pts',(2.4694582538911,-1.87685283533148,11.7208308238094));
#61748=CARTESIAN_POINT('Ctrl Pts',(1.67209801460167,-2.42634732122405,11.6682104534391));
#61749=CARTESIAN_POINT('Ctrl Pts',(0.874737775312261,-2.9758418071166,11.6155900830687));
#61750=CARTESIAN_POINT('Ctrl Pts',(-0.219918963182118,-3.09393540378431,
11.5629697126983));
#61751=CARTESIAN_POINT('Ctrl Pts',(-1.11612955404462,-2.72714647754463,
11.510349342328));
#61752=CARTESIAN_POINT('Ctrl Pts',(-2.01234014490716,-2.36035755130494,
11.4577289719576));
#61753=CARTESIAN_POINT('Ctrl Pts',(-2.7101045881378,-1.50868610215784,11.4051086015872));
#61754=CARTESIAN_POINT('Ctrl Pts',(-2.89342282416388,-0.557832820042644,
11.3524882312168));
#61755=CARTESIAN_POINT('Ctrl Pts',(-2.9286231547134,-0.375252240171749,
11.3423841931744));
#61756=CARTESIAN_POINT('Ctrl Pts',(-2.94485546023631,-0.189014750280763,
11.332280155132));
#61757=CARTESIAN_POINT('Ctrl Pts',(-2.94318142996902,-0.00248705772575741,
11.3221761170896));
#61758=CARTESIAN_POINT('Ctrl Pts',(-2.94145083142593,-0.00261642954227547,
11.1778238829104));
#61759=CARTESIAN_POINT('Ctrl Pts',(-2.94362790824268,-0.247980760321293,
11.1910950089415));
#61760=CARTESIAN_POINT('Ctrl Pts',(-2.9154621622164,-0.492852393533084,
11.2043661349727));
#61761=CARTESIAN_POINT('Ctrl Pts',(-2.85500395443405,-0.729473081400432,
11.2176372610038));
#61762=CARTESIAN_POINT('Ctrl Pts',(-2.61508239022462,-1.6684755368126,11.2703022246705));
#61763=CARTESIAN_POINT('Ctrl Pts',(-1.86661606494013,-2.4775413196809,11.3229671883372));
#61764=CARTESIAN_POINT('Ctrl Pts',(-0.949093412422085,-2.7896953688222,
11.3756321520039));
#61765=CARTESIAN_POINT('Ctrl Pts',(-0.0315707599040525,-3.10184941796349,
11.4282971156705));
#61766=CARTESIAN_POINT('Ctrl Pts',(1.05500821984753,-2.91709173337779,11.4809620793372));
#61767=CARTESIAN_POINT('Ctrl Pts',(1.81779437152408,-2.31922447800469,11.5336270430039));
#61768=CARTESIAN_POINT('Ctrl Pts',(2.58058052320064,-1.7213572226316,11.5862920066706));
#61769=CARTESIAN_POINT('Ctrl Pts',(3.01957384680218,-0.710380396471107,
11.6389569703373));
#61770=CARTESIAN_POINT('Ctrl Pts',(2.93565629151018,0.255148376847553,11.691621934004));
#61771=CARTESIAN_POINT('Ctrl Pts',(2.85173873621817,1.22067715016623,11.7442868976707));
#61772=CARTESIAN_POINT('Ctrl Pts',(2.24491030203262,2.14075787064307,11.7969518613373));
#61773=CARTESIAN_POINT('Ctrl Pts',(1.39041548234847,2.59806145861508,11.849616825004));
#61774=CARTESIAN_POINT('Ctrl Pts',(0.535920662664327,3.05536504658708,11.9022817886707));
#61775=CARTESIAN_POINT('Ctrl Pts',(-0.566240542518395,3.04989150205426,
11.9549467523374));
#61776=CARTESIAN_POINT('Ctrl Pts',(-1.41615121076395,2.58412350821102,12.0076117160041));
#61777=CARTESIAN_POINT('Ctrl Pts',(-2.26606187900951,2.11835551436778,12.0602766796708));
#61778=CARTESIAN_POINT('Ctrl Pts',(-2.86372201031791,1.19229307121411,12.1129416433374));
#61779=CARTESIAN_POINT('Ctrl Pts',(-2.93804565964555,0.22597844177242,12.1656066070041));
#61780=CARTESIAN_POINT('Ctrl Pts',(-2.94379288681505,0.151256200025011,
12.1696790323062));
#61781=CARTESIAN_POINT('Ctrl Pts',(-2.94641083929854,0.0762932715455572,
12.1737514576083));
#61782=CARTESIAN_POINT('Ctrl Pts',(-2.94599368555865,0.00130075687149912,
12.1778238829104));
#61783=CARTESIAN_POINT('Origin',(0.,0.,0.));
#61784=CARTESIAN_POINT('',(-2.93733773658367,0.000353650820144602,13.3221761170896));
#61785=CARTESIAN_POINT('',(-2.93794966127546,0.0013934910171998,13.1778238829104));
#61786=CARTESIAN_POINT('',(-2.942,-3.60291088309151E-16,0.));
#61787=CARTESIAN_POINT('Ctrl Pts',(-2.93733773658367,0.000353650820144602,
13.3221761170896));
#61788=CARTESIAN_POINT('Ctrl Pts',(-2.93784318272048,0.466397170874405,
13.2970579329098));
#61789=CARTESIAN_POINT('Ctrl Pts',(-2.8333193685149,0.932226520914598,13.27193974873));
#61790=CARTESIAN_POINT('Ctrl Pts',(-2.62254748003497,1.34362161549686,13.2468215645502));
#61791=CARTESIAN_POINT('Ctrl Pts',(-2.18099904818651,2.20545788879211,13.1942011941798));
#61792=CARTESIAN_POINT('Ctrl Pts',(-1.27316460447925,2.82840106158337,13.1415808238094));
#61793=CARTESIAN_POINT('Ctrl Pts',(-0.31018098965669,2.93033473129373,13.0889604534391));
#61794=CARTESIAN_POINT('Ctrl Pts',(0.652802625165875,3.03226840100409,13.0363400830687));
#61795=CARTESIAN_POINT('Ctrl Pts',(1.67093541110377,2.61319256763355,12.9837197126983));
#61796=CARTESIAN_POINT('Ctrl Pts',(2.28313120153524,1.86289672775273,12.9310993423279));
#61797=CARTESIAN_POINT('Ctrl Pts',(2.89532699196672,1.1126008878719,12.8784789719576));
#61798=CARTESIAN_POINT('Ctrl Pts',(3.10158578689178,0.0310850414808014,
12.8258586015872));
#61799=CARTESIAN_POINT('Ctrl Pts',(2.80849777284497,-0.891859624755379,
12.7732382312168));
#61800=CARTESIAN_POINT('Ctrl Pts',(2.51540975879817,-1.81480429099155,12.7206178608465));
#61801=CARTESIAN_POINT('Ctrl Pts',(1.72297493577951,-2.57917777707278,12.6679974904761));
#61802=CARTESIAN_POINT('Ctrl Pts',(0.790067400131255,-2.83881430845519,
12.6153771201057));
#61803=CARTESIAN_POINT('Ctrl Pts',(-0.142840135516982,-3.0984508398376,
12.5627567497353));
#61804=CARTESIAN_POINT('Ctrl Pts',(-1.21622038379481,-2.85335041652122,
12.510136379365));
#61805=CARTESIAN_POINT('Ctrl Pts',(-1.94396638611522,-2.21451296488091,
12.4575160089946));
#61806=CARTESIAN_POINT('Ctrl Pts',(-2.56788867194677,-1.66681511174075,
12.4124027116929));
#61807=CARTESIAN_POINT('Ctrl Pts',(-2.93776159700942,-0.829711212970877,
12.3672894143913));
#61808=CARTESIAN_POINT('Ctrl Pts',(-2.9445363666432,0.00211803469319205,
12.3221761170896));
#61809=CARTESIAN_POINT('Ctrl Pts',(-2.94599368555865,0.00130075687149912,
12.1778238829104));
#61810=CARTESIAN_POINT('Ctrl Pts',(-2.94101617029297,-0.893516551252978,
12.226416421275));
#61811=CARTESIAN_POINT('Ctrl Pts',(-2.50391622116005,-1.79254618589271,
12.2750089596396));
#61812=CARTESIAN_POINT('Ctrl Pts',(-1.79466984706922,-2.33716467042755,
12.3236014980042));
#61813=CARTESIAN_POINT('Ctrl Pts',(-1.02598321781837,-2.92742633745608,
12.3762664616709));
#61814=CARTESIAN_POINT('Ctrl Pts',(0.0623772080302214,-3.10138285578342,
12.4289314253375));
#61815=CARTESIAN_POINT('Ctrl Pts',(0.976754244976282,-2.78013123936204,
12.4815963890042));
#61816=CARTESIAN_POINT('Ctrl Pts',(1.89113128192235,-2.45887962294065,12.5342613526709));
#61817=CARTESIAN_POINT('Ctrl Pts',(2.6315249299659,-1.64241987177053,12.5869263163376));
#61818=CARTESIAN_POINT('Ctrl Pts',(2.86210835815027,-0.701080799331296,
12.6395912800043));
#61819=CARTESIAN_POINT('Ctrl Pts',(3.09269178633465,0.240258273107937,12.692256243671));
#61820=CARTESIAN_POINT('Ctrl Pts',(2.81346499465986,1.30647666681628,12.7449212073377));
#61821=CARTESIAN_POINT('Ctrl Pts',(2.15107931219979,2.01396036610533,12.7975861710043));
#61822=CARTESIAN_POINT('Ctrl Pts',(1.48869362973973,2.72144406539436,12.850251134671));
#61823=CARTESIAN_POINT('Ctrl Pts',(0.443149056494409,3.07019307026412,12.9029160983377));
#61824=CARTESIAN_POINT('Ctrl Pts',(-0.511317558922748,2.90202221756343,
12.9555810620044));
#61825=CARTESIAN_POINT('Ctrl Pts',(-1.46578417433991,2.73385136486274,13.0082460256711));
#61826=CARTESIAN_POINT('Ctrl Pts',(-2.3291728319289,2.04876065459161,13.0609109893378));
#61827=CARTESIAN_POINT('Ctrl Pts',(-2.7098688231833,1.1574927237348,13.1135759530044));
#61828=CARTESIAN_POINT('Ctrl Pts',(-2.86467717936984,0.795062526234979,
13.1349919296398));
#61829=CARTESIAN_POINT('Ctrl Pts',(-2.93966715879244,0.398538727939818,
13.1564079062751));
#61830=CARTESIAN_POINT('Ctrl Pts',(-2.93794966127546,0.0013934910171998,
13.1778238829104));
#61831=CARTESIAN_POINT('Origin',(0.,0.,0.));
#61832=CARTESIAN_POINT('',(-2.94325266537063,-0.0024318079996577,14.3221761170896));
#61833=CARTESIAN_POINT('',(-2.94111188951679,-0.00259486169482749,14.1778238829104));
#61834=CARTESIAN_POINT('',(-2.942,-3.60291088309151E-16,0.));
#61835=CARTESIAN_POINT('Ctrl Pts',(-2.94325266537063,-0.0024318079996577,
14.3221761170896));
#61836=CARTESIAN_POINT('Ctrl Pts',(-2.93620194204164,0.786300619982285,
14.2794468217987));
#61837=CARTESIAN_POINT('Ctrl Pts',(-2.60854122084458,1.58016790859219,14.2367175265078));
#61838=CARTESIAN_POINT('Ctrl Pts',(-2.04150376744995,2.12493551247607,14.1939882312168));
#61839=CARTESIAN_POINT('Ctrl Pts',(-1.34320718641939,2.79580716825642,14.1413678608465));
#61840=CARTESIAN_POINT('Ctrl Pts',(-0.281884150596186,3.08890703892681,
14.0887474904761));
#61841=CARTESIAN_POINT('Ctrl Pts',(0.661753798897932,2.87144767774516,14.0361271201057));
#61842=CARTESIAN_POINT('Ctrl Pts',(1.60539174839208,2.65398831656351,13.9835067497354));
#61843=CARTESIAN_POINT('Ctrl Pts',(2.43134461155714,1.92596972352975,13.930886379365));
#61844=CARTESIAN_POINT('Ctrl Pts',(2.76559296922098,1.01711939779235,13.8782660089946));
#61845=CARTESIAN_POINT('Ctrl Pts',(3.09984132688481,0.108269072054953,13.8256456386242));
#61846=CARTESIAN_POINT('Ctrl Pts',(2.94238517904746,-0.981412986386104,
13.7730252682539));
#61847=CARTESIAN_POINT('Ctrl Pts',(2.36451469520878,-1.75845069530582,13.7204048978835));
#61848=CARTESIAN_POINT('Ctrl Pts',(1.7866442113701,-2.53548840422553,13.6677845275131));
#61849=CARTESIAN_POINT('Ctrl Pts',(0.788359391530092,-2.99988176362388,
13.6151641571428));
#61850=CARTESIAN_POINT('Ctrl Pts',(-0.178232238982059,-2.94131149038551,
13.5625437867724));
#61851=CARTESIAN_POINT('Ctrl Pts',(-1.14482386949421,-2.88274121714715,
13.509923416402));
#61852=CARTESIAN_POINT('Ctrl Pts',(-2.07972231067849,-2.30120731127206,
13.4573030460317));
#61853=CARTESIAN_POINT('Ctrl Pts',(-2.5595403212758,-1.46007567143488,13.4046826756613));
#61854=CARTESIAN_POINT('Ctrl Pts',(-2.81031856879004,-1.02045582826861,
13.3771804894707));
#61855=CARTESIAN_POINT('Ctrl Pts',(-2.9367843178467,-0.509922711901109,
13.3496783032802));
#61856=CARTESIAN_POINT('Ctrl Pts',(-2.93733773658367,0.000353650820144602,
13.3221761170896));
#61857=CARTESIAN_POINT('Ctrl Pts',(-2.93794966127546,0.0013934910171998,
13.1778238829104));
#61858=CARTESIAN_POINT('Ctrl Pts',(-2.9354435856223,-0.578098472832708,
13.2090728699418));
#61859=CARTESIAN_POINT('Ctrl Pts',(-2.76961959866241,-1.15891354184382,
13.2403218569731));
#61860=CARTESIAN_POINT('Ctrl Pts',(-2.45014221851649,-1.63706498032062,
13.2715708440045));
#61861=CARTESIAN_POINT('Ctrl Pts',(-1.91171629767549,-2.44290960207673,
13.3242358076712));
#61862=CARTESIAN_POINT('Ctrl Pts',(-0.936861131073665,-2.95715369414646,
13.3769007713379));
#61863=CARTESIAN_POINT('Ctrl Pts',(0.032249473718084,-2.94654692146698,
13.4295657350046));
#61864=CARTESIAN_POINT('Ctrl Pts',(1.00136007850986,-2.9359401487875,13.4822306986712));
#61865=CARTESIAN_POINT('Ctrl Pts',(1.96472612149158,-2.40048251135878,13.5348956623379));
#61866=CARTESIAN_POINT('Ctrl Pts',(2.48538560527679,-1.58304647931889,13.5875606260046));
#61867=CARTESIAN_POINT('Ctrl Pts',(3.00604508906198,-0.765610447279041,
13.6402255896713));
#61868=CARTESIAN_POINT('Ctrl Pts',(3.08399801365073,0.333803979371919,13.692890553338));
#61869=CARTESIAN_POINT('Ctrl Pts',(2.68388585052197,1.21652624548705,13.7455555170047));
#61870=CARTESIAN_POINT('Ctrl Pts',(2.28377368739319,2.0992485116022,13.7982204806713));
#61871=CARTESIAN_POINT('Ctrl Pts',(1.40559643654686,2.76527861718149,13.850885444338));
#61872=CARTESIAN_POINT('Ctrl Pts',(0.447678061833244,2.91251851826326,13.9035504080047));
#61873=CARTESIAN_POINT('Ctrl Pts',(-0.510240312880357,3.05975841934504,
13.9562153716714));
#61874=CARTESIAN_POINT('Ctrl Pts',(-1.54789981146125,2.68820811592931,14.0088803353381));
#61875=CARTESIAN_POINT('Ctrl Pts',(-2.1946428070508,1.96639671204873,14.0615452990048));
#61876=CARTESIAN_POINT('Ctrl Pts',(-2.67062249982462,1.435169358057,14.1003048269733));
#61877=CARTESIAN_POINT('Ctrl Pts',(-2.93486488519192,0.714225423327012,
14.1390643549419));
#61878=CARTESIAN_POINT('Ctrl Pts',(-2.94111188951679,-0.00259486169482749,
14.1778238829104));
#61879=CARTESIAN_POINT('Origin',(0.,0.,-1.84858989190501));
#61880=CARTESIAN_POINT('',(-2.37275986033066,-0.00196044888638088,14.651410108095));
#61881=CARTESIAN_POINT('',(-2.37517539399571,0.0009292342096269,14.848589891905));
#61882=CARTESIAN_POINT('',(-2.37175,-2.62313128856983E-13,-1.84858989190501));
#61883=CARTESIAN_POINT('',(-2.34668236863853,0.343918483395512,15.62825));
#61884=CARTESIAN_POINT('Ctrl Pts',(-2.37275986033066,-0.00196044888638126,
14.651410108095));
#61885=CARTESIAN_POINT('Ctrl Pts',(-2.37407562336888,-0.149148890039704,
14.6613011831744));
#61886=CARTESIAN_POINT('Ctrl Pts',(-2.29486163858049,-1.07797575416432,
14.7238126286243));
#61887=CARTESIAN_POINT('Ctrl Pts',(-1.07036982067409,-2.58532778276268,
14.8389444444444));
#61888=CARTESIAN_POINT('Ctrl Pts',(1.57881200919325,-2.30987053095853,14.9968055555556));
#61889=CARTESIAN_POINT('Ctrl Pts',(2.79654399706859,0.0566462213665858,
15.1546666666667));
#61890=CARTESIAN_POINT('Ctrl Pts',(1.48409012818578,2.37398300468726,15.3125277777778));
#61891=CARTESIAN_POINT('Ctrl Pts',(-1.17817012667699,2.53688639776398,15.4703888888889));
#61892=CARTESIAN_POINT('Ctrl Pts',(-2.23297482288527,1.11978691060522,15.5756296296296));
#61893=CARTESIAN_POINT('Ctrl Pts',(-2.34668236863854,0.343918483395395,
15.62825));
#61894=CARTESIAN_POINT('',(-0.439445221994505,2.33068358199182,15.62825));
#61895=CARTESIAN_POINT('Origin',(0.,0.,15.62825));
#61896=CARTESIAN_POINT('Ctrl Pts',(-2.37517539399571,0.000929234209626874,
14.848589891905));
#61897=CARTESIAN_POINT('Ctrl Pts',(-2.37154287511732,-0.72977569986937,
14.8978167399366));
#61898=CARTESIAN_POINT('Ctrl Pts',(-1.620069408967,-2.24871933567263,14.9997085516349));
#61899=CARTESIAN_POINT('Ctrl Pts',(0.958368222991996,-2.62865236842956,
15.1542653269999));
#61900=CARTESIAN_POINT('Ctrl Pts',(2.7277014223945,-0.634378452891388,15.3122602179999));
#61901=CARTESIAN_POINT('Ctrl Pts',(2.01676643438217,1.93930517753648,15.470255109));
#61902=CARTESIAN_POINT('Ctrl Pts',(0.331786659212352,2.47609764328476,15.5755850363333));
#61903=CARTESIAN_POINT('Ctrl Pts',(-0.439445221994538,2.33068358199181,
15.62825));
#61904=CARTESIAN_POINT('Origin',(0.,0.,-1.84858989190501));
#61905=CARTESIAN_POINT('',(-2.36799142649297,0.000285102424211894,13.651410108095));
#61906=CARTESIAN_POINT('',(-2.37103403261776,-0.00209189776527924,13.848589891905));
#61907=CARTESIAN_POINT('',(-2.37175,-2.62313128856983E-13,-1.84858989190501));
#61908=CARTESIAN_POINT('Ctrl Pts',(-2.36799142649297,0.000285102424211897,
13.651410108095));
#61909=CARTESIAN_POINT('Ctrl Pts',(-2.36754527731231,-0.41108402173757,
13.6789122942855));
#61910=CARTESIAN_POINT('Ctrl Pts',(-2.07052456040773,-1.61013525385437,
13.7590348508465));
#61911=CARTESIAN_POINT('Ctrl Pts',(-0.16923542984156,-2.79279215602584,
13.8917777777778));
#61912=CARTESIAN_POINT('Ctrl Pts',(2.24512421134353,-1.66965318578134,14.0496388888889));
#61913=CARTESIAN_POINT('Ctrl Pts',(2.62593313585052,0.965751391486786,14.2075));
#61914=CARTESIAN_POINT('Ctrl Pts',(0.628359679142483,2.72647005025058,14.3653611111111));
#61915=CARTESIAN_POINT('Ctrl Pts',(-1.77762972544941,2.06202090562868,14.5133311471428));
#61916=CARTESIAN_POINT('Ctrl Pts',(-2.36707578383325,0.633891398858792,
14.6086808128041));
#61917=CARTESIAN_POINT('Ctrl Pts',(-2.37275986033066,-0.00196044888638126,
14.651410108095));
#61918=CARTESIAN_POINT('Ctrl Pts',(-2.37103403261776,-0.00209189776527889,
13.848589891905));
#61919=CARTESIAN_POINT('Ctrl Pts',(-2.37284080801943,-0.20941258958213,
13.8624953276032));
#61920=CARTESIAN_POINT('Ctrl Pts',(-2.25333213139831,-1.19988405133594,
13.929065726968));
#61921=CARTESIAN_POINT('Ctrl Pts',(-0.869666078203209,-2.66015561356989,
14.0483010899995));
#61922=CARTESIAN_POINT('Ctrl Pts',(1.75267763866885,-2.18191305067097,14.2062959809995));
#61923=CARTESIAN_POINT('Ctrl Pts',(2.78512620401791,0.275629071355557,14.3642908719996));
#61924=CARTESIAN_POINT('Ctrl Pts',(1.29091271455523,2.48320730756548,14.5222857629997));
#61925=CARTESIAN_POINT('Ctrl Pts',(-1.37414448785656,2.43798182357128,14.6802806539997));
#61926=CARTESIAN_POINT('Ctrl Pts',(-2.35095938458833,0.884486526760038,
14.7890486969682));
#61927=CARTESIAN_POINT('Ctrl Pts',(-2.37542909742077,0.0519633377314283,
14.8451517762699));
#61928=CARTESIAN_POINT('Ctrl Pts',(-2.37517539399571,0.000929234209626874,
14.848589891905));
#61929=CARTESIAN_POINT('Origin',(0.,0.,-1.84858989190501));
#61930=CARTESIAN_POINT('',(-2.3737947408518,0.00170749448784205,12.651410108095));
#61931=CARTESIAN_POINT('',(-2.36848474137664,0.00112338963946246,12.848589891905));
#61932=CARTESIAN_POINT('',(-2.37175,-2.62313128856983E-13,-1.84858989190501));
#61933=CARTESIAN_POINT('Ctrl Pts',(-2.3737947408518,0.00170749448784207,
12.651410108095));
#61934=CARTESIAN_POINT('Ctrl Pts',(-2.36833312974404,-0.668887685031927,
12.6965234053967));
#61935=CARTESIAN_POINT('Ctrl Pts',(-1.72235411599047,-2.13088047848934,
12.7942570730687));
#61936=CARTESIAN_POINT('Ctrl Pts',(0.750172845833004,-2.69546828972993,
12.9446111111111));
#61937=CARTESIAN_POINT('Ctrl Pts',(2.66668266040929,-0.846825037914988,
13.1024722222222));
#61938=CARTESIAN_POINT('Ctrl Pts',(2.16784415239069,1.76882949166842,13.2603333333333));
#61939=CARTESIAN_POINT('Ctrl Pts',(-0.294517949969841,2.78236767093066,
13.4181944444444));
#61940=CARTESIAN_POINT('Ctrl Pts',(-2.10760963637491,1.5382497642797,13.548553369365));
#61941=CARTESIAN_POINT('Ctrl Pts',(-2.36839890163746,0.375995067988055,
13.6262919239152));
#61942=CARTESIAN_POINT('Ctrl Pts',(-2.36799142649297,0.000285102424211897,
13.651410108095));
#61943=CARTESIAN_POINT('Ctrl Pts',(-2.36848474137664,0.00112338963946246,
12.848589891905));
#61944=CARTESIAN_POINT('Ctrl Pts',(-2.36646442019019,-0.466045225337024,
12.8798388789364));
#61945=CARTESIAN_POINT('Ctrl Pts',(-2.00748312661735,-1.72341304420753,
12.9637528296344));
#61946=CARTESIAN_POINT('Ctrl Pts',(0.0306296239850783,-2.7985342282319,
13.1003317439992));
#61947=CARTESIAN_POINT('Ctrl Pts',(2.36053793034993,-1.50352574600393,13.2583266349992));
#61948=CARTESIAN_POINT('Ctrl Pts',(2.54906768788899,1.15541663986578,13.4163215259993));
#61949=CARTESIAN_POINT('Ctrl Pts',(0.42518914129335,2.76621565710669,13.5743164169993));
#61950=CARTESIAN_POINT('Ctrl Pts',(-1.86352481270074,1.94670562977947,13.7184058723013));
#61951=CARTESIAN_POINT('Ctrl Pts',(-2.36599788968529,0.57578658999839,13.8098303639365));
#61952=CARTESIAN_POINT('Ctrl Pts',(-2.37103403261776,-0.00209189776527889,
13.848589891905));
#61953=CARTESIAN_POINT('Origin',(0.,0.,-1.84858989190501));
#61954=CARTESIAN_POINT('',(-2.37270243253876,-0.00200498951788303,11.651410108095));
#61955=CARTESIAN_POINT('',(-2.37496958658182,0.00104863022067879,11.848589891905));
#61956=CARTESIAN_POINT('',(-2.37175,-2.62313128856983E-13,-1.84858989190501));
#61957=CARTESIAN_POINT('Ctrl Pts',(-2.37270243253876,-0.00200498951788284,
11.651410108095));
#61958=CARTESIAN_POINT('Ctrl Pts',(-2.37405198430164,-0.152377883745359,
11.6615141461374));
#61959=CARTESIAN_POINT('Ctrl Pts',(-2.29281607417404,-1.08441874324097,
11.7242385545502));
#61960=CARTESIAN_POINT('Ctrl Pts',(-1.05977053720295,-2.58943908287633,
11.8395833333333));
#61961=CARTESIAN_POINT('Ctrl Pts',(1.58766534266525,-2.30382879610199,11.9974444444444));
#61962=CARTESIAN_POINT('Ctrl Pts',(2.79707340746319,0.0684743370742143,
12.1553055555555));
#61963=CARTESIAN_POINT('Ctrl Pts',(1.47303233105958,2.37875683253439,12.3131666666667));
#61964=CARTESIAN_POINT('Ctrl Pts',(-1.18520769732058,2.53448043892505,12.4710277777778));
#61965=CARTESIAN_POINT('Ctrl Pts',(-2.31706196946124,1.00613052370996,12.5837755915872));
#61966=CARTESIAN_POINT('Ctrl Pts',(-2.37470357962243,0.113297808503467,
12.6439030350263));
#61967=CARTESIAN_POINT('Ctrl Pts',(-2.3737947408518,0.00170749448784207,
12.651410108095));
#61968=CARTESIAN_POINT('Ctrl Pts',(-2.37496958658182,0.00104863022067909,
11.848589891905));
#61969=CARTESIAN_POINT('Ctrl Pts',(-2.37095686672064,-0.72032558818314,
11.8971824302696));
#61970=CARTESIAN_POINT('Ctrl Pts',(-1.63667192852724,-2.23060698037937,
11.9984399323009));
#61971=CARTESIAN_POINT('Ctrl Pts',(0.927689321261817,-2.64047796075702,
12.1523623979988));
#61972=CARTESIAN_POINT('Ctrl Pts',(2.71833714731268,-0.66586366962402,12.3103572889989));
#61973=CARTESIAN_POINT('Ctrl Pts',(2.04302496870488,1.91279385105346,12.468352179999));
#61974=CARTESIAN_POINT('Ctrl Pts',(-0.48563275555883,2.75624604578475,12.626347070999));
#61975=CARTESIAN_POINT('Ctrl Pts',(-2.16074812800628,1.4270578867686,12.7530929749677));
#61976=CARTESIAN_POINT('Ctrl Pts',(-2.36986933510064,0.32128967640745,12.8271739152697));
#61977=CARTESIAN_POINT('Ctrl Pts',(-2.36848474137664,0.00112338963946246,
12.848589891905));
#61978=CARTESIAN_POINT('Origin',(0.,0.,-1.84858989190501));
#61979=CARTESIAN_POINT('',(-2.3680043592011,0.000335278925106314,10.651410108095));
#61980=CARTESIAN_POINT('',(-2.37130727717011,-0.00210928510120167,10.848589891905));
#61981=CARTESIAN_POINT('',(-2.37175,-2.62313128856983E-13,-1.84858989190501));
#61982=CARTESIAN_POINT('Ctrl Pts',(-2.3680043592011,0.000335278925106194,
10.651410108095));
#61983=CARTESIAN_POINT('Ctrl Pts',(-2.36747521485208,-0.414214015593381,
10.6791252572485));
#61984=CARTESIAN_POINT('Ctrl Pts',(-2.06710351553143,-1.61654972761244,
10.7594607767724));
#61985=CARTESIAN_POINT('Ctrl Pts',(-0.158018739337926,-2.79344562132492,
10.8924166666667));
#61986=CARTESIAN_POINT('Ctrl Pts',(2.25180017160661,-1.66063371893121,11.0502777777778));
#61987=CARTESIAN_POINT('Ctrl Pts',(2.62205116590109,0.976297109112734,11.2081388888889));
#61988=CARTESIAN_POINT('Ctrl Pts',(0.617379419647229,2.72894686881467,11.366));
#61989=CARTESIAN_POINT('Ctrl Pts',(-1.78238141625357,2.05587933285381,11.5137570730687));
#61990=CARTESIAN_POINT('Ctrl Pts',(-2.36702371369352,0.630742424660346,
11.608893775767));
#61991=CARTESIAN_POINT('Ctrl Pts',(-2.37270243253876,-0.00200498951788284,
11.651410108095));
#61992=CARTESIAN_POINT('Ctrl Pts',(-2.37130727717011,-0.00210928510120129,
10.848589891905));
#61993=CARTESIAN_POINT('Ctrl Pts',(-2.37306236960384,-0.199914469168129,
10.8618610179362));
#61994=CARTESIAN_POINT('Ctrl Pts',(-2.26024839139859,-1.18071373741556,
10.927797107634));
#61995=CARTESIAN_POINT('Ctrl Pts',(-0.90141796228012,-2.64956165719617,
11.0463981609985));
#61996=CARTESIAN_POINT('Ctrl Pts',(1.72648179491819,-2.20272375262492,11.2043930519985));
#61997=CARTESIAN_POINT('Ctrl Pts',(2.7881905800153,0.242331605070017,11.3623879429986));
#61998=CARTESIAN_POINT('Ctrl Pts',(1.32057126786748,2.46755402056041,11.5203828339987));
#61999=CARTESIAN_POINT('Ctrl Pts',(-1.34501422335496,2.45431621031658,11.6783777249987));
#62000=CARTESIAN_POINT('Ctrl Pts',(-2.34590203170026,0.903460530701682,
11.7877800776342));
#62001=CARTESIAN_POINT('Ctrl Pts',(-2.37530588310888,0.0615052912262518,
11.8445174666029));
#62002=CARTESIAN_POINT('Ctrl Pts',(-2.37496958658182,0.00104863022067909,
11.848589891905));
#62003=CARTESIAN_POINT('Origin',(0.,0.,-1.84858989190501));
#62004=CARTESIAN_POINT('',(-2.37387835550442,0.0016747535505271,9.65141010809499));
#62005=CARTESIAN_POINT('',(-2.36835645684558,0.000990747813277848,9.84858989190503));
#62006=CARTESIAN_POINT('',(-2.37175,-2.62313128856983E-13,-1.84858989190501));
#62007=CARTESIAN_POINT('Ctrl Pts',(-2.37387835550442,0.00167475355052717,
9.65141010809499));
#62008=CARTESIAN_POINT('Ctrl Pts',(-2.36846517734921,-0.672024104003181,
9.69673636835963));
#62009=CARTESIAN_POINT('Ctrl Pts',(-1.71729169385484,-2.1369916722257,9.79468299899462));
#62010=CARTESIAN_POINT('Ctrl Pts',(0.760987165659879,-2.69243512365168,
9.94525));
#62011=CARTESIAN_POINT('Ctrl Pts',(2.6700603672968,-0.836113626465368,10.1031111111111));
#62012=CARTESIAN_POINT('Ctrl Pts',(2.16072649637127,1.7775177549783,10.2609722222222));
#62013=CARTESIAN_POINT('Ctrl Pts',(-0.305685313585232,2.78116249982291,
10.4188333333333));
#62014=CARTESIAN_POINT('Ctrl Pts',(-2.11081288774265,1.53182193243431,10.5489792952909));
#62015=CARTESIAN_POINT('Ctrl Pts',(-2.36847985572451,0.37285508129321,10.6265048868781));
#62016=CARTESIAN_POINT('Ctrl Pts',(-2.3680043592011,0.000335278925106194,
10.651410108095));
#62017=CARTESIAN_POINT('Ctrl Pts',(-2.36835645684558,0.00099074781327764,
9.84858989190503));
#62018=CARTESIAN_POINT('Ctrl Pts',(-2.36661646666674,-0.456757128880904,
9.87920456926939));
#62019=CARTESIAN_POINT('Ctrl Pts',(-2.01853982608692,-1.70439405627733,
9.96248421030043));
#62020=CARTESIAN_POINT('Ctrl Pts',(-0.00283249851198579,-2.79870028674429,
10.0984288149982));
#62021=CARTESIAN_POINT('Ctrl Pts',(2.34239313895008,-1.53164150527581,10.2564237059982));
#62022=CARTESIAN_POINT('Ctrl Pts',(2.56269918704329,1.12485741087042,10.4144185969983));
#62023=CARTESIAN_POINT('Ctrl Pts',(0.458233353927178,2.76093344928963,10.5724134879983));
#62024=CARTESIAN_POINT('Ctrl Pts',(-1.85023633825226,1.96536160231837,10.7171372529672));
#62025=CARTESIAN_POINT('Ctrl Pts',(-2.36609748365237,0.585053046589831,
10.8091960542695));
#62026=CARTESIAN_POINT('Ctrl Pts',(-2.37130727717011,-0.00210928510120129,
10.848589891905));
#62027=CARTESIAN_POINT('Origin',(0.,0.,-1.84858989190501));
#62028=CARTESIAN_POINT('',(-2.37260887298938,-0.00202072084187682,8.65141010809499));
#62029=CARTESIAN_POINT('',(-2.3747901511292,0.00119133359606532,8.84858989190503));
#62030=CARTESIAN_POINT('',(-2.37175,-2.62313128856983E-13,-1.84858989190501));
#62031=CARTESIAN_POINT('Ctrl Pts',(-2.37260887298937,-0.00202072084187674,
8.65141010809499));
#62032=CARTESIAN_POINT('Ctrl Pts',(-2.37399141457934,-0.155578652695773,
8.66172710910036));
#62033=CARTESIAN_POINT('Ctrl Pts',(-2.29073220490892,-1.09084435213441,
8.72466448047611));
#62034=CARTESIAN_POINT('Ctrl Pts',(-1.04936735270146,-2.59367240037321,
8.84022222222223));
#62035=CARTESIAN_POINT('Ctrl Pts',(1.59690068918271,-2.29743695240177,8.99808333333332));
#62036=CARTESIAN_POINT('Ctrl Pts',(2.79677599470576,0.0797019247629725,
9.15594444444445));
#62037=CARTESIAN_POINT('Ctrl Pts',(1.46347155312646,2.38465078671139,9.31380555555555));
#62038=CARTESIAN_POINT('Ctrl Pts',(-1.19537219008389,2.52970229247383,9.47166666666666));
#62039=CARTESIAN_POINT('Ctrl Pts',(-2.31895585283185,0.999716542450464,
9.58420151751315));
#62040=CARTESIAN_POINT('Ctrl Pts',(-2.37474946901026,0.110089469797055,
9.64411599798926));
#62041=CARTESIAN_POINT('Ctrl Pts',(-2.37387835550442,0.00167475355052717,
9.65141010809499));
#62042=CARTESIAN_POINT('Ctrl Pts',(-2.3747901511292,0.00119133359606537,
8.84858989190503));
#62043=CARTESIAN_POINT('Ctrl Pts',(-2.37038906205444,-0.71090872088079,
8.89654812060261));
#62044=CARTESIAN_POINT('Ctrl Pts',(-1.65267775677864,-2.21269450774448,
8.99717131296688));
#62045=CARTESIAN_POINT('Ctrl Pts',(0.896053003445084,-2.6513808351669,9.15045946899784));
#62046=CARTESIAN_POINT('Ctrl Pts',(2.71018167460651,-0.698316982967359,
9.30845435999788));
#62047=CARTESIAN_POINT('Ctrl Pts',(2.06574861445826,1.88823038317285,9.46644925099794));
#62048=CARTESIAN_POINT('Ctrl Pts',(-0.45264386973844,2.76185532663481,9.62444414199799));
#62049=CARTESIAN_POINT('Ctrl Pts',(-2.15199374797492,1.44623886325989,9.75182435563369));
#62050=CARTESIAN_POINT('Ctrl Pts',(-2.36960968846224,0.330684626839437,
9.8265396056027));
#62051=CARTESIAN_POINT('Ctrl Pts',(-2.36835645684558,0.00099074781327764,
9.84858989190503));
#62052=CARTESIAN_POINT('Origin',(0.,0.,-1.84858989190501));
#62053=CARTESIAN_POINT('',(-2.36801892187683,0.000385579322849399,7.65141010809499));
#62054=CARTESIAN_POINT('',(-2.37158591103805,-0.00211396583053219,7.84858989190503));
#62055=CARTESIAN_POINT('',(-2.37175,-2.62313128856983E-13,-1.84858989190501));
#62056=CARTESIAN_POINT('Ctrl Pts',(-2.36801892187683,0.000385579322849869,
7.65141010809499));
#62057=CARTESIAN_POINT('Ctrl Pts',(-2.36740549965901,-0.417342685994756,
7.67933822021147));
#62058=CARTESIAN_POINT('Ctrl Pts',(-2.06366306314178,-1.62296175556451,
7.75988670269832));
#62059=CARTESIAN_POINT('Ctrl Pts',(-0.146803886877873,-2.79405744038503,
7.89305555555557));
#62060=CARTESIAN_POINT('Ctrl Pts',(2.25844822171206,-1.65158105802259,8.05091666666665));
#62061=CARTESIAN_POINT('Ctrl Pts',(2.61811094239596,0.986814802625037,8.20877777777778));
#62062=CARTESIAN_POINT('Ctrl Pts',(0.606419780073446,2.73140319464357,8.36663888888888));
#62063=CARTESIAN_POINT('Ctrl Pts',(-1.7871649975578,2.04969182184781,8.51418299899463));
#62064=CARTESIAN_POINT('Ctrl Pts',(-2.36693996130543,0.627621353124904,
8.60910673873));
#62065=CARTESIAN_POINT('Ctrl Pts',(-2.37260887298937,-0.00202072084187674,
8.65141010809499));
#62066=CARTESIAN_POINT('Ctrl Pts',(-2.37158591103805,-0.002113965830532,
7.84858989190503));
#62067=CARTESIAN_POINT('Ctrl Pts',(-2.37327853101496,-0.190408271679788,
7.86122670826915));
#62068=CARTESIAN_POINT('Ctrl Pts',(-2.26703071089283,-1.16154754141212,
7.92652848829996));
#62069=CARTESIAN_POINT('Ctrl Pts',(-0.9330321424437,-2.63859476601473,8.04449523199746));
#62070=CARTESIAN_POINT('Ctrl Pts',(1.70002224901497,-2.22320841823872,8.2024901229975));
#62071=CARTESIAN_POINT('Ctrl Pts',(2.79088864512093,0.208978201275766,8.36048501399757));
#62072=CARTESIAN_POINT('Ctrl Pts',(1.34997937336987,2.45158867054595,8.51847990499762));
#62073=CARTESIAN_POINT('Ctrl Pts',(-1.31557386100644,2.47022200101732,8.67647479599767));
#62074=CARTESIAN_POINT('Ctrl Pts',(-2.34084261733164,0.922522196646213,
8.78651145830014));
#62075=CARTESIAN_POINT('Ctrl Pts',(-2.37522208450983,0.0710785316625285,
8.84388315693593));
#62076=CARTESIAN_POINT('Ctrl Pts',(-2.3747901511292,0.00119133359606537,
8.84858989190503));
#62077=CARTESIAN_POINT('Origin',(0.,0.,-1.84858989190501));
#62078=CARTESIAN_POINT('',(-2.37396076251026,0.0016408096299993,6.65141010809499));
#62079=CARTESIAN_POINT('',(-2.36824488832617,0.00085307042009708,6.84858989190503));
#62080=CARTESIAN_POINT('',(-2.37175,-2.62313128856983E-13,-1.84858989190501));
#62081=CARTESIAN_POINT('Ctrl Pts',(-2.37396076251026,0.00164080962999946,
6.65141010809499));
#62082=CARTESIAN_POINT('Ctrl Pts',(-2.36860111288507,-0.675161988858878,
6.69694933132258));
#62083=CARTESIAN_POINT('Ctrl Pts',(-1.71220786555833,-2.14309654094568,
6.79510892492056));
#62084=CARTESIAN_POINT('Ctrl Pts',(0.771789132562049,-2.68935864031417,
6.94588888888888));
#62085=CARTESIAN_POINT('Ctrl Pts',(2.67339522049833,-0.825388609316905,
7.10375));
#62086=CARTESIAN_POINT('Ctrl Pts',(2.15357369271338,1.7861771220756,7.26161111111111));
#62087=CARTESIAN_POINT('Ctrl Pts',(-0.3168471224657,2.77991299546561,7.41947222222222));
#62088=CARTESIAN_POINT('Ctrl Pts',(-2.11399942046796,1.52539245310181,7.54940522121685));
#62089=CARTESIAN_POINT('Ctrl Pts',(-2.36856127073871,0.369714310321545,
7.62671784984111));
#62090=CARTESIAN_POINT('Ctrl Pts',(-2.36801892187683,0.000385579322849869,
7.65141010809499));
#62091=CARTESIAN_POINT('Ctrl Pts',(-2.36824488832617,0.000853070420097184,
6.84858989190503));
#62092=CARTESIAN_POINT('Ctrl Pts',(-2.36678180876479,-0.447463537758943,
6.87857025960238));
#62093=CARTESIAN_POINT('Ctrl Pts',(-2.02943011823198,-1.68535627820218,
6.96121559096642));
#62094=CARTESIAN_POINT('Ctrl Pts',(-0.0362940343214689,-2.79846637663312,
7.09652588599712));
#62095=CARTESIAN_POINT('Ctrl Pts',(2.32391314315961,-1.55953807940794,7.2545207769972));
#62096=CARTESIAN_POINT('Ctrl Pts',(2.57596499873257,1.09413693995685,7.41251566799723));
#62097=CARTESIAN_POINT('Ctrl Pts',(0.491210792034311,2.75525738831465,7.5705105589973));
#62098=CARTESIAN_POINT('Ctrl Pts',(-1.83676464589149,1.98397717256952,7.71586863363322));
#62099=CARTESIAN_POINT('Ctrl Pts',(-2.36622439910258,0.594323617306658,
7.80856174460247));
#62100=CARTESIAN_POINT('Ctrl Pts',(-2.37158591103805,-0.002113965830532,
7.84858989190503));
#62101=CARTESIAN_POINT('Origin',(0.,0.,-1.84858989190501));
#62102=CARTESIAN_POINT('',(-2.37251499866524,-0.00203510706959473,5.65141010809499));
#62103=CARTESIAN_POINT('',(-2.37459246787895,0.00132584644941116,5.84858989190502));
#62104=CARTESIAN_POINT('',(-2.37175,-2.62313128856983E-13,-1.84858989190501));
#62105=CARTESIAN_POINT('Ctrl Pts',(-2.37251499866524,-0.00203510706959476,
5.65141010809499));
#62106=CARTESIAN_POINT('Ctrl Pts',(-2.37392982983489,-0.158778764602934,
5.66194007206332));
#62107=CARTESIAN_POINT('Ctrl Pts',(-2.28863365792017,-1.09727074999648,
5.72509040640203));
#62108=CARTESIAN_POINT('Ctrl Pts',(-1.03894725747156,-2.59786392206505,
5.84086111111111));
#62109=CARTESIAN_POINT('Ctrl Pts',(1.60611030100396,-2.29100808867664,5.99872222222222));
#62110=CARTESIAN_POINT('Ctrl Pts',(2.79643351757374,0.090928230838667,6.15658333333333));
#62111=CARTESIAN_POINT('Ctrl Pts',(1.45388718569001,2.39050630885174,6.31444444444444));
#62112=CARTESIAN_POINT('Ctrl Pts',(-1.20551740739643,2.52488339173069,6.47230555555556));
#62113=CARTESIAN_POINT('Ctrl Pts',(-2.3208356274226,0.99330351170231,6.58462744343907));
#62114=CARTESIAN_POINT('Ctrl Pts',(-2.37479416424485,0.106880641648857,
6.64432896095221));
#62115=CARTESIAN_POINT('Ctrl Pts',(-2.37396076251026,0.00164080962999946,
6.65141010809499));
#62116=CARTESIAN_POINT('Ctrl Pts',(-2.37459246787895,0.00132584644941126,
5.84858989190502));
#62117=CARTESIAN_POINT('Ctrl Pts',(-2.3698592307678,-0.701510136856058,
5.8959138109356));
#62118=CARTESIAN_POINT('Ctrl Pts',(-1.6684907359976,-2.19471791424095,5.99590269363287));
#62119=CARTESIAN_POINT('Ctrl Pts',(0.864288593995119,-2.66190468356086,
6.14855653999681));
#62120=CARTESIAN_POINT('Ctrl Pts',(2.70163876039796,-0.730670463607777,
6.30655143099686));
#62121=CARTESIAN_POINT('Ctrl Pts',(2.08817696449889,1.86339697407977,6.46454632199692));
#62122=CARTESIAN_POINT('Ctrl Pts',(-0.419590302218696,2.76706980330411,
6.62254121299697));
#62123=CARTESIAN_POINT('Ctrl Pts',(-2.14308835195883,1.46541542002878,6.75055573629967));
#62124=CARTESIAN_POINT('Ctrl Pts',(-2.36935192507288,0.340071095547311,
6.82590529593569));
#62125=CARTESIAN_POINT('Ctrl Pts',(-2.36824488832617,0.000853070420097184,
6.84858989190503));
#62126=CARTESIAN_POINT('Origin',(0.,0.,-1.84858989190501));
#62127=CARTESIAN_POINT('',(-2.36803551809634,0.000435659979227324,4.65141010809499));
#62128=CARTESIAN_POINT('',(-2.37186713520955,-0.00210673407030348,4.84858989190502));
#62129=CARTESIAN_POINT('',(-2.37175,-2.62313128856983E-13,-1.84858989190501));
#62130=CARTESIAN_POINT('Ctrl Pts',(-2.36803551809634,0.000435659979227676,
4.65141010809499));
#62131=CARTESIAN_POINT('Ctrl Pts',(-2.36733685507668,-0.420470574046625,
4.67955118317444));
#62132=CARTESIAN_POINT('Ctrl Pts',(-2.06020439223756,-1.62937224150312,
4.76031262862425));
#62133=CARTESIAN_POINT('Ctrl Pts',(-0.135586668767159,-2.79462423533096,
4.89369444444444));
#62134=CARTESIAN_POINT('Ctrl Pts',(2.2650598786042,-1.64250178316317,5.05155555555556));
#62135=CARTESIAN_POINT('Ctrl Pts',(2.61412853009539,0.997316594419356,5.20941666666666));
#62136=CARTESIAN_POINT('Ctrl Pts',(0.595450368366912,2.73381550588105,5.36727777777778));
#62137=CARTESIAN_POINT('Ctrl Pts',(-1.79192767962886,2.0434990191552,5.51460892492054));
#62138=CARTESIAN_POINT('Ctrl Pts',(-2.36685963088812,0.624501153297232,
5.60931970169295));
#62139=CARTESIAN_POINT('Ctrl Pts',(-2.37251499866524,-0.00203510706959476,
5.65141010809499));
#62140=CARTESIAN_POINT('Ctrl Pts',(-2.37186713520955,-0.00210673407030307,
4.84858989190502));
#62141=CARTESIAN_POINT('Ctrl Pts',(-2.37348726775032,-0.180895246540068,
4.86059239860214));
#62142=CARTESIAN_POINT('Ctrl Pts',(-2.27367886126175,-1.14238681798702,
4.92525986896595));
#62143=CARTESIAN_POINT('Ctrl Pts',(-0.964512940920624,-2.62725067416123,
5.04259230299644));
#62144=CARTESIAN_POINT('Ctrl Pts',(1.67331967629405,-2.24337526486265,5.20058719399648));
#62145=CARTESIAN_POINT('Ctrl Pts',(2.79318773824162,0.175594923072764,5.35858208499656));
#62146=CARTESIAN_POINT('Ctrl Pts',(1.37919449268132,2.43527285317938,5.51657697599659));
#62147=CARTESIAN_POINT('Ctrl Pts',(-1.28594543116668,2.48577466117395,5.67457186699666));
#62148=CARTESIAN_POINT('Ctrl Pts',(-2.33566190719347,0.94159330950118,5.78524283896613));
#62149=CARTESIAN_POINT('Ctrl Pts',(-2.37512666773395,0.0806489125773547,
5.84324884726892));
#62150=CARTESIAN_POINT('Ctrl Pts',(-2.37459246787895,0.00132584644941126,
5.84858989190502));
#62151=CARTESIAN_POINT('Origin',(0.,0.,-1.84858989190501));
#62152=CARTESIAN_POINT('',(-2.37404189208837,0.00160568163382189,3.65141010809499));
#62153=CARTESIAN_POINT('',(-2.36815046112586,0.00071106261527204,3.84858989190502));
#62154=CARTESIAN_POINT('',(-2.37175,-2.62313128856983E-13,-1.84858989190501));
#62155=CARTESIAN_POINT('Ctrl Pts',(-2.37404189208837,0.0016056816338219,
3.65141010809499));
#62156=CARTESIAN_POINT('Ctrl Pts',(-2.36874097406567,-0.678301390146093,
3.69716229428555));
#62157=CARTESIAN_POINT('Ctrl Pts',(-1.70710264047504,-2.14919504149034,
3.79553485084648));
#62158=CARTESIAN_POINT('Ctrl Pts',(0.782578662553965,-2.68623882063674,
3.94652777777777));
#62159=CARTESIAN_POINT('Ctrl Pts',(2.67668699402767,-0.814650291328897,
4.10438888888889));
#62160=CARTESIAN_POINT('Ctrl Pts',(2.14638618582228,1.79480770611467,4.26225));
#62161=CARTESIAN_POINT('Ctrl Pts',(-0.328003825581952,2.77861869501174,
4.42011111111111));
#62162=CARTESIAN_POINT('Ctrl Pts',(-2.1171683957745,1.51896204170615,4.54983114714277));
#62163=CARTESIAN_POINT('Ctrl Pts',(-2.3686432695173,0.366572631058683,4.62693081280407));
#62164=CARTESIAN_POINT('Ctrl Pts',(-2.36803551809634,0.000435659979227676,
4.65141010809499));
#62165=CARTESIAN_POINT('Ctrl Pts',(-2.36815046112586,0.000711062615271901,
3.84858989190502));
#62166=CARTESIAN_POINT('Ctrl Pts',(-2.36695951468436,-0.438164069114789,
3.87793594993537));
#62167=CARTESIAN_POINT('Ctrl Pts',(-2.04015506879268,-1.66630099353556,
3.9599469716324));
#62168=CARTESIAN_POINT('Ctrl Pts',(-0.0697503817448946,-2.79783241149437,
4.09462295699612));
#62169=CARTESIAN_POINT('Ctrl Pts',(2.30510093209087,-1.58721170953314,4.25261784799616));
#62170=CARTESIAN_POINT('Ctrl Pts',(2.5888625630092,1.06326005653742,4.41061273899623));
#62171=CARTESIAN_POINT('Ctrl Pts',(0.524118009051023,2.74918744918107,4.56860762999628));
#62172=CARTESIAN_POINT('Ctrl Pts',(-1.82311086019465,2.00255204277458,4.71460001429921));
#62173=CARTESIAN_POINT('Ctrl Pts',(-2.36637840094874,0.603598422228309,
4.80792743493546));
#62174=CARTESIAN_POINT('Ctrl Pts',(-2.37186713520955,-0.00210673407030307,
4.84858989190502));
#62175=CARTESIAN_POINT('Origin',(0.,0.,-1.84858989190501));
#62176=CARTESIAN_POINT('',(-2.37242086931256,-0.00204814969984112,2.65141010809499));
#62177=CARTESIAN_POINT('',(-2.37437841508221,0.00145143062880153,2.84858989190502));
#62178=CARTESIAN_POINT('',(-2.37175,-2.62313128856983E-13,-1.84858989190501));
#62179=CARTESIAN_POINT('Ctrl Pts',(-2.37242086931256,-0.00204814969984169,
2.65141010809499));
#62180=CARTESIAN_POINT('Ctrl Pts',(-2.37386724785776,-0.161978223542019,
2.66215303502629));
#62181=CARTESIAN_POINT('Ctrl Pts',(-2.28652040521148,-1.10369798895945,
2.72551633232796));
#62182=CARTESIAN_POINT('Ctrl Pts',(-1.02851040967351,-2.60201352259292,
2.84149999999999));
#62183=CARTESIAN_POINT('Ctrl Pts',(1.61529402596567,-2.28454233775194,2.99936111111111));
#62184=CARTESIAN_POINT('Ctrl Pts',(2.79604598097933,0.102153087721166,3.15722222222222));
#62185=CARTESIAN_POINT('Ctrl Pts',(1.44427938842878,2.39632330140064,3.31508333333333));
#62186=CARTESIAN_POINT('Ctrl Pts',(-1.21564319790733,2.5200238088076,3.47294444444445));
#62187=CARTESIAN_POINT('Ctrl Pts',(-2.32270131739363,0.986891451715146,
3.58505336936499));
#62188=CARTESIAN_POINT('Ctrl Pts',(-2.37483765037521,0.103671339757588,
3.64454192391517));
#62189=CARTESIAN_POINT('Ctrl Pts',(-2.37404189208837,0.0016056816338219,
3.65141010809499));
#62190=CARTESIAN_POINT('Ctrl Pts',(-2.37437841508221,0.00145143062880148,
2.84858989190502));
#62191=CARTESIAN_POINT('Ctrl Pts',(-2.36936657242201,-0.69212851464997,
2.89527950126859));
#62192=CARTESIAN_POINT('Ctrl Pts',(-1.68411161328175,-2.17667922631145,
2.99463407429885));
#62193=CARTESIAN_POINT('Ctrl Pts',(0.832400628534772,-2.67204800324426,
3.1466536109958));
#62194=CARTESIAN_POINT('Ctrl Pts',(2.69270963387839,-0.762919488957052,
3.30464850199585));
#62195=CARTESIAN_POINT('Ctrl Pts',(2.11030679852043,1.83829718168443,3.4626433929959));
#62196=CARTESIAN_POINT('Ctrl Pts',(-0.386476751895552,2.77188871376435,
3.62063828399595));
#62197=CARTESIAN_POINT('Ctrl Pts',(-2.13403081733917,1.48458669705641,3.74928711696566));
#62198=CARTESIAN_POINT('Ctrl Pts',(-2.36909680859298,0.349449137499666,
3.82527098626868));
#62199=CARTESIAN_POINT('Ctrl Pts',(-2.36815046112586,0.000711062615271901,
3.84858989190502));
#62200=CARTESIAN_POINT('Origin',(0.,0.,-1.84858989190501));
#62201=CARTESIAN_POINT('',(-2.36805372255214,0.000487775483918624,1.65141010809499));
#62202=CARTESIAN_POINT('',(-2.37214954248261,-0.00208751672060303,1.84858989190502));
#62203=CARTESIAN_POINT('',(-2.37175,-2.62313128856983E-13,-1.84858989190501));
#62204=CARTESIAN_POINT('Ctrl Pts',(-2.36805372255214,0.000487775483918769,
1.65141010809499));
#62205=CARTESIAN_POINT('Ctrl Pts',(-2.36726911244657,-0.423596588857836,
1.6797641461374));
#62206=CARTESIAN_POINT('Ctrl Pts',(-2.0567282222087,-1.63578530702029,1.76073855455018));
#62207=CARTESIAN_POINT('Ctrl Pts',(-0.124366744542119,-2.79514315034066,
1.89433333333333));
#62208=CARTESIAN_POINT('Ctrl Pts',(2.27163476293377,-1.63339753074864,2.05219444444444));
#62209=CARTESIAN_POINT('Ctrl Pts',(2.61010413592219,1.00780309522069,2.21005555555555));
#62210=CARTESIAN_POINT('Ctrl Pts',(0.584471286669745,2.73618335546233,2.36791666666667));
#62211=CARTESIAN_POINT('Ctrl Pts',(-1.79666946585791,2.03730116384381,2.51503485084647));
#62212=CARTESIAN_POINT('Ctrl Pts',(-2.36678268187025,0.621381820955435,
2.60953266465592));
#62213=CARTESIAN_POINT('Ctrl Pts',(-2.37242086931256,-0.00204814969984169,
2.65141010809499));
#62214=CARTESIAN_POINT('Ctrl Pts',(-2.37214954248261,-0.00208751672060286,
1.84858989190502));
#62215=CARTESIAN_POINT('Ctrl Pts',(-2.37368814589582,-0.171375740131997,
1.85995808893514));
#62216=CARTESIAN_POINT('Ctrl Pts',(-2.28019409230745,-1.12323247312203,
1.92399124963194));
#62217=CARTESIAN_POINT('Ctrl Pts',(-0.995855715555496,-2.61553061219188,
2.04068937399542));
#62218=CARTESIAN_POINT('Ctrl Pts',(1.64637781974439,-2.26322161422709,2.19868426499547));
#62219=CARTESIAN_POINT('Ctrl Pts',(2.79508756969503,0.142186649832604,2.35667915599553));
#62220=CARTESIAN_POINT('Ctrl Pts',(1.40821242874264,2.41860884498944,2.51467404699558));
#62221=CARTESIAN_POINT('Ctrl Pts',(-1.25613315819632,2.50097199645567,2.67266893799564));
#62222=CARTESIAN_POINT('Ctrl Pts',(-2.33035893824447,0.960673681793537,
2.78397421963211));
#62223=CARTESIAN_POINT('Ctrl Pts',(-2.37501983264844,0.0902160608552179,
2.84261453760191));
#62224=CARTESIAN_POINT('Ctrl Pts',(-2.37437841508221,0.00145143062880148,
2.84858989190502));
#62225=CARTESIAN_POINT('Origin',(0.,0.,-1.84858989190501));
#62226=CARTESIAN_POINT('',(-2.37409249406917,0.00172857025301859,0.651410108094985));
#62227=CARTESIAN_POINT('',(-2.36806791026422,0.000580996437929415,0.848589891905023));
#62228=CARTESIAN_POINT('',(-2.37175,-2.62313128856983E-13,-1.84858989190501));
#62229=CARTESIAN_POINT('Ctrl Pts',(-2.37409249406917,0.00172857025301858,
0.651410108094986));
#62230=CARTESIAN_POINT('Ctrl Pts',(-2.36885059157359,-0.681255271864669,
0.697375257248508));
#62231=CARTESIAN_POINT('Ctrl Pts',(-1.70202128243095,-2.15553453151225,
0.7959607767724));
#62232=CARTESIAN_POINT('Ctrl Pts',(0.793380919254056,-2.68293732976497,
0.947166666666663));
#62233=CARTESIAN_POINT('Ctrl Pts',(2.67992237177449,-0.803971281251394,
1.10502777777777));
#62234=CARTESIAN_POINT('Ctrl Pts',(2.13917103413275,1.80344728451176,1.26288888888888));
#62235=CARTESIAN_POINT('Ctrl Pts',(-0.339158877291603,2.77725977180218,
1.42075));
#62236=CARTESIAN_POINT('Ctrl Pts',(-2.12031894951391,1.51253569372851,1.5502570730687));
#62237=CARTESIAN_POINT('Ctrl Pts',(-2.36872521807391,0.363433332120877,
1.62714377576703));
#62238=CARTESIAN_POINT('Ctrl Pts',(-2.36805372255214,0.000487775483918769,
1.65141010809499));
#62239=CARTESIAN_POINT('Ctrl Pts',(-2.36806791026422,0.000580996437929554,
0.848589891905023));
#62240=CARTESIAN_POINT('Ctrl Pts',(-2.36714590954407,-0.428850691797627,
0.877301640268363));
#62241=CARTESIAN_POINT('Ctrl Pts',(-2.05072593975983,-1.64725737587436,
0.958678352298389));
#62242=CARTESIAN_POINT('Ctrl Pts',(-0.103189861818606,-2.79677945469355,
1.0927200279951));
#62243=CARTESIAN_POINT('Ctrl Pts',(2.28595558559378,-1.6146683983646,1.25071491899515));
#62244=CARTESIAN_POINT('Ctrl Pts',(2.60139192527736,1.0322363870214,1.4087098099952));
#62245=CARTESIAN_POINT('Ctrl Pts',(0.556949311928898,2.7427217714679,1.56670470099526));
#62246=CARTESIAN_POINT('Ctrl Pts',(-1.80927361374524,2.02108563130788,1.7133313949652));
#62247=CARTESIAN_POINT('Ctrl Pts',(-2.36656032319539,0.612878624174093,
1.80729312526845));
#62248=CARTESIAN_POINT('Ctrl Pts',(-2.37214954248261,-0.00208751672060286,
1.84858989190502));
#62249=CARTESIAN_POINT('Origin',(0.,0.,15.5));
#62250=CARTESIAN_POINT('',(-2.86987326377042,0.00104132824445593,15.1339652973708));
#62251=CARTESIAN_POINT('Ctrl Pts',(-0.439445221994174,2.33068358199188,
15.62825));
#62252=CARTESIAN_POINT('Ctrl Pts',(-0.359491362851287,2.34930954683752,
15.6247606402091));
#62253=CARTESIAN_POINT('Ctrl Pts',(-0.27873128971825,2.36341107797762,15.6212855109979));
#62254=CARTESIAN_POINT('Ctrl Pts',(-0.197490043658781,2.37317361481181,
15.6178198845782));
#62255=CARTESIAN_POINT('Ctrl Pts',(-0.114097433923979,2.38319467509491,
15.6142624842978));
#62256=CARTESIAN_POINT('Ctrl Pts',(-0.0301970746788968,2.38864392614809,
15.610715096763));
#62257=CARTESIAN_POINT('Ctrl Pts',(0.0538748377108959,2.38966967391038,
15.6071726085593));
#62258=CARTESIAN_POINT('Ctrl Pts',(0.0936167287327529,2.39015455827456,
15.6054980281181));
#62259=CARTESIAN_POINT('Ctrl Pts',(0.133397101437596,2.38965022998153,15.6038245424699));
#62260=CARTESIAN_POINT('Ctrl Pts',(0.17318082101162,2.38816842541213,15.6021516114778));
#62261=CARTESIAN_POINT('Ctrl Pts',(0.19744268730314,2.38726475565179,15.601131384398));
#62262=CARTESIAN_POINT('Ctrl Pts',(0.221705799792773,2.38599750448324,15.6001113636003));
#62263=CARTESIAN_POINT('Ctrl Pts',(0.245962166148401,2.38436888753973,15.5990914265778));
#62264=CARTESIAN_POINT('Ctrl Pts',(0.26185491634123,2.38330181913124,15.5984231647255));
#62265=CARTESIAN_POINT('Ctrl Pts',(0.277745619245824,2.38207945021967,15.597754902985));
#62266=CARTESIAN_POINT('Ctrl Pts',(0.293615508622687,2.38070402970992,15.5970873017022));
#62267=CARTESIAN_POINT('Ctrl Pts',(0.379355905904818,2.37327303267301,15.5934804461119));
#62268=CARTESIAN_POINT('Ctrl Pts',(0.46460122999168,2.36137220783444,15.5898881158652));
#62269=CARTESIAN_POINT('Ctrl Pts',(0.548999070996607,2.3451645872232,15.5863050764217));
#62270=CARTESIAN_POINT('Ctrl Pts',(0.634137600151781,2.32881472609505,15.582690591685));
#62271=CARTESIAN_POINT('Ctrl Pts',(0.718414656351904,2.30808199543454,15.5790855615419));
#62272=CARTESIAN_POINT('Ctrl Pts',(0.801467682213623,2.28308069981211,15.5754846124216));
#62273=CARTESIAN_POINT('Ctrl Pts',(0.852459500288906,2.26773072905791,15.573273748452));
#62274=CARTESIAN_POINT('Ctrl Pts',(0.902989840792886,2.2507706713731,15.5710644228464));
#62275=CARTESIAN_POINT('Ctrl Pts',(0.952972256247749,2.23221757070223,15.5688553919549));
#62276=CARTESIAN_POINT('Ctrl Pts',(0.964785636442244,2.22783253188374,15.5683332858993));
#62277=CARTESIAN_POINT('Ctrl Pts',(0.976567164733754,2.22335887755768,15.5678112499871));
#62278=CARTESIAN_POINT('Ctrl Pts',(0.98830665315667,2.21880049805757,15.5672896716409));
#62279=CARTESIAN_POINT('Ctrl Pts',(1.07009362440554,2.18704306198486,15.5636559261431));
#62280=CARTESIAN_POINT('Ctrl Pts',(1.14996182974845,2.15113305037133,15.5600390318413));
#62281=CARTESIAN_POINT('Ctrl Pts',(1.22755227573139,2.11121890826833,15.5564336755567));
#62282=CARTESIAN_POINT('Ctrl Pts',(1.30476387614222,2.07149965222131,15.552845922899));
#62283=CARTESIAN_POINT('Ctrl Pts',(1.37972085381243,2.02781498993708,15.5492695958616));
#62284=CARTESIAN_POINT('Ctrl Pts',(1.45205674723287,1.98026157738062,15.5456994587133));
#62285=CARTESIAN_POINT('Ctrl Pts',(1.51163119176407,1.94109750537355,15.5427591627211));
#62286=CARTESIAN_POINT('Ctrl Pts',(1.56942781249227,1.89930836286272,15.5398230652386));
#62287=CARTESIAN_POINT('Ctrl Pts',(1.62522850219512,1.85492460083693,15.5368882414682));
#62288=CARTESIAN_POINT('Ctrl Pts',(1.65312884704655,1.83273271982404,15.5354208295831));
#62289=CARTESIAN_POINT('Ctrl Pts',(1.68052998038672,1.80989186082895,15.5339537361259));
#62290=CARTESIAN_POINT('Ctrl Pts',(1.70740302888556,1.78640394209333,15.532486595497));
#62291=CARTESIAN_POINT('Ctrl Pts',(1.72592667853778,1.77021366960761,15.5314752923321));
#62292=CARTESIAN_POINT('Ctrl Pts',(1.74419939199006,1.753715928893,15.5304639667541));
#62293=CARTESIAN_POINT('Ctrl Pts',(1.76221135665739,1.73691101229318,15.5294524990243));
#62294=CARTESIAN_POINT('Ctrl Pts',(1.77033011726031,1.72933631972932,15.528996587384));
#62295=CARTESIAN_POINT('Ctrl Pts',(1.77839409985328,1.72170084478485,15.5285407465195));
#62296=CARTESIAN_POINT('Ctrl Pts',(1.78639747681482,1.71400960641012,15.5280852527741));
#62297=CARTESIAN_POINT('Ctrl Pts',(1.84657495109044,1.65617910540199,15.5246603905846));
#62298=CARTESIAN_POINT('Ctrl Pts',(1.90341295390484,1.59512114682347,15.5212504095826));
#62299=CARTESIAN_POINT('Ctrl Pts',(1.95689046613085,1.53122773141625,15.5178508639384));
#62300=CARTESIAN_POINT('Ctrl Pts',(2.01194103421405,1.46545487347031,15.5143513197161));
#62301=CARTESIAN_POINT('Ctrl Pts',(2.06343093897923,1.39667671283205,15.5108628337987));
#62302=CARTESIAN_POINT('Ctrl Pts',(2.11130423046702,1.3252770563036,15.507380556377));
#62303=CARTESIAN_POINT('Ctrl Pts',(2.15745742078722,1.25644281002257,15.5040233981871));
#62304=CARTESIAN_POINT('Ctrl Pts',(2.20024928268006,1.18517117106803,15.500672010362));
#62305=CARTESIAN_POINT('Ctrl Pts',(2.23959635988792,1.11177753196584,15.4973220472993));
#62306=CARTESIAN_POINT('Ctrl Pts',(2.25681070616636,1.07966781485864,15.4958564384594));
#62307=CARTESIAN_POINT('Ctrl Pts',(2.27336525378777,1.04715163497876,15.4943911023279));
#62308=CARTESIAN_POINT('Ctrl Pts',(2.28925084670373,1.0142542353915,15.4929256750031));
#62309=CARTESIAN_POINT('Ctrl Pts',(2.29885484868501,0.994365352899876,15.4920397170785));
#62310=CARTESIAN_POINT('Ctrl Pts',(2.30821431569525,0.974337119524171,15.491153725822));
#62311=CARTESIAN_POINT('Ctrl Pts',(2.3173269757796,0.954175024263046,15.4902676208197));
#62312=CARTESIAN_POINT('Ctrl Pts',(2.32227232757467,0.943233251710468,15.4897867402729));
#62313=CARTESIAN_POINT('Ctrl Pts',(2.32714420559321,0.932253683866113,15.4893058986854));
#62314=CARTESIAN_POINT('Ctrl Pts',(2.33193873109372,0.921245710398884,15.4888254510349));
#62315=CARTESIAN_POINT('Ctrl Pts',(2.36754247444614,0.839501424730483,15.4852576871677));
#62316=CARTESIAN_POINT('Ctrl Pts',(2.39894281260828,0.756064329075142,15.4817059560376));
#62317=CARTESIAN_POINT('Ctrl Pts',(2.42608268559146,0.671340103595013,15.4781652340513));
#62318=CARTESIAN_POINT('Ctrl Pts',(2.453534139292,0.58564319725637,15.4745838626229));
#62319=CARTESIAN_POINT('Ctrl Pts',(2.47662715562456,0.498628540954889,15.4710137545713));
#62320=CARTESIAN_POINT('Ctrl Pts',(2.49525785992387,0.410687466692489,15.4674497112883));
#62321=CARTESIAN_POINT('Ctrl Pts',(2.51258257274376,0.328910963121187,15.4641355034428));
#62322=CARTESIAN_POINT('Ctrl Pts',(2.52604844140045,0.24633247953868,15.4608265399003));
#62323=CARTESIAN_POINT('Ctrl Pts',(2.53553303361489,0.163255416668028,15.4575186404574));
#62324=CARTESIAN_POINT('Ctrl Pts',(2.53942998139287,0.129121426694033,15.4561595191486));
#62325=CARTESIAN_POINT('Ctrl Pts',(2.54265436806282,0.0949032017028567,
15.4548005774761));
#62326=CARTESIAN_POINT('Ctrl Pts',(2.54519570834653,0.0606216731012661,
15.4534415254952));
#62327=CARTESIAN_POINT('Ctrl Pts',(2.54650804671318,0.0429188233335401,
15.4527397162695));
#62328=CARTESIAN_POINT('Ctrl Pts',(2.5476382209856,0.0251990932110098,15.4520378776284));
#62329=CARTESIAN_POINT('Ctrl Pts',(2.54858465973821,0.00746537430393359,
15.4513359696452));
#62330=CARTESIAN_POINT('Ctrl Pts',(2.54936740774304,-0.00720121986763361,
15.4507554597369));
#62331=CARTESIAN_POINT('Ctrl Pts',(2.55002444266908,-0.0218786230829287,
15.4501748534934));
#62332=CARTESIAN_POINT('Ctrl Pts',(2.55055443165925,-0.0365475000712079,
15.4495948274855));
#62333=CARTESIAN_POINT('Ctrl Pts',(2.55387898415761,-0.128563471239416,
15.4459563992365));
#62334=CARTESIAN_POINT('Ctrl Pts',(2.55221836548087,-0.22040066645441,15.4423345418383));
#62335=CARTESIAN_POINT('Ctrl Pts',(2.5454697064449,-0.311650010793409,15.4387239299593));
#62336=CARTESIAN_POINT('Ctrl Pts',(2.53872104740894,-0.402899355132408,
15.4351133180804));
#62337=CARTESIAN_POINT('Ctrl Pts',(2.52688470709894,-0.49356189746232,15.4315139517205));
#62338=CARTESIAN_POINT('Ctrl Pts',(2.50980235603637,-0.583236219097685,
15.4279205055482));
#62339=CARTESIAN_POINT('Ctrl Pts',(2.49326213150481,-0.670064631014266,
15.424441101202));
#62340=CARTESIAN_POINT('Ctrl Pts',(2.47180332144007,-0.755967381987536,
15.420967247239));
#62341=CARTESIAN_POINT('Ctrl Pts',(2.44569482135312,-0.840684658565203,
15.4174941094224));
#62342=CARTESIAN_POINT('Ctrl Pts',(2.43658807165331,-0.870234384917672,
15.4162826650015));
#62343=CARTESIAN_POINT('Ctrl Pts',(2.42691516765274,-0.899639766052948,
15.41507130771));
#62344=CARTESIAN_POINT('Ctrl Pts',(2.41668612527745,-0.928889320342703,
15.4138598323975));
#62345=CARTESIAN_POINT('Ctrl Pts',(2.41079789512425,-0.945726488595391,
15.4131624606198));
#62346=CARTESIAN_POINT('Ctrl Pts',(2.40472537046329,-0.962512016907764,
15.4124650497348));
#62347=CARTESIAN_POINT('Ctrl Pts',(2.39847036187175,-0.979243667871416,
15.4117675606113));
#62348=CARTESIAN_POINT('Ctrl Pts',(2.39421301098727,-0.990631743201221,
15.4112928281));
#62349=CARTESIAN_POINT('Ctrl Pts',(2.38987156242605,-1.0019935463669,15.4108181134517));
#62350=CARTESIAN_POINT('Ctrl Pts',(2.38545028303317,-1.01331939423191,15.4103437824454));
#62351=CARTESIAN_POINT('Ctrl Pts',(2.35279097735238,-1.09698167717045,15.4068399728119));
#62352=CARTESIAN_POINT('Ctrl Pts',(2.31572987674733,-1.17881857921774,15.4033514296728));
#62353=CARTESIAN_POINT('Ctrl Pts',(2.27459874133947,-1.25857844945699,15.3998733992833));
#62354=CARTESIAN_POINT('Ctrl Pts',(2.23281288372258,-1.33960793109688,15.396340005877));
#62355=CARTESIAN_POINT('Ctrl Pts',(2.18682594253521,-1.41849449977561,15.3928174625663));
#62356=CARTESIAN_POINT('Ctrl Pts',(2.13693151879332,-1.49496175096055,15.3893007849646));
#62357=CARTESIAN_POINT('Ctrl Pts',(2.08679723793274,-1.57179660263405,15.385767201663));
#62358=CARTESIAN_POINT('Ctrl Pts',(2.03271725897117,-1.64618961960946,15.3822395406022));
#62359=CARTESIAN_POINT('Ctrl Pts',(1.97494281786374,-1.71783598585985,15.3787127451654));
#62360=CARTESIAN_POINT('Ctrl Pts',(1.95216878512211,-1.74607817495815,15.3773225222016));
#62361=CARTESIAN_POINT('Ctrl Pts',(1.92882022676702,-1.77389324483966,15.3759324337425));
#62362=CARTESIAN_POINT('Ctrl Pts',(1.90491084697345,-1.80126106485015,15.3745421700657));
#62363=CARTESIAN_POINT('Ctrl Pts',(1.89303589564547,-1.8148537022746,15.3738516748025));
#62364=CARTESIAN_POINT('Ctrl Pts',(1.88102258946071,-1.82833599951471,15.3731611363172));
#62365=CARTESIAN_POINT('Ctrl Pts',(1.86887253021617,-1.84170540057035,15.3724705166642));
#62366=CARTESIAN_POINT('Ctrl Pts',(1.86055716973053,-1.85085526453538,15.3719978645349));
#62367=CARTESIAN_POINT('Ctrl Pts',(1.8521789913077,-1.85995082597714,15.3715252464369));
#62368=CARTESIAN_POINT('Ctrl Pts',(1.84374494253208,-1.86898463564396,15.3710530027583));
#62369=CARTESIAN_POINT('Ctrl Pts',(1.77862481272331,-1.93873557897155,15.3674067623267));
#62370=CARTESIAN_POINT('Ctrl Pts',(1.71007452953627,-2.00492197279666,15.3637769310107));
#62371=CARTESIAN_POINT('Ctrl Pts',(1.63841756617314,-2.06724394639147,15.3601581531957));
#62372=CARTESIAN_POINT('Ctrl Pts',(1.56864469297252,-2.1279272764847,15.3566345245939));
#62373=CARTESIAN_POINT('Ctrl Pts',(1.49592552744324,-2.18494739655425,15.3531213758712));
#62374=CARTESIAN_POINT('Ctrl Pts',(1.42051657448793,-2.237996979208,15.3496137628515));
#62375=CARTESIAN_POINT('Ctrl Pts',(1.34626553575621,-2.29023197866037,15.3461600096832));
#62376=CARTESIAN_POINT('Ctrl Pts',(1.26940602418092,-2.33861808827242,15.3427116235202));
#62377=CARTESIAN_POINT('Ctrl Pts',(1.19015227451303,-2.38282228508801,15.3392638844625));
#62378=CARTESIAN_POINT('Ctrl Pts',(1.16438136391748,-2.39719614637352,15.3381427845096));
#62379=CARTESIAN_POINT('Ctrl Pts',(1.1383570943619,-2.4111274748391,15.3370217529787));
#62380=CARTESIAN_POINT('Ctrl Pts',(1.11208629310672,-2.42460372067378,15.3359006275904));
#62381=CARTESIAN_POINT('Ctrl Pts',(1.09252404263768,-2.4346386523776,15.3350657944447));
#62382=CARTESIAN_POINT('Ctrl Pts',(1.07282508844486,-2.44442123549769,15.3342309092564));
#62383=CARTESIAN_POINT('Ctrl Pts',(1.05299217133848,-2.4539460706498,15.3333959050218));
#62384=CARTESIAN_POINT('Ctrl Pts',(1.04038456497523,-2.46000092237074,15.3328651003678));
#62385=CARTESIAN_POINT('Ctrl Pts',(1.02772285622574,-2.46595150778408,15.3323342505181));
#62386=CARTESIAN_POINT('Ctrl Pts',(1.01502087310116,-2.47179063085649,15.3318038822616));
#62387=CARTESIAN_POINT('Ctrl Pts',(0.982652722257195,-2.48667032440912,
15.3304523578927));
#62388=CARTESIAN_POINT('Ctrl Pts',(0.950002091670773,-2.50083650005249,
15.3291030741213));
#62389=CARTESIAN_POINT('Ctrl Pts',(0.917084170499721,-2.5142729570447,15.3277557583224));
#62390=CARTESIAN_POINT('Ctrl Pts',(0.834495683370104,-2.5479839757206,15.3243754484619));
#62391=CARTESIAN_POINT('Ctrl Pts',(0.750226663082229,-2.57710500546031,
15.3210075263739));
#62392=CARTESIAN_POINT('Ctrl Pts',(0.664646844355562,-2.60177034865307,
15.317647686521));
#62393=CARTESIAN_POINT('Ctrl Pts',(0.576787650214132,-2.6270926408521,15.3141983590239));
#62394=CARTESIAN_POINT('Ctrl Pts',(0.487546169865586,-2.64771888106776,
15.3107575500279));
#62395=CARTESIAN_POINT('Ctrl Pts',(0.397298853288816,-2.66374516605354,
15.3073206007236));
#62396=CARTESIAN_POINT('Ctrl Pts',(0.308910977458226,-2.67944124812091,
15.3039544657529));
#62397=CARTESIAN_POINT('Ctrl Pts',(0.219557440695963,-2.69072476824651,
15.3005920330634));
#62398=CARTESIAN_POINT('Ctrl Pts',(0.129581594551193,-2.69764046998944,
15.2972289259214));
#62399=CARTESIAN_POINT('Ctrl Pts',(0.0974227261046785,-2.7001122571645,
15.2960268953233));
#62400=CARTESIAN_POINT('Ctrl Pts',(0.0651843226484069,-2.70202565483482,
15.2948247785662));
#62401=CARTESIAN_POINT('Ctrl Pts',(0.0328820436324132,-2.7033813247538,
15.2936223758136));
#62402=CARTESIAN_POINT('Ctrl Pts',(0.0192199250543532,-2.70395469987624,
15.2931138244208));
#62403=CARTESIAN_POINT('Ctrl Pts',(0.00555605037576419,-2.70442788901379,
15.2926055817652));
#62404=CARTESIAN_POINT('Ctrl Pts',(-0.00810768527292701,-2.70480131817288,
15.2920976575977));
#62405=CARTESIAN_POINT('Ctrl Pts',(-0.102177189495074,-2.70737223265483,
15.2886007973064));
#62406=CARTESIAN_POINT('Ctrl Pts',(-0.196248953232544,-2.705219350857,15.2851186519246));
#62407=CARTESIAN_POINT('Ctrl Pts',(-0.28992790026966,-2.69846111693802,
15.2816464960614));
#62408=CARTESIAN_POINT('Ctrl Pts',(-0.384721183626751,-2.69162249200534,
15.2781330379685));
#62409=CARTESIAN_POINT('Ctrl Pts',(-0.479113197863739,-2.68006831395088,
15.2746298084638));
#62410=CARTESIAN_POINT('Ctrl Pts',(-0.572703609774366,-2.66386867615587,
15.2711319115131));
#62411=CARTESIAN_POINT('Ctrl Pts',(-0.670406973022026,-2.64695712438838,
15.2674802949704));
#62412=CARTESIAN_POINT('Ctrl Pts',(-0.767237930320469,-2.62498318167097,
15.2638344899723));
#62413=CARTESIAN_POINT('Ctrl Pts',(-0.862734200133818,-2.5979664405403,
15.2601889262148));
#62414=CARTESIAN_POINT('Ctrl Pts',(-0.899309423475345,-2.58761898568426,
15.258792669493));
#62415=CARTESIAN_POINT('Ctrl Pts',(-0.935688693950487,-2.57653116703875,
15.2573964481588));
#62416=CARTESIAN_POINT('Ctrl Pts',(-0.971845190453781,-2.56470173355219,
15.2559999492582));
#62417=CARTESIAN_POINT('Ctrl Pts',(-0.985718422450195,-2.56016278506391,
15.2554641132369));
#62418=CARTESIAN_POINT('Ctrl Pts',(-0.999558849945709,-2.55551463851664,
15.2549282363508));
#62419=CARTESIAN_POINT('Ctrl Pts',(-1.01336493152648,-2.55075717270086,
15.254392300921));
#62420=CARTESIAN_POINT('Ctrl Pts',(-1.02713823497804,-2.5460110019675,15.2538576378986));
#62421=CARTESIAN_POINT('Ctrl Pts',(-1.0408680078023,-2.54115923920241,15.2533232792799));
#62422=CARTESIAN_POINT('Ctrl Pts',(-1.05455083068562,-2.53620294641156,
15.2527892870021));
#62423=CARTESIAN_POINT('Ctrl Pts',(-1.14480706402235,-2.50350966941525,
15.2492669048126));
#62424=CARTESIAN_POINT('Ctrl Pts',(-1.23304972084596,-2.46626241239109,
15.2457593395817));
#62425=CARTESIAN_POINT('Ctrl Pts',(-1.3188786706842,-2.42453542284507,15.242261762893));
#62426=CARTESIAN_POINT('Ctrl Pts',(-1.40341018907482,-2.38343919842613,
15.238817057246));
#62427=CARTESIAN_POINT('Ctrl Pts',(-1.48560133565556,-2.33799743942912,
15.2353820404405));
#62428=CARTESIAN_POINT('Ctrl Pts',(-1.56505752288372,-2.28823266258407,
15.2319520997326));
#62429=CARTESIAN_POINT('Ctrl Pts',(-1.59875150777533,-2.26712954025155,
15.2304976079627));
#62430=CARTESIAN_POINT('Ctrl Pts',(-1.63195344745741,-2.24524844976825,
15.2290440290004));
#62431=CARTESIAN_POINT('Ctrl Pts',(-1.66463195977674,-2.22258855435451,
15.2275910110965));
#62432=CARTESIAN_POINT('Ctrl Pts',(-1.74176819837999,-2.16910083489293,
15.2241612241271));
#62433=CARTESIAN_POINT('Ctrl Pts',(-1.81599039866318,-2.11127647963352,
15.2207345632396));
#62434=CARTESIAN_POINT('Ctrl Pts',(-1.88715256813859,-2.04946422501414,
15.2173064022613));
#62435=CARTESIAN_POINT('Ctrl Pts',(-1.90164577925548,-2.03687526008497,
15.2166082074035));
#62436=CARTESIAN_POINT('Ctrl Pts',(-1.91601194648249,-2.02412075255685,
15.215909950323));
#62437=CARTESIAN_POINT('Ctrl Pts',(-1.9302496520377,-2.01120346334021,15.2152115919387));
#62438=CARTESIAN_POINT('Ctrl Pts',(-1.94128816753001,-2.0011886687103,15.2146701535858));
#62439=CARTESIAN_POINT('Ctrl Pts',(-1.95224352654855,-1.99108137253609,
15.2141289446068));
#62440=CARTESIAN_POINT('Ctrl Pts',(-1.96311133771197,-1.98088698275119,
15.2135881466736));
#62441=CARTESIAN_POINT('Ctrl Pts',(-2.03178675603926,-1.91646702066845,
15.2101707589647));
#62442=CARTESIAN_POINT('Ctrl Pts',(-2.09701995613675,-1.8485265277173,15.2067672577273));
#62443=CARTESIAN_POINT('Ctrl Pts',(-2.15871310631003,-1.77747212767664,
15.2033732357386));
#62444=CARTESIAN_POINT('Ctrl Pts',(-2.22164945390415,-1.7049858888237,15.1999108197811));
#62445=CARTESIAN_POINT('Ctrl Pts',(-2.28090217022322,-1.62925832538052,
15.19645826896));
#62446=CARTESIAN_POINT('Ctrl Pts',(-2.33633512040192,-1.55067589533689,
15.1930109042136));
#62447=CARTESIAN_POINT('Ctrl Pts',(-2.39218601791983,-1.47150097801918,
15.1895375474008));
#62448=CARTESIAN_POINT('Ctrl Pts',(-2.44415984798534,-1.38942718616138,
15.1860694551604));
#62449=CARTESIAN_POINT('Ctrl Pts',(-2.49207710040016,-1.30481547317471,
15.1826018417945));
#62450=CARTESIAN_POINT('Ctrl Pts',(-2.52022211747796,-1.25511733759765,
15.1805650798249));
#62451=CARTESIAN_POINT('Ctrl Pts',(-2.54696681998739,-1.20454303320315,
15.1785284830672));
#62452=CARTESIAN_POINT('Ctrl Pts',(-2.57226731600719,-1.15316195438398,
15.1764910817393));
#62453=CARTESIAN_POINT('Ctrl Pts',(-2.57933924906923,-1.13880004030214,
15.1759215922795));
#62454=CARTESIAN_POINT('Ctrl Pts',(-2.58629893239321,-1.12437358425022,
15.1753519825172));
#62455=CARTESIAN_POINT('Ctrl Pts',(-2.59313735551554,-1.10990147500019,
15.1747829112963));
#62456=CARTESIAN_POINT('Ctrl Pts',(-2.63517066423893,-1.02094666405867,
15.1712850367298));
#62457=CARTESIAN_POINT('Ctrl Pts',(-2.6726976453638,-0.930127060905838,
15.167801819036));
#62458=CARTESIAN_POINT('Ctrl Pts',(-2.70558302354023,-0.837840896222647,
15.1643285389057));
#62459=CARTESIAN_POINT('Ctrl Pts',(-2.73847376195491,-0.745539689114618,
15.1608546926391));
#62460=CARTESIAN_POINT('Ctrl Pts',(-2.76672184052432,-0.651770570287676,
15.1573907871758));
#62461=CARTESIAN_POINT('Ctrl Pts',(-2.79014819101862,-0.556903769359717,
15.1539321008988));
#62462=CARTESIAN_POINT('Ctrl Pts',(-2.81305355218475,-0.464146754627161,
15.1505503339286));
#62463=CARTESIAN_POINT('Ctrl Pts',(-2.83134952927604,-0.370339481518358,
15.1471735565822));
#62464=CARTESIAN_POINT('Ctrl Pts',(-2.8448219024633,-0.275813943398833,
15.1437973553073));
#62465=CARTESIAN_POINT('Ctrl Pts',(-2.85447686455589,-0.208072315799913,
15.1413778042102));
#62466=CARTESIAN_POINT('Ctrl Pts',(-2.86165354894421,-0.139961477196466,
15.1389585489751));
#62467=CARTESIAN_POINT('Ctrl Pts',(-2.86625656775569,-0.071602632167948,
15.1365379651471));
#62468=CARTESIAN_POINT('Ctrl Pts',(-2.8678889837078,-0.0473598311579388,
15.1356795285827));
#62469=CARTESIAN_POINT('Ctrl Pts',(-2.86919553394546,-0.0231160969724086,
15.1348219958471));
#62470=CARTESIAN_POINT('Ctrl Pts',(-2.87017396612668,0.00112290304428943,
15.1339652973708));
#62471=CARTESIAN_POINT('',(0.261080338132197,2.92584241055005,15.058));
#62472=CARTESIAN_POINT('Ctrl Pts',(0.260984867623723,2.92515103163649,15.058));
#62473=CARTESIAN_POINT('Ctrl Pts',(0.163110290089364,2.92129299518303,15.0703787026841));
#62474=CARTESIAN_POINT('Ctrl Pts',(0.0656985383021158,2.91278590387498,
15.0828015605825));
#62475=CARTESIAN_POINT('Ctrl Pts',(-0.0308724856851826,2.89964343902045,
15.0952881213498));
#62476=CARTESIAN_POINT('Ctrl Pts',(-0.13093434020212,2.88602590291106,15.1082260438789));
#62477=CARTESIAN_POINT('Ctrl Pts',(-0.230094798512676,2.86743186329655,
15.121232357953));
#62478=CARTESIAN_POINT('Ctrl Pts',(-0.327908726704405,2.84382209488468,
15.1343288085909));
#62479=CARTESIAN_POINT('Ctrl Pts',(-0.401269172848201,2.82611476857578,
15.1441511465694));
#62480=CARTESIAN_POINT('Ctrl Pts',(-0.473871776581697,2.80558493098147,
15.154024186365));
#62481=CARTESIAN_POINT('Ctrl Pts',(-0.54551386023679,2.78219703023119,15.1639571016578));
#62482=CARTESIAN_POINT('Ctrl Pts',(-0.599245422978111,2.76465610466849,
15.1714067881273));
#62483=CARTESIAN_POINT('Ctrl Pts',(-0.652436445713434,2.74550717996222,
15.178890154564));
#62484=CARTESIAN_POINT('Ctrl Pts',(-0.704995275147146,2.7247296345796,15.186411071114));
#62485=CARTESIAN_POINT('Ctrl Pts',(-0.720729468886594,2.71850959642421,
15.1886625588158));
#62486=CARTESIAN_POINT('Ctrl Pts',(-0.736406966678059,2.71214357207348,
15.1909174117022));
#62487=CARTESIAN_POINT('Ctrl Pts',(-0.752025204049111,2.70563092815761,
15.1931757336031));
#62488=CARTESIAN_POINT('Ctrl Pts',(-0.764775912501757,2.70031401422844,
15.1950194246335));
#62489=CARTESIAN_POINT('Ctrl Pts',(-0.777478081511626,2.69490314594757,
15.196864120682));
#62490=CARTESIAN_POINT('Ctrl Pts',(-0.790130440968904,2.6893983882733,15.1987098648068));
#62491=CARTESIAN_POINT('Ctrl Pts',(-0.873485337988913,2.65313254310755,
15.2108697952897));
#62492=CARTESIAN_POINT('Ctrl Pts',(-0.954683148186728,2.61279395749136,
15.2230755503321));
#62493=CARTESIAN_POINT('Ctrl Pts',(-1.0333900295422,2.56835839969231,15.2353460721376));
#62494=CARTESIAN_POINT('Ctrl Pts',(-1.07474974365993,2.54500793864519,15.2417941141031));
#62495=CARTESIAN_POINT('Ctrl Pts',(-1.11542111238663,2.52052546068703,15.2482600407761));
#62496=CARTESIAN_POINT('Ctrl Pts',(-1.15535178122673,2.49490314259947,15.2547466008415));
#62497=CARTESIAN_POINT('Ctrl Pts',(-1.23327915249916,2.44489947493076,15.2674055567063));
#62498=CARTESIAN_POINT('Ctrl Pts',(-1.30838829429154,2.39055588937394,15.2801430971848));
#62499=CARTESIAN_POINT('Ctrl Pts',(-1.38046450469962,2.33219918561456,15.2929796526032));
#62500=CARTESIAN_POINT('Ctrl Pts',(-1.45426350057602,2.27244762382022,15.3061230309111));
#62501=CARTESIAN_POINT('Ctrl Pts',(-1.52488347180723,2.20848778279982,15.3193702140928));
#62502=CARTESIAN_POINT('Ctrl Pts',(-1.59204074405781,2.14065188994946,15.332743132764));
#62503=CARTESIAN_POINT('Ctrl Pts',(-1.60237109058904,2.13021715582588,15.3348001979094));
#62504=CARTESIAN_POINT('Ctrl Pts',(-1.61262065491134,2.1196893711682,15.3368604944486));
#62505=CARTESIAN_POINT('Ctrl Pts',(-1.62278430900332,2.10907388768773,15.3389232952054));
#62506=CARTESIAN_POINT('Ctrl Pts',(-1.68486768809848,2.04423056665054,15.3515236493914));
#62507=CARTESIAN_POINT('Ctrl Pts',(-1.74353795945352,1.97633977637267,15.3641743680265));
#62508=CARTESIAN_POINT('Ctrl Pts',(-1.79863355499942,1.90572574364455,15.3768970731667));
#62509=CARTESIAN_POINT('Ctrl Pts',(-1.8536060338742,1.83526950510231,15.3895913481376));
#62510=CARTESIAN_POINT('Ctrl Pts',(-1.90502010402237,1.76210117952091,15.4023572882508));
#62511=CARTESIAN_POINT('Ctrl Pts',(-1.95266740197694,1.68652354076833,15.4152163709358));
#62512=CARTESIAN_POINT('Ctrl Pts',(-1.999553014057,1.61215408007279,15.4278698893587));
#62513=CARTESIAN_POINT('Ctrl Pts',(-2.04279147033365,1.53545080587127,15.4406135962167));
#62514=CARTESIAN_POINT('Ctrl Pts',(-2.08213462636226,1.45669772176484,15.4534679553077));
#62515=CARTESIAN_POINT('Ctrl Pts',(-2.10370638024081,1.41351760306046,15.4605159681915));
#62516=CARTESIAN_POINT('Ctrl Pts',(-2.12410620181193,1.36972125073741,15.4675972464718));
#62517=CARTESIAN_POINT('Ctrl Pts',(-2.14328646703913,1.32535636167276,15.4747151632939));
#62518=CARTESIAN_POINT('Ctrl Pts',(-2.15012579550102,1.30953666132481,15.4772532810172));
#62519=CARTESIAN_POINT('Ctrl Pts',(-2.15681001155505,1.29364468163272,15.4797960573454));
#62520=CARTESIAN_POINT('Ctrl Pts',(-2.16333680365848,1.27768262506038,15.4823436452153));
#62521=CARTESIAN_POINT('Ctrl Pts',(-2.16791412260327,1.2664882400105,15.4841302996752));
#62522=CARTESIAN_POINT('Ctrl Pts',(-2.17241292255598,1.25526195256421,15.4859189101699));
#62523=CARTESIAN_POINT('Ctrl Pts',(-2.17682958710993,1.24401228867859,15.4877083034276));
#62524=CARTESIAN_POINT('Ctrl Pts',(-2.20791015801245,1.16484712416239,15.5003004673422));
#62525=CARTESIAN_POINT('Ctrl Pts',(-2.2349734122897,1.08441291813616,15.5129492481641));
#62526=CARTESIAN_POINT('Ctrl Pts',(-2.25783961089921,1.00297802743715,15.5256767231474));
#62527=CARTESIAN_POINT('Ctrl Pts',(-2.28035828534265,0.922780797311416,
15.5382107639178));
#62528=CARTESIAN_POINT('Ctrl Pts',(-2.29880657051476,0.841612257746407,
15.5508211250137));
#62529=CARTESIAN_POINT('Ctrl Pts',(-2.31296316132111,0.759731453145844,
15.5635288923091));
#62530=CARTESIAN_POINT('Ctrl Pts',(-2.32670958827523,0.680223009708963,
15.5758684730222));
#62531=CARTESIAN_POINT('Ctrl Pts',(-2.33640931253598,0.600042348520933,
15.5882998973352));
#62532=CARTESIAN_POINT('Ctrl Pts',(-2.34181299591968,0.519439649300842,
15.6008424709262));
#62533=CARTESIAN_POINT('Ctrl Pts',(-2.34572284670801,0.461119332452094,
15.609917686434));
#62534=CARTESIAN_POINT('Ctrl Pts',(-2.34738263953658,0.402578305857885,
15.6190510917899));
#62535=CARTESIAN_POINT('Ctrl Pts',(-2.34668236863854,0.343918483395394,
15.62825));
#62536=CARTESIAN_POINT('',(-2.14373220034752,2.0119373894844,15.058));
#62537=CARTESIAN_POINT('Origin',(0.,0.,15.058));
#62538=CARTESIAN_POINT('Ctrl Pts',(-2.87017396612668,0.00112290304428943,
15.1339652973708));
#62539=CARTESIAN_POINT('Ctrl Pts',(-2.87266912500978,0.0629362380616879,
15.1317805789463));
#62540=CARTESIAN_POINT('Ctrl Pts',(-2.87303098230106,0.124718621761705,
15.1296012856735));
#62541=CARTESIAN_POINT('Ctrl Pts',(-2.87121685856479,0.18637804904607,15.1274262638706));
#62542=CARTESIAN_POINT('Ctrl Pts',(-2.86841400163638,0.281643079490827,
15.1240658123162));
#62543=CARTESIAN_POINT('Ctrl Pts',(-2.86041988710444,0.376614623554742,
15.1207155571276));
#62544=CARTESIAN_POINT('Ctrl Pts',(-2.84750858059062,0.47099184224787,15.1173712434175));
#62545=CARTESIAN_POINT('Ctrl Pts',(-2.83433033308302,0.567320307975548,
15.1139577860911));
#62546=CARTESIAN_POINT('Ctrl Pts',(-2.81602924148459,0.663030385704492,
15.1105505184628));
#62547=CARTESIAN_POINT('Ctrl Pts',(-2.79284156103339,0.757800921120369,
15.1071449162423));
#62548=CARTESIAN_POINT('Ctrl Pts',(-2.77879319434313,0.815218101582043,
15.1050816159094));
#62549=CARTESIAN_POINT('Ctrl Pts',(-2.76295010551778,0.872290339259573,
15.1030189268812));
#62550=CARTESIAN_POINT('Ctrl Pts',(-2.74535586092349,0.928944130664371,
15.100955843023));
#62551=CARTESIAN_POINT('Ctrl Pts',(-2.7354097693855,0.960970728468381,15.099789574088));
#62552=CARTESIAN_POINT('Ctrl Pts',(-2.72490394590206,0.992863566804536,
15.098623178978));
#62553=CARTESIAN_POINT('Ctrl Pts',(-2.7138453785436,1.0246089965303,15.0974564759315));
#62554=CARTESIAN_POINT('Ctrl Pts',(-2.70868377697821,1.03942621963478,15.0969119156755));
#62555=CARTESIAN_POINT('Ctrl Pts',(-2.7034040983514,1.05420445638712,15.0963675402945));
#62556=CARTESIAN_POINT('Ctrl Pts',(-2.69801003661965,1.06893536837389,15.0958235919881));
#62557=CARTESIAN_POINT('Ctrl Pts',(-2.66394262772994,1.16197175299988,15.0923881642358));
#62558=CARTESIAN_POINT('Ctrl Pts',(-2.62528653689294,1.25320878716493,15.0889665364856));
#62559=CARTESIAN_POINT('Ctrl Pts',(-2.58232115247044,1.34232723597939,15.0855542358814));
#62560=CARTESIAN_POINT('Ctrl Pts',(-2.53887733631532,1.43243804397901,15.0821039383428));
#62561=CARTESIAN_POINT('Ctrl Pts',(-2.49102735184572,1.52038366982231,15.0786631768276));
#62562=CARTESIAN_POINT('Ctrl Pts',(-2.43900735397324,1.60582293428401,15.0752273273902));
#62563=CARTESIAN_POINT('Ctrl Pts',(-2.38725398360023,1.69082428143753,15.071809088333));
#62564=CARTESIAN_POINT('Ctrl Pts',(-2.33137274895099,1.77334571203064,15.0683957111292));
#62565=CARTESIAN_POINT('Ctrl Pts',(-2.27155099682431,1.8530278346518,15.064982642569));
#62566=CARTESIAN_POINT('Ctrl Pts',(-2.23076137590659,1.90735930205439,15.0626554326866));
#62567=CARTESIAN_POINT('Ctrl Pts',(-2.18813878650124,1.96037022431859,15.0603283662998));
#62568=CARTESIAN_POINT('Ctrl Pts',(-2.14373220034752,2.0119373894844,15.058));
#62569=CARTESIAN_POINT('',(-2.,-2.44929359829471E-16,16.));
#62570=CARTESIAN_POINT('',(-2.5,-3.06161699786838E-16,15.5));
#62571=CARTESIAN_POINT('Origin',(0.,0.,16.));
#62572=CARTESIAN_POINT('Ctrl Pts',(1.70810875200393,-2.39535560853239,-0.329233991005387));
#62573=CARTESIAN_POINT('Ctrl Pts',(2.5000696979919,-1.83061464970825,-0.276613620635017));
#62574=CARTESIAN_POINT('Ctrl Pts',(3.46698259537958,0.135843711197753,-0.171372879894276));
#62575=CARTESIAN_POINT('Ctrl Pts',(1.78000461065578,2.98198357260362,-0.013511768783165));
#62576=CARTESIAN_POINT('Ctrl Pts',(-1.52068059202578,3.11864337292237,0.144349342327946));
#62577=CARTESIAN_POINT('Ctrl Pts',(-3.44323740053193,0.434868872546417,
0.302210453439058));
#62578=CARTESIAN_POINT('Ctrl Pts',(-2.24748662857037,-2.64500439253867,
0.460071564550167));
#62579=CARTESIAN_POINT('Ctrl Pts',(0.98413688813967,-3.32800743087112,0.61793267566128));
#62580=CARTESIAN_POINT('Ctrl Pts',(3.3242675736315,-0.997273536182889,0.775793786772391));
#62581=CARTESIAN_POINT('Ctrl Pts',(2.65350107828341,2.23705783115145,0.933654897883501));
#62582=CARTESIAN_POINT('Ctrl Pts',(-0.420704297245377,3.44500822120461,
1.09151600899461));
#62583=CARTESIAN_POINT('Ctrl Pts',(-3.11384086799285,1.53272940938773,1.24937712010572));
#62584=CARTESIAN_POINT('Ctrl Pts',(-2.98662452021757,-1.76786447124123,
1.40723823121684));
#62585=CARTESIAN_POINT('Ctrl Pts',(-0.154268773033873,-3.46719137695888,
1.56509934232795));
#62586=CARTESIAN_POINT('Ctrl Pts',(2.81781362814421,-2.02612228753563,1.72296045343906));
#62587=CARTESIAN_POINT('Ctrl Pts',(3.23766264061691,1.25011350527631,1.88082156455017));
#62588=CARTESIAN_POINT('Ctrl Pts',(0.724998218776244,3.39405562633926,2.03868267566128));
#62589=CARTESIAN_POINT('Ctrl Pts',(-2.44433298400306,2.46383378430329,2.19654378677239));
#62590=CARTESIAN_POINT('Ctrl Pts',(-3.39970985401105,-0.698006346200326,
2.35440489788351));
#62591=CARTESIAN_POINT('Ctrl Pts',(-1.27579956793912,-3.22762676650925,
2.51226600899461));
#62592=CARTESIAN_POINT('Ctrl Pts',(2.00366607964198,-2.83382462640088,2.67012712010573));
#62593=CARTESIAN_POINT('Ctrl Pts',(3.46831127903076,0.12671419166248,2.82798823121683));
#62594=CARTESIAN_POINT('Ctrl Pts',(1.79153366111842,2.9724815653929,2.98584934232795));
#62595=CARTESIAN_POINT('Ctrl Pts',(-1.50792549309295,3.12592391504671,3.14371045343906));
#62596=CARTESIAN_POINT('Ctrl Pts',(-3.44158119482194,0.448060782465637,
3.30157156455017));
#62597=CARTESIAN_POINT('Ctrl Pts',(-2.25802486298351,-2.63563337612261,
3.45943267566128));
#62598=CARTESIAN_POINT('Ctrl Pts',(0.970737398643871,-3.33210271331857,
3.61729378677239));
#62599=CARTESIAN_POINT('Ctrl Pts',(3.32025430017048,-1.01052014634333,3.7751548978835));
#62600=CARTESIAN_POINT('Ctrl Pts',(2.66245099976358,2.22634100195603,3.93301600899462));
#62601=CARTESIAN_POINT('Ctrl Pts',(-0.406867188726441,3.44669387613558,
4.09087712010572));
#62602=CARTESIAN_POINT('Ctrl Pts',(-3.10766543711734,1.54520390729755,4.24873823121684));
#62603=CARTESIAN_POINT('Ctrl Pts',(-2.99369583814259,-1.75585443953709,
4.40659934232795));
#62604=CARTESIAN_POINT('Ctrl Pts',(-0.16818635164463,-3.46654769699322,
4.56446045343906));
#62605=CARTESIAN_POINT('Ctrl Pts',(2.80965791624474,-2.03741551431062,4.72232156455017));
#62606=CARTESIAN_POINT('Ctrl Pts',(3.24265463709948,1.23710569022097,4.88018267566128));
#62607=CARTESIAN_POINT('Ctrl Pts',(0.738617048059715,3.39111846455234,5.0380437867724));
#62608=CARTESIAN_POINT('Ctrl Pts',(-2.43442290318405,2.47362582310745,5.1959048978835));
#62609=CARTESIAN_POINT('Ctrl Pts',(-3.40248440570545,-0.684353310232048,
5.35376600899462));
#62610=CARTESIAN_POINT('Ctrl Pts',(-1.28874579170717,-3.22247945977245,
5.51162712010572));
#62611=CARTESIAN_POINT('Ctrl Pts',(1.99227427239527,-2.84184496548404,5.66948823121683));
#62612=CARTESIAN_POINT('Ctrl Pts',(3.46879199270663,0.112790494414327,5.82734934232795));
#62613=CARTESIAN_POINT('Ctrl Pts',(1.803451502182,2.96526596843754,5.98521045343906));
#62614=CARTESIAN_POINT('Ctrl Pts',(-1.49536511544646,3.13195190828366,6.14307156455017));
#62615=CARTESIAN_POINT('Ctrl Pts',(-3.4397548386282,0.461872530499354,6.30093267566129));
#62616=CARTESIAN_POINT('Ctrl Pts',(-2.26858675213732,-2.62654787360198,
6.45879378677239));
#62617=CARTESIAN_POINT('Ctrl Pts',(0.957353695793138,-3.33597264458916,
6.61665489788351));
#62618=CARTESIAN_POINT('Ctrl Pts',(3.31617107144768,-1.02384032406894,6.77451600899461));
#62619=CARTESIAN_POINT('Ctrl Pts',(2.67136662968815,2.21563532967061,6.93237712010573));
#62620=CARTESIAN_POINT('Ctrl Pts',(-0.393028031746144,3.44829937078522,
7.09023823121684));
#62621=CARTESIAN_POINT('Ctrl Pts',(-3.10143756889894,1.55766639256237,7.24809934232795));
#62622=CARTESIAN_POINT('Ctrl Pts',(-3.00072015011765,-1.74382285940228,
7.40596045343905));
#62623=CARTESIAN_POINT('Ctrl Pts',(-0.182100573498421,-3.46584462511342,
7.56382156455018));
#62624=CARTESIAN_POINT('Ctrl Pts',(2.80145659039814,-2.04867775807003,7.72168267566128));
#62625=CARTESIAN_POINT('Ctrl Pts',(3.24759455782818,1.22407890769377,7.8795437867724));
#62626=CARTESIAN_POINT('Ctrl Pts',(0.752223882355328,3.38812615100299,8.03740489788349));
#62627=CARTESIAN_POINT('Ctrl Pts',(-2.42447354494764,2.4833782664236,8.19526600899462));
#62628=CARTESIAN_POINT('Ctrl Pts',(-3.40520415435994,-0.670689385204343,
8.35312712010572));
#62629=CARTESIAN_POINT('Ctrl Pts',(-1.30167123501543,-3.21728015258687,
8.51098823121684));
#62630=CARTESIAN_POINT('Ctrl Pts',(1.98085035420065,-2.84981954842042,8.66884934232795));
#62631=CARTESIAN_POINT('Ctrl Pts',(3.46921681308078,0.098864999537257,8.82671045343906));
#62632=CARTESIAN_POINT('Ctrl Pts',(1.81534028008778,2.95800257805621,8.98457156455017));
#62633=CARTESIAN_POINT('Ctrl Pts',(-1.4827806401293,3.13792943795007,9.14243267566127));
#62634=CARTESIAN_POINT('Ctrl Pts',(-3.4378730539225,0.475676832953572,9.3002937867724));
#62635=CARTESIAN_POINT('Ctrl Pts',(-2.27911208446667,-2.61742004476474,
9.45815489788349));
#62636=CARTESIAN_POINT('Ctrl Pts',(0.943954565772613,-3.3397888199782,9.61601600899462));
#62637=CARTESIAN_POINT('Ctrl Pts',(3.31203440522278,-1.03714400297725,9.77387712010572));
#62638=CARTESIAN_POINT('Ctrl Pts',(2.68023921253269,2.20489395389312,9.93173823121684));
#62639=CARTESIAN_POINT('Ctrl Pts',(-0.379182541400898,3.44984929882113,
10.0895993423279));
#62640=CARTESIAN_POINT('Ctrl Pts',(-3.09515972337558,1.57010377716378,10.2474604534391));
#62641=CARTESIAN_POINT('Ctrl Pts',(-3.00769610777576,-1.73176317886687,
10.4053215645502));
#62642=CARTESIAN_POINT('Ctrl Pts',(-0.196011860918037,-3.46508570377902,
10.5631826756613));
#62643=CARTESIAN_POINT('Ctrl Pts',(2.79321012116224,-2.05990698897259,10.7210437867724));
#62644=CARTESIAN_POINT('Ctrl Pts',(3.25248214612884,1.2110324001305,10.8789048978835));
#62645=CARTESIAN_POINT('Ctrl Pts',(0.765818594962506,3.38507924024569,11.0367660089946));
#62646=CARTESIAN_POINT('Ctrl Pts',(-2.41448511783304,2.49309069223908,11.1946271201057));
#62647=CARTESIAN_POINT('Ctrl Pts',(-3.40786903136843,-0.657014653010787,
11.3524882312168));
#62648=CARTESIAN_POINT('Ctrl Pts',(-1.3145757016765,-3.21202900045202,11.510349342328));
#62649=CARTESIAN_POINT('Ctrl Pts',(1.96939451380669,-2.85774821044889,11.668210453439));
#62650=CARTESIAN_POINT('Ctrl Pts',(3.46958573405997,0.0849379149034097,
11.8260715645502));
#62651=CARTESIAN_POINT('Ctrl Pts',(1.82719979676502,2.95069151525923,11.9839326756613));
#62652=CARTESIAN_POINT('Ctrl Pts',(-1.47017225488226,3.14385641459579,12.1417937867724));
#62653=CARTESIAN_POINT('Ctrl Pts',(-3.43593590116163,0.489473446687968,
12.2996548978835));
#62654=CARTESIAN_POINT('Ctrl Pts',(-2.28960063207268,-2.60824999320481,
12.4575160089946));
#62655=CARTESIAN_POINT('Ctrl Pts',(0.930540112760845,-3.34355126315401,
12.6153771201057));
#62656=CARTESIAN_POINT('Ctrl Pts',(3.30784458181684,-1.05043080491032,12.7732382312169));
#62657=CARTESIAN_POINT('Ctrl Pts',(2.68906819704165,2.19411673426304,12.9310993423279));
#62658=CARTESIAN_POINT('Ctrl Pts',(-0.365330160772045,3.45134423437463,
13.0889604534391));
#62659=CARTESIAN_POINT('Ctrl Pts',(-3.08883349189378,1.58251471600082,13.2468215645502));
#62660=CARTESIAN_POINT('Ctrl Pts',(-3.01462075186278,-1.71967340539697,
13.4046826756613));
#62661=CARTESIAN_POINT('Ctrl Pts',(-0.209925428309919,-3.46427512302224,
13.5625437867724));
#62662=CARTESIAN_POINT('Ctrl Pts',(2.78492903121011,-2.07109504482717,13.7204048978835));
#62663=CARTESIAN_POINT('Ctrl Pts',(3.25729747472216,1.19795113049603,13.8782660089946));
#62664=CARTESIAN_POINT('Ctrl Pts',(0.779438885227093,3.38200690959721,14.0361271201057));
#62665=CARTESIAN_POINT('Ctrl Pts',(-2.40453022224261,2.50270729758603,14.1939882312168));
#62666=CARTESIAN_POINT('Ctrl Pts',(-3.41034060095634,-0.643223025084935,
14.351849342328));
#62667=CARTESIAN_POINT('Ctrl Pts',(-1.3277234162215,-3.20692920286191,14.5097104534391));
#62668=CARTESIAN_POINT('Ctrl Pts',(1.95841253548915,-2.86524258546647,14.6675715645502));
#62669=CARTESIAN_POINT('Ctrl Pts',(3.46892903525912,0.0702659147297645,
14.8254326756613));
#62670=CARTESIAN_POINT('Ctrl Pts',(1.8409162673649,2.94476989555806,14.9832937867724));
#62671=CARTESIAN_POINT('Ctrl Pts',(-1.46144261101867,3.14684084841223,15.1411548978835));
#62672=CARTESIAN_POINT('Ctrl Pts',(-2.76985851330384,1.3890220685151,15.2463956386242));
#62673=CARTESIAN_POINT('Ctrl Pts',(-2.91090525077878,0.426608275808748,
15.2990160089946));
#62674=CARTESIAN_POINT('Ctrl Pts',(1.59774743137963,-2.24059110187414,-0.219489327336926));
#62675=CARTESIAN_POINT('Ctrl Pts',(2.33853958862414,-1.71233819332979,-0.166868956966556));
#62676=CARTESIAN_POINT('Ctrl Pts',(3.24298000926863,0.127066816079881,-0.061628216225815));
#62677=CARTESIAN_POINT('Ctrl Pts',(1.66499808117169,2.78931689094975,0.0962328948852963));
#62678=CARTESIAN_POINT('Ctrl Pts',(-1.42242905026252,2.9171470684346,0.254094005996407));
#62679=CARTESIAN_POINT('Ctrl Pts',(-3.22076899721748,0.406771889250497,
0.411955117107519));
#62680=CARTESIAN_POINT('Ctrl Pts',(-2.10227597256058,-2.4741100174146,0.56981622821863));
#62681=CARTESIAN_POINT('Ctrl Pts',(0.9205515651778,-3.11298406383574,0.72767733932974));
#62682=CARTESIAN_POINT('Ctrl Pts',(3.10948583967916,-0.932839451205724,
0.885538450440853));
#62683=CARTESIAN_POINT('Ctrl Pts',(2.48205773023319,2.09252098227156,1.04339956155196));
#62684=CARTESIAN_POINT('Ctrl Pts',(-0.393522490594119,3.22242540473713,
1.20126067266308));
#62685=CARTESIAN_POINT('Ctrl Pts',(-2.91265485451303,1.43369939061326,1.35912178377418));
#62686=CARTESIAN_POINT('Ctrl Pts',(-2.79365798581306,-1.65364231910831,
1.5169828948853));
#62687=CARTESIAN_POINT('Ctrl Pts',(-0.144301430203291,-3.24317530141947,
1.67484400599641));
#62688=CARTESIAN_POINT('Ctrl Pts',(2.6357540064074,-1.8952140352733,1.83270511710752));
#62689=CARTESIAN_POINT('Ctrl Pts',(3.02847647238534,1.16934336859111,1.99056622821863));
#62690=CARTESIAN_POINT('Ctrl Pts',(0.67815590807408,3.17476486938028,2.14842733932974));
#62691=CARTESIAN_POINT('Ctrl Pts',(-2.28640403724036,2.30464488610489,2.30628845044085));
#62692=CARTESIAN_POINT('Ctrl Pts',(-3.18005377603123,-0.652907986929923,
2.46414956155196));
#62693=CARTESIAN_POINT('Ctrl Pts',(-1.19336984851725,-3.01908901853714,
2.62201067266307));
#62694=CARTESIAN_POINT('Ctrl Pts',(1.87420872841654,-2.65073053018457,2.77987178377419));
#62695=CARTESIAN_POINT('Ctrl Pts',(3.24422284634695,0.118527157015377,2.9377328948853));
#62696=CARTESIAN_POINT('Ctrl Pts',(1.67578223688854,2.78042881072881,3.09559400599641));
#62697=CARTESIAN_POINT('Ctrl Pts',(-1.41049806136441,2.92395721296701,3.25345511710752));
#62698=CARTESIAN_POINT('Ctrl Pts',(-3.21921979935999,0.419111466671254,
3.41131622821863));
#62699=CARTESIAN_POINT('Ctrl Pts',(-2.11213332909314,-2.46534446464132,
3.56917733932974));
#62700=CARTESIAN_POINT('Ctrl Pts',(0.908017819947236,-3.11681474909129,
3.72703845044085));
#62701=CARTESIAN_POINT('Ctrl Pts',(3.10573186478955,-0.94523019467185,3.88489956155197));
#62702=CARTESIAN_POINT('Ctrl Pts',(2.49042939511648,2.08249657000891,4.04276067266307));
#62703=CARTESIAN_POINT('Ctrl Pts',(-0.380579401011611,3.2240021490943,4.20062178377419));
#62704=CARTESIAN_POINT('Ctrl Pts',(-2.90687841972373,1.44536790818848,4.3584828948853));
#62705=CARTESIAN_POINT('Ctrl Pts',(-2.8002724241724,-1.64240825846459,4.5163440059964));
#62706=CARTESIAN_POINT('Ctrl Pts',(-0.157319790685473,-3.24257320977247,
4.67420511710753));
#62707=CARTESIAN_POINT('Ctrl Pts',(2.62812523703122,-1.90577760392813,4.83206622821863));
#62708=CARTESIAN_POINT('Ctrl Pts',(3.03314593476479,1.15717599162043,4.98992733932975));
#62709=CARTESIAN_POINT('Ctrl Pts',(0.690894821495446,3.17201747832858,5.14778845044085));
#62710=CARTESIAN_POINT('Ctrl Pts',(-2.27713424914591,2.31380425890769,5.30564956155197));
#62711=CARTESIAN_POINT('Ctrl Pts',(-3.18264906326793,-0.640137076925948,
5.46351067266308));
#62712=CARTESIAN_POINT('Ctrl Pts',(-1.20547961362863,-3.01427428053665,
5.62137178377419));
#62713=CARTESIAN_POINT('Ctrl Pts',(1.86355294859817,-2.65823267321491,5.7792328948853));
#62714=CARTESIAN_POINT('Ctrl Pts',(3.24467250099567,0.105503073222438,5.93709400599641));
#62715=CARTESIAN_POINT('Ctrl Pts',(1.68693006335134,2.77367941524228,6.09495511710752));
#62716=CARTESIAN_POINT('Ctrl Pts',(-1.39874921276312,2.92959573609933,6.25281622821863));
#62717=CARTESIAN_POINT('Ctrl Pts',(-3.21751144448276,0.432030834315646,
6.41067733932974));
#62718=CARTESIAN_POINT('Ctrl Pts',(-2.12201281202782,-2.45684597864148,
6.56853845044085));
#62719=CARTESIAN_POINT('Ctrl Pts',(0.895498841382776,-3.12043464316416,
6.72639956155197));
#62720=CARTESIAN_POINT('Ctrl Pts',(3.10191245446456,-0.957689752484927,
6.88426067266308));
#62721=CARTESIAN_POINT('Ctrl Pts',(2.4987689840299,2.07248259380561,7.04212178377418));
#62722=CARTESIAN_POINT('Ctrl Pts',(-0.367634395319329,3.22550391234535,
7.1999828948853));
#62723=CARTESIAN_POINT('Ctrl Pts',(-2.90105293558095,1.45702518925863,7.3578440059964));
#62724=CARTESIAN_POINT('Ctrl Pts',(-2.8068428936476,-1.63115404163953,7.51570511710752));
#62725=CARTESIAN_POINT('Ctrl Pts',(-0.170335011291572,-3.24191556353729,
7.67356622821863));
#62726=CARTESIAN_POINT('Ctrl Pts',(2.62045380083611,-1.91631219138755,7.83142733932975));
#62727=CARTESIAN_POINT('Ctrl Pts',(3.03776668601744,1.14499087267086,7.98928845044085));
#62728=CARTESIAN_POINT('Ctrl Pts',(0.703622514928034,3.16921849888318,8.14714956155197));
#62729=CARTESIAN_POINT('Ctrl Pts',(-2.26782772135753,2.32292659449655,8.30501067266308));
#62730=CARTESIAN_POINT('Ctrl Pts',(-3.18519308830241,-0.627355981407313,
8.46287178377418));
#62731=CARTESIAN_POINT('Ctrl Pts',(-1.21756994091078,-3.00941090184898,
8.62073289488531));
#62732=CARTESIAN_POINT('Ctrl Pts',(1.852867132528,-2.6656920164142,8.77859400599641));
#62733=CARTESIAN_POINT('Ctrl Pts',(3.24506987362244,0.0924773079458306,
8.93645511710752));
#62734=CARTESIAN_POINT('Ctrl Pts',(1.698050704434,2.7668853142746,9.09431622821864));
#62735=CARTESIAN_POINT('Ctrl Pts',(-1.3869778234475,2.93518705612466,9.25217733932973));
#62736=CARTESIAN_POINT('Ctrl Pts',(-3.21575124234316,0.444943237441223,
9.41003845044086));
#62737=CARTESIAN_POINT('Ctrl Pts',(-2.13185810008334,-2.44830790103859,
9.56789956155196));
#62738=CARTESIAN_POINT('Ctrl Pts',(0.882965432401702,-3.12400425453603,
9.72576067266308));
#62739=CARTESIAN_POINT('Ctrl Pts',(3.09804305924746,-0.970133877473286,
9.88362178377418));
#62740=CARTESIAN_POINT('Ctrl Pts',(2.50706830714555,2.06243522092151,10.0414828948853));
#62741=CARTESIAN_POINT('Ctrl Pts',(-0.354683465462343,3.22695369915506,
10.1993440059964));
#62742=CARTESIAN_POINT('Ctrl Pts',(-2.89518070317902,1.4686589914253,10.3572051171075));
#62743=CARTESIAN_POINT('Ctrl Pts',(-2.81336813298999,-1.61987353998757,
10.5150662282186));
#62744=CARTESIAN_POINT('Ctrl Pts',(-0.183347487058001,-3.24120567629433,
10.6729273393297));
#62745=CARTESIAN_POINT('Ctrl Pts',(2.61274013797703,-1.9268158989588,10.8307884504409));
#62746=CARTESIAN_POINT('Ctrl Pts',(3.04233848605292,1.13278730312457,10.988649561552));
#62747=CARTESIAN_POINT('Ctrl Pts',(0.716338869857416,3.16636844976869,11.1465106726631));
#62748=CARTESIAN_POINT('Ctrl Pts',(-2.25848464894066,2.33201149812516,11.3043717837742));
#62749=CARTESIAN_POINT('Ctrl Pts',(-3.18768578696123,-0.61456477697643,
11.4622328948853));
#62750=CARTESIAN_POINT('Ctrl Pts',(-1.22964064685199,-3.00449902792679,
11.6200940059964));
#62751=CARTESIAN_POINT('Ctrl Pts',(1.84215145675955,-2.67310840566659,11.7779551171075));
#62752=CARTESIAN_POINT('Ctrl Pts',(3.24541495852771,0.0794500556270124,
11.9358162282186));
#62753=CARTESIAN_POINT('Ctrl Pts',(1.70914397486321,2.76004662101762,12.0936773393297));
#62754=CARTESIAN_POINT('Ctrl Pts',(-1.37518406902836,2.94073108937221,12.2515384504409));
#62755=CARTESIAN_POINT('Ctrl Pts',(-3.21393924949186,0.457848448617044,
12.409399561552));
#62756=CARTESIAN_POINT('Ctrl Pts',(-2.14166898008542,-2.43973032873338,
12.5672606726631));
#62757=CARTESIAN_POINT('Ctrl Pts',(0.870417690451563,-3.12752360534598,
12.7251217837742));
#62758=CARTESIAN_POINT('Ctrl Pts',(3.09412394134766,-0.98256221591188,12.8829828948853));
#62759=CARTESIAN_POINT('Ctrl Pts',(2.51532684882466,2.05235432006483,13.0408440059964));
#62760=CARTESIAN_POINT('Ctrl Pts',(-0.341726090504644,3.22835204655998,
13.1987051171075));
#62761=CARTESIAN_POINT('Ctrl Pts',(-2.88926321104715,1.48026805649486,13.3565662282186));
#62762=CARTESIAN_POINT('Ctrl Pts',(-2.81984537414356,-1.60856488971291,
13.5144273393297));
#62763=CARTESIAN_POINT('Ctrl Pts',(-0.196362095487134,-3.24044746735677,
13.6722884504409));
#62764=CARTESIAN_POINT('Ctrl Pts',(2.60499409125458,-1.93728109181189,13.830149561552));
#62765=CARTESIAN_POINT('Ctrl Pts',(3.04684269509828,1.12055121749295,13.9880106726631));
#62766=CARTESIAN_POINT('Ctrl Pts',(0.729079149865556,3.16349462314833,14.1458717837742));
#62767=CARTESIAN_POINT('Ctrl Pts',(-2.24917294156805,2.34100677226896,14.3037328948853));
#62768=CARTESIAN_POINT('Ctrl Pts',(-3.1899976678388,-0.601664229474863,
14.4615940059964));
#62769=CARTESIAN_POINT('Ctrl Pts',(-1.24193888437236,-2.9997287294955,14.6194551171075));
#62770=CARTESIAN_POINT('Ctrl Pts',(1.83187902672385,-2.68011856729716,14.7773162282186));
#62771=CARTESIAN_POINT('Ctrl Pts',(3.24480068919561,0.0657260169420378,
14.9351773393297));
#62772=CARTESIAN_POINT('Ctrl Pts',(1.72197422097186,2.75450759860113,15.0930384504409));
#62773=CARTESIAN_POINT('Ctrl Pts',(-1.36701844957144,2.94352269819615,15.250899561552));
#62774=CARTESIAN_POINT('Ctrl Pts',(-2.59089728316432,1.29927701587847,15.3561403022927));
#62775=CARTESIAN_POINT('Ctrl Pts',(-2.72283095673204,0.399045011670964,
15.4087606726631));
#62776=CARTESIAN_POINT('Ctrl Pts',(1.48738611075532,-2.0858265952159,-0.109744663668465));
#62777=CARTESIAN_POINT('Ctrl Pts',(2.17700947925639,-1.59406173695134,-0.0571242932980945));
#62778=CARTESIAN_POINT('Ctrl Pts',(3.01897742315769,0.118289920962009,0.0481164474426461));
#62779=CARTESIAN_POINT('Ctrl Pts',(1.5499915516876,2.59665020929587,0.205977558553758));
#62780=CARTESIAN_POINT('Ctrl Pts',(-1.32417750849926,2.71565076394683,0.363838669664868));
#62781=CARTESIAN_POINT('Ctrl Pts',(-2.99830059390304,0.37867490595458,0.521699780775981));
#62782=CARTESIAN_POINT('Ctrl Pts',(-1.95706531655079,-2.30321564229053,
0.679560891887089));
#62783=CARTESIAN_POINT('Ctrl Pts',(0.856966242215927,-2.89796069680035,
0.837422002998203));
#62784=CARTESIAN_POINT('Ctrl Pts',(2.89470410572683,-0.86840536622856,0.995283114109312));
#62785=CARTESIAN_POINT('Ctrl Pts',(2.31061438218297,1.94798413339166,1.15314422522042));
#62786=CARTESIAN_POINT('Ctrl Pts',(-0.36634068394286,2.99984258826965,1.31100533633153));
#62787=CARTESIAN_POINT('Ctrl Pts',(-2.71146884103322,1.33466937183879,1.46886644744265));
#62788=CARTESIAN_POINT('Ctrl Pts',(-2.60069145140856,-1.53942016697539,
1.62672755855376));
#62789=CARTESIAN_POINT('Ctrl Pts',(-0.134334087372704,-3.01915922588007,
1.78458866966487));
#62790=CARTESIAN_POINT('Ctrl Pts',(2.45369438467058,-1.76430578301097,1.94244978077598));
#62791=CARTESIAN_POINT('Ctrl Pts',(2.81929030415377,1.0885732319059,2.10031089188709));
#62792=CARTESIAN_POINT('Ctrl Pts',(0.63131359737191,2.95547411242131,2.2581720029982));
#62793=CARTESIAN_POINT('Ctrl Pts',(-2.12847509047765,2.14545598790649,2.41603311410931));
#62794=CARTESIAN_POINT('Ctrl Pts',(-2.96039769805142,-0.607809627659522,
2.57389422522043));
#62795=CARTESIAN_POINT('Ctrl Pts',(-1.11094012909538,-2.81055127056503,
2.73175533633153));
#62796=CARTESIAN_POINT('Ctrl Pts',(1.74475137719111,-2.46763643396825,2.88961644744264));
#62797=CARTESIAN_POINT('Ctrl Pts',(3.02013441366314,0.110340122368272,3.04747755855376));
#62798=CARTESIAN_POINT('Ctrl Pts',(1.56003081265866,2.58837605606472,3.20533866966487));
#62799=CARTESIAN_POINT('Ctrl Pts',(-1.31307062963587,2.72199051088731,3.36319978077598));
#62800=CARTESIAN_POINT('Ctrl Pts',(-2.99685840389804,0.390162150876873,
3.52106089188709));
#62801=CARTESIAN_POINT('Ctrl Pts',(-1.96624179520275,-2.29505555316004,
3.6789220029982));
#62802=CARTESIAN_POINT('Ctrl Pts',(0.845298241250599,-2.90152678486402,
3.83678311410932));
#62803=CARTESIAN_POINT('Ctrl Pts',(2.89120942940861,-0.879940243000373,
3.99464422522043));
#62804=CARTESIAN_POINT('Ctrl Pts',(2.31840779046938,1.93865213806179,4.15250533633154));
#62805=CARTESIAN_POINT('Ctrl Pts',(-0.354291613296782,3.00131042205302,
4.31036644744265));
#62806=CARTESIAN_POINT('Ctrl Pts',(-2.70609140233011,1.34553190907942,4.46822755855376));
#62807=CARTESIAN_POINT('Ctrl Pts',(-2.60684901020221,-1.52896207739209,
4.62608866966487));
#62808=CARTESIAN_POINT('Ctrl Pts',(-0.146453229726317,-3.01859872255171,
4.78394978077598));
#62809=CARTESIAN_POINT('Ctrl Pts',(2.44659255781772,-1.77413969354566,4.94181089188709));
#62810=CARTESIAN_POINT('Ctrl Pts',(2.82363723243009,1.07724629301989,5.09967200299821));
#62811=CARTESIAN_POINT('Ctrl Pts',(0.643172594931182,2.95291649210482,5.25753311410931));
#62812=CARTESIAN_POINT('Ctrl Pts',(-2.11984559510778,2.15398269470792,5.41539422522043));
#62813=CARTESIAN_POINT('Ctrl Pts',(-2.96281372083041,-0.595920843619846,
5.57325533633153));
#62814=CARTESIAN_POINT('Ctrl Pts',(-1.12221343555009,-2.80606910130085,
5.73111644744265));
#62815=CARTESIAN_POINT('Ctrl Pts',(1.73483162480106,-2.47462038094578,5.88897755855376));
#62816=CARTESIAN_POINT('Ctrl Pts',(3.02055300928471,0.0982156520305535,
6.04683866966487));
#62817=CARTESIAN_POINT('Ctrl Pts',(1.57040862452068,2.58209286204701,6.20469978077598));
#62818=CARTESIAN_POINT('Ctrl Pts',(-1.30213331007977,2.72723956391501,6.36256089188709));
#62819=CARTESIAN_POINT('Ctrl Pts',(-2.99526805033731,0.402189138131933,
6.52042200299821));
#62820=CARTESIAN_POINT('Ctrl Pts',(-1.97543887191833,-2.28714408368097,
6.67828311410931));
#62821=CARTESIAN_POINT('Ctrl Pts',(0.833643986972413,-2.90489664173917,
6.83614422522043));
#62822=CARTESIAN_POINT('Ctrl Pts',(2.88765383748144,-0.891539180900916,
6.99400533633154));
#62823=CARTESIAN_POINT('Ctrl Pts',(2.32617133837164,1.9293298579406,7.15186644744265));
#62824=CARTESIAN_POINT('Ctrl Pts',(-0.342240758892514,3.00270845390548,
7.30972755855377));
#62825=CARTESIAN_POINT('Ctrl Pts',(-2.70066830226297,1.35638398595488,7.46758866966487));
#62826=CARTESIAN_POINT('Ctrl Pts',(-2.61296563717754,-1.51848522387679,
7.62544978077598));
#62827=CARTESIAN_POINT('Ctrl Pts',(-0.158569449084724,-3.01798650196116,
7.78331089188708));
#62828=CARTESIAN_POINT('Ctrl Pts',(2.43945101127409,-1.78394662470507,7.94117200299821));
#62829=CARTESIAN_POINT('Ctrl Pts',(2.8279388142067,1.06590283764795,8.09903311410931));
#62830=CARTESIAN_POINT('Ctrl Pts',(0.655021147500741,2.95031084676337,8.25689422522044));
#62831=CARTESIAN_POINT('Ctrl Pts',(-2.11118189776743,2.16247492256949,8.41475533633153));
#62832=CARTESIAN_POINT('Ctrl Pts',(-2.96518202224487,-0.584022577610279,
8.57261644744266));
#62833=CARTESIAN_POINT('Ctrl Pts',(-1.13346864680612,-2.8015416511111,8.73047755855375));
#62834=CARTESIAN_POINT('Ctrl Pts',(1.72488391085535,-2.48156448440799,8.88833866966489));
#62835=CARTESIAN_POINT('Ctrl Pts',(3.0209229341641,0.0860896163543999,9.04619978077597));
#62836=CARTESIAN_POINT('Ctrl Pts',(1.58076112878023,2.575768050493,9.2040608918871));
#62837=CARTESIAN_POINT('Ctrl Pts',(-1.2911750067657,2.73244467429924,9.3619220029982));
#62838=CARTESIAN_POINT('Ctrl Pts',(-2.99362943076381,0.414209641928883,
9.51978311410932));
#62839=CARTESIAN_POINT('Ctrl Pts',(-1.98460411570002,-2.27919575731244,
9.67764422522042));
#62840=CARTESIAN_POINT('Ctrl Pts',(0.821976299030791,-2.90821968909385,
9.83550533633154));
#62841=CARTESIAN_POINT('Ctrl Pts',(2.88405171327213,-0.903123751969326,
9.99336644744264));
#62842=CARTESIAN_POINT('Ctrl Pts',(2.33389740175841,1.9199764879499,10.1512275585538));
#62843=CARTESIAN_POINT('Ctrl Pts',(-0.330184389523787,3.00405809948898,
10.3090886696649));
#62844=CARTESIAN_POINT('Ctrl Pts',(-2.69520168298246,1.36721420568682,10.466949780776));
#62845=CARTESIAN_POINT('Ctrl Pts',(-2.61904015820422,-1.50798390110827,
10.6248108918871));
#62846=CARTESIAN_POINT('Ctrl Pts',(-0.170683113197963,-3.01732564880962,
10.7826720029982));
#62847=CARTESIAN_POINT('Ctrl Pts',(2.43227015479182,-1.793724808945,10.9405331141093));
#62848=CARTESIAN_POINT('Ctrl Pts',(2.83219482597701,1.05454220611865,11.0983942252204));
#62849=CARTESIAN_POINT('Ctrl Pts',(0.666859144752323,2.94765765929168,11.2562553363315));
#62850=CARTESIAN_POINT('Ctrl Pts',(-2.10248418004828,2.17093230401124,11.4141164474427));
#62851=CARTESIAN_POINT('Ctrl Pts',(-2.96750254255404,-0.572114900942073,
11.5719775585538));
#62852=CARTESIAN_POINT('Ctrl Pts',(-1.14470559202747,-2.79696905540156,
11.7298386696649));
#62853=CARTESIAN_POINT('Ctrl Pts',(1.7149083997124,-2.48846860088429,11.887699780776));
#62854=CARTESIAN_POINT('Ctrl Pts',(3.02124418299545,0.0739621963506113,
12.0455608918871));
#62855=CARTESIAN_POINT('Ctrl Pts',(1.5910881529614,2.56940172677601,12.2034220029982));
#62856=CARTESIAN_POINT('Ctrl Pts',(-1.28019588317448,2.73760576414863,12.3612831141093));
#62857=CARTESIAN_POINT('Ctrl Pts',(-2.99194259782208,0.42622345054612,12.5191442252204));
#62858=CARTESIAN_POINT('Ctrl Pts',(-1.99373732809816,-2.27121066426194,
12.6770053363315));
#62859=CARTESIAN_POINT('Ctrl Pts',(0.810295268142284,-2.91149594753796,
12.8348664474426));
#62860=CARTESIAN_POINT('Ctrl Pts',(2.88040330087848,-0.914693626913434,
12.9927275585538));
#62861=CARTESIAN_POINT('Ctrl Pts',(2.34158550060768,1.91059190586663,13.1505886696649));
#62862=CARTESIAN_POINT('Ctrl Pts',(-0.318122020237242,3.00535985874532,
13.308449780776));
#62863=CARTESIAN_POINT('Ctrl Pts',(-2.68969293020052,1.37802139698889,13.4663108918871));
#62864=CARTESIAN_POINT('Ctrl Pts',(-2.62506999642434,-1.49745637402886,
13.6241720029982));
#62865=CARTESIAN_POINT('Ctrl Pts',(-0.182798762664348,-3.0166198116913,
13.7820331141093));
#62866=CARTESIAN_POINT('Ctrl Pts',(2.42505915129906,-1.80346713879661,13.9398942252204));
#62867=CARTESIAN_POINT('Ctrl Pts',(2.8363879154744,1.04315130448987,14.0977553363316));
#62868=CARTESIAN_POINT('Ctrl Pts',(0.678719414504022,2.94498233669946,14.2556164474426));
#62869=CARTESIAN_POINT('Ctrl Pts',(-2.09381566089348,2.17930624695187,14.4134775585538));
#62870=CARTESIAN_POINT('Ctrl Pts',(-2.96965473472126,-0.560105433864789,
14.5713386696649));
#62871=CARTESIAN_POINT('Ctrl Pts',(-1.15615435252323,-2.79252825612909,
14.729199780776));
#62872=CARTESIAN_POINT('Ctrl Pts',(1.70534551795855,-2.49499454912784,14.8870608918871));
#62873=CARTESIAN_POINT('Ctrl Pts',(3.0206723431321,0.0611861191543108,15.0449220029982));
#62874=CARTESIAN_POINT('Ctrl Pts',(1.60303217457882,2.56424530164419,15.2027831141093));
#62875=CARTESIAN_POINT('Ctrl Pts',(-1.27259428812422,2.74020454798006,15.3606442252204));
#62876=CARTESIAN_POINT('Ctrl Pts',(-2.41193605302479,1.20953196324185,15.4658849659612));
#62877=CARTESIAN_POINT('Ctrl Pts',(-2.53475666268529,0.371481747533179,
15.5185053363315));
#62878=CARTESIAN_POINT('Ctrl Pts',(1.37702479013102,-1.93106208855765,-3.60822483003176E-15));
#62879=CARTESIAN_POINT('Ctrl Pts',(2.01547936988864,-1.47578528057288,0.0526203703703667));
#62880=CARTESIAN_POINT('Ctrl Pts',(2.79497483704674,0.109513025844136,0.157861111111108));
#62881=CARTESIAN_POINT('Ctrl Pts',(1.4349850222035,2.40398352764199,0.315722222222219));
#62882=CARTESIAN_POINT('Ctrl Pts',(-1.225925966736,2.51415445945906,0.473583333333329));
#62883=CARTESIAN_POINT('Ctrl Pts',(-2.77583219058859,0.350577922658662,
0.631444444444441));
#62884=CARTESIAN_POINT('Ctrl Pts',(-1.811854660541,-2.13232126716645,0.789305555555552));
#62885=CARTESIAN_POINT('Ctrl Pts',(0.793380919254056,-2.68293732976497,
0.947166666666663));
#62886=CARTESIAN_POINT('Ctrl Pts',(2.67992237177449,-0.803971281251394,
1.10502777777777));
#62887=CARTESIAN_POINT('Ctrl Pts',(2.13917103413275,1.80344728451176,1.26288888888888));
#62888=CARTESIAN_POINT('Ctrl Pts',(-0.339158877291603,2.77725977180218,
1.42075));
#62889=CARTESIAN_POINT('Ctrl Pts',(-2.51028282755341,1.23563935306431,1.57861111111111));
#62890=CARTESIAN_POINT('Ctrl Pts',(-2.40772491700405,-1.42519801484247,
1.73647222222222));
#62891=CARTESIAN_POINT('Ctrl Pts',(-0.124366744542119,-2.79514315034066,
1.89433333333333));
#62892=CARTESIAN_POINT('Ctrl Pts',(2.27163476293377,-1.63339753074864,2.05219444444444));
#62893=CARTESIAN_POINT('Ctrl Pts',(2.61010413592219,1.00780309522069,2.21005555555555));
#62894=CARTESIAN_POINT('Ctrl Pts',(0.584471286669745,2.73618335546233,2.36791666666667));
#62895=CARTESIAN_POINT('Ctrl Pts',(-1.97054614371495,1.98626708970809,2.52577777777777));
#62896=CARTESIAN_POINT('Ctrl Pts',(-2.7407416200716,-0.562711268389121,
2.68363888888889));
#62897=CARTESIAN_POINT('Ctrl Pts',(-1.02851040967351,-2.60201352259292,
2.84149999999999));
#62898=CARTESIAN_POINT('Ctrl Pts',(1.61529402596567,-2.28454233775194,2.99936111111111));
#62899=CARTESIAN_POINT('Ctrl Pts',(2.79604598097933,0.102153087721166,3.15722222222222));
#62900=CARTESIAN_POINT('Ctrl Pts',(1.44427938842878,2.39632330140064,3.31508333333333));
#62901=CARTESIAN_POINT('Ctrl Pts',(-1.21564319790733,2.5200238088076,3.47294444444445));
#62902=CARTESIAN_POINT('Ctrl Pts',(-2.77449700843608,0.361212835082494,
3.63080555555555));
#62903=CARTESIAN_POINT('Ctrl Pts',(-1.82035026131238,-2.12476664167876,
3.78866666666667));
#62904=CARTESIAN_POINT('Ctrl Pts',(0.782578662553965,-2.68623882063674,
3.94652777777777));
#62905=CARTESIAN_POINT('Ctrl Pts',(2.67668699402767,-0.814650291328897,
4.10438888888889));
#62906=CARTESIAN_POINT('Ctrl Pts',(2.14638618582228,1.79480770611467,4.26225));
#62907=CARTESIAN_POINT('Ctrl Pts',(-0.328003825581952,2.77861869501174,
4.42011111111111));
#62908=CARTESIAN_POINT('Ctrl Pts',(-2.50530438493649,1.24569590997036,4.57797222222222));
#62909=CARTESIAN_POINT('Ctrl Pts',(-2.41342559623202,-1.41551589631959,
4.73583333333333));
#62910=CARTESIAN_POINT('Ctrl Pts',(-0.135586668767159,-2.79462423533096,
4.89369444444444));
#62911=CARTESIAN_POINT('Ctrl Pts',(2.2650598786042,-1.64250178316317,5.05155555555556));
#62912=CARTESIAN_POINT('Ctrl Pts',(2.61412853009539,0.997316594419356,5.20941666666666));
#62913=CARTESIAN_POINT('Ctrl Pts',(0.595450368366912,2.73381550588105,5.36727777777778));
#62914=CARTESIAN_POINT('Ctrl Pts',(-1.96255694106964,1.99416113050815,5.52513888888888));
#62915=CARTESIAN_POINT('Ctrl Pts',(-2.74297837839289,-0.551704610313744,
5.683));
#62916=CARTESIAN_POINT('Ctrl Pts',(-1.03894725747156,-2.59786392206505,
5.84086111111111));
#62917=CARTESIAN_POINT('Ctrl Pts',(1.60611030100396,-2.29100808867664,5.99872222222222));
#62918=CARTESIAN_POINT('Ctrl Pts',(2.79643351757374,0.090928230838667,6.15658333333333));
#62919=CARTESIAN_POINT('Ctrl Pts',(1.45388718569001,2.39050630885174,6.31444444444444));
#62920=CARTESIAN_POINT('Ctrl Pts',(-1.20551740739643,2.52488339173069,6.47230555555556));
#62921=CARTESIAN_POINT('Ctrl Pts',(-2.77302465619186,0.372347441948222,
6.63016666666666));
#62922=CARTESIAN_POINT('Ctrl Pts',(-1.82886493180883,-2.11744218872047,
6.78802777777778));
#62923=CARTESIAN_POINT('Ctrl Pts',(0.771789132562049,-2.68935864031417,
6.94588888888888));
#62924=CARTESIAN_POINT('Ctrl Pts',(2.67339522049833,-0.825388609316905,
7.10375));
#62925=CARTESIAN_POINT('Ctrl Pts',(2.15357369271338,1.7861771220756,7.26161111111111));
#62926=CARTESIAN_POINT('Ctrl Pts',(-0.3168471224657,2.77991299546561,7.41947222222222));
#62927=CARTESIAN_POINT('Ctrl Pts',(-2.50028366894498,1.25574278265114,7.57733333333334));
#62928=CARTESIAN_POINT('Ctrl Pts',(-2.41908838070749,-1.40581640611404,
7.73519444444443));
#62929=CARTESIAN_POINT('Ctrl Pts',(-0.146803886877873,-2.79405744038503,
7.89305555555557));
#62930=CARTESIAN_POINT('Ctrl Pts',(2.25844822171206,-1.65158105802259,8.05091666666665));
#62931=CARTESIAN_POINT('Ctrl Pts',(2.61811094239596,0.986814802625037,8.20877777777778));
#62932=CARTESIAN_POINT('Ctrl Pts',(0.606419780073446,2.73140319464357,8.36663888888888));
#62933=CARTESIAN_POINT('Ctrl Pts',(-1.95453607417732,2.00202325064244,8.52450000000001));
#62934=CARTESIAN_POINT('Ctrl Pts',(-2.74517095618734,-0.540689173813247,
8.68236111111111));
#62935=CARTESIAN_POINT('Ctrl Pts',(-1.04936735270146,-2.59367240037321,
8.84022222222223));
#62936=CARTESIAN_POINT('Ctrl Pts',(1.59690068918271,-2.29743695240177,8.99808333333332));
#62937=CARTESIAN_POINT('Ctrl Pts',(2.79677599470576,0.0797019247629725,
9.15594444444445));
#62938=CARTESIAN_POINT('Ctrl Pts',(1.46347155312646,2.38465078671139,9.31380555555555));
#62939=CARTESIAN_POINT('Ctrl Pts',(-1.19537219008389,2.52970229247383,9.47166666666666));
#62940=CARTESIAN_POINT('Ctrl Pts',(-2.77150761918447,0.383476046416537,
9.62952777777778));
#62941=CARTESIAN_POINT('Ctrl Pts',(-1.83735013131669,-2.1100836135863,9.78738888888888));
#62942=CARTESIAN_POINT('Ctrl Pts',(0.760987165659879,-2.69243512365168,
9.94525));
#62943=CARTESIAN_POINT('Ctrl Pts',(2.6700603672968,-0.836113626465368,10.1031111111111));
#62944=CARTESIAN_POINT('Ctrl Pts',(2.16072649637127,1.7775177549783,10.2609722222222));
#62945=CARTESIAN_POINT('Ctrl Pts',(-0.305685313585232,2.78116249982291,
10.4188333333333));
#62946=CARTESIAN_POINT('Ctrl Pts',(-2.4952226627859,1.26576941994835,10.5766944444444));
#62947=CARTESIAN_POINT('Ctrl Pts',(-2.42471218341845,-1.39609426222898,
10.7345555555556));
#62948=CARTESIAN_POINT('Ctrl Pts',(-0.158018739337926,-2.79344562132492,
10.8924166666667));
#62949=CARTESIAN_POINT('Ctrl Pts',(2.25180017160661,-1.66063371893121,11.0502777777778));
#62950=CARTESIAN_POINT('Ctrl Pts',(2.62205116590109,0.976297109112734,11.2081388888889));
#62951=CARTESIAN_POINT('Ctrl Pts',(0.617379419647229,2.72894686881467,11.366));
#62952=CARTESIAN_POINT('Ctrl Pts',(-1.9464837111559,2.00985310989732,11.5238611111111));
#62953=CARTESIAN_POINT('Ctrl Pts',(-2.74731929814685,-0.529665024907718,
11.6817222222222));
#62954=CARTESIAN_POINT('Ctrl Pts',(-1.05977053720295,-2.58943908287633,
11.8395833333333));
#62955=CARTESIAN_POINT('Ctrl Pts',(1.58766534266525,-2.30382879610199,11.9974444444444));
#62956=CARTESIAN_POINT('Ctrl Pts',(2.79707340746319,0.0684743370742143,
12.1553055555555));
#62957=CARTESIAN_POINT('Ctrl Pts',(1.47303233105958,2.37875683253439,12.3131666666667));
#62958=CARTESIAN_POINT('Ctrl Pts',(-1.18520769732058,2.53448043892505,12.4710277777778));
#62959=CARTESIAN_POINT('Ctrl Pts',(-2.76994594615232,0.394598452475193,
12.6288888888889));
#62960=CARTESIAN_POINT('Ctrl Pts',(-1.8458056761109,-2.1026909997905,12.78675));
#62961=CARTESIAN_POINT('Ctrl Pts',(0.750172845833004,-2.69546828972993,
12.9446111111111));
#62962=CARTESIAN_POINT('Ctrl Pts',(2.66668266040929,-0.846825037914988,
13.1024722222222));
#62963=CARTESIAN_POINT('Ctrl Pts',(2.16784415239069,1.76882949166842,13.2603333333333));
#62964=CARTESIAN_POINT('Ctrl Pts',(-0.294517949969841,2.78236767093066,
13.4181944444444));
#62965=CARTESIAN_POINT('Ctrl Pts',(-2.49012264935389,1.27577473748293,13.5760555555556));
#62966=CARTESIAN_POINT('Ctrl Pts',(-2.43029461870512,-1.3863478583448,13.7339166666666));
#62967=CARTESIAN_POINT('Ctrl Pts',(-0.16923542984156,-2.79279215602584,
13.8917777777778));
#62968=CARTESIAN_POINT('Ctrl Pts',(2.24512421134353,-1.66965318578134,14.0496388888889));
#62969=CARTESIAN_POINT('Ctrl Pts',(2.62593313585052,0.965751391486786,14.2075));
#62970=CARTESIAN_POINT('Ctrl Pts',(0.628359679142483,2.72647005025058,14.3653611111111));
#62971=CARTESIAN_POINT('Ctrl Pts',(-1.93845838021891,2.01760572163479,14.5232222222222));
#62972=CARTESIAN_POINT('Ctrl Pts',(-2.74931180160372,-0.518546638254714,
14.6810833333333));
#62973=CARTESIAN_POINT('Ctrl Pts',(-1.07036982067409,-2.58532778276268,
14.8389444444444));
#62974=CARTESIAN_POINT('Ctrl Pts',(1.57881200919325,-2.30987053095853,14.9968055555556));
#62975=CARTESIAN_POINT('Ctrl Pts',(2.79654399706859,0.0566462213665858,
15.1546666666667));
#62976=CARTESIAN_POINT('Ctrl Pts',(1.48409012818578,2.37398300468726,15.3125277777778));
#62977=CARTESIAN_POINT('Ctrl Pts',(-1.17817012667699,2.53688639776398,15.4703888888889));
#62978=CARTESIAN_POINT('Ctrl Pts',(-2.23297482288527,1.11978691060522,15.5756296296296));
#62979=CARTESIAN_POINT('Ctrl Pts',(-2.34668236863854,0.343918483395395,
15.62825));
#62980=CARTESIAN_POINT('',(1.37702479013102,-1.93106208855765,0.));
#62981=CARTESIAN_POINT('Ctrl Pts',(1.37702479013102,-1.93106208855765,-3.60822483003176E-15));
#62982=CARTESIAN_POINT('Ctrl Pts',(2.01547936988864,-1.47578528057288,0.0526203703703667));
#62983=CARTESIAN_POINT('Ctrl Pts',(2.79497483704674,0.109513025844136,0.157861111111108));
#62984=CARTESIAN_POINT('Ctrl Pts',(1.4349850222035,2.40398352764199,0.315722222222219));
#62985=CARTESIAN_POINT('Ctrl Pts',(-1.225925966736,2.51415445945906,0.473583333333329));
#62986=CARTESIAN_POINT('Ctrl Pts',(-2.32453883371355,0.980556500150706,
0.585479295290919));
#62987=CARTESIAN_POINT('Ctrl Pts',(-2.37485146083742,0.100616720091163,
0.644754886878137));
#62988=CARTESIAN_POINT('Ctrl Pts',(-2.37409249406917,0.00172857025301858,
0.651410108094986));
#62989=CARTESIAN_POINT('Ctrl Pts',(1.29200104020317,2.64812001020929,8.84708972748172E-17));
#62990=CARTESIAN_POINT('Ctrl Pts',(1.36315737313149,2.60529414881161,1.11522009070411E-16));
#62991=CARTESIAN_POINT('Ctrl Pts',(1.43224767624703,2.55934891308958,-5.0435019692162E-16));
#62992=CARTESIAN_POINT('Ctrl Pts',(1.49903325513988,2.51027466650741,-4.38885039422132E-16));
#62993=CARTESIAN_POINT('Ctrl Pts',(1.57786836962904,2.45234638450537,-3.65724347932505E-16));
#62994=CARTESIAN_POINT('Ctrl Pts',(1.65349331585608,2.39005818913334,-5.19266877679362E-16));
#62995=CARTESIAN_POINT('Ctrl Pts',(1.72573019513852,2.32378926839401,-6.48786580015326E-16));
#62996=CARTESIAN_POINT('Ctrl Pts',(1.76374109312884,2.28891869797108,-7.16939582223243E-16));
#62997=CARTESIAN_POINT('Ctrl Pts',(1.80081318017132,2.2529453987339,-5.63901193634668E-16));
#62998=CARTESIAN_POINT('Ctrl Pts',(1.83691551656788,2.21592189026143,-5.759281940243E-16));
#62999=CARTESIAN_POINT('Ctrl Pts',(1.85077163488616,2.20171222503873,-5.80544170635404E-16));
#63000=CARTESIAN_POINT('Ctrl Pts',(1.86448486767998,2.18734784556943,1.18680337545582E-16));
#63001=CARTESIAN_POINT('Ctrl Pts',(1.87805332095389,2.17283167229843,1.45716771982052E-16));
#63002=CARTESIAN_POINT('Ctrl Pts',(1.88973877018296,2.16033002584437,1.69001141656681E-16));
#63003=CARTESIAN_POINT('Ctrl Pts',(1.90131548250979,2.14771713833219,-1.20552840767492E-16));
#63004=CARTESIAN_POINT('Ctrl Pts',(1.91277473204616,2.1350036118777,-1.04083408558608E-16));
#63005=CARTESIAN_POINT('Ctrl Pts',(1.9778462733255,2.06280963801715,-1.05614606835039E-17));
#63006=CARTESIAN_POINT('Ctrl Pts',(2.03920496551099,1.98729716595704,-4.81412066085989E-16));
#63007=CARTESIAN_POINT('Ctrl Pts',(2.09668120715734,1.90884345828848,-3.33066907387547E-16));
#63008=CARTESIAN_POINT('Ctrl Pts',(2.14417843271961,1.84401087107344,-2.10477411937863E-16));
#63009=CARTESIAN_POINT('Ctrl Pts',(2.18902362087598,1.7771688452355,-1.7119245770294E-16));
#63010=CARTESIAN_POINT('Ctrl Pts',(2.23109606376114,1.7085204430367,-1.94289029309402E-16));
#63011=CARTESIAN_POINT('Ctrl Pts',(2.24950275752339,1.67848676707472,-2.0439377938723E-16));
#63012=CARTESIAN_POINT('Ctrl Pts',(2.26737842523222,1.6481072631063,-4.61788465798711E-16));
#63013=CARTESIAN_POINT('Ctrl Pts',(2.28471149018554,1.61739870311764,-5.13478148889135E-16));
#63014=CARTESIAN_POINT('Ctrl Pts',(2.29518347047447,1.59884575614786,-5.44707094486553E-16));
#63015=CARTESIAN_POINT('Ctrl Pts',(2.30545737670969,1.58017269818218,-5.13081578012294E-16));
#63016=CARTESIAN_POINT('Ctrl Pts',(2.3155304906665,1.56138322284078,-5.55111512312578E-16));
#63017=CARTESIAN_POINT('Ctrl Pts',(2.32274660107223,1.54792294341672,-5.85220637212436E-16));
#63018=CARTESIAN_POINT('Ctrl Pts',(2.32985933504635,1.5344033850802,-2.08590721469464E-17));
#63019=CARTESIAN_POINT('Ctrl Pts',(2.33686168047272,1.52083799385098,-2.77555756156289E-17));
#63020=CARTESIAN_POINT('Ctrl Pts',(2.38047027627073,1.43635663411551,-7.07050181056999E-17));
#63021=CARTESIAN_POINT('Ctrl Pts',(2.41986655819018,1.34997905359849,1.3198210981114E-16));
#63022=CARTESIAN_POINT('Ctrl Pts',(2.45488985599288,1.26205357875123,5.55111512312578E-17));
#63023=CARTESIAN_POINT('Ctrl Pts',(2.48959846523414,1.17491812491653,-2.02727065483809E-17));
#63024=CARTESIAN_POINT('Ctrl Pts',(2.52001253380174,1.08626153918075,-4.44579204063227E-16));
#63025=CARTESIAN_POINT('Ctrl Pts',(2.54592562425351,0.996413712953991,-4.9960036108132E-16));
#63026=CARTESIAN_POINT('Ctrl Pts',(2.57101139534936,0.909434430942866,-5.528648743571E-16));
#63027=CARTESIAN_POINT('Ctrl Pts',(2.59187898968551,0.821337996875181,-7.89241560757653E-18));
#63028=CARTESIAN_POINT('Ctrl Pts',(2.60829286172102,0.732427405689614,-8.32667268468867E-17));
#63029=CARTESIAN_POINT('Ctrl Pts',(2.61783087340729,0.680761945161682,-1.27066328786625E-16));
#63030=CARTESIAN_POINT('Ctrl Pts',(2.62586408863254,0.628821695636964,-4.14952786105416E-17));
#63031=CARTESIAN_POINT('Ctrl Pts',(2.63233843305125,0.576668196894126,-5.55111512312578E-17));
#63032=CARTESIAN_POINT('Ctrl Pts',(2.63414224296016,0.562137768524485,-5.94160979378542E-17));
#63033=CARTESIAN_POINT('Ctrl Pts',(2.63582527555606,0.547588319420663,3.76279563716787E-16));
#63034=CARTESIAN_POINT('Ctrl Pts',(2.63738542604938,0.533029261526728,3.60822483003176E-16));
#63035=CARTESIAN_POINT('Ctrl Pts',(2.64690685377435,0.444176924476997,2.66489610960485E-16));
#63036=CARTESIAN_POINT('Ctrl Pts',(2.65183263786108,0.355196731300303,5.62349138697447E-16));
#63037=CARTESIAN_POINT('Ctrl Pts',(2.65198717743404,0.266381980286723,3.88578058618805E-16));
#63038=CARTESIAN_POINT('Ctrl Pts',(2.65207998114243,0.213047173573617,2.84225494854879E-16));
#63039=CARTESIAN_POINT('Ctrl Pts',(2.65045121279133,0.159772024909719,-3.854419951949E-17));
#63040=CARTESIAN_POINT('Ctrl Pts',(2.64705383408491,0.106621318043217,-8.32667268468867E-17));
#63041=CARTESIAN_POINT('Ctrl Pts',(2.64128166054733,0.0163178428672467,
-1.29468843946197E-16));
#63042=CARTESIAN_POINT('Ctrl Pts',(2.63040647827402,-0.0736278476965388,
-4.84995897836269E-16));
#63043=CARTESIAN_POINT('Ctrl Pts',(2.61462343406994,-0.162881882998066,
-6.10622663543836E-16));
#63044=CARTESIAN_POINT('Ctrl Pts',(2.59852152905154,-0.253939094797703,
-7.38787434739808E-16));
#63045=CARTESIAN_POINT('Ctrl Pts',(2.57731092756958,-0.344277415185344,
-3.0810955291451E-16));
#63046=CARTESIAN_POINT('Ctrl Pts',(2.55115372858487,-0.433510589178544,
-3.60822483003176E-16));
#63047=CARTESIAN_POINT('Ctrl Pts',(2.54730992415644,-0.446623417870874,
-3.68568656216471E-16));
#63048=CARTESIAN_POINT('Ctrl Pts',(2.54335838534963,-0.4597150170452,-1.33461876853334E-16));
#63049=CARTESIAN_POINT('Ctrl Pts',(2.53930241226215,-0.472774949708627,
-1.38777878078145E-16));
#63050=CARTESIAN_POINT('Ctrl Pts',(2.51300579541719,-0.557448106523011,
-1.73243798916645E-16));
#63051=CARTESIAN_POINT('Ctrl Pts',(2.48237490705721,-0.640633082262047,
2.2266366763076E-16));
#63052=CARTESIAN_POINT('Ctrl Pts',(2.4476284488952,-0.722031078376524,1.66533453693773E-16));
#63053=CARTESIAN_POINT('Ctrl Pts',(2.41285997251409,-0.803480654968775,
1.10367671027941E-16));
#63054=CARTESIAN_POINT('Ctrl Pts',(2.37397005509887,-0.883141781461701,
-2.60473824643759E-16));
#63055=CARTESIAN_POINT('Ctrl Pts',(2.33113438836321,-0.960686402199183,
-2.22044604925031E-16));
#63056=CARTESIAN_POINT('Ctrl Pts',(2.28891526223189,-1.03711491080453,-1.84168503113759E-16));
#63057=CARTESIAN_POINT('Ctrl Pts',(2.24286247138705,-1.11148803969701,-4.86311355035046E-16));
#63058=CARTESIAN_POINT('Ctrl Pts',(2.19311210725222,-1.18345333925267,-6.10622663543836E-16));
#63059=CARTESIAN_POINT('Ctrl Pts',(2.16658994742807,-1.22181838863071,-6.76893623556989E-16));
#63060=CARTESIAN_POINT('Ctrl Pts',(2.13901644812981,-1.25949841963374,-1.03661145615814E-16));
#63061=CARTESIAN_POINT('Ctrl Pts',(2.11040940583919,-1.29643454206688,-5.55111512312578E-17));
#63062=CARTESIAN_POINT('Ctrl Pts',(2.10166865720486,-1.30772020237512,-4.0799144537779E-17));
#63063=CARTESIAN_POINT('Ctrl Pts',(2.09283023898332,-1.31893783850973,-3.98702450321844E-16));
#63064=CARTESIAN_POINT('Ctrl Pts',(2.08389831377262,-1.33008110200649,-3.88578058618805E-16));
#63065=CARTESIAN_POINT('Ctrl Pts',(2.03043260129099,-1.39678368942974,-3.27974347428123E-16));
#63066=CARTESIAN_POINT('Ctrl Pts',(1.97380215986925,-1.46059813131217,-2.08556400160018E-16));
#63067=CARTESIAN_POINT('Ctrl Pts',(1.91417150281915,-1.52123259912064,-1.11022302462516E-16));
#63068=CARTESIAN_POINT('Ctrl Pts',(1.85542332105702,-1.58096973622562,-1.49316138302572E-17));
#63069=CARTESIAN_POINT('Ctrl Pts',(1.79376241718216,-1.63762085789259,-5.35520206863283E-16));
#63070=CARTESIAN_POINT('Ctrl Pts',(1.72931881925135,-1.69086532717403,-5.55111512312578E-16));
#63071=CARTESIAN_POINT('Ctrl Pts',(1.66690919772329,-1.7424292882658,-5.74084474679515E-16));
#63072=CARTESIAN_POINT('Ctrl Pts',(1.60188918190129,-1.79079854027645,-4.05239810717764E-16));
#63073=CARTESIAN_POINT('Ctrl Pts',(1.53436012060039,-1.83563678794726,-4.44089209850063E-16));
#63074=CARTESIAN_POINT('Ctrl Pts',(1.48333459704145,-1.8695169429323,-4.73444140786276E-16));
#63075=CARTESIAN_POINT('Ctrl Pts',(1.43087616732457,-1.90138023485661,-2.26823314612322E-16));
#63076=CARTESIAN_POINT('Ctrl Pts',(1.37702479013106,-1.93106208855762,-2.22044604925031E-16));
#63077=CARTESIAN_POINT('Ctrl Pts',(0.260984867623806,2.92515103163649,15.058));
#63078=CARTESIAN_POINT('Ctrl Pts',(0.721611965671866,2.88493263312463,15.0330979289241));
#63079=CARTESIAN_POINT('Ctrl Pts',(1.17298362662806,2.74202417939443,15.0081958578483));
#63080=CARTESIAN_POINT('Ctrl Pts',(1.56185858228333,2.49936439089571,14.9832937867724));
#63081=CARTESIAN_POINT('Ctrl Pts',(2.3835871899963,1.98660190194863,14.930673416402));
#63082=CARTESIAN_POINT('Ctrl Pts',(2.92625811262771,1.02843390833919,14.8780530460316));
#63083=CARTESIAN_POINT('Ctrl Pts',(2.94584082398175,0.0600984948350938,
14.8254326756613));
#63084=CARTESIAN_POINT('Ctrl Pts',(2.96542353533579,-0.90823691866899,14.7728123052909));
#63085=CARTESIAN_POINT('Ctrl Pts',(2.46191803541247,-1.88673975206773,14.7201919349205));
#63086=CARTESIAN_POINT('Ctrl Pts',(1.6624759601657,-2.43293893833301,14.6675715645502));
#63087=CARTESIAN_POINT('Ctrl Pts',(0.863033884918936,-2.97913812459828,
14.6149511941798));
#63088=CARTESIAN_POINT('Ctrl Pts',(-0.232344765651281,-3.0930336637301,
14.5623308238094));
#63089=CARTESIAN_POINT('Ctrl Pts',(-1.12713695505886,-2.72269707033318,
14.5097104534391));
#63090=CARTESIAN_POINT('Ctrl Pts',(-2.02192914446644,-2.35236047693625,
14.4570900830687));
#63091=CARTESIAN_POINT('Ctrl Pts',(-2.71613487271139,-1.49779175101059,
14.4044697126983));
#63092=CARTESIAN_POINT('Ctrl Pts',(-2.89560267371491,-0.546185667602603,
14.351849342328));
#63093=CARTESIAN_POINT('Ctrl Pts',(-2.9293373183321,-0.367311836977727,
14.3419582672485));
#63094=CARTESIAN_POINT('Ctrl Pts',(-2.94488478294563,-0.185009395803266,
14.3320671921691));
#63095=CARTESIAN_POINT('Ctrl Pts',(-2.94325266537063,-0.0024318079996577,
14.3221761170896));
#63096=CARTESIAN_POINT('Origin',(0.,0.,-1.84858989190501));
#63097=CARTESIAN_POINT('',(-1.37702479013098,-1.93106208855768,0.));
#63098=CARTESIAN_POINT('Ctrl Pts',(-1.37994859234593,-1.93347131995891,
-1.03866568124111E-15));
#63099=CARTESIAN_POINT('Ctrl Pts',(-0.794305021574331,-2.34617453422284,
0.0482502273315914));
#63100=CARTESIAN_POINT('Ctrl Pts',(0.853330802601401,-2.62819893329841,
0.149165418329868));
#63101=CARTESIAN_POINT('Ctrl Pts',(2.68321992772198,-0.795544356782894,
0.30274557299483));
#63102=CARTESIAN_POINT('Ctrl Pts',(2.13222685489998,1.81318819272267,0.460740463994884));
#63103=CARTESIAN_POINT('Ctrl Pts',(-0.353356050373597,2.77617865909866,
0.618735354994938));
#63104=CARTESIAN_POINT('Ctrl Pts',(-2.12480812784407,1.50378450145058,0.74801849763165));
#63105=CARTESIAN_POINT('Ctrl Pts',(-2.36883710346974,0.358840951777969,
0.824636676601679));
#63106=CARTESIAN_POINT('Ctrl Pts',(-2.36806791026422,0.000580996437929554,
0.848589891905023));
#63107=CARTESIAN_POINT('Origin',(0.,0.,0.));
#63108=CARTESIAN_POINT('Ctrl Pts',(-1.03908919352511,2.13201587949043,-0.329233991005384));
#63109=CARTESIAN_POINT('Ctrl Pts',(-1.74458119175558,1.78817739379635,-0.2765690273387));
#63110=CARTESIAN_POINT('Ctrl Pts',(-2.77573338088225,0.351504794741619,
-0.171239100005331));
#63111=CARTESIAN_POINT('Ctrl Pts',(-1.80933791412281,-2.1375423700464,-0.013244209005277));
#63112=CARTESIAN_POINT('Ctrl Pts',(0.800729748594893,-2.68087948155196,
0.144750681994776));
#63113=CARTESIAN_POINT('Ctrl Pts',(2.68321992772198,-0.795544356782894,
0.30274557299483));
#63114=CARTESIAN_POINT('Ctrl Pts',(2.13222685489998,1.81318819272267,0.460740463994884));
#63115=CARTESIAN_POINT('Ctrl Pts',(-0.353356050373597,2.77617865909866,
0.618735354994938));
#63116=CARTESIAN_POINT('Ctrl Pts',(-2.51821971460423,1.2212058130903,0.77673024599499));
#63117=CARTESIAN_POINT('Ctrl Pts',(-2.39875016986203,-1.44183805604875,
0.934725136995045));
#63118=CARTESIAN_POINT('Ctrl Pts',(-0.103189861818606,-2.79677945469355,
1.0927200279951));
#63119=CARTESIAN_POINT('Ctrl Pts',(2.28595558559378,-1.6146683983646,1.25071491899515));
#63120=CARTESIAN_POINT('Ctrl Pts',(2.60139192527736,1.0322363870214,1.4087098099952));
#63121=CARTESIAN_POINT('Ctrl Pts',(0.556949311928898,2.7427217714679,1.56670470099526));
#63122=CARTESIAN_POINT('Ctrl Pts',(-1.99273057992189,1.96513605211958,1.72469959199531));
#63123=CARTESIAN_POINT('Ctrl Pts',(-2.73469173326279,-0.595142683011921,
1.88269448299537));
#63124=CARTESIAN_POINT('Ctrl Pts',(-0.995855715555496,-2.61553061219188,
2.04068937399542));
#63125=CARTESIAN_POINT('Ctrl Pts',(1.64637781974439,-2.26322161422709,2.19868426499547));
#63126=CARTESIAN_POINT('Ctrl Pts',(2.79508756969503,0.142186649832604,2.35667915599553));
#63127=CARTESIAN_POINT('Ctrl Pts',(1.40821242874264,2.41860884498944,2.51467404699558));
#63128=CARTESIAN_POINT('Ctrl Pts',(-1.25613315819632,2.50097199645567,2.67266893799564));
#63129=CARTESIAN_POINT('Ctrl Pts',(-2.78096812139655,0.314559449318749,
2.83066382899569));
#63130=CARTESIAN_POINT('Ctrl Pts',(-1.78302687496254,-2.15720801874703,
2.98865871999574));
#63131=CARTESIAN_POINT('Ctrl Pts',(0.832400628534772,-2.67204800324426,
3.1466536109958));
#63132=CARTESIAN_POINT('Ctrl Pts',(2.69270963387839,-0.762919488957052,
3.30464850199585));
#63133=CARTESIAN_POINT('Ctrl Pts',(2.11030679852043,1.83829718168443,3.4626433929959));
#63134=CARTESIAN_POINT('Ctrl Pts',(-0.386476751895552,2.77188871376435,
3.62063828399595));
#63135=CARTESIAN_POINT('Ctrl Pts',(-2.53266500493224,1.1909405067813,3.77863317499601));
#63136=CARTESIAN_POINT('Ctrl Pts',(-2.38132711099884,-1.47037835529628,
3.93662806599605));
#63137=CARTESIAN_POINT('Ctrl Pts',(-0.0697503817448946,-2.79783241149437,
4.09462295699612));
#63138=CARTESIAN_POINT('Ctrl Pts',(2.30510093209087,-1.58721170953314,4.25261784799616));
#63139=CARTESIAN_POINT('Ctrl Pts',(2.5888625630092,1.06326005653742,4.41061273899623));
#63140=CARTESIAN_POINT('Ctrl Pts',(0.524118009051023,2.74918744918107,4.56860762999628));
#63141=CARTESIAN_POINT('Ctrl Pts',(-2.01608414683087,1.9411687281004,4.72660252099633));
#63142=CARTESIAN_POINT('Ctrl Pts',(-2.72738037475851,-0.627795834204506,
4.88459741199638));
#63143=CARTESIAN_POINT('Ctrl Pts',(-0.964512940920624,-2.62725067416123,
5.04259230299644));
#63144=CARTESIAN_POINT('Ctrl Pts',(1.67331967629405,-2.24337526486265,5.20058719399648));
#63145=CARTESIAN_POINT('Ctrl Pts',(2.79318773824162,0.175594923072764,5.35858208499656));
#63146=CARTESIAN_POINT('Ctrl Pts',(1.37919449268132,2.43527285317938,5.51657697599659));
#63147=CARTESIAN_POINT('Ctrl Pts',(-1.28594543116668,2.48577466117395,5.67457186699666));
#63148=CARTESIAN_POINT('Ctrl Pts',(-2.78453026564846,0.281287251330417,
5.8325667579967));
#63149=CARTESIAN_POINT('Ctrl Pts',(-1.75710748413146,-2.17837200846936,
5.99056164899676));
#63150=CARTESIAN_POINT('Ctrl Pts',(0.864288593995119,-2.66190468356086,
6.14855653999681));
#63151=CARTESIAN_POINT('Ctrl Pts',(2.70163876039796,-0.730670463607777,
6.30655143099686));
#63152=CARTESIAN_POINT('Ctrl Pts',(2.08817696449889,1.86339697407977,6.46454632199692));
#63153=CARTESIAN_POINT('Ctrl Pts',(-0.419590302218696,2.76706980330411,
6.62254121299697));
#63154=CARTESIAN_POINT('Ctrl Pts',(-2.54672306405081,1.16057440653543,6.78053610399702));
#63155=CARTESIAN_POINT('Ctrl Pts',(-2.3635768050391,-1.49874480975067,6.93853099499709));
#63156=CARTESIAN_POINT('Ctrl Pts',(-0.0362940343214689,-2.79846637663312,
7.09652588599712));
#63157=CARTESIAN_POINT('Ctrl Pts',(2.32391314315961,-1.55953807940794,7.2545207769972));
#63158=CARTESIAN_POINT('Ctrl Pts',(2.57596499873257,1.09413693995685,7.41251566799723));
#63159=CARTESIAN_POINT('Ctrl Pts',(0.491210792034311,2.75525738831465,7.5705105589973));
#63160=CARTESIAN_POINT('Ctrl Pts',(-2.03914898665099,1.91692533196097,7.72850544999735));
#63161=CARTESIAN_POINT('Ctrl Pts',(-2.71967939412015,-0.66035998612245,
7.8865003409974));
#63162=CARTESIAN_POINT('Ctrl Pts',(-0.9330321424437,-2.63859476601473,8.04449523199746));
#63163=CARTESIAN_POINT('Ctrl Pts',(1.70002224901497,-2.22320841823872,8.2024901229975));
#63164=CARTESIAN_POINT('Ctrl Pts',(2.79088864512093,0.208978201275766,8.36048501399757));
#63165=CARTESIAN_POINT('Ctrl Pts',(1.34997937336987,2.45158867054595,8.51847990499762));
#63166=CARTESIAN_POINT('Ctrl Pts',(-1.31557386100644,2.47022200101732,8.67647479599767));
#63167=CARTESIAN_POINT('Ctrl Pts',(-2.78769435259396,0.247974826523285,
8.83446968699772));
#63168=CARTESIAN_POINT('Ctrl Pts',(-1.73093690286391,-2.19922458070505,
8.99246457799778));
#63169=CARTESIAN_POINT('Ctrl Pts',(0.896053003445084,-2.6513808351669,9.15045946899784));
#63170=CARTESIAN_POINT('Ctrl Pts',(2.71018167460651,-0.698316982967359,
9.30845435999788));
#63171=CARTESIAN_POINT('Ctrl Pts',(2.06574861445826,1.88823038317285,9.46644925099794));
#63172=CARTESIAN_POINT('Ctrl Pts',(-0.45264386973844,2.76185532663481,9.62444414199799));
#63173=CARTESIAN_POINT('Ctrl Pts',(-2.5604170561675,1.13004239591331,9.78243903299804));
#63174=CARTESIAN_POINT('Ctrl Pts',(-2.34548861359897,-1.52689701078686,
9.9404339239981));
#63175=CARTESIAN_POINT('Ctrl Pts',(-0.00283249851198579,-2.79870028674429,
10.0984288149982));
#63176=CARTESIAN_POINT('Ctrl Pts',(2.34239313895008,-1.53164150527581,10.2564237059982));
#63177=CARTESIAN_POINT('Ctrl Pts',(2.56269918704329,1.12485741087042,10.4144185969983));
#63178=CARTESIAN_POINT('Ctrl Pts',(0.458233353927178,2.76093344928963,10.5724134879983));
#63179=CARTESIAN_POINT('Ctrl Pts',(-2.06192231968409,1.89240790151988,10.7304083789984));
#63180=CARTESIAN_POINT('Ctrl Pts',(-2.71158962134898,-0.692829736205835,
10.8884032699984));
#63181=CARTESIAN_POINT('Ctrl Pts',(-0.90141796228012,-2.64956165719617,
11.0463981609985));
#63182=CARTESIAN_POINT('Ctrl Pts',(1.72648179491819,-2.20272375262492,11.2043930519985));
#63183=CARTESIAN_POINT('Ctrl Pts',(2.7881905800153,0.242331605070017,11.3623879429986));
#63184=CARTESIAN_POINT('Ctrl Pts',(1.32057126786748,2.46755402056041,11.5203828339987));
#63185=CARTESIAN_POINT('Ctrl Pts',(-1.34501422335496,2.45431621031658,11.6783777249987));
#63186=CARTESIAN_POINT('Ctrl Pts',(-2.79045992331823,0.214626951768239,
11.8363726159988));
#63187=CARTESIAN_POINT('Ctrl Pts',(-1.70451887724915,-2.21976276122321,
11.9943675069988));
#63188=CARTESIAN_POINT('Ctrl Pts',(0.927689321261817,-2.64047796075702,
12.1523623979988));
#63189=CARTESIAN_POINT('Ctrl Pts',(2.71833714731268,-0.66586366962402,12.3103572889989));
#63190=CARTESIAN_POINT('Ctrl Pts',(2.04302496870488,1.91279385105346,12.468352179999));
#63191=CARTESIAN_POINT('Ctrl Pts',(-0.48563275555883,2.75624604578475,12.626347070999));
#63192=CARTESIAN_POINT('Ctrl Pts',(-2.57374497374716,1.09934880708429,12.7843419619991));
#63193=CARTESIAN_POINT('Ctrl Pts',(-2.32706521767492,-1.55483087129818,
12.9423368529991));
#63194=CARTESIAN_POINT('Ctrl Pts',(0.0306296239850783,-2.7985342282319,
13.1003317439992));
#63195=CARTESIAN_POINT('Ctrl Pts',(2.36053793034993,-1.50352574600393,13.2583266349992));
#63196=CARTESIAN_POINT('Ctrl Pts',(2.54906768788899,1.15541663986578,13.4163215259993));
#63197=CARTESIAN_POINT('Ctrl Pts',(0.42518914129335,2.76621565710669,13.5743164169993));
#63198=CARTESIAN_POINT('Ctrl Pts',(-2.08439846825039,1.86761834358563,13.7323113079994));
#63199=CARTESIAN_POINT('Ctrl Pts',(-2.7031168406022,-0.725197389434075,
13.8903061989994));
#63200=CARTESIAN_POINT('Ctrl Pts',(-0.869666078203209,-2.66015561356989,
14.0483010899995));
#63201=CARTESIAN_POINT('Ctrl Pts',(1.75267763866885,-2.18191305067097,14.2062959809995));
#63202=CARTESIAN_POINT('Ctrl Pts',(2.78512620401791,0.275629071355557,14.3642908719996));
#63203=CARTESIAN_POINT('Ctrl Pts',(1.29091271455523,2.48320730756548,14.5222857629997));
#63204=CARTESIAN_POINT('Ctrl Pts',(-1.37414448785656,2.43798182357128,14.6802806539997));
#63205=CARTESIAN_POINT('Ctrl Pts',(-2.79305172314729,0.181396953694044,
14.8382755449998));
#63206=CARTESIAN_POINT('Ctrl Pts',(-1.67742675687761,-2.24026772494819,
14.9962704359998));
#63207=CARTESIAN_POINT('Ctrl Pts',(0.958368222991996,-2.62865236842956,
15.1542653269999));
#63208=CARTESIAN_POINT('Ctrl Pts',(2.7277014223945,-0.634378452891388,15.3122602179999));
#63209=CARTESIAN_POINT('Ctrl Pts',(2.01676643438217,1.93930517753648,15.470255109));
#63210=CARTESIAN_POINT('Ctrl Pts',(0.331786659212352,2.47609764328476,15.5755850363333));
#63211=CARTESIAN_POINT('Ctrl Pts',(-0.439445221994538,2.33068358199181,
15.62825));
#63212=CARTESIAN_POINT('Ctrl Pts',(-1.12236674703448,2.30288577939268,-0.219489327336923));
#63213=CARTESIAN_POINT('Ctrl Pts',(-1.88440023178909,1.93149044095738,-0.166824363670239));
#63214=CARTESIAN_POINT('Ctrl Pts',(-2.99819386511655,0.37967606197771,-0.0614944363368692));
#63215=CARTESIAN_POINT('Ctrl Pts',(-1.9543468660962,-2.30885518920509,0.096500454663184));
#63216=CARTESIAN_POINT('Ctrl Pts',(0.864904041716857,-2.89573792283723,
0.254495345663238));
#63217=CARTESIAN_POINT('Ctrl Pts',(2.89826594350265,-0.859303067925248,
0.412490236663291));
#63218=CARTESIAN_POINT('Ctrl Pts',(2.30311366337569,1.95850572434841,0.570485127663346));
#63219=CARTESIAN_POINT('Ctrl Pts',(-0.381675686047029,2.99867483004853,
0.728480018663398));
#63220=CARTESIAN_POINT('Ctrl Pts',(-2.72004182798788,1.31907905927489,0.886474909663454));
#63221=CARTESIAN_POINT('Ctrl Pts',(-2.59099742531531,-1.55739382028214,
1.0444698006635));
#63222=CARTESIAN_POINT('Ctrl Pts',(-0.111459988476451,-3.02092667145178,
1.20246469166356));
#63223=CARTESIAN_POINT('Ctrl Pts',(2.46916294621846,-1.74407560881646,1.36045958266361));
#63224=CARTESIAN_POINT('Ctrl Pts',(2.80987985548213,1.11496472400166,1.51845447366367));
#63225=CARTESIAN_POINT('Ctrl Pts',(0.60158588058462,2.96253654820512,1.67644936466372));
#63226=CARTESIAN_POINT('Ctrl Pts',(-2.15243749298894,2.12263140839256,1.83444425566377));
#63227=CARTESIAN_POINT('Ctrl Pts',(-2.95386294451934,-0.642840250207365,
1.99243914666383));
#63228=CARTESIAN_POINT('Ctrl Pts',(-1.07566833237088,-2.82515168405898,
2.15043403766388));
#63229=CARTESIAN_POINT('Ctrl Pts',(1.77832637414643,-2.44460696618424,2.30842892866393));
#63230=CARTESIAN_POINT('Ctrl Pts',(3.01909919073696,0.153582164686878,2.46642381966399));
#63231=CARTESIAN_POINT('Ctrl Pts',(1.52107327516274,2.61244766918467,2.62441871066404));
#63232=CARTESIAN_POINT('Ctrl Pts',(-1.35680564805421,2.70141179561648,2.7824136016641));
#63233=CARTESIAN_POINT('Ctrl Pts',(-3.00384814265038,0.339769740731444,
2.94040849266415));
#63234=CARTESIAN_POINT('Ctrl Pts',(-1.92592713503036,-2.33009693659115,
3.0984033836642));
#63235=CARTESIAN_POINT('Ctrl Pts',(0.899113176712534,-2.88619864782458,
3.25639827466426));
#63236=CARTESIAN_POINT('Ctrl Pts',(2.90851619987664,-0.824063487913928,
3.41439316566431));
#63237=CARTESIAN_POINT('Ctrl Pts',(2.27943682934948,1.98562706719167,3.57238805666436));
#63238=CARTESIAN_POINT('Ctrl Pts',(-0.417450838226782,2.99404106807715,
3.73038294766441));
#63239=CARTESIAN_POINT('Ctrl Pts',(-2.73564483263507,1.2863881472707,3.88837783866447));
#63240=CARTESIAN_POINT('Ctrl Pts',(-2.57217799958985,-1.5882214749488,4.04637272966452));
#63241=CARTESIAN_POINT('Ctrl Pts',(-0.0753405093145775,-3.02206401722216,
4.20436762066458));
#63242=CARTESIAN_POINT('Ctrl Pts',(2.48984269190601,-1.71441841026206,4.36236251166463));
#63243=CARTESIAN_POINT('Ctrl Pts',(2.79634633048836,1.1484747780497,4.52035740266469));
#63244=CARTESIAN_POINT('Ctrl Pts',(0.566123320833673,2.9695204161036,4.67835229366474));
#63245=CARTESIAN_POINT('Ctrl Pts',(-2.1776627259012,2.09674322895411,4.83634718466479));
#63246=CARTESIAN_POINT('Ctrl Pts',(-2.94596561894615,-0.678110380349046,
4.99434207566485));
#63247=CARTESIAN_POINT('Ctrl Pts',(-1.04181359860098,-2.83781104757613,
5.1523369666649));
#63248=CARTESIAN_POINT('Ctrl Pts',(1.80742747930962,-2.42317003592312,5.31033185766495));
#63249=CARTESIAN_POINT('Ctrl Pts',(3.01704709774863,0.189667935951029,5.46832674866501));
#63250=CARTESIAN_POINT('Ctrl Pts',(1.48972970359473,2.63044721030322,5.62632163966506));
#63251=CARTESIAN_POINT('Ctrl Pts',(-1.38900721847178,2.68499647355363,5.78431653066512));
#63252=CARTESIAN_POINT('Ctrl Pts',(-3.00769577409666,0.303830950437453,
5.94231142166516));
#63253=CARTESIAN_POINT('Ctrl Pts',(-1.89793044085485,-2.35295710917974,
6.10030631266523));
#63254=CARTESIAN_POINT('Ctrl Pts',(0.933556795495496,-2.87524239422467,
6.25830120366527));
#63255=CARTESIAN_POINT('Ctrl Pts',(2.91816094909363,-0.789229872184075,
6.41629609466533));
#63256=CARTESIAN_POINT('Ctrl Pts',(2.25553340510261,2.01273847641193,6.57429098566538));
#63257=CARTESIAN_POINT('Ctrl Pts',(-0.453218266076613,2.98883594719704,
6.73228587666544));
#63258=CARTESIAN_POINT('Ctrl Pts',(-2.75082957152067,1.25358836322381,6.89028076766548));
#63259=CARTESIAN_POINT('Ctrl Pts',(-2.55300509962799,-1.61886135207317,
7.04827565866555));
#63260=CARTESIAN_POINT('Ctrl Pts',(-0.0392028109733089,-3.02274879134448,
7.20627054966559));
#63261=CARTESIAN_POINT('Ctrl Pts',(2.51016260310644,-1.68452688370611,7.36426544066566));
#63262=CARTESIAN_POINT('Ctrl Pts',(2.78241509402469,1.18182628186475,7.5222603316657));
#63263=CARTESIAN_POINT('Ctrl Pts',(0.530578762823495,2.97607682904918,7.68025522266576));
#63264=CARTESIAN_POINT('Ctrl Pts',(-2.2025760917615,2.07055685166173,7.83825011366581));
#63265=CARTESIAN_POINT('Ctrl Pts',(-2.93764744506665,-0.713284378390626,
7.99624500466586));
#63266=CARTESIAN_POINT('Ctrl Pts',(-1.0078097791014,-2.85006430894292,8.15423989566592));
#63267=CARTESIAN_POINT('Ctrl Pts',(1.83627012329917,-2.40138692222673,8.31223478666596));
#63268=CARTESIAN_POINT('Ctrl Pts',(3.01456374436274,0.225726708956776,8.47022967766603));
#63269=CARTESIAN_POINT('Ctrl Pts',(1.45817314557243,2.64807065492862,8.62822456866608));
#63270=CARTESIAN_POINT('Ctrl Pts',(-1.42101021169528,2.66819734918923,8.78621945966612));
#63271=CARTESIAN_POINT('Ctrl Pts',(-3.01111344602942,0.267848709355943,
8.9442143506662));
#63272=CARTESIAN_POINT('Ctrl Pts',(-1.86966242464576,-2.37548090580212,
9.10220924166623));
#63273=CARTESIAN_POINT('Ctrl Pts',(0.967866955901341,-2.86387511453221,
9.26020413266631));
#63274=CARTESIAN_POINT('Ctrl Pts',(2.92738853310682,-0.754283429618888,
9.41819902366633));
#63275=CARTESIAN_POINT('Ctrl Pts',(2.23130754034209,2.03956215310421,9.57619391466641));
#63276=CARTESIAN_POINT('Ctrl Pts',(-0.488920903815691,2.98320355754919,
9.73418880566644));
#63277=CARTESIAN_POINT('Ctrl Pts',(-2.76562106534208,1.22060937195346,9.89218369666651));
#63278=CARTESIAN_POINT('Ctrl Pts',(-2.53346723443519,-1.64926980449067,
10.0501785876666));
#63279=CARTESIAN_POINT('Ctrl Pts',(-0.00305950842402692,-3.02300144812525,
10.2081734786666));
#63280=CARTESIAN_POINT('Ctrl Pts',(2.53012367371502,-1.65439454534941,10.3661683696667));
#63281=CARTESIAN_POINT('Ctrl Pts',(2.76808609704807,1.21500883753128,10.5241632606667));
#63282=CARTESIAN_POINT('Ctrl Pts',(0.494958355870487,2.98220779656589,10.6821581516668));
#63283=CARTESIAN_POINT('Ctrl Pts',(-2.22717458809345,2.0440744776545,10.8401530426668));
#63284=CARTESIAN_POINT('Ctrl Pts',(-2.92890931940236,-0.748356408785326,
10.9981479336669));
#63285=CARTESIAN_POINT('Ctrl Pts',(-0.973661888071959,-2.86191013898051,
11.1561428246669));
#63286=CARTESIAN_POINT('Ctrl Pts',(1.86485026314516,-2.37926051801397,11.314137715667));
#63287=CARTESIAN_POINT('Ctrl Pts',(3.01164944347811,0.261753213276476,11.472132606667));
#63288=CARTESIAN_POINT('Ctrl Pts',(1.42640813452734,2.66531554408024,11.6301274976671));
#63289=CARTESIAN_POINT('Ctrl Pts',(-1.45281006480367,2.6510167927182,11.7881223886671));
#63290=CARTESIAN_POINT('Ctrl Pts',(-3.01410066275426,0.231828177198969,
11.9461172796672));
#63291=CARTESIAN_POINT('Ctrl Pts',(-1.84112713272175,-2.39766511385838,
12.1041121706673));
#63292=CARTESIAN_POINT('Ctrl Pts',(1.00203875880082,-2.85209843187493,12.2621070616673));
#63293=CARTESIAN_POINT('Ctrl Pts',(2.9361976242116,-0.71922915328282,12.4201019526674));
#63294=CARTESIAN_POINT('Ctrl Pts',(2.20676271346495,2.0660942542105,12.5780968436674));
#63295=CARTESIAN_POINT('Ctrl Pts',(-0.52455367595618,2.97714472223446,12.7360917346675));
#63296=CARTESIAN_POINT('Ctrl Pts',(-2.78001714567073,1.1874558528297,12.8940866256675));
#63297=CARTESIAN_POINT('Ctrl Pts',(-2.51356729987571,-1.67944241753446,
13.0520815166676));
#63298=CARTESIAN_POINT('Ctrl Pts',(0.0330844278327718,-3.02282208089334,
13.2100764076676));
#63299=CARTESIAN_POINT('Ctrl Pts',(2.5497226750577,-1.62402545531265,13.3680712986677));
#63300=CARTESIAN_POINT('Ctrl Pts',(2.75336210467249,1.24801722858484,13.5260661896677));
#63301=CARTESIAN_POINT('Ctrl Pts',(0.459265822762407,2.98791334565805,13.6840610806678));
#63302=CARTESIAN_POINT('Ctrl Pts',(-2.25145208218098,2.01729816656161,13.8420559716679));
#63303=CARTESIAN_POINT('Ctrl Pts',(-2.91975748968037,-0.78331815979697,
14.0000508626679));
#63304=CARTESIAN_POINT('Ctrl Pts',(-0.939365256882179,-2.87335314543991,
14.158045753668));
#63305=CARTESIAN_POINT('Ctrl Pts',(1.893145566493,-2.35678194735699,14.316040644668));
#63306=CARTESIAN_POINT('Ctrl Pts',(3.0083394738034,0.297719296989276,14.4740355356681));
#63307=CARTESIAN_POINT('Ctrl Pts',(1.3943726035929,2.68222336000765,14.6320304266681));
#63308=CARTESIAN_POINT('Ctrl Pts',(-1.4842749673478,2.63337329047569,14.7900253176682));
#63309=CARTESIAN_POINT('Ctrl Pts',(-3.01690018175728,0.195934968921086,
14.9480202086682));
#63310=CARTESIAN_POINT('Ctrl Pts',(-1.81186372087882,-2.41981344296957,
15.1060150996683));
#63311=CARTESIAN_POINT('Ctrl Pts',(1.03517641373175,-2.8393250802945,15.2640099906683));
#63312=CARTESIAN_POINT('Ctrl Pts',(2.94631239686769,-0.685220561427491,
15.4220048816684));
#63313=CARTESIAN_POINT('Ctrl Pts',(2.17839969522424,2.09473032457841,15.5799997726684));
#63314=CARTESIAN_POINT('Ctrl Pts',(0.358377621218746,2.67454389339306,15.6853297000018));
#63315=CARTESIAN_POINT('Ctrl Pts',(-0.474664453622694,2.51747565713054,
15.7379946636685));
#63316=CARTESIAN_POINT('Ctrl Pts',(-1.20564430054385,2.47375567929493,-0.109744663668462));
#63317=CARTESIAN_POINT('Ctrl Pts',(-2.02421927182262,2.0748034881184,-0.057079700001777));
#63318=CARTESIAN_POINT('Ctrl Pts',(-3.22065434935084,0.407847329213798,
0.0482502273315919));
#63319=CARTESIAN_POINT('Ctrl Pts',(-2.09935581806959,-2.48016800836378,
0.206245118331646));
#63320=CARTESIAN_POINT('Ctrl Pts',(0.929078334838823,-3.11059636412251,
0.364240009331699));
#63321=CARTESIAN_POINT('Ctrl Pts',(3.11331195928332,-0.923061779067598,
0.522234900331752));
#63322=CARTESIAN_POINT('Ctrl Pts',(2.4740004718514,2.10382325597413,0.680229791331807));
#63323=CARTESIAN_POINT('Ctrl Pts',(-0.409995321720456,3.2211710009984,0.83822468233186));
#63324=CARTESIAN_POINT('Ctrl Pts',(-2.92186394137152,1.41695230545948,0.996219573331913));
#63325=CARTESIAN_POINT('Ctrl Pts',(-2.78324468076858,-1.67294958451553,
1.15421446433197));
#63326=CARTESIAN_POINT('Ctrl Pts',(-0.119730115134298,-3.24507388821001,
1.31220935533202));
#63327=CARTESIAN_POINT('Ctrl Pts',(2.65237030684314,-1.87348281926831,1.47020424633207));
#63328=CARTESIAN_POINT('Ctrl Pts',(3.0183677856869,1.19769306098192,1.62819913733213));
#63329=CARTESIAN_POINT('Ctrl Pts',(0.646222449240343,3.18235132494235,1.78619402833218));
#63330=CARTESIAN_POINT('Ctrl Pts',(-2.31214440605599,2.28012676466554,1.94418891933223));
#63331=CARTESIAN_POINT('Ctrl Pts',(-3.17303415577589,-0.690537817402807,
2.10218381033229));
#63332=CARTESIAN_POINT('Ctrl Pts',(-1.15548094918627,-3.03477275592607,
2.26017870133234));
#63333=CARTESIAN_POINT('Ctrl Pts',(1.91027492854846,-2.62599231814139,2.4181735923324));
#63334=CARTESIAN_POINT('Ctrl Pts',(3.24311081177889,0.16497767954115,2.57616848333245));
#63335=CARTESIAN_POINT('Ctrl Pts',(1.63393412158284,2.80628649337991,2.7341633743325));
#63336=CARTESIAN_POINT('Ctrl Pts',(-1.45747813791209,2.90185159477728,2.89215826533256));
#63337=CARTESIAN_POINT('Ctrl Pts',(-3.22672816390422,0.364980032144142,
3.05015315633261));
#63338=CARTESIAN_POINT('Ctrl Pts',(-2.06882739509817,-2.50298585443527,
3.20814804733266));
#63339=CARTESIAN_POINT('Ctrl Pts',(0.965825724890286,-3.10034929240489,
3.36614293833272));
#63340=CARTESIAN_POINT('Ctrl Pts',(3.1243227658749,-0.885207486870811,3.52413782933277));
#63341=CARTESIAN_POINT('Ctrl Pts',(2.44856686017853,2.13295695269892,3.68213272033283));
#63342=CARTESIAN_POINT('Ctrl Pts',(-0.448424924558006,3.21619342238995,
3.84012761133287));
#63343=CARTESIAN_POINT('Ctrl Pts',(-2.9386246603379,1.3818357877601,3.99812250233293));
#63344=CARTESIAN_POINT('Ctrl Pts',(-2.76302888818086,-1.70606459460131,
4.15611739333298));
#63345=CARTESIAN_POINT('Ctrl Pts',(-0.0809306368842651,-3.24629562294995,
4.31411228433304));
#63346=CARTESIAN_POINT('Ctrl Pts',(2.67458445172116,-1.84162511099097,4.47210717533309));
#63347=CARTESIAN_POINT('Ctrl Pts',(3.00383009796752,1.23368949956199,4.63010206633314));
#63348=CARTESIAN_POINT('Ctrl Pts',(0.608128632616327,3.18985338302612,4.7880969573332));
#63349=CARTESIAN_POINT('Ctrl Pts',(-2.33924130497153,2.25231772980782,4.94609184833325));
#63350=CARTESIAN_POINT('Ctrl Pts',(-3.16455086313379,-0.728424926493586,
5.10408673933331));
#63351=CARTESIAN_POINT('Ctrl Pts',(-1.11911425628133,-3.04837142099104,
5.26208163033336));
#63352=CARTESIAN_POINT('Ctrl Pts',(1.94153528232519,-2.60296480698359,5.42007652133342));
#63353=CARTESIAN_POINT('Ctrl Pts',(3.24090645725565,0.20374094882929,5.57807141233347));
#63354=CARTESIAN_POINT('Ctrl Pts',(1.60026491450814,2.82562156742707,5.73606630333352));
#63355=CARTESIAN_POINT('Ctrl Pts',(-1.49206900577688,2.8842182859333,5.89406119433358));
#63356=CARTESIAN_POINT('Ctrl Pts',(-3.23086128254485,0.326374649544494,
6.05205608533362));
#63357=CARTESIAN_POINT('Ctrl Pts',(-2.03875339757824,-2.52754220989012,
6.21005097633369));
#63358=CARTESIAN_POINT('Ctrl Pts',(1.00282499699587,-3.08858010488847,6.36804586733373));
#63359=CARTESIAN_POINT('Ctrl Pts',(3.1346831377893,-0.847789280760374,6.52604075833379));
#63360=CARTESIAN_POINT('Ctrl Pts',(2.42288984570632,2.16207997874408,6.68403564933384));
#63361=CARTESIAN_POINT('Ctrl Pts',(-0.486846229934527,3.21060209108997,
6.8420305403339));
#63362=CARTESIAN_POINT('Ctrl Pts',(-2.95493607899053,1.34660231991219,7.00002543133394));
#63363=CARTESIAN_POINT('Ctrl Pts',(-2.74243339421689,-1.73897789439567,
7.15802032233401));
#63364=CARTESIAN_POINT('Ctrl Pts',(-0.042111587625147,-3.24703120605584,
7.31601521333405));
#63365=CARTESIAN_POINT('Ctrl Pts',(2.69641206305327,-1.80951568800428,7.47401010433411));
#63366=CARTESIAN_POINT('Ctrl Pts',(2.98886518931682,1.26951562377266,7.63200499533417));
#63367=CARTESIAN_POINT('Ctrl Pts',(0.56994673361268,3.19689626978371,7.78999988633422));
#63368=CARTESIAN_POINT('Ctrl Pts',(-2.36600319687202,2.2241883713625,7.94799477733426));
#63369=CARTESIAN_POINT('Ctrl Pts',(-3.15561549601314,-0.766208770658805,
8.10598966833433));
#63370=CARTESIAN_POINT('Ctrl Pts',(-1.0825874157591,-3.06153385187112,8.26398455933438));
#63371=CARTESIAN_POINT('Ctrl Pts',(1.97251799758337,-2.57956542621475,8.42197945033443));
#63372=CARTESIAN_POINT('Ctrl Pts',(3.23823884360454,0.242475216637791,8.57997434133449));
#63373=CARTESIAN_POINT('Ctrl Pts',(1.566366917775,2.84455263931128,8.73796923233454));
#63374=CARTESIAN_POINT('Ctrl Pts',(-1.52644656238412,2.86617269736115,8.89596412333459));
#63375=CARTESIAN_POINT('Ctrl Pts',(-3.23453253946489,0.287722592188601,
9.05395901433465));
#63376=CARTESIAN_POINT('Ctrl Pts',(-2.0083879464276,-2.55173723089919,9.21195390533469));
#63377=CARTESIAN_POINT('Ctrl Pts',(1.0396809083576,-3.07636939389751,9.36994879633477));
#63378=CARTESIAN_POINT('Ctrl Pts',(3.14459539160713,-0.810249876270418,
9.5279436873348));
#63379=CARTESIAN_POINT('Ctrl Pts',(2.39686646622593,2.19089392303558,9.68593857833487));
#63380=CARTESIAN_POINT('Ctrl Pts',(-0.525197937892946,3.20455178846357,
9.8439334693349));
#63381=CARTESIAN_POINT('Ctrl Pts',(-2.97082507451666,1.31117634799362,10.001928360335));
#63382=CARTESIAN_POINT('Ctrl Pts',(-2.72144585527141,-1.77164259819448,
10.159923251335));
#63383=CARTESIAN_POINT('Ctrl Pts',(-0.00328651833606387,-3.24730260950622,
10.3179181423351));
#63384=CARTESIAN_POINT('Ctrl Pts',(2.71785420847995,-1.77714758542301,10.4759130333351));
#63385=CARTESIAN_POINT('Ctrl Pts',(2.97347300705285,1.30516026419214,10.6339079243352));
#63386=CARTESIAN_POINT('Ctrl Pts',(0.531683357813799,3.20348214384215,10.7919028153352));
#63387=CARTESIAN_POINT('Ctrl Pts',(-2.39242685650282,2.19574105378912,10.9498977063353));
#63388=CARTESIAN_POINT('Ctrl Pts',(-3.14622901745573,-0.803883081364814,
11.1078925973353));
#63389=CARTESIAN_POINT('Ctrl Pts',(-1.0459058138638,-3.07425862076485,11.2658874883354));
#63390=CARTESIAN_POINT('Ctrl Pts',(2.00321873137213,-2.55579728340303,11.4238823793354));
#63391=CARTESIAN_POINT('Ctrl Pts',(3.23510830694092,0.281174821482934,11.5818772703355));
#63392=CARTESIAN_POINT('Ctrl Pts',(1.5322450011872,2.86307706760007,11.7398721613356));
#63393=CARTESIAN_POINT('Ctrl Pts',(-1.56060590625239,2.84771737511982,11.8978670523356));
#63394=CARTESIAN_POINT('Ctrl Pts',(-3.23774140219028,0.2490294026297,12.0558619433357));
#63395=CARTESIAN_POINT('Ctrl Pts',(-1.97773538819436,-2.57556746649356,
12.2138568343357));
#63396=CARTESIAN_POINT('Ctrl Pts',(1.07638819633982,-3.06371890299285,12.3718517253358));
#63397=CARTESIAN_POINT('Ctrl Pts',(3.15405810111051,-0.772594636941618,
12.5298466163358));
#63398=CARTESIAN_POINT('Ctrl Pts',(2.37050045822502,2.21939465736754,12.6878415073359));
#63399=CARTESIAN_POINT('Ctrl Pts',(-0.563474596353531,3.19804339868417,
12.8458363983359));
#63400=CARTESIAN_POINT('Ctrl Pts',(-2.98628931759431,1.2755628985751,13.003831289336));
#63401=CARTESIAN_POINT('Ctrl Pts',(-2.70006938207651,-1.80405396377073,
13.161826180336));
#63402=CARTESIAN_POINT('Ctrl Pts',(0.0355392316804697,-3.24710993355476,
13.3198210713361));
#63403=CARTESIAN_POINT('Ctrl Pts',(2.73890741976546,-1.74452516462138,13.4778159623361));
#63404=CARTESIAN_POINT('Ctrl Pts',(2.95765652145599,1.3406178173039,13.6358108533362));
#63405=CARTESIAN_POINT('Ctrl Pts',(0.493342504231463,3.20961103420941,13.7938057443362));
#63406=CARTESIAN_POINT('Ctrl Pts',(-2.41850569611158,2.16697798953759,13.9518006353363));
#63407=CARTESIAN_POINT('Ctrl Pts',(-3.13639813875855,-0.841438930159867,
14.1097955263364));
#63408=CARTESIAN_POINT('Ctrl Pts',(-1.00906443556115,-3.08655067730993,
14.2677904173364));
#63409=CARTESIAN_POINT('Ctrl Pts',(2.03361349431715,-2.53165084404301,14.4257853083365));
#63410=CARTESIAN_POINT('Ctrl Pts',(3.23155274358889,0.319809522622996,14.5837801993365));
#63411=CARTESIAN_POINT('Ctrl Pts',(1.49783249263057,2.88123941244982,14.7417750903366));
#63412=CARTESIAN_POINT('Ctrl Pts',(-1.59440544683904,2.8287647573801,14.8997699813366));
#63413=CARTESIAN_POINT('Ctrl Pts',(-3.24074864036727,0.210472984148126,
15.0577648723367));
#63414=CARTESIAN_POINT('Ctrl Pts',(-1.94630068488002,-2.59935916099094,
15.2157597633367));
#63415=CARTESIAN_POINT('Ctrl Pts',(1.1119846044715,-3.04999779215944,15.3737546543368));
#63416=CARTESIAN_POINT('Ctrl Pts',(3.16492337134089,-0.73606266996359,15.5317495453368));
#63417=CARTESIAN_POINT('Ctrl Pts',(2.34003295606631,2.25015547162033,15.6897444363369));
#63418=CARTESIAN_POINT('Ctrl Pts',(0.384968583225142,2.87299014350137,15.7950743636703));
#63419=CARTESIAN_POINT('Ctrl Pts',(-0.50988368525085,2.70426773226927,15.847739327337));
#63420=CARTESIAN_POINT('Ctrl Pts',(-1.28892185405322,2.64462557919718,-2.77555756156289E-16));
#63421=CARTESIAN_POINT('Ctrl Pts',(-2.16403831185614,2.21811653527943,0.0526649636666843));
#63422=CARTESIAN_POINT('Ctrl Pts',(-3.44311483358514,0.436018596449888,
0.157994891000053));
#63423=CARTESIAN_POINT('Ctrl Pts',(-2.24436477004298,-2.65148082752247,
0.315989782000107));
#63424=CARTESIAN_POINT('Ctrl Pts',(0.99325262796079,-3.32545480540779,0.47398467300016));
#63425=CARTESIAN_POINT('Ctrl Pts',(3.32835797506399,-0.986820490209951,
0.631979564000214));
#63426=CARTESIAN_POINT('Ctrl Pts',(2.64488728032712,2.24914078759987,0.789974455000268));
#63427=CARTESIAN_POINT('Ctrl Pts',(-0.438314957393884,3.44366717194826,
0.947969346000321));
#63428=CARTESIAN_POINT('Ctrl Pts',(-3.12368605475517,1.51482555164407,1.10596423700038));
#63429=CARTESIAN_POINT('Ctrl Pts',(-2.97549193622185,-1.78850534874892,
1.26395912800043));
#63430=CARTESIAN_POINT('Ctrl Pts',(-0.128000241792142,-3.46922110496824,
1.42195401900048));
#63431=CARTESIAN_POINT('Ctrl Pts',(2.83557766746782,-2.00289002972017,1.57994891000054));
#63432=CARTESIAN_POINT('Ctrl Pts',(3.22685571589167,1.28042139796218,1.73794380100059));
#63433=CARTESIAN_POINT('Ctrl Pts',(0.690859017896064,3.40216610167957,1.89593869200064));
#63434=CARTESIAN_POINT('Ctrl Pts',(-2.47185131912304,2.43762212093852,2.0539335830007));
#63435=CARTESIAN_POINT('Ctrl Pts',(-3.39220536703243,-0.738235384598252,
2.21192847400075));
#63436=CARTESIAN_POINT('Ctrl Pts',(-1.23529356600166,-3.24439382779317,
2.3699233650008));
#63437=CARTESIAN_POINT('Ctrl Pts',(2.0422234829505,-2.80737767009854,2.52791825600086));
#63438=CARTESIAN_POINT('Ctrl Pts',(3.46712243282082,0.176373194395425,2.68591314700091));
#63439=CARTESIAN_POINT('Ctrl Pts',(1.74679496800295,3.00012531757514,2.84390803800096));
#63440=CARTESIAN_POINT('Ctrl Pts',(-1.55815062776997,3.10229139393809,3.00190292900102));
#63441=CARTESIAN_POINT('Ctrl Pts',(-3.44960818515806,0.390190323556838,
3.15989782000107));
#63442=CARTESIAN_POINT('Ctrl Pts',(-2.21172765516599,-2.67587477227939,
3.31789271100113));
#63443=CARTESIAN_POINT('Ctrl Pts',(1.03253827306805,-3.31449993698521,3.47588760200118));
#63444=CARTESIAN_POINT('Ctrl Pts',(3.34012933187316,-0.946351485827688,
3.63388249300123));
#63445=CARTESIAN_POINT('Ctrl Pts',(2.61769689100758,2.28028683820616,3.79187738400129));
#63446=CARTESIAN_POINT('Ctrl Pts',(-0.479399010889233,3.43834577670275,
3.94987227500134));
#63447=CARTESIAN_POINT('Ctrl Pts',(-3.14160448804072,1.4772834282495,4.1078671660014));
#63448=CARTESIAN_POINT('Ctrl Pts',(-2.95387977677187,-1.82390771425382,
4.26586205700145));
#63449=CARTESIAN_POINT('Ctrl Pts',(-0.0865207644539496,-3.47052722867774,
4.4238569480015));
#63450=CARTESIAN_POINT('Ctrl Pts',(2.85932621153631,-1.96883181171989,4.58185183900155));
#63451=CARTESIAN_POINT('Ctrl Pts',(3.21131386544667,1.31890422107427,4.73984673000161));
#63452=CARTESIAN_POINT('Ctrl Pts',(0.65013394439898,3.41018634994864,4.89784162100166));
#63453=CARTESIAN_POINT('Ctrl Pts',(-2.50081988404187,2.40789223066154,5.05583651200171));
#63454=CARTESIAN_POINT('Ctrl Pts',(-3.38313610732142,-0.77873947263813,
5.21383140300178));
#63455=CARTESIAN_POINT('Ctrl Pts',(-1.19641491396169,-3.25893179440594,
5.37182629400181));
#63456=CARTESIAN_POINT('Ctrl Pts',(2.07564308534076,-2.78275957804407,5.52982118500188));
#63457=CARTESIAN_POINT('Ctrl Pts',(3.46476581676266,0.217813961707557,5.68781607600192));
#63458=CARTESIAN_POINT('Ctrl Pts',(1.71080012542156,3.02079592455092,5.84581096700199));
#63459=CARTESIAN_POINT('Ctrl Pts',(-1.59513079308199,3.08344009831299,6.00380585800203));
#63460=CARTESIAN_POINT('Ctrl Pts',(-3.45402679099304,0.348918348651528,
6.1618007490021));
#63461=CARTESIAN_POINT('Ctrl Pts',(-2.17957635430163,-2.7021273106005,6.31979564000214));
#63462=CARTESIAN_POINT('Ctrl Pts',(1.07209319849625,-3.30191781555228,6.4777905310022));
#63463=CARTESIAN_POINT('Ctrl Pts',(3.35120532648497,-0.906348689336672,
6.63578542200224));
#63464=CARTESIAN_POINT('Ctrl Pts',(2.59024628631004,2.31142148107623,6.79378031300231));
#63465=CARTESIAN_POINT('Ctrl Pts',(-0.520474193792445,3.4323682349829,6.95177520400236));
#63466=CARTESIAN_POINT('Ctrl Pts',(-3.15904258646038,1.43961627660056,7.10977009500241));
#63467=CARTESIAN_POINT('Ctrl Pts',(-2.93186168880579,-1.85909443671817,
7.26776498600247));
#63468=CARTESIAN_POINT('Ctrl Pts',(-0.0450203642769841,-3.47131362076721,
7.42575987700253));
#63469=CARTESIAN_POINT('Ctrl Pts',(2.8826615230001,-1.93450449230244,7.58375476800256));
#63470=CARTESIAN_POINT('Ctrl Pts',(3.19531528460895,1.35720496568057,7.74174965900264));
#63471=CARTESIAN_POINT('Ctrl Pts',(0.609314704401862,3.41771571051825,7.89974455000267));
#63472=CARTESIAN_POINT('Ctrl Pts',(-2.52943030198254,2.37781989106326,8.05773944100274));
#63473=CARTESIAN_POINT('Ctrl Pts',(-3.37358354695964,-0.819133162926983,
8.21573433200278));
#63474=CARTESIAN_POINT('Ctrl Pts',(-1.15736505241679,-3.27300339479932,
8.37372922300284));
#63475=CARTESIAN_POINT('Ctrl Pts',(2.10876587186757,-2.75774393020277,8.53172411400289));
#63476=CARTESIAN_POINT('Ctrl Pts',(3.46191394284634,0.259223724318805,8.68971900500295));
#63477=CARTESIAN_POINT('Ctrl Pts',(1.67456068997757,3.04103462369395,8.847713896003));
#63478=CARTESIAN_POINT('Ctrl Pts',(-1.63188291307296,3.06414804553306,9.00570878700305));
#63479=CARTESIAN_POINT('Ctrl Pts',(-3.45795163290035,0.307596475021262,
9.16370367800311));
#63480=CARTESIAN_POINT('Ctrl Pts',(-2.14711346820945,-2.72799355599627,
9.32169856900316));
#63481=CARTESIAN_POINT('Ctrl Pts',(1.11149486081386,-3.28886367326282,9.47969346000322));
#63482=CARTESIAN_POINT('Ctrl Pts',(3.36180225010744,-0.866216322921951,
9.63768835100326));
#63483=CARTESIAN_POINT('Ctrl Pts',(2.56242539210976,2.34222569296695,9.79568324200333));
#63484=CARTESIAN_POINT('Ctrl Pts',(-0.561474971970195,3.42590001937795,
9.95367813300337));
#63485=CARTESIAN_POINT('Ctrl Pts',(-3.17602908369125,1.40174332403378,10.1116730240034));
#63486=CARTESIAN_POINT('Ctrl Pts',(-2.90942447610763,-1.8940153918983,10.2696679150035));
#63487=CARTESIAN_POINT('Ctrl Pts',(-0.0035135282481055,-3.47160377088719,
10.4276628060035));
#63488=CARTESIAN_POINT('Ctrl Pts',(2.90558474324488,-1.89990062549661,10.5856576970036));
#63489=CARTESIAN_POINT('Ctrl Pts',(3.17885991705762,1.39531169085301,10.7436525880036));
#63490=CARTESIAN_POINT('Ctrl Pts',(0.568408359757113,3.4247564911184,10.9016474790037));
#63491=CARTESIAN_POINT('Ctrl Pts',(-2.55767912491219,2.34740762992373,11.0596423700038));
#63492=CARTESIAN_POINT('Ctrl Pts',(-3.36354871550911,-0.859409753944302,
11.2176372610038));
#63493=CARTESIAN_POINT('Ctrl Pts',(-1.11814973965565,-3.2866071025492,11.3756321520039));
#63494=CARTESIAN_POINT('Ctrl Pts',(2.14158719959911,-2.73233404879208,11.5336270430039));
#63495=CARTESIAN_POINT('Ctrl Pts',(3.45856717040372,0.300596429689395,11.691621934004));
#63496=CARTESIAN_POINT('Ctrl Pts',(1.63808186784707,3.0608385911199,11.849616825004));
#63497=CARTESIAN_POINT('Ctrl Pts',(-1.66840174770112,3.04441795752144,12.0076117160041));
#63498=CARTESIAN_POINT('Ctrl Pts',(-3.46138214162631,0.266230628060431,
12.1656066070041));
#63499=CARTESIAN_POINT('Ctrl Pts',(-2.11434364366697,-2.75346981912873,
12.3236014980042));
#63500=CARTESIAN_POINT('Ctrl Pts',(1.15073763387882,-3.27533937411076,12.4815963890042));
#63501=CARTESIAN_POINT('Ctrl Pts',(3.37191857800943,-0.825960120600417,
12.6395912800043));
#63502=CARTESIAN_POINT('Ctrl Pts',(2.53423820298509,2.37269506052457,12.7975861710043));
#63503=CARTESIAN_POINT('Ctrl Pts',(-0.602395516750883,3.41894207513388,
12.9555810620044));
#63504=CARTESIAN_POINT('Ctrl Pts',(-3.19256148951789,1.3636699443205,13.1135759530045));
#63505=CARTESIAN_POINT('Ctrl Pts',(-2.8865714642773,-1.928665510007,13.2715708440045));
#63506=CARTESIAN_POINT('Ctrl Pts',(0.0379940355281645,-3.4713977862162,
13.4295657350046));
#63507=CARTESIAN_POINT('Ctrl Pts',(2.92809216447323,-1.8650248739301,13.5875606260046));
#63508=CARTESIAN_POINT('Ctrl Pts',(3.16195093823948,1.43321840602296,13.7455555170047));
#63509=CARTESIAN_POINT('Ctrl Pts',(0.527419185700519,3.43130872276077,13.9035504080047));
#63510=CARTESIAN_POINT('Ctrl Pts',(-2.58555931004217,2.31665781251357,14.0615452990048));
#63511=CARTESIAN_POINT('Ctrl Pts',(-3.35303878783672,-0.89955970052277,
14.2195401900048));
#63512=CARTESIAN_POINT('Ctrl Pts',(-1.07876361424012,-3.29974820917995,
14.3775350810049));
#63513=CARTESIAN_POINT('Ctrl Pts',(2.1740814221413,-2.70651974072904,14.5355299720049));
#63514=CARTESIAN_POINT('Ctrl Pts',(3.45476601337439,0.341899748256715,14.693524863005));
#63515=CARTESIAN_POINT('Ctrl Pts',(1.60129238166824,3.08025546489199,14.851519754005));
#63516=CARTESIAN_POINT('Ctrl Pts',(-1.70453592633028,3.02415622428451,15.0095146450051));
#63517=CARTESIAN_POINT('Ctrl Pts',(-3.46459709897726,0.225010999375169,
15.1675095360052));
#63518=CARTESIAN_POINT('Ctrl Pts',(-2.08073764888123,-2.77890487901232,
15.3255044270052));
#63519=CARTESIAN_POINT('Ctrl Pts',(1.18879279521126,-3.26067050402438,15.4834993180053));
#63520=CARTESIAN_POINT('Ctrl Pts',(3.38353434581409,-0.786904778499691,
15.6414942090053));
#63521=CARTESIAN_POINT('Ctrl Pts',(2.50166621690838,2.40558061866225,15.7994891000054));
#63522=CARTESIAN_POINT('Ctrl Pts',(0.411559545231536,3.07143639360967,15.9048190273387));
#63523=CARTESIAN_POINT('Ctrl Pts',(-0.545102916879006,2.891059807408,15.9574839910054));
#63524=CARTESIAN_POINT('Ctrl Pts',(-2.94111188951679,-0.00259486169482749,
14.1778238829104));
#63525=CARTESIAN_POINT('Ctrl Pts',(-2.94335307565858,-0.259762554464039,
14.1917293186085));
#63526=CARTESIAN_POINT('Ctrl Pts',(-2.91238767988341,-0.516399492336486,
14.2056347543067));
#63527=CARTESIAN_POINT('Ctrl Pts',(-2.84607967927153,-0.763554866459577,
14.2195401900048));
#63528=CARTESIAN_POINT('Ctrl Pts',(-2.59494706330453,-1.69962253674182,
14.2722051536715));
#63529=CARTESIAN_POINT('Ctrl Pts',(-1.83685533877235,-2.49968537296086,
14.3248701173382));
#63530=CARTESIAN_POINT('Ctrl Pts',(-0.915668637109368,-2.80084537966192,
14.3775350810049));
#63531=CARTESIAN_POINT('Ctrl Pts',(0.00551806455364026,-3.10200538636298,
14.4302000446716));
#63532=CARTESIAN_POINT('Ctrl Pts',(1.0897997433475,-2.90426256354601,14.4828650083382));
#63533=CARTESIAN_POINT('Ctrl Pts',(1.84538801461659,-2.29732123730656,14.5355299720049));
#63534=CARTESIAN_POINT('Ctrl Pts',(2.60097628588567,-1.6903799110671,14.5881949356716));
#63535=CARTESIAN_POINT('Ctrl Pts',(3.02787114963004,-0.674240081405173,
14.6408598993383));
#63536=CARTESIAN_POINT('Ctrl Pts',(2.93240630955118,0.29022245286501,14.693524863005));
#63537=CARTESIAN_POINT('Ctrl Pts',(2.83694146947232,1.25468498713517,14.7461898266717));
#63538=CARTESIAN_POINT('Ctrl Pts',(2.21911692557029,2.16747022601356,14.7988547903384));
#63539=CARTESIAN_POINT('Ctrl Pts',(1.35923326895286,2.61451297201819,14.851519754005));
#63540=CARTESIAN_POINT('Ctrl Pts',(0.499349612335403,3.06155571802283,14.9041847176717));
#63541=CARTESIAN_POINT('Ctrl Pts',(-0.602593156997484,3.04285597115367,
14.9568496813384));
#63542=CARTESIAN_POINT('Ctrl Pts',(-1.4469080704384,2.56698189356751,15.0095146450051));
#63543=CARTESIAN_POINT('Ctrl Pts',(-1.70601080500511,2.42094600950443,15.0256764300034));
#63544=CARTESIAN_POINT('Ctrl Pts',(-1.94085146734146,2.2318557880317,15.0418382150017));
#63545=CARTESIAN_POINT('Ctrl Pts',(-2.14373220034761,2.01193738948431,15.058));
#63546=CARTESIAN_POINT('Ctrl Pts',(-1.37994859234592,-1.93347131995891,
-1.83880688453542E-16));
#63547=CARTESIAN_POINT('Ctrl Pts',(-1.43831895271373,-1.90176082500493,
-1.96503831907269E-16));
#63548=CARTESIAN_POINT('Ctrl Pts',(-1.49514575458196,-1.86752259046863,
-3.60259795903682E-17));
#63549=CARTESIAN_POINT('Ctrl Pts',(-1.55024291463987,-1.83079524515745,
-1.11022302462516E-16));
#63550=CARTESIAN_POINT('Ctrl Pts',(-1.61820139003649,-1.78549464545158,
-1.89647209120044E-16));
#63551=CARTESIAN_POINT('Ctrl Pts',(-1.68352982136479,-1.73640902813589,
4.37133882625492E-17));
#63552=CARTESIAN_POINT('Ctrl Pts',(-1.74614398662112,-1.68389593204229,
2.08166817117217E-17));
#63553=CARTESIAN_POINT('Ctrl Pts',(-1.78291149355231,-1.65305984859862,
7.3715640875763E-18));
#63554=CARTESIAN_POINT('Ctrl Pts',(-1.81874277362574,-1.62104095184393,
-1.13501056944751E-16));
#63555=CARTESIAN_POINT('Ctrl Pts',(-1.85361742493061,-1.58790418430478,
-1.38777878078145E-16));
#63556=CARTESIAN_POINT('Ctrl Pts',(-1.86599100473682,-1.57614720832583,
-1.47746133009421E-16));
#63557=CARTESIAN_POINT('Ctrl Pts',(-1.87824533378606,-1.56424827137885,
6.18933070998169E-17));
#63558=CARTESIAN_POINT('Ctrl Pts',(-1.89037564784625,-1.55221386701801,
6.93889390390723E-18));
#63559=CARTESIAN_POINT('Ctrl Pts',(-1.9520612058093,-1.49101603289205,-2.72517484859507E-16));
#63560=CARTESIAN_POINT('Ctrl Pts',(-2.01038866542646,-1.42647262579372,
-5.93465220813464E-16));
#63561=CARTESIAN_POINT('Ctrl Pts',(-2.06526482907838,-1.35900295762991,
-3.95516952522712E-16));
#63562=CARTESIAN_POINT('Ctrl Pts',(-2.11328147227381,-1.29996699798658,
-2.22312217768304E-16));
#63563=CARTESIAN_POINT('Ctrl Pts',(-2.15865566139155,-1.2386893890933,-3.33360010116584E-16));
#63564=CARTESIAN_POINT('Ctrl Pts',(-2.20130818996771,-1.17541961668097,
-3.46944695195361E-16));
#63565=CARTESIAN_POINT('Ctrl Pts',(-2.22006840714514,-1.1475911452903,-3.52919760469855E-16));
#63566=CARTESIAN_POINT('Ctrl Pts',(-2.23830186692143,-1.11937693173939,
-3.24730293914024E-16));
#63567=CARTESIAN_POINT('Ctrl Pts',(-2.25600064404541,-1.09079672684346,
-3.05311331771918E-16));
#63568=CARTESIAN_POINT('Ctrl Pts',(-2.26668277274188,-1.07354709288677,
-2.93590982320615E-16));
#63569=CARTESIAN_POINT('Ctrl Pts',(-2.27717011522814,-1.05616412126237,
7.72460434588031E-17));
#63570=CARTESIAN_POINT('Ctrl Pts',(-2.28746078556243,-1.03865201740679,
1.38777878078145E-16));
#63571=CARTESIAN_POINT('Ctrl Pts',(-2.2952947631346,-1.02532057986291,1.85620211640871E-16));
#63572=CARTESIAN_POINT('Ctrl Pts',(-2.30301001735291,-1.01192234024488,
-2.74638834286083E-16));
#63573=CARTESIAN_POINT('Ctrl Pts',(-2.31060459934883,-0.99846213025753,
-2.77555756156289E-16));
#63574=CARTESIAN_POINT('Ctrl Pts',(-2.35418081118604,-0.921230103254969,
-2.94292477860916E-16));
#63575=CARTESIAN_POINT('Ctrl Pts',(-2.39380271969424,-0.841933889485626,
-3.78845217127159E-17));
#63576=CARTESIAN_POINT('Ctrl Pts',(-2.42937389319446,-0.760969916140703,
-6.93889390390723E-17));
#63577=CARTESIAN_POINT('Ctrl Pts',(-2.46720610926394,-0.674859556767564,
-1.02895900045749E-16));
#63578=CARTESIAN_POINT('Ctrl Pts',(-2.5004573035107,-0.586862180324133,
-9.42383278312778E-17));
#63579=CARTESIAN_POINT('Ctrl Pts',(-2.52897137574918,-0.497406668002497,
0.));
#63580=CARTESIAN_POINT('Ctrl Pts',(-2.55035692992803,-0.430315033761271,
7.06787458734584E-17));
#63581=CARTESIAN_POINT('Ctrl Pts',(-2.56907707912655,-0.362402071614612,
2.24154037051898E-16));
#63582=CARTESIAN_POINT('Ctrl Pts',(-2.58504714386116,-0.293835873442853,
2.77555756156289E-16));
#63583=CARTESIAN_POINT('Ctrl Pts',(-2.59702469241211,-0.242411224814034,
3.17607045484582E-16));
#63584=CARTESIAN_POINT('Ctrl Pts',(-2.60745499960513,-0.1906188874626,1.72939271916983E-16));
#63585=CARTESIAN_POINT('Ctrl Pts',(-2.61629539664834,-0.138527206391925,
1.38777878078145E-16));
#63586=CARTESIAN_POINT('Ctrl Pts',(-2.61869711284596,-0.124375191094725,
1.29497076264031E-16));
#63587=CARTESIAN_POINT('Ctrl Pts',(-2.62098183196127,-0.110198515695441,
1.70346493820844E-17));
#63588=CARTESIAN_POINT('Ctrl Pts',(-2.62314735205575,-0.0960068887486099,
2.77555756156289E-17));
#63589=CARTESIAN_POINT('Ctrl Pts',(-2.63712677206149,-0.00439346333649258,
9.69640447732094E-17));
#63590=CARTESIAN_POINT('Ctrl Pts',(-2.64610759043344,0.0876011416361361,
-2.12521409618605E-16));
#63591=CARTESIAN_POINT('Ctrl Pts',(-2.64996359474771,0.179577964648124,
-5.55111512312578E-17));
#63592=CARTESIAN_POINT('Ctrl Pts',(-2.65210628483955,0.230687302523444,
3.17357233945851E-17));
#63593=CARTESIAN_POINT('Ctrl Pts',(-2.65266584064783,0.281791760322423,
2.25858622101648E-16));
#63594=CARTESIAN_POINT('Ctrl Pts',(-2.65161463128253,0.332826444242184,
1.94289029309402E-16));
#63595=CARTESIAN_POINT('Ctrl Pts',(-2.64978728963931,0.421541220055518,
1.40408657934648E-16));
#63596=CARTESIAN_POINT('Ctrl Pts',(-2.6430958113368,0.510044886368098,1.72520161624302E-16));
#63597=CARTESIAN_POINT('Ctrl Pts',(-2.63178393076928,0.598076371345786,
1.66533453693773E-16));
#63598=CARTESIAN_POINT('Ctrl Pts',(-2.62024798910265,0.687851547937211,
1.60428163503557E-16));
#63599=CARTESIAN_POINT('Ctrl Pts',(-2.60390669120625,0.777136386959749,
-1.34425914858345E-16));
#63600=CARTESIAN_POINT('Ctrl Pts',(-2.58296460883121,0.865656938831555,
-1.11022302462516E-16));
#63601=CARTESIAN_POINT('Ctrl Pts',(-2.57869408333521,0.883708117645516,
-1.06249819877211E-16));
#63602=CARTESIAN_POINT('Ctrl Pts',(-2.57423206760738,0.901727502426255,
-4.70036822748448E-17));
#63603=CARTESIAN_POINT('Ctrl Pts',(-2.56958003501042,0.919712740461561,
-5.55111512312578E-17));
#63604=CARTESIAN_POINT('Ctrl Pts',(-2.56604635272843,0.933374320783267,
-6.19734215806574E-17));
#63605=CARTESIAN_POINT('Ctrl Pts',(-2.56240532303519,0.947007284078113,
8.26362614469453E-17));
#63606=CARTESIAN_POINT('Ctrl Pts',(-2.5586586911495,0.960608258314244,8.32667268468867E-17));
#63607=CARTESIAN_POINT('Ctrl Pts',(-2.53407091484386,1.04986648337083,8.74042409382574E-17));
#63608=CARTESIAN_POINT('Ctrl Pts',(-2.504930952964,1.13777933274063,7.81122475311754E-16));
#63609=CARTESIAN_POINT('Ctrl Pts',(-2.47152838793823,1.2240648243653,6.38378239159465E-16));
#63610=CARTESIAN_POINT('Ctrl Pts',(-2.43748524526305,1.31200505589874,4.92896525595146E-16));
#63611=CARTESIAN_POINT('Ctrl Pts',(-2.39901427145562,1.39825569878996,-4.49689980744232E-17));
#63612=CARTESIAN_POINT('Ctrl Pts',(-2.35636659634517,1.48252101187545,-5.55111512312578E-17));
#63613=CARTESIAN_POINT('Ctrl Pts',(-2.31336109209446,1.56749334086406,-6.61417567970626E-17));
#63614=CARTESIAN_POINT('Ctrl Pts',(-2.26610821171127,1.65044775809861,-5.44480906746773E-17));
#63615=CARTESIAN_POINT('Ctrl Pts',(-2.21481327415801,1.731071203515,-5.55111512312578E-17));
#63616=CARTESIAN_POINT('Ctrl Pts',(-2.18401751630642,1.77947481253834,-5.61493770883036E-17));
#63617=CARTESIAN_POINT('Ctrl Pts',(-2.15176385823466,1.82703799978858,3.67516605336294E-16));
#63618=CARTESIAN_POINT('Ctrl Pts',(-2.11808850376184,1.87368930169054,3.88578058618805E-16));
#63619=CARTESIAN_POINT('Ctrl Pts',(-2.1089145366433,1.88639822536441,3.94315699184355E-16));
#63620=CARTESIAN_POINT('Ctrl Pts',(-2.09963412322397,1.89904053530927,1.84615714870052E-16));
#63621=CARTESIAN_POINT('Ctrl Pts',(-2.09025911328956,1.91160012317952,1.66533453693773E-16));
#63622=CARTESIAN_POINT('Ctrl Pts',(-2.03145402967869,1.99038058527982,5.31118266465956E-17));
#63623=CARTESIAN_POINT('Ctrl Pts',(-1.96883756375661,2.06603912302101,4.62847422951145E-16));
#63624=CARTESIAN_POINT('Ctrl Pts',(-1.90268196527442,2.13826743811961,3.33066907387547E-16));
#63625=CARTESIAN_POINT('Ctrl Pts',(-1.83635976195865,2.21067765145044,2.0295955537029E-16));
#63626=CARTESIAN_POINT('Ctrl Pts',(-1.76648017672323,2.2796412428746,3.28001727774597E-18));
#63627=CARTESIAN_POINT('Ctrl Pts',(-1.6932675195623,2.34483179093341,0.));
#63628=CARTESIAN_POINT('Ctrl Pts',(-1.62146081066126,2.40877044429043,-3.21702906282713E-18));
#63629=CARTESIAN_POINT('Ctrl Pts',(-1.54644728359632,2.46908034426641,-8.3280583097932E-18));
#63630=CARTESIAN_POINT('Ctrl Pts',(-1.46839770082455,2.52542611967769,-5.55111512312578E-17));
#63631=CARTESIAN_POINT('Ctrl Pts',(-1.41023968234018,2.56741172077267,-9.06692532072844E-17));
#63632=CARTESIAN_POINT('Ctrl Pts',(-1.35039506896231,2.60719581243537,-1.11866688105539E-17));
#63633=CARTESIAN_POINT('Ctrl Pts',(-1.28892185405323,2.64462557919718,0.));
#63634=CARTESIAN_POINT('Origin',(0.,0.,0.));
#63635=CARTESIAN_POINT('Origin',(-1.44337567297407,-2.5,-6.));
#63636=CARTESIAN_POINT('',(-1.44337567297407,-2.5,-6.));
#63637=CARTESIAN_POINT('',(1.44337567297406,-2.5,-6.));
#63638=CARTESIAN_POINT('',(-0.721687836487033,-2.5,-6.));
#63639=CARTESIAN_POINT('',(-1.44337567297407,-2.5,-3.));
#63640=CARTESIAN_POINT('',(-1.44337567297407,-2.5,-6.));
#63641=CARTESIAN_POINT('',(1.44337567297406,-2.5,-3.));
#63642=CARTESIAN_POINT('',(-1.44337567297407,-2.5,-3.));
#63643=CARTESIAN_POINT('',(1.44337567297406,-2.5,-6.));
#63644=CARTESIAN_POINT('Origin',(-2.88675134594813,3.53525079574969E-16,
-6.));
#63645=CARTESIAN_POINT('',(-2.88675134594813,3.53525079574969E-16,-6.));
#63646=CARTESIAN_POINT('',(-2.52590742770461,-0.625,-6.));
#63647=CARTESIAN_POINT('',(-2.88675134594813,5.55111512312578E-16,-3.));
#63648=CARTESIAN_POINT('',(-2.88675134594813,3.53525079574969E-16,-6.));
#63649=CARTESIAN_POINT('',(-2.88675134594813,3.53525079574969E-16,-3.));
#63650=CARTESIAN_POINT('Origin',(-1.44337567297406,2.5,-6.));
#63651=CARTESIAN_POINT('',(-1.44337567297406,2.5,-6.));
#63652=CARTESIAN_POINT('',(-1.80421959121758,1.875,-6.));
#63653=CARTESIAN_POINT('',(-1.44337567297406,2.5,-3.));
#63654=CARTESIAN_POINT('',(-1.44337567297406,2.5,-6.));
#63655=CARTESIAN_POINT('',(-1.44337567297406,2.5,-3.));
#63656=CARTESIAN_POINT('Origin',(1.44337567297406,2.5,-6.));
#63657=CARTESIAN_POINT('',(1.44337567297406,2.5,-6.));
#63658=CARTESIAN_POINT('',(0.721687836487033,2.5,-6.));
#63659=CARTESIAN_POINT('',(1.44337567297406,2.5,-3.));
#63660=CARTESIAN_POINT('',(1.44337567297406,2.5,-6.));
#63661=CARTESIAN_POINT('',(1.44337567297406,2.5,-3.));
#63662=CARTESIAN_POINT('Origin',(2.88675134594813,0.,-6.));
#63663=CARTESIAN_POINT('',(2.88675134594813,0.,-6.));
#63664=CARTESIAN_POINT('',(2.52590742770461,0.625,-6.));
#63665=CARTESIAN_POINT('',(2.88675134594813,0.,-3.));
#63666=CARTESIAN_POINT('',(2.88675134594813,0.,-6.));
#63667=CARTESIAN_POINT('',(2.88675134594813,0.,-3.));
#63668=CARTESIAN_POINT('Origin',(1.44337567297406,-2.5,-6.));
#63669=CARTESIAN_POINT('',(1.80421959121758,-1.875,-6.));
#63670=CARTESIAN_POINT('',(1.44337567297406,-2.5,-3.));
#63671=CARTESIAN_POINT('Origin',(0.,0.,-3.));
#63672=CARTESIAN_POINT('Origin',(0.,0.,0.));
#63673=CARTESIAN_POINT('',(-5.,-6.12323399573677E-16,0.));
#63674=CARTESIAN_POINT('Origin',(0.,0.,0.));
#63675=CARTESIAN_POINT('Origin',(0.,0.,-6.));
#63676=CARTESIAN_POINT('',(-5.,-6.12323399573677E-16,-6.));
#63677=CARTESIAN_POINT('',(-5.,-6.12323399573677E-16,-6.));
#63678=CARTESIAN_POINT('Origin',(0.,0.,-6.));
#63679=CARTESIAN_POINT('Origin',(0.,0.,-6.));
#63680=CARTESIAN_POINT('Origin',(0.,0.,16.));
#63681=CARTESIAN_POINT('',(0.,0.,0.));
#63682=CARTESIAN_POINT('Origin',(0.,0.,0.));
#63683=CARTESIAN_POINT('',(-3.5,-4.28626379701574E-16,2.));
#63684=CARTESIAN_POINT('Origin',(0.,0.,2.));
#63685=CARTESIAN_POINT('',(-3.5,-4.28626379701574E-16,0.));
#63686=CARTESIAN_POINT('',(-3.5,-4.28626379701574E-16,0.));
#63687=CARTESIAN_POINT('Origin',(0.,0.,0.));
#63688=CARTESIAN_POINT('Origin',(0.,0.,0.));
#63689=CARTESIAN_POINT('',(-7.,-8.57252759403147E-16,2.));
#63690=CARTESIAN_POINT('Origin',(0.,0.,2.));
#63691=CARTESIAN_POINT('',(-7.,-8.57252759403147E-16,0.));
#63692=CARTESIAN_POINT('',(-7.,-8.57252759403147E-16,0.));
#63693=CARTESIAN_POINT('Origin',(0.,0.,0.));
#63694=CARTESIAN_POINT('Origin',(0.,0.,2.));
#63695=CARTESIAN_POINT('Origin',(0.,0.,0.));
#63696=CARTESIAN_POINT('',(0.,0.,50.));
#63697=CARTESIAN_POINT('',(0.,0.,450.));
#63698=CARTESIAN_POINT('',(0.,0.,456.));
#63699=CARTESIAN_POINT('',(0.,0.,-4.));
#63700=CARTESIAN_POINT('',(0.,0.,0.));
#63701=CARTESIAN_POINT('',(0.,0.,0.));
#63702=CARTESIAN_POINT('',(0.,0.,0.));
#63703=CARTESIAN_POINT('',(0.,0.,40.));
#63704=CARTESIAN_POINT('',(0.,0.,48.));
#63705=CARTESIAN_POINT('',(15.,0.,20.));
#63706=CARTESIAN_POINT('',(15.,0.,18.));
#63707=CARTESIAN_POINT('',(-7.5,12.9903810567666,20.));
#63708=CARTESIAN_POINT('',(-7.5,12.9903810567666,18.));
#63709=CARTESIAN_POINT('',(-7.50000000000001,-12.9903810567666,20.));
#63710=CARTESIAN_POINT('',(-7.50000000000001,-12.9903810567666,18.));
#63711=CARTESIAN_POINT('',(-250.,-200.,0.));
#63712=CARTESIAN_POINT('',(0.,0.,0.));
#63713=CARTESIAN_POINT('',(250.,-200.,0.));
#63714=CARTESIAN_POINT('',(-250.,200.,0.));
#63715=CARTESIAN_POINT('',(250.,200.,0.));
#63716=UNCERTAINTY_MEASURE_WITH_UNIT(LENGTH_MEASURE(0.01),#63756,
'DISTANCE_ACCURACY_VALUE',
'Maximum model space distance between geometric entities at asserted c
onnectivities');
#63717=UNCERTAINTY_MEASURE_WITH_UNIT(LENGTH_MEASURE(0.01),#63756,
'DISTANCE_ACCURACY_VALUE',
'Maximum model space distance between geometric entities at asserted c
onnectivities');
#63718=UNCERTAINTY_MEASURE_WITH_UNIT(LENGTH_MEASURE(0.01),#63756,
'DISTANCE_ACCURACY_VALUE',
'Maximum model space distance between geometric entities at asserted c
onnectivities');
#63719=UNCERTAINTY_MEASURE_WITH_UNIT(LENGTH_MEASURE(0.01),#63756,
'DISTANCE_ACCURACY_VALUE',
'Maximum model space distance between geometric entities at asserted c
onnectivities');
#63720=UNCERTAINTY_MEASURE_WITH_UNIT(LENGTH_MEASURE(0.01),#63756,
'DISTANCE_ACCURACY_VALUE',
'Maximum model space distance between geometric entities at asserted c
onnectivities');
#63721=UNCERTAINTY_MEASURE_WITH_UNIT(LENGTH_MEASURE(0.01),#63756,
'DISTANCE_ACCURACY_VALUE',
'Maximum model space distance between geometric entities at asserted c
onnectivities');
#63722=UNCERTAINTY_MEASURE_WITH_UNIT(LENGTH_MEASURE(0.01),#63756,
'DISTANCE_ACCURACY_VALUE',
'Maximum model space distance between geometric entities at asserted c
onnectivities');
#63723=UNCERTAINTY_MEASURE_WITH_UNIT(LENGTH_MEASURE(0.01),#63756,
'DISTANCE_ACCURACY_VALUE',
'Maximum model space distance between geometric entities at asserted c
onnectivities');
#63724=UNCERTAINTY_MEASURE_WITH_UNIT(LENGTH_MEASURE(0.01),#63756,
'DISTANCE_ACCURACY_VALUE',
'Maximum model space distance between geometric entities at asserted c
onnectivities');
#63725=UNCERTAINTY_MEASURE_WITH_UNIT(LENGTH_MEASURE(0.01),#63756,
'DISTANCE_ACCURACY_VALUE',
'Maximum model space distance between geometric entities at asserted c
onnectivities');
#63726=UNCERTAINTY_MEASURE_WITH_UNIT(LENGTH_MEASURE(0.01),#63756,
'DISTANCE_ACCURACY_VALUE',
'Maximum model space distance between geometric entities at asserted c
onnectivities');
#63727=UNCERTAINTY_MEASURE_WITH_UNIT(LENGTH_MEASURE(0.01),#63756,
'DISTANCE_ACCURACY_VALUE',
'Maximum model space distance between geometric entities at asserted c
onnectivities');
#63728=UNCERTAINTY_MEASURE_WITH_UNIT(LENGTH_MEASURE(0.01),#63756,
'DISTANCE_ACCURACY_VALUE',
'Maximum model space distance between geometric entities at asserted c
onnectivities');
#63729=UNCERTAINTY_MEASURE_WITH_UNIT(LENGTH_MEASURE(0.01),#63756,
'DISTANCE_ACCURACY_VALUE',
'Maximum model space distance between geometric entities at asserted c
onnectivities');
#63730=UNCERTAINTY_MEASURE_WITH_UNIT(LENGTH_MEASURE(0.01),#63756,
'DISTANCE_ACCURACY_VALUE',
'Maximum model space distance between geometric entities at asserted c
onnectivities');
#63731=UNCERTAINTY_MEASURE_WITH_UNIT(LENGTH_MEASURE(0.01),#63756,
'DISTANCE_ACCURACY_VALUE',
'Maximum model space distance between geometric entities at asserted c
onnectivities');
#63732=UNCERTAINTY_MEASURE_WITH_UNIT(LENGTH_MEASURE(0.01),#63756,
'DISTANCE_ACCURACY_VALUE',
'Maximum model space distance between geometric entities at asserted c
onnectivities');
#63733=UNCERTAINTY_MEASURE_WITH_UNIT(LENGTH_MEASURE(0.01),#63756,
'DISTANCE_ACCURACY_VALUE',
'Maximum model space distance between geometric entities at asserted c
onnectivities');
#63734=UNCERTAINTY_MEASURE_WITH_UNIT(LENGTH_MEASURE(0.01),#63756,
'DISTANCE_ACCURACY_VALUE',
'Maximum model space distance between geometric entities at asserted c
onnectivities');
#63735=UNCERTAINTY_MEASURE_WITH_UNIT(LENGTH_MEASURE(0.01),#63756,
'DISTANCE_ACCURACY_VALUE',
'Maximum model space distance between geometric entities at asserted c
onnectivities');
#63736=(
GEOMETRIC_REPRESENTATION_CONTEXT(3)
GLOBAL_UNCERTAINTY_ASSIGNED_CONTEXT((#63716))
GLOBAL_UNIT_ASSIGNED_CONTEXT((#63756,#63758,#63759))
REPRESENTATION_CONTEXT('','3D')
);
#63737=(
GEOMETRIC_REPRESENTATION_CONTEXT(3)
GLOBAL_UNCERTAINTY_ASSIGNED_CONTEXT((#63717))
GLOBAL_UNIT_ASSIGNED_CONTEXT((#63756,#63758,#63759))
REPRESENTATION_CONTEXT('','3D')
);
#63738=(
GEOMETRIC_REPRESENTATION_CONTEXT(3)
GLOBAL_UNCERTAINTY_ASSIGNED_CONTEXT((#63718))
GLOBAL_UNIT_ASSIGNED_CONTEXT((#63756,#63758,#63759))
REPRESENTATION_CONTEXT('','3D')
);
#63739=(
GEOMETRIC_REPRESENTATION_CONTEXT(3)
GLOBAL_UNCERTAINTY_ASSIGNED_CONTEXT((#63719))
GLOBAL_UNIT_ASSIGNED_CONTEXT((#63756,#63758,#63759))
REPRESENTATION_CONTEXT('','3D')
);
#63740=(
GEOMETRIC_REPRESENTATION_CONTEXT(3)
GLOBAL_UNCERTAINTY_ASSIGNED_CONTEXT((#63720))
GLOBAL_UNIT_ASSIGNED_CONTEXT((#63756,#63758,#63759))
REPRESENTATION_CONTEXT('','3D')
);
#63741=(
GEOMETRIC_REPRESENTATION_CONTEXT(3)
GLOBAL_UNCERTAINTY_ASSIGNED_CONTEXT((#63721))
GLOBAL_UNIT_ASSIGNED_CONTEXT((#63756,#63758,#63759))
REPRESENTATION_CONTEXT('','3D')
);
#63742=(
GEOMETRIC_REPRESENTATION_CONTEXT(3)
GLOBAL_UNCERTAINTY_ASSIGNED_CONTEXT((#63722))
GLOBAL_UNIT_ASSIGNED_CONTEXT((#63756,#63758,#63759))
REPRESENTATION_CONTEXT('','3D')
);
#63743=(
GEOMETRIC_REPRESENTATION_CONTEXT(3)
GLOBAL_UNCERTAINTY_ASSIGNED_CONTEXT((#63723))
GLOBAL_UNIT_ASSIGNED_CONTEXT((#63756,#63758,#63759))
REPRESENTATION_CONTEXT('','3D')
);
#63744=(
GEOMETRIC_REPRESENTATION_CONTEXT(3)
GLOBAL_UNCERTAINTY_ASSIGNED_CONTEXT((#63724))
GLOBAL_UNIT_ASSIGNED_CONTEXT((#63756,#63758,#63759))
REPRESENTATION_CONTEXT('','3D')
);
#63745=(
GEOMETRIC_REPRESENTATION_CONTEXT(3)
GLOBAL_UNCERTAINTY_ASSIGNED_CONTEXT((#63725))
GLOBAL_UNIT_ASSIGNED_CONTEXT((#63756,#63758,#63759))
REPRESENTATION_CONTEXT('','3D')
);
#63746=(
GEOMETRIC_REPRESENTATION_CONTEXT(3)
GLOBAL_UNCERTAINTY_ASSIGNED_CONTEXT((#63726))
GLOBAL_UNIT_ASSIGNED_CONTEXT((#63756,#63758,#63759))
REPRESENTATION_CONTEXT('','3D')
);
#63747=(
GEOMETRIC_REPRESENTATION_CONTEXT(3)
GLOBAL_UNCERTAINTY_ASSIGNED_CONTEXT((#63727))
GLOBAL_UNIT_ASSIGNED_CONTEXT((#63756,#63758,#63759))
REPRESENTATION_CONTEXT('','3D')
);
#63748=(
GEOMETRIC_REPRESENTATION_CONTEXT(3)
GLOBAL_UNCERTAINTY_ASSIGNED_CONTEXT((#63728))
GLOBAL_UNIT_ASSIGNED_CONTEXT((#63756,#63758,#63759))
REPRESENTATION_CONTEXT('','3D')
);
#63749=(
GEOMETRIC_REPRESENTATION_CONTEXT(3)
GLOBAL_UNCERTAINTY_ASSIGNED_CONTEXT((#63729))
GLOBAL_UNIT_ASSIGNED_CONTEXT((#63756,#63758,#63759))
REPRESENTATION_CONTEXT('','3D')
);
#63750=(
GEOMETRIC_REPRESENTATION_CONTEXT(3)
GLOBAL_UNCERTAINTY_ASSIGNED_CONTEXT((#63730))
GLOBAL_UNIT_ASSIGNED_CONTEXT((#63756,#63758,#63759))
REPRESENTATION_CONTEXT('','3D')
);
#63751=(
GEOMETRIC_REPRESENTATION_CONTEXT(3)
GLOBAL_UNCERTAINTY_ASSIGNED_CONTEXT((#63731))
GLOBAL_UNIT_ASSIGNED_CONTEXT((#63756,#63758,#63759))
REPRESENTATION_CONTEXT('','3D')
);
#63752=(
GEOMETRIC_REPRESENTATION_CONTEXT(3)
GLOBAL_UNCERTAINTY_ASSIGNED_CONTEXT((#63732))
GLOBAL_UNIT_ASSIGNED_CONTEXT((#63756,#63758,#63759))
REPRESENTATION_CONTEXT('','3D')
);
#63753=(
GEOMETRIC_REPRESENTATION_CONTEXT(3)
GLOBAL_UNCERTAINTY_ASSIGNED_CONTEXT((#63733))
GLOBAL_UNIT_ASSIGNED_CONTEXT((#63756,#63758,#63759))
REPRESENTATION_CONTEXT('','3D')
);
#63754=(
GEOMETRIC_REPRESENTATION_CONTEXT(3)
GLOBAL_UNCERTAINTY_ASSIGNED_CONTEXT((#63734))
GLOBAL_UNIT_ASSIGNED_CONTEXT((#63756,#63758,#63759))
REPRESENTATION_CONTEXT('','3D')
);
#63755=(
GEOMETRIC_REPRESENTATION_CONTEXT(3)
GLOBAL_UNCERTAINTY_ASSIGNED_CONTEXT((#63735))
GLOBAL_UNIT_ASSIGNED_CONTEXT((#63756,#63758,#63759))
REPRESENTATION_CONTEXT('','3D')
);
#63756=(
LENGTH_UNIT()
NAMED_UNIT(*)
SI_UNIT(.MILLI.,.METRE.)
);
#63757=(
LENGTH_UNIT()
NAMED_UNIT(*)
SI_UNIT($,.METRE.)
);
#63758=(
NAMED_UNIT(*)
PLANE_ANGLE_UNIT()
SI_UNIT($,.RADIAN.)
);
#63759=(
NAMED_UNIT(*)
SI_UNIT($,.STERADIAN.)
SOLID_ANGLE_UNIT()
);
#63760=SHAPE_DEFINITION_REPRESENTATION(#63779,#63858);
#63761=SHAPE_DEFINITION_REPRESENTATION(#63780,#63859);
#63762=SHAPE_DEFINITION_REPRESENTATION(#63781,#63860);
#63763=SHAPE_DEFINITION_REPRESENTATION(#63782,#63861);
#63764=SHAPE_DEFINITION_REPRESENTATION(#63783,#63862);
#63765=SHAPE_DEFINITION_REPRESENTATION(#63784,#63863);
#63766=SHAPE_DEFINITION_REPRESENTATION(#63785,#63864);
#63767=SHAPE_DEFINITION_REPRESENTATION(#63826,#63865);
#63768=SHAPE_DEFINITION_REPRESENTATION(#63827,#63866);
#63769=SHAPE_DEFINITION_REPRESENTATION(#63828,#63867);
#63770=SHAPE_DEFINITION_REPRESENTATION(#63829,#63868);
#63771=SHAPE_DEFINITION_REPRESENTATION(#63830,#63869);
#63772=SHAPE_DEFINITION_REPRESENTATION(#63831,#63870);
#63773=SHAPE_DEFINITION_REPRESENTATION(#63832,#63871);
#63774=SHAPE_DEFINITION_REPRESENTATION(#63833,#63872);
#63775=SHAPE_DEFINITION_REPRESENTATION(#63834,#63873);
#63776=SHAPE_DEFINITION_REPRESENTATION(#63835,#63874);
#63777=SHAPE_DEFINITION_REPRESENTATION(#63836,#63875);
#63778=SHAPE_DEFINITION_REPRESENTATION(#63837,#63876);
#63779=PRODUCT_DEFINITION_SHAPE('',$,#63878);
#63780=PRODUCT_DEFINITION_SHAPE('',$,#63879);
#63781=PRODUCT_DEFINITION_SHAPE('',$,#63880);
#63782=PRODUCT_DEFINITION_SHAPE('',$,#63881);
#63783=PRODUCT_DEFINITION_SHAPE('',$,#63882);
#63784=PRODUCT_DEFINITION_SHAPE('',$,#63883);
#63785=PRODUCT_DEFINITION_SHAPE('',$,#63884);
#63786=PRODUCT_DEFINITION_SHAPE($,$,#194);
#63787=PRODUCT_DEFINITION_SHAPE($,$,#195);
#63788=PRODUCT_DEFINITION_SHAPE($,$,#196);
#63789=PRODUCT_DEFINITION_SHAPE($,$,#197);
#63790=PRODUCT_DEFINITION_SHAPE($,$,#198);
#63791=PRODUCT_DEFINITION_SHAPE($,$,#199);
#63792=PRODUCT_DEFINITION_SHAPE($,$,#200);
#63793=PRODUCT_DEFINITION_SHAPE($,$,#201);
#63794=PRODUCT_DEFINITION_SHAPE($,$,#202);
#63795=PRODUCT_DEFINITION_SHAPE($,$,#203);
#63796=PRODUCT_DEFINITION_SHAPE($,$,#204);
#63797=PRODUCT_DEFINITION_SHAPE($,$,#205);
#63798=PRODUCT_DEFINITION_SHAPE($,$,#206);
#63799=PRODUCT_DEFINITION_SHAPE($,$,#207);
#63800=PRODUCT_DEFINITION_SHAPE($,$,#208);
#63801=PRODUCT_DEFINITION_SHAPE($,$,#209);
#63802=PRODUCT_DEFINITION_SHAPE($,$,#210);
#63803=PRODUCT_DEFINITION_SHAPE($,$,#211);
#63804=PRODUCT_DEFINITION_SHAPE($,$,#212);
#63805=PRODUCT_DEFINITION_SHAPE($,$,#213);
#63806=PRODUCT_DEFINITION_SHAPE($,$,#214);
#63807=PRODUCT_DEFINITION_SHAPE($,$,#215);
#63808=PRODUCT_DEFINITION_SHAPE($,$,#216);
#63809=PRODUCT_DEFINITION_SHAPE($,$,#217);
#63810=PRODUCT_DEFINITION_SHAPE($,$,#218);
#63811=PRODUCT_DEFINITION_SHAPE($,$,#219);
#63812=PRODUCT_DEFINITION_SHAPE($,$,#220);
#63813=PRODUCT_DEFINITION_SHAPE($,$,#221);
#63814=PRODUCT_DEFINITION_SHAPE($,$,#222);
#63815=PRODUCT_DEFINITION_SHAPE($,$,#223);
#63816=PRODUCT_DEFINITION_SHAPE($,$,#224);
#63817=PRODUCT_DEFINITION_SHAPE($,$,#225);
#63818=PRODUCT_DEFINITION_SHAPE($,$,#226);
#63819=PRODUCT_DEFINITION_SHAPE($,$,#227);
#63820=PRODUCT_DEFINITION_SHAPE($,$,#228);
#63821=PRODUCT_DEFINITION_SHAPE($,$,#229);
#63822=PRODUCT_DEFINITION_SHAPE($,$,#230);
#63823=PRODUCT_DEFINITION_SHAPE($,$,#231);
#63824=PRODUCT_DEFINITION_SHAPE($,$,#232);
#63825=PRODUCT_DEFINITION_SHAPE($,$,#233);
#63826=PRODUCT_DEFINITION_SHAPE('',$,#63885);
#63827=PRODUCT_DEFINITION_SHAPE('',$,#63886);
#63828=PRODUCT_DEFINITION_SHAPE('',$,#63887);
#63829=PRODUCT_DEFINITION_SHAPE('',$,#63888);
#63830=PRODUCT_DEFINITION_SHAPE('',$,#63889);
#63831=PRODUCT_DEFINITION_SHAPE('',$,#63890);
#63832=PRODUCT_DEFINITION_SHAPE('',$,#63891);
#63833=PRODUCT_DEFINITION_SHAPE('',$,#63892);
#63834=PRODUCT_DEFINITION_SHAPE('',$,#63893);
#63835=PRODUCT_DEFINITION_SHAPE('',$,#63894);
#63836=PRODUCT_DEFINITION_SHAPE('',$,#63895);
#63837=PRODUCT_DEFINITION_SHAPE('',$,#63896);
#63838=PRODUCT_DEFINITION_SHAPE($,$,#234);
#63839=PRODUCT_DEFINITION_SHAPE($,$,#235);
#63840=PRODUCT_DEFINITION_SHAPE($,$,#236);
#63841=PRODUCT_DEFINITION_SHAPE($,$,#237);
#63842=PRODUCT_DEFINITION_SHAPE($,$,#238);
#63843=PRODUCT_DEFINITION_SHAPE($,$,#239);
#63844=PRODUCT_DEFINITION_SHAPE($,$,#240);
#63845=PRODUCT_DEFINITION_SHAPE($,$,#241);
#63846=PRODUCT_DEFINITION_SHAPE($,$,#242);
#63847=PRODUCT_DEFINITION_SHAPE($,$,#243);
#63848=PRODUCT_DEFINITION_SHAPE($,$,#244);
#63849=PRODUCT_DEFINITION_SHAPE($,$,#245);
#63850=PRODUCT_DEFINITION_SHAPE($,$,#246);
#63851=PRODUCT_DEFINITION_SHAPE($,$,#247);
#63852=PRODUCT_DEFINITION_SHAPE($,$,#248);
#63853=PRODUCT_DEFINITION_SHAPE($,$,#249);
#63854=PRODUCT_DEFINITION_SHAPE($,$,#250);
#63855=PRODUCT_DEFINITION_SHAPE($,$,#251);
#63856=PRODUCT_DEFINITION_SHAPE($,$,#252);
#63857=PRODUCT_DEFINITION_SHAPE($,$,#253);
#63858=SHAPE_REPRESENTATION('',(#14502,#15510,#15511,#15512,#15513,#15514),
#63736);
#63859=SHAPE_REPRESENTATION('',(#14503,#14700,#14701,#14702,#14703,#14704,
#14705,#14706,#14707,#14708,#14709,#14710,#14711,#14712,#14713,#14714,#14715,
#14716,#14717,#14718,#14719,#14720,#14721,#14722,#14723,#14724,#14725,#14726,
#14727,#14728,#14729,#14730,#14731,#14732,#14733,#14734,#14735,#14736,#14737,
#14738,#14739),#63737);
#63860=SHAPE_REPRESENTATION('',(#14504),#63738);
#63861=SHAPE_REPRESENTATION('',(#14515),#63739);
#63862=SHAPE_REPRESENTATION('',(#14526),#63740);
#63863=SHAPE_REPRESENTATION('',(#14621),#63741);
#63864=SHAPE_REPRESENTATION('',(#14691),#63742);
#63865=SHAPE_REPRESENTATION('',(#14740,#15495,#15496,#15497,#15498,#15499,
#15500,#15501,#15502,#15503,#15504,#15505,#15506,#15507,#15508,#15509),
#63743);
#63866=SHAPE_REPRESENTATION('',(#14741),#63744);
#63867=SHAPE_REPRESENTATION('',(#15053),#63745);
#63868=SHAPE_REPRESENTATION('',(#15079),#63746);
#63869=SHAPE_REPRESENTATION('',(#15139),#63747);
#63870=SHAPE_REPRESENTATION('',(#15145),#63748);
#63871=SHAPE_REPRESENTATION('',(#15232),#63749);
#63872=SHAPE_REPRESENTATION('',(#15253),#63750);
#63873=SHAPE_REPRESENTATION('',(#15394),#63751);
#63874=SHAPE_REPRESENTATION('',(#15425),#63752);
#63875=SHAPE_REPRESENTATION('',(#15434),#63753);
#63876=SHAPE_REPRESENTATION('',(#15486),#63754);
#63877=PRODUCT_DEFINITION_CONTEXT('part definition',#63936,'design');
#63878=PRODUCT_DEFINITION('MAS-649','MAS-649',#63897,#63877);
#63879=PRODUCT_DEFINITION('Connecting frame','Connecting frame',#63898,
#63877);
#63880=PRODUCT_DEFINITION('Longitudinal rail','Longitudinal rail',#63899,
#63877);
#63881=PRODUCT_DEFINITION('Transverse rail','Transverse rail',#63900,#63877);
#63882=PRODUCT_DEFINITION('Corner plate','Corner plate',#63901,#63877);
#63883=PRODUCT_DEFINITION('Socket head cap screw M8x25',
'Socket head cap screw M8x25',#63902,#63877);
#63884=PRODUCT_DEFINITION('Flat Washer M8','Flat washer M8',#63903,#63877);
#63885=PRODUCT_DEFINITION('Support leg','Support leg',#63904,#63877);
#63886=PRODUCT_DEFINITION('Leg post','Leg post',#63905,#63877);
#63887=PRODUCT_DEFINITION('Mounting plate','Mounting plate',#63906,#63877);
#63888=PRODUCT_DEFINITION('Socket head cap screw M10x20',
'Socket head cap screw M10x20',#63907,#63877);
#63889=PRODUCT_DEFINITION('Grip sole','Grip sole',#63908,#63877);
#63890=PRODUCT_DEFINITION('Swivel pad','Swivel pad',#63909,#63877);
#63891=PRODUCT_DEFINITION('Ball retainer','Ball retainer',#63910,#63877);
#63892=PRODUCT_DEFINITION('Adjusting spindle','Adjusting spindle',#63911,
#63877);
#63893=PRODUCT_DEFINITION('Lock nut M10','Lock nut M10',#63912,#63877);
#63894=PRODUCT_DEFINITION('Flat washer M10','Flat washer M10',#63913,#63877);
#63895=PRODUCT_DEFINITION('Socket head cap screw M6x16',
'Socket head cap screw M6x16',#63914,#63877);
#63896=PRODUCT_DEFINITION('Flat washer M6','Flat washer M6',#63915,#63877);
#63897=PRODUCT_DEFINITION_FORMATION('',$,#63938);
#63898=PRODUCT_DEFINITION_FORMATION('',$,#63939);
#63899=PRODUCT_DEFINITION_FORMATION('',$,#63940);
#63900=PRODUCT_DEFINITION_FORMATION('',$,#63941);
#63901=PRODUCT_DEFINITION_FORMATION('',$,#63942);
#63902=PRODUCT_DEFINITION_FORMATION('',$,#63943);
#63903=PRODUCT_DEFINITION_FORMATION('',$,#63944);
#63904=PRODUCT_DEFINITION_FORMATION('',$,#63945);
#63905=PRODUCT_DEFINITION_FORMATION('',$,#63946);
#63906=PRODUCT_DEFINITION_FORMATION('',$,#63947);
#63907=PRODUCT_DEFINITION_FORMATION('',$,#63948);
#63908=PRODUCT_DEFINITION_FORMATION('',$,#63949);
#63909=PRODUCT_DEFINITION_FORMATION('',$,#63950);
#63910=PRODUCT_DEFINITION_FORMATION('',$,#63951);
#63911=PRODUCT_DEFINITION_FORMATION('',$,#63952);
#63912=PRODUCT_DEFINITION_FORMATION('',$,#63953);
#63913=PRODUCT_DEFINITION_FORMATION('',$,#63954);
#63914=PRODUCT_DEFINITION_FORMATION('',$,#63955);
#63915=PRODUCT_DEFINITION_FORMATION('',$,#63956);
#63916=PRODUCT_RELATED_PRODUCT_CATEGORY('MAS-649','MAS-649',(#63938));
#63917=PRODUCT_RELATED_PRODUCT_CATEGORY('Connecting frame',
'Connecting frame',(#63939));
#63918=PRODUCT_RELATED_PRODUCT_CATEGORY('Longitudinal rail',
'Longitudinal rail',(#63940));
#63919=PRODUCT_RELATED_PRODUCT_CATEGORY('Transverse rail',
'Transverse rail',(#63941));
#63920=PRODUCT_RELATED_PRODUCT_CATEGORY('Corner plate','Corner plate',(#63942));
#63921=PRODUCT_RELATED_PRODUCT_CATEGORY('Socket head cap screw M8x25',
'Socket head cap screw M8x25',(#63943));
#63922=PRODUCT_RELATED_PRODUCT_CATEGORY('Flat washer M8',
'Flat washer M8',(#63944));
#63923=PRODUCT_RELATED_PRODUCT_CATEGORY('Support leg','Support leg',(#63945));
#63924=PRODUCT_RELATED_PRODUCT_CATEGORY('Leg post','Leg post',(#63946));
#63925=PRODUCT_RELATED_PRODUCT_CATEGORY('Mounting plate',
'Mounting plate',(#63947));
#63926=PRODUCT_RELATED_PRODUCT_CATEGORY('Socket head cap screw M10x20',
'Socket head cap screw M10x20',(#63948));
#63927=PRODUCT_RELATED_PRODUCT_CATEGORY('Grip sole','Grip sole',(#63949));
#63928=PRODUCT_RELATED_PRODUCT_CATEGORY('Swivel pad','Swivel pad',(#63950));
#63929=PRODUCT_RELATED_PRODUCT_CATEGORY('Ball retainer','Ball retainer',
(#63951));
#63930=PRODUCT_RELATED_PRODUCT_CATEGORY('Adjusting spindle',
'Adjusting spindle',(#63952));
#63931=PRODUCT_RELATED_PRODUCT_CATEGORY('Lock nut M10','Lock nut M10',(#63953));
#63932=PRODUCT_RELATED_PRODUCT_CATEGORY('Flat washer M10',
'Flat washer M10',(#63954));
#63933=PRODUCT_RELATED_PRODUCT_CATEGORY('Socket head cap screw M6x16',
'Socket head cap screw M6x16',(#63955));
#63934=PRODUCT_RELATED_PRODUCT_CATEGORY('Flat washer M6',
'Flat washer M6',(#63956));
#63935=APPLICATION_PROTOCOL_DEFINITION('international standard',
'automotive_design',2009,#63936);
#63936=APPLICATION_CONTEXT(
'Core Data for Automotive Mechanical Design Process');
#63937=PRODUCT_CONTEXT('part definition',#63936,'mechanical');
#63938=PRODUCT('MAS-649','MAS-649',
'Independent equipment support assembly with bolted 600 x 500 mm welde
d perimeter frame, four adjustable legs and swivel feet. Nominal overa
ll height 518 mm. No load rating assigned.',(#63937));
#63939=PRODUCT('Connecting frame','Connecting frame',$,(#63937));
#63940=PRODUCT('Longitudinal rail','Longitudinal rail',
'Steel rectangular hollow section, 50 x 40 mm, 4 mm wall. Square cut e
nds; weld to adjoining rails and corner plates.',(#63937));
#63941=PRODUCT('Transverse rail','Transverse rail',
'Steel rectangular hollow section, 50 x 40 mm, 4 mm wall. Square cut e
nds; weld to adjoining rails and corner plates.',(#63937));
#63942=PRODUCT('Corner plate','Corner plate',
'Weld rails to upper face. Four M8x1 attachment taps on 70 mm square p
attern match the leg plate clearance holes.',(#63937));
#63943=PRODUCT('Socket head cap screw M8x25',
'Socket head cap screw M8x25',$,(#63937));
#63944=PRODUCT('Flat Washer M8','Flat washer M8','NOT SPECIFIED',(#63937));
#63945=PRODUCT('Support leg','Support leg',$,(#63937));
#63946=PRODUCT('Leg post','Leg post',
'Independent aluminum extrusion section. Whole-mm nominal die dimensio
ns; parametric saw-cut length. Select structural loading, tolerances a
nd finish for the assembly application.',(#63937));
#63947=PRODUCT('Mounting plate','Mounting plate','Mounting plate',(#63937));
#63948=PRODUCT('Socket head cap screw M10x20',
'Socket head cap screw M10x20',$,(#63937));
#63949=PRODUCT('Grip sole','Grip sole',
'Bonded elastomer sole; nominal diameter 60 mm, thickness 4 mm.',(#63937));
#63950=PRODUCT('Swivel pad','Swivel pad',$,(#63937));
#63951=PRODUCT('Ball retainer','Ball retainer',$,(#63937));
#63952=PRODUCT('Adjusting spindle','Adjusting spindle',$,(#63937));
#63953=PRODUCT('Lock nut M10','Lock nut M10',$,(#63937));
#63954=PRODUCT('Flat washer M10','Flat washer M10',$,(#63937));
#63955=PRODUCT('Socket head cap screw M6x16',
'Socket head cap screw M6x16',$,(#63937));
#63956=PRODUCT('Flat washer M6','Flat washer M6',$,(#63937));
#63957=PRESENTATION_STYLE_ASSIGNMENT((#63964));
#63958=PRESENTATION_STYLE_ASSIGNMENT((#63965));
#63959=PRESENTATION_STYLE_ASSIGNMENT((#63966));
#63960=PRESENTATION_STYLE_ASSIGNMENT((#63967));
#63961=PRESENTATION_STYLE_ASSIGNMENT((#63968));
#63962=PRESENTATION_STYLE_ASSIGNMENT((#63969));
#63963=PRESENTATION_STYLE_ASSIGNMENT((#63970));
#63964=SURFACE_STYLE_USAGE(.BOTH.,#63971);
#63965=SURFACE_STYLE_USAGE(.BOTH.,#63972);
#63966=SURFACE_STYLE_USAGE(.BOTH.,#63973);
#63967=SURFACE_STYLE_USAGE(.BOTH.,#63974);
#63968=SURFACE_STYLE_USAGE(.BOTH.,#63975);
#63969=SURFACE_STYLE_USAGE(.BOTH.,#63976);
#63970=SURFACE_STYLE_USAGE(.BOTH.,#63977);
#63971=SURFACE_SIDE_STYLE('',(#63978));
#63972=SURFACE_SIDE_STYLE('',(#63979));
#63973=SURFACE_SIDE_STYLE('',(#63980));
#63974=SURFACE_SIDE_STYLE('',(#63981));
#63975=SURFACE_SIDE_STYLE('',(#63982));
#63976=SURFACE_SIDE_STYLE('',(#63983));
#63977=SURFACE_SIDE_STYLE('',(#63984));
#63978=SURFACE_STYLE_FILL_AREA(#63985);
#63979=SURFACE_STYLE_FILL_AREA(#63986);
#63980=SURFACE_STYLE_FILL_AREA(#63987);
#63981=SURFACE_STYLE_FILL_AREA(#63988);
#63982=SURFACE_STYLE_FILL_AREA(#63989);
#63983=SURFACE_STYLE_FILL_AREA(#63990);
#63984=SURFACE_STYLE_FILL_AREA(#63991);
#63985=FILL_AREA_STYLE('Steel - Satin',(#63992));
#63986=FILL_AREA_STYLE('Dark blue',(#63993));
#63987=FILL_AREA_STYLE('Sky blue',(#63994));
#63988=FILL_AREA_STYLE('Dark gray',(#63995));
#63989=FILL_AREA_STYLE('Light gray',(#63996));
#63990=FILL_AREA_STYLE('Gray',(#63997));
#63991=FILL_AREA_STYLE('Light blue',(#63998));
#63992=FILL_AREA_STYLE_COLOUR('Steel - Satin',#63999);
#63993=FILL_AREA_STYLE_COLOUR('Dark blue',#64000);
#63994=FILL_AREA_STYLE_COLOUR('Sky blue',#64001);
#63995=FILL_AREA_STYLE_COLOUR('Dark gray',#64002);
#63996=FILL_AREA_STYLE_COLOUR('Light gray',#64003);
#63997=FILL_AREA_STYLE_COLOUR('Gray',#64004);
#63998=FILL_AREA_STYLE_COLOUR('Light blue',#64005);
#63999=COLOUR_RGB('Steel - Satin',0.627450980392157,0.627450980392157,0.627450980392157);
#64000=COLOUR_RGB('Dark blue',0.0901960784313725,0.270588235294118,0.513725490196078);
#64001=COLOUR_RGB('Sky blue',0.317647058823529,0.686274509803922,0.890196078431372);
#64002=COLOUR_RGB('Dark gray',0.250980392156863,0.282352941176471,0.32156862745098);
#64003=COLOUR_RGB('Light gray',0.725490196078431,0.752941176470588,0.792156862745098);
#64004=COLOUR_RGB('Gray',0.407843137254902,0.447058823529412,0.498039215686275);
#64005=COLOUR_RGB('Light blue',0.662745098039216,0.831372549019608,0.949019607843137);
ENDSEC;
END-ISO-10303-21;
